#106531 = VERTEX_POINT ( 'NONE', #76599 ) ;
#106532 = CARTESIAN_POINT ( 'NONE',  ( 5.436732529336289588, -1.586671906620169104, 1.244382051841623538 ) ) ;
#106533 = CARTESIAN_POINT ( 'NONE',  ( -7.811469059767924605, 12.26513100303794168, -0.7998128361456281477 ) ) ;
#106534 = CARTESIAN_POINT ( 'NONE',  ( 1.499999999999990896, 4.275000000000021672, 1.214306433183764966E-14 ) ) ;
#106535 = CARTESIAN_POINT ( 'NONE',  ( 11.86145016429273191, 10.19999999999999929, 1.099999999999996758 ) ) ;
#106536 = CARTESIAN_POINT ( 'NONE',  ( 1.622189073652591240, 2.139406107190901185, -0.3685050674664645531 ) ) ;
#106537 = DIRECTION ( 'NONE',  ( 0.000000000000000000, 1.000000000000000000, 0.000000000000000000 ) ) ;
#106538 = CARTESIAN_POINT ( 'NONE',  ( 0.1938080739139167730, 1.976361990896974508, -0.7691651810952588875 ) ) ;
#106539 = CARTESIAN_POINT ( 'NONE',  ( 0.7499999999999902300, 2.264583334016148530, 1.299038105676669330 ) ) ;
#106540 = CARTESIAN_POINT ( 'NONE',  ( -1.797304807700269569, 14.48004927660067764, -11.89862588611542726 ) ) ;
#106541 = SURFACE_STYLE_USAGE ( .BOTH. , #91331 ) ;
#106542 = CARTESIAN_POINT ( 'NONE',  ( 4.895464504754282409, 8.144056917144915531, 1.010406422583273178 ) ) ;
#106543 = CARTESIAN_POINT ( 'NONE',  ( 0.9837496482606482573, 1.382075509872608299, 1.528818673835147024 ) ) ;
#106544 = CARTESIAN_POINT ( 'NONE',  ( -8.130085669689073313, 12.63685038127928806, 0.7998128361456481317 ) ) ;
#106545 = CARTESIAN_POINT ( 'NONE',  ( -0.6823417656250003738, 0.7177083336747519526, -1.181850606188749264 ) ) ;
#106546 = CARTESIAN_POINT ( 'NONE',  ( -0.4019237886466871523, 9.198664549684631098, -1.499999999999998668 ) ) ;
#106547 = VERTEX_POINT ( 'NONE', #130761 ) ;
#106548 = CARTESIAN_POINT ( 'NONE',  ( 3.176317266091326807, 0.8619891151622931513, 1.707069686517001195 ) ) ;
#106549 = CIRCLE ( 'NONE', #6118, 1.224999999999996980 ) ;
#106550 = CARTESIAN_POINT ( 'NONE',  ( 4.961649905909814251, 1.750258134581949232, -0.2615843724830448913 ) ) ;
#106551 = CARTESIAN_POINT ( 'NONE',  ( 5.254667053748194760, 8.288139441751686931, 1.199719254218452047 ) ) ;
#106552 = CARTESIAN_POINT ( 'NONE',  ( -4.334856428067329404, 6.080418470877079429, -1.599625672291256295 ) ) ;
#106553 = CARTESIAN_POINT ( 'NONE',  ( 0.2986855335190057859, -0.2218818089524568216, -1.797891974444510765 ) ) ;
#106555 = CARTESIAN_POINT ( 'NONE',  ( 6.116788041597909675, 0.1929307199614685164, 1.905880049602140636 ) ) ;
#106554 = CARTESIAN_POINT ( 'NONE',  ( 7.721398836998401904, -6.134628647623499909, 7.721398836998376147 ) ) ;
#106556 = CARTESIAN_POINT ( 'NONE',  ( 0.4849360239999983557, 1.980737741294085419, 0.6024896509310638804 ) ) ;
#106557 = CARTESIAN_POINT ( 'NONE',  ( -1.402160292154681736E-14, -0.8656249996585829720, 1.575800808251672791 ) ) ;
#106558 = AXIS2_PLACEMENT_3D ( 'NONE', #214401, #132179, #64986 ) ;
#106559 = CARTESIAN_POINT ( 'NONE',  ( 5.998880656844745474, 1.528293836345222312, -1.078463600801618405 ) ) ;
#106560 = CARTESIAN_POINT ( 'NONE',  ( 2.666400811807769777, -1.259032629953384719, 1.322343945743660543 ) ) ;
#106561 = ADVANCED_FACE ( 'NONE', ( #47332 ), #39578, .T. ) ;
#106563 = CARTESIAN_POINT ( 'NONE',  ( 6.465908158583062892, 6.764574590967027845, 0.2795716154820517829 ) ) ;
#106562 = CARTESIAN_POINT ( 'NONE',  ( 6.059228469117068805, -1.890744221452178353, -1.137928576693452820 ) ) ;
#106564 = CARTESIAN_POINT ( 'NONE',  ( 1.364683531249988757, 0.6343750003414208027, 0.000000000000000000 ) ) ;
#106565 = CARTESIAN_POINT ( 'NONE',  ( 2.840340301219072217, -1.062657783794159538, 1.767763702702547679 ) ) ;
#106566 = CARTESIAN_POINT ( 'NONE',  ( -8.538937818508475885, 8.856515631215026829, 1.040834085586084257E-14 ) ) ;
#106567 = CARTESIAN_POINT ( 'NONE',  ( 9.250740883225924804, 9.686952540052077509, 1.040834085586084257E-14 ) ) ;
#106568 = CARTESIAN_POINT ( 'NONE',  ( 4.005544317833563461, 6.760553239859419250, -1.199719254218452047 ) ) ;
#106569 = CARTESIAN_POINT ( 'NONE',  ( 0.6499751493908960676, 0.6786997614584532323, -2.052318101833712660 ) ) ;
#106570 = CARTESIAN_POINT ( 'NONE',  ( 6.408651866624735405, 0.6456447432892989946, 1.967203394946090977 ) ) ;
#106571 =( BOUNDED_SURFACE ( )  B_SPLINE_SURFACE ( 3, 3, ( 
 ( #185995, #120019, #203304, #54951, #121104, #33354, #139418, #92811, #39772, #23499, #205453, #123251, #6171, #105877, #157801, #7238 ),
 ( #106961, #10452, #204364, #73315, #125365, #88531, #56020, #72239, #24565, #171901, #141581, #8325, #191328, #57086, #189215, #138347 ),
 ( #206520, #109107, #142636, #140509, #42994, #75469, #76525, #91748, #207589, #154592, #188140, #9397, #158854, #175122, #59208, #122174 ),
 ( #26708, #89605, #40855, #155656, #172986, #74409, #38704, #208645, #90671, #60277, #156734, #187071, #58152, #104784, #124311, #190270 ),
 ( #41927, #108038, #25636, #174064, #170830, #22421, #94941, #11524, #2440, #18706, #209709, #159919, #97075, #179380, #12581, #126434 ),
 ( #79725, #145841, #133584, #128576, #78653, #46187, #93881, #110172, #129638, #63484, #211846, #67439, #150877, #117355, #34957, #61353 ),
 ( #29927, #1378, #176183, #160989, #31000, #84789, #195625, #199588, #47260, #111237, #27782, #177240, #144781, #62412, #192397, #166044 ) ),
 .UNSPECIFIED., .T., .F., .F. ) 
 B_SPLINE_SURFACE_WITH_KNOTS ( ( 4, 3, 4 ),
 ( 4, 2, 2, 2, 2, 2, 2, 4 ),
 ( 0.000000000000000000, 0.5000000000000000000, 1.000000000000000000 ),
 ( 0.6095821870314059865, 0.6120980958896804491, 0.6146140047479549118, 0.6196458224645037260, 0.6297094578976014656, 0.6397880689092279027, 0.6448273744150412323, 0.6498666799208544509 ),
 .UNSPECIFIED. ) 
 GEOMETRIC_REPRESENTATION_ITEM ( )  RATIONAL_B_SPLINE_SURFACE ( (
 ( 1.000000000000000000, 1.000000000000000000, 1.000000000000000000, 1.000000000000000000, 1.000000000000000000, 1.000000000000000000, 1.000000000000000000, 1.000000000000000000, 1.000000000000000000, 1.000000000000000000, 1.000000000000000000, 1.000000000000000000, 1.000000000000000000, 1.000000000000000000, 1.000000000000000000, 1.000000000000000000),
 ( 0.3333333333333333703, 0.3333333333333333703, 0.3333333333333333703, 0.3333333333333333703, 0.3333333333333333703, 0.3333333333333333703, 0.3333333333333333703, 0.3333333333333333703, 0.3333333333333333703, 0.3333333333333333703, 0.3333333333333333703, 0.3333333333333333703, 0.3333333333333333703, 0.3333333333333333703, 0.3333333333333333703, 0.3333333333333333703),
 ( 0.3333333333333333703, 0.3333333333333333703, 0.3333333333333333703, 0.3333333333333333703, 0.3333333333333333703, 0.3333333333333333703, 0.3333333333333333703, 0.3333333333333333703, 0.3333333333333333703, 0.3333333333333333703, 0.3333333333333333703, 0.3333333333333333703, 0.3333333333333333703, 0.3333333333333333703, 0.3333333333333333703, 0.3333333333333333703),
 ( 1.000000000000000000, 1.000000000000000000, 1.000000000000000000, 1.000000000000000000, 1.000000000000000000, 1.000000000000000000, 1.000000000000000000, 1.000000000000000000, 1.000000000000000000, 1.000000000000000000, 1.000000000000000000, 1.000000000000000000, 1.000000000000000000, 1.000000000000000000, 1.000000000000000000, 1.000000000000000000),
 ( 0.3333333333333333703, 0.3333333333333333703, 0.3333333333333333703, 0.3333333333333333703, 0.3333333333333333703, 0.3333333333333333703, 0.3333333333333333703, 0.3333333333333333703, 0.3333333333333333703, 0.3333333333333333703, 0.3333333333333333703, 0.3333333333333333703, 0.3333333333333333703, 0.3333333333333333703, 0.3333333333333333703, 0.3333333333333333703),
 ( 0.3333333333333333703, 0.3333333333333333703, 0.3333333333333333703, 0.3333333333333333703, 0.3333333333333333703, 0.3333333333333333703, 0.3333333333333333703, 0.3333333333333333703, 0.3333333333333333703, 0.3333333333333333703, 0.3333333333333333703, 0.3333333333333333703, 0.3333333333333333703, 0.3333333333333333703, 0.3333333333333333703, 0.3333333333333333703),
 ( 1.000000000000000000, 1.000000000000000000, 1.000000000000000000, 1.000000000000000000, 1.000000000000000000, 1.000000000000000000, 1.000000000000000000, 1.000000000000000000, 1.000000000000000000, 1.000000000000000000, 1.000000000000000000, 1.000000000000000000, 1.000000000000000000, 1.000000000000000000, 1.000000000000000000, 1.000000000000000000) ) ) 
 REPRESENTATION_ITEM ( '' )  SURFACE ( )  );
#106572 = CARTESIAN_POINT ( 'NONE',  ( -1.364683531250000748, -0.4281249996585800854, 0.000000000000000000 ) ) ;
#106573 = CARTESIAN_POINT ( 'NONE',  ( 4.059979352932830743, 2.145800628424157974, -0.2601280725000321148 ) ) ;
#106575 = CARTESIAN_POINT ( 'NONE',  ( 2.084357000244409175, 1.132115006494602394, -1.602057852124554316 ) ) ;
#106574 = CARTESIAN_POINT ( 'NONE',  ( 4.723309930327257433, 1.758355855194023487, 0.9934411112178792580 ) ) ;
#106576 = LINE ( 'NONE', #4714, #80609 ) ;
#106577 = ORIENTED_EDGE ( 'NONE', *, *, #42175, .T. ) ;
#106580 = CARTESIAN_POINT ( 'NONE',  ( 7.131225611108096274, 8.382479970123348778, 1.082531754730558626 ) ) ;
#106579 = CARTESIAN_POINT ( 'NONE',  ( 1.001543065824772753E-15, -3.521874999522041083, 3.793834371823811669 ) ) ;
#106578 = DIRECTION ( 'NONE',  ( -0.000000000000000000, 1.000000000000000000, -0.000000000000000000 ) ) ;
#106581 = CARTESIAN_POINT ( 'NONE',  ( -6.095272577795516789, 9.268845886473535245, 1.199719254218452047 ) ) ;
#106582 = CARTESIAN_POINT ( 'NONE',  ( 2.852750215419812108, -1.865046845876184189, -0.7672916333427428626 ) ) ;
#106583 = CARTESIAN_POINT ( 'NONE',  ( -4.497554271431319250, 6.270232621468402989, -1.599625672291256295 ) ) ;
#106584 = FACE_OUTER_BOUND ( 'NONE', #25579, .T. ) ;
#106585 = CARTESIAN_POINT ( 'NONE',  ( 5.660397963661894849, 1.910509065610028090, 0.08734628876111423523 ) ) ;
#106587 = DIRECTION ( 'NONE',  ( 0.000000000000000000, 0.000000000000000000, -1.000000000000000000 ) ) ;
#106586 = B_SPLINE_CURVE_WITH_KNOTS ( 'NONE', 3,
 ( #51983, #16247, #81284, #34650, #146311, #131163, #150560, #33588, #1062, #163612, #17317, #180906, #18391, #113861, #82333, #101789, #63964, #114908, #183034, #35712, #62647, #67127, #197154, #50911, #184093, #100720, #84468, #48791, #2120, #68195 ),
 .UNSPECIFIED., .F., .F.,
 ( 4, 2, 2, 2, 2, 2, 2, 2, 2, 2, 2, 2, 2, 2, 4 ),
 ( -5.999999999772596264E-08, 0.0009256177583834637734, 0.001851295516766925239, 0.002776973275150386271, 0.003702651033533847953, 0.004628328791917308768, 0.005554006550300769583, 0.006479684308684230398, 0.007405362067067692081, 0.009256717583834615445, 0.01018239534221807886, 0.01110807310060153881, 0.01203375085898500049, 0.01295942861736846217, 0.01481078413413538554 ),
 .UNSPECIFIED. ) ;
#106588 = CARTESIAN_POINT ( 'NONE',  ( 5.951666246274803562, 7.006327377817825663, 1.082531754730558626 ) ) ;
#106590 = CARTESIAN_POINT ( 'NONE',  ( 3.866814677988283044, -0.2004539179165897023, -2.006445418776988010 ) ) ;
#106589 = CARTESIAN_POINT ( 'NONE',  ( -8.392133896734675247, 10.81390885098904420, 1.443375672974064550 ) ) ;
#106591 = CARTESIAN_POINT ( 'NONE',  ( 1.499999999999989120, 3.754166666666685082, 0.8660254037844524744 ) ) ;
#106592 = CARTESIAN_POINT ( 'NONE',  ( -1.402160292154681736E-14, 14.73437500034139980, 1.575800808251682339 ) ) ;
#106593 = VECTOR ( 'NONE', #102765, 1000.000000000000000 ) ;
#106594 = CARTESIAN_POINT ( 'NONE',  ( 6.370102249521607973, 0.8915232854993185851, 1.476320845237573787 ) ) ;
#106595 = CARTESIAN_POINT ( 'NONE',  ( 6.038177310039780643, 8.137902509836795417, -1.599625672291283607 ) ) ;
#106596 = CARTESIAN_POINT ( 'NONE',  ( 9.408995418203975447, 10.07950886410055524, 0.7216878364870438212 ) ) ;
#106597 = CARTESIAN_POINT ( 'NONE',  ( 10.99861980075107937, -9.900000000000074962, -0.1919816227428264854 ) ) ;
#106598 = CARTESIAN_POINT ( 'NONE',  ( 4.147608549738549755, 0.6325110726591242072, -1.760471310998643624 ) ) ;
#106599 = CARTESIAN_POINT ( 'NONE',  ( 4.663288057535368125, 8.288536188413402783, 0.5084364831346009916 ) ) ;
#106600 = CARTESIAN_POINT ( 'NONE',  ( 1.674760025662187735, 1.393346669028448392, -1.531324272915953744 ) ) ;
#106601 = CARTESIAN_POINT ( 'NONE',  ( -1.387358672531441961, 7.251968950356099342, -4.302625267141395149 ) ) ;
#106602 = ORIENTED_EDGE ( 'NONE', *, *, #190530, .T. ) ;
#106603 = CARTESIAN_POINT ( 'NONE',  ( 4.686278372178935392, 5.496354851410763409, 1.199719254218452047 ) ) ;
#106604 = CARTESIAN_POINT ( 'NONE',  ( -0.05311194370935175268, -1.802413661875476913, -0.9041393574176490588 ) ) ;
#106605 = CARTESIAN_POINT ( 'NONE',  ( 6.633470331352866900, -0.1302952867699505302, 1.781688180685939926 ) ) ;
#106606 = EDGE_CURVE ( 'NONE', #51151, #134523, #85200, .T. ) ;
#106607 = CARTESIAN_POINT ( 'NONE',  ( 3.865483193227626124, 7.523831135491951372, -0.7216878364870338292 ) ) ;
#106608 = FACE_OUTER_BOUND ( 'NONE', #87550, .T. ) ;
#106609 = CARTESIAN_POINT ( 'NONE',  ( 7.415946836550712185, 10.63539316174243865, 1.082531754730558626 ) ) ;
#106610 = EDGE_CURVE ( 'NONE', #12264, #207276, #1512, .T. ) ;
#106611 = CARTESIAN_POINT ( 'NONE',  ( 6.401421083946654100, 10.62007503124645957, -0.7998128361456291469 ) ) ;
#106613 = CARTESIAN_POINT ( 'NONE',  ( 6.380494711820015930, -0.5163536399260219012, -1.844617532318414632 ) ) ;
#106612 = CARTESIAN_POINT ( 'NONE',  ( -5.422371370461663176, 8.413518134592214537, -1.199719254218446718 ) ) ;
#106614 = CARTESIAN_POINT ( 'NONE',  ( 0.000000000000000000, -4.000000000000003553, 0.000000000000000000 ) ) ;
#106615 = SURFACE_STYLE_USAGE ( .BOTH. , #142301 ) ;
#106617 = ORIENTED_EDGE ( 'NONE', *, *, #32909, .T. ) ;
#106616 = CARTESIAN_POINT ( 'NONE',  ( 3.389175213736285386, 6.897862149426897460, 0.7216878364870317197 ) ) ;
#106618 = CARTESIAN_POINT ( 'NONE',  ( -6.860062538834774237, 10.94723069537516302, 0.7216878364870458196 ) ) ;
#106619 = CARTESIAN_POINT ( 'NONE',  ( 3.379894511112140787, 1.369989894601089775, 1.672159933133889442 ) ) ;
#106620 = CARTESIAN_POINT ( 'NONE',  ( -2.810282979782591006, 6.500690253046801814, 0.000000000000000000 ) ) ;
#106621 = EDGE_CURVE ( 'NONE', #40241, #5998, #163080, .T. ) ;
#106622 = CARTESIAN_POINT ( 'NONE',  ( 8.000720045840086669, 8.506797273001177828, 0.7216878364870267237 ) ) ;
#106623 = CARTESIAN_POINT ( 'NONE',  ( 0.9144942500491149984, -2.120778211678171488, 0.005759991200282586418 ) ) ;
#106624 = CARTESIAN_POINT ( 'NONE',  ( 5.666980381186065507, -1.651371415153819688, -0.7785968546244539379 ) ) ;
#106625 = CARTESIAN_POINT ( 'NONE',  ( 9.013329340612937557, 11.11377505082129069, -8.022259956411712523 ) ) ;
#106626 = CARTESIAN_POINT ( 'NONE',  ( 1.141796867408477967, 0.8028701493673767731, -1.800646566474963572 ) ) ;
#106627 = CARTESIAN_POINT ( 'NONE',  ( 3.550944491985886575, 0.2853618425060593378, 1.890879049853078087 ) ) ;
#106628 = ORIENTED_EDGE ( 'NONE', *, *, #52227, .T. ) ;
#106629 = CARTESIAN_POINT ( 'NONE',  ( -11.48243876534946040, 9.799999999999998934, -3.200000000000001510 ) ) ;
#106630 = CARTESIAN_POINT ( 'NONE',  ( 5.230891393285493685, -1.853837313009810028, -0.6654804215649990917 ) ) ;
#106631 = CARTESIAN_POINT ( 'NONE',  ( 0.6560686395847237229, -1.407132438187887136, 1.338565165000434876 ) ) ;
#106632 = ORIENTED_EDGE ( 'NONE', *, *, #51505, .T. ) ;
#106633 = CARTESIAN_POINT ( 'NONE',  ( -4.664887371553763096, 7.600063145858131364, -1.199719254218453823 ) ) ;
#106635 = CARTESIAN_POINT ( 'NONE',  ( -1.225000000000045386, 1.312500000682802259, -4.336808689942017736E-14 ) ) ;
#106634 = CARTESIAN_POINT ( 'NONE',  ( -5.472651281771599763, 6.413789912602166687, 1.199719254218452935 ) ) ;
#106636 = CARTESIAN_POINT ( 'NONE',  ( 5.356880090730850696, 9.263794182579101033, 0.7216878364870317197 ) ) ;
#106638 = VERTEX_POINT ( 'NONE', #641 ) ;
#106637 = CARTESIAN_POINT ( 'NONE',  ( 3.879479457080482696, 0.2311173251203814394, -1.898182577502210977 ) ) ;
#106639 = CARTESIAN_POINT ( 'NONE',  ( 1.255210933454937283, -1.738917431694649185, 1.358592805172780693 ) ) ;
#106640 = CARTESIAN_POINT ( 'NONE',  ( 9.333041836227119248, 3.553052365627043407, -7.472413793103452662 ) ) ;
#106641 = CARTESIAN_POINT ( 'NONE',  ( 6.639320575229259447, 0.002292789353198348111, 1.996863816985874118 ) ) ;
#106642 = CARTESIAN_POINT ( 'NONE',  ( 0.000000000000000000, -8.176568542494905500, 0.000000000000000000 ) ) ;
#106643 = CARTESIAN_POINT ( 'NONE',  ( -4.596923820214036560, 8.483565078729160547, 0.2266403168418751335 ) ) ;
#106644 = CARTESIAN_POINT ( 'NONE',  ( -0.08896015503664694846, 7.049507384514476449, -3.948637857580539201 ) ) ;
#106645 = CARTESIAN_POINT ( 'NONE',  ( 2.277862540309500083, -2.008769142935047380, 0.5008063122204224893 ) ) ;
#106646 = CARTESIAN_POINT ( 'NONE',  ( -5.388475986427523345, 8.373973519885682393, 1.199719254218452047 ) ) ;
#106647 = TOROIDAL_SURFACE ( 'NONE', #26953, 2.349999999999999645, 0.1000000000000000056 ) ;
#106648 = CARTESIAN_POINT ( 'NONE',  ( -4.603881723180708541, 8.384271979250147666, 0.04571010684512218092 ) ) ;
#106649 = CARTESIAN_POINT ( 'NONE',  ( 0.1280963075596490419, -1.331634228802502928, -1.703589906866372017 ) ) ;
#106650 = CARTESIAN_POINT ( 'NONE',  ( 4.313465427442102929, 8.184126765324453601, 0.7998128361456462443 ) ) ;
#106651 = CARTESIAN_POINT ( 'NONE',  ( -11.95061148709128140, 8.982475982309534146, -1.242198177808604198 ) ) ;
#106652 = CARTESIAN_POINT ( 'NONE',  ( 3.757017964762656703, 7.397288368949487491, -1.734723475976807094E-15 ) ) ;
#106653 = CARTESIAN_POINT ( 'NONE',  ( 1.772826578343081660, 3.950000000000036593, -0.4000000000000478728 ) ) ;
#106654 = CARTESIAN_POINT ( 'NONE',  ( 4.403700966340357681, 4.032072637018845107, -0.7998128361456211532 ) ) ;
#106655 = CARTESIAN_POINT ( 'NONE',  ( 1.364683531249996529, 13.27604166700806410, 0.7879004041258405033 ) ) ;
#106657 = CARTESIAN_POINT ( 'NONE',  ( -5.769876891067536206, 8.889217585290882795, 1.199719254218454489 ) ) ;
#106656 = CARTESIAN_POINT ( 'NONE',  ( 6.825078400183548055, 3.702925343214446663, 2.370119418288775925 ) ) ;
#106658 = CARTESIAN_POINT ( 'NONE',  ( 5.221237796217499394, 1.709784868986977902, 0.2885349091684140665 ) ) ;
#106659 = CARTESIAN_POINT ( 'NONE',  ( -4.711622075948912247, 5.455646162483875017, -1.199719254218446718 ) ) ;
#106660 = CIRCLE ( 'NONE', #47901, 0.08000000000000018208 ) ;
#106661 = CARTESIAN_POINT ( 'NONE',  ( 2.008725816923035978, 0.6454906730102347723, 1.967154155859623055 ) ) ;
#106662 = CARTESIAN_POINT ( 'NONE',  ( 3.374719764411674205, -0.4154235484931252942, -2.075916080105549177 ) ) ;
#106664 = CARTESIAN_POINT ( 'NONE',  ( 6.425674737872927089, 9.584038729905381970, -1.199719254218440723 ) ) ;
#106663 = B_SPLINE_CURVE_WITH_KNOTS ( 'NONE', 3,
 ( #18989, #69858, #120857, #22168, #85071, #185753, #38461 ),
 .UNSPECIFIED., .F., .F.,
 ( 4, 3, 4 ),
 ( 0.000000000000000000, 2.757963454290271384E-05, 5.739065715766676189E-05 ),
 .UNSPECIFIED. ) ;
#106666 = EDGE_CURVE ( 'NONE', #167216, #45056, #2298, .T. ) ;
#106665 = CARTESIAN_POINT ( 'NONE',  ( -1.201851678989727383E-14, 3.571875000341422357, 1.575800808251672791 ) ) ;
#106667 = CARTESIAN_POINT ( 'NONE',  ( 1.533974946755271240, 1.168952700103634390, 1.584878304665905180 ) ) ;
#106668 = CARTESIAN_POINT ( 'NONE',  ( 5.809489818682099127, 6.211223759639540987, 0.9523037572534819306 ) ) ;
#106669 = CYLINDRICAL_SURFACE ( 'NONE', #84058, 2.500000000000007994 ) ;
#106670 = CARTESIAN_POINT ( 'NONE',  ( 4.207168913946373934, -0.3938425722496830539, 2.258028373892074558 ) ) ;
#106671 = CARTESIAN_POINT ( 'NONE',  ( 1.945663734523142230, 0.6997465788082489757, -1.686465609443507763 ) ) ;
#106672 = ADVANCED_FACE ( 'NONE', ( #29999 ), #103601, .F. ) ;
#106673 = CARTESIAN_POINT ( 'NONE',  ( 6.215487077222150880, 6.216099443039444949, 0.000000000000000000 ) ) ;
#106674 = CARTESIAN_POINT ( 'NONE',  ( 6.439759776366769550, 8.536139043893143707, 1.443375672974076540 ) ) ;
#106675 = CARTESIAN_POINT ( 'NONE',  ( -6.835281999583978418, 11.12624609948998966, -0.7998128361456291469 ) ) ;
#106676 = CARTESIAN_POINT ( 'NONE',  ( 2.531496316177814787, -0.1932786158439051827, 2.003878288502713101 ) ) ;
#106677 = CARTESIAN_POINT ( 'NONE',  ( 3.045700443693433179, 1.383923128670875746, 1.390673908496591782 ) ) ;
#106678 = CARTESIAN_POINT ( 'NONE',  ( -6.821723845970312894, 11.11042825360738284, 0.000000000000000000 ) ) ;
#106679 = CARTESIAN_POINT ( 'NONE',  ( -4.740547266272593596, 8.682388910626682943, -0.7998128361456281477 ) ) ;
#106680 = CARTESIAN_POINT ( 'NONE',  ( 0.1751657365761339624, 7.629137130509054288, -2.644001943226172102 ) ) ;
#106682 = CARTESIAN_POINT ( 'NONE',  ( 4.082668839255446436, -0.1736907016443404450, -1.761279006307460371 ) ) ;
#106681 = CARTESIAN_POINT ( 'NONE',  ( 5.876921326125680523, 1.932075295558054240, -0.7991432938223922422 ) ) ;
#106683 = CARTESIAN_POINT ( 'NONE',  ( 6.021229617800532452, 6.197391773621639288, 0.000000000000000000 ) ) ;
#106684 = CARTESIAN_POINT ( 'NONE',  ( 1.078377591563362436, -2.138745004354754897, -0.4770250503970187572 ) ) ;
#106685 = CARTESIAN_POINT ( 'NONE',  ( 5.613164593121685364, -1.696513092703657799, 0.3873091720919922265 ) ) ;
#106686 = CARTESIAN_POINT ( 'NONE',  ( 6.591235234537977661, 10.84152487360300299, 0.7998128361456462443 ) ) ;
#106687 = CARTESIAN_POINT ( 'NONE',  ( -4.650083499807243115, 5.295740330745369207, -1.052294140492322283 ) ) ;
#106688 = CARTESIAN_POINT ( 'NONE',  ( 5.854147224351119227, 0.1731004610599009841, -2.292201554650086237 ) ) ;
#106689 = CARTESIAN_POINT ( 'NONE',  ( 0.1333692844072559558, 0.7140749627707367875, -2.136770008611441618 ) ) ;
#106690 = CARTESIAN_POINT ( 'NONE',  ( 5.395702507230883072, 0.1292110896585068891, 1.729053200853872596 ) ) ;
#106691 = CARTESIAN_POINT ( 'NONE',  ( 1.612255294781844706, -2.189918024983358080, 0.2725913246661854084 ) ) ;
#106692 = CARTESIAN_POINT ( 'NONE',  ( 5.723135995274492238, -1.960344405425541670, -0.9336216343173405763 ) ) ;
#106693 = CARTESIAN_POINT ( 'NONE',  ( -1.999999999999988010, 2.428612866367529932E-14, 1.500000000000001332 ) ) ;
#106694 = CARTESIAN_POINT ( 'NONE',  ( 0.09316046741510237983, 1.845552173327277501, 1.037660268145562004 ) ) ;
#106695 = CARTESIAN_POINT ( 'NONE',  ( 4.500000000000003553, -2.561000571632643674E-13, -2.052068128417943171 ) ) ;
#106696 = CARTESIAN_POINT ( 'NONE',  ( 6.827182134110200806, 2.035520418778674845, 2.394189263408800450 ) ) ;
#106697 = CARTESIAN_POINT ( 'NONE',  ( 4.875960570263176308, 1.108828003875685475, 1.575097709652195643 ) ) ;
#106698 = CARTESIAN_POINT ( 'NONE',  ( 1.717743135698499124, 1.849103211704594463, 1.230578002476825583 ) ) ;
#106699 = ORIENTED_EDGE ( 'NONE', *, *, #38876, .F. ) ;
#106700 = CARTESIAN_POINT ( 'NONE',  ( 1.499999999999989120, 4.254166666666687746, 0.8660254037844524744 ) ) ;
#106701 = CARTESIAN_POINT ( 'NONE',  ( 5.820528018968444961, 5.685037531751635953, 0.7998128361456341429 ) ) ;
#106702 = CARTESIAN_POINT ( 'NONE',  ( 5.445571254183207088, 9.504916896522420444, -0.7998128361456281477 ) ) ;
#106703 = VECTOR ( 'NONE', #127459, 1000.000000000000000 ) ;
#106704 = CARTESIAN_POINT ( 'NONE',  ( 3.370003599138057471, 0.5381768412672756074, -2.155016279732512974 ) ) ;
#106705 = CARTESIAN_POINT ( 'NONE',  ( -8.893785580884703279, 10.43879993486270585, 1.082531754730558626 ) ) ;
#106706 = FACE_OUTER_BOUND ( 'NONE', #18379, .T. ) ;
#106707 = CARTESIAN_POINT ( 'NONE',  ( 6.155038550924139429, 9.164333495178082600, 1.082531754730558626 ) ) ;
#106708 = CARTESIAN_POINT ( 'NONE',  ( -8.310784975052671442, 11.67937098999472667, -1.082531754730543083 ) ) ;
#106709 = CARTESIAN_POINT ( 'NONE',  ( 5.234856708652215751, 9.121433570154021453, 0.7216878364870317197 ) ) ;
#106710 = CARTESIAN_POINT ( 'NONE',  ( 2.127577483945505055, 0.4445034925110411539, 1.966644524931899563 ) ) ;
#106712 = CARTESIAN_POINT ( 'NONE',  ( 0.3036763228623740041, -1.592034637876770908, -1.310935287704196206 ) ) ;
#106711 = CARTESIAN_POINT ( 'NONE',  ( 8.589254009457354400, 9.979550084910457031, -1.199719254218446718 ) ) ;
#106713 = CARTESIAN_POINT ( 'NONE',  ( -10.99917004716958857, -6.764708007038216842, 0.1531059978909550534 ) ) ;
#106714 = CARTESIAN_POINT ( 'NONE',  ( 6.821160681006781523, 9.051383109298340557, 1.443375672974063439 ) ) ;
#106715 = CARTESIAN_POINT ( 'NONE',  ( 6.620655732516682157, 0.01042156863441953685, 1.726407961933309476 ) ) ;
#106716 = CARTESIAN_POINT ( 'NONE',  ( -2.530224277154541124, 2.018041202053984406, 11.90376931803457872 ) ) ;
#106717 = CARTESIAN_POINT ( 'NONE',  ( -1.201851678989727383E-14, 1.821875000341421691, 1.575800808251672791 ) ) ;
#106718 = CARTESIAN_POINT ( 'NONE',  ( 1.000807349803897628, 1.442299932730039869, 1.025250199436118503 ) ) ;
#106719 = CARTESIAN_POINT ( 'NONE',  ( 0.4752326960846975923, -2.001511663014220677, -0.2440270837566413387 ) ) ;
#106720 = CARTESIAN_POINT ( 'NONE',  ( 0.4504185290156897947, -1.555054577268409899, -0.9855837367087336709 ) ) ;
#106721 = CARTESIAN_POINT ( 'NONE',  ( 4.142302782979132125, 0.6112592793995803575, 2.209291399377455889 ) ) ;
#106722 = CARTESIAN_POINT ( 'NONE',  ( 2.044624030687072214, -1.478315374303545315, -1.097237131862264903 ) ) ;
#106723 = CARTESIAN_POINT ( 'NONE',  ( 10.07387183015377197, 11.71160420905630062, -1.199719254218440723 ) ) ;
#106724 = CARTESIAN_POINT ( 'NONE',  ( 7.416522329255045065, 14.99999999999999645, -9.452665224861386051 ) ) ;
#106725 = CARTESIAN_POINT ( 'NONE',  ( 3.487140482124751362, 1.650829432287181264, -0.7796944959364560113 ) ) ;
#106726 = CARTESIAN_POINT ( 'NONE',  ( 4.026017654026761150, -1.753031021560845559, 0.9963007555989014108 ) ) ;
#106727 = CARTESIAN_POINT ( 'NONE',  ( -9.938290294017125603, 11.55342575023019691, -1.199719254218441611 ) ) ;
#106729 = CARTESIAN_POINT ( 'NONE',  ( -9.584291988782265292, -7.189630408304557463, 0.001123102408834306858 ) ) ;
#106728 = CARTESIAN_POINT ( 'NONE',  ( 3.626065245518626412, -1.345661663401491293, -1.818709669598504997 ) ) ;
#106730 = CARTESIAN_POINT ( 'NONE',  ( 5.807678370005410429, -0.5150985282868367765, 2.041858835689168927 ) ) ;
#106731 = CARTESIAN_POINT ( 'NONE',  ( 9.257559171758622085, 13.68169161456526162, 6.840446529487702598 ) ) ;
#106732 = CARTESIAN_POINT ( 'NONE',  ( 2.066927875543830950, 1.535623996113824496, -1.388825173883188713 ) ) ;
#106733 = CARTESIAN_POINT ( 'NONE',  ( 5.190073875932979419, 4.949507698210251938, 0.7998128361456341429 ) ) ;
#106734 = CARTESIAN_POINT ( 'NONE',  ( 0.6801582343749813520, 0.005208333674754095366, 1.178068619123793015 ) ) ;
#106735 = CARTESIAN_POINT ( 'NONE',  ( 5.391314312714450274, -0.05227466736787074464, -2.120015263102632552 ) ) ;
#106737 = CARTESIAN_POINT ( 'NONE',  ( 0.8383531591091289981, 1.897801360490163569, 0.3304300003270659314 ) ) ;
#106736 = CARTESIAN_POINT ( 'NONE',  ( -8.157201976916404362, 12.66848607304450702, -0.7998128361456281477 ) ) ;
#106738 = CARTESIAN_POINT ( 'NONE',  ( -5.113360211009450040, 5.994616996712990975, -1.199719254218453823 ) ) ;
#106739 = CARTESIAN_POINT ( 'NONE',  ( 7.086107841436786181, 11.41887624831828418, 1.040834085586084257E-14 ) ) ;
#106740 = CARTESIAN_POINT ( 'NONE',  ( 4.217995187182915551, 7.935095128439824563, 0.7216878364870257245 ) ) ;
#106741 = CARTESIAN_POINT ( 'NONE',  ( 4.677432586336220055, 6.849818891840005364, 1.226792522213099979 ) ) ;
#106742 = CARTESIAN_POINT ( 'NONE',  ( -1.737499999999997824, -0.5979166657107508609, 3.009438278150925683 ) ) ;
#106743 = VECTOR ( 'NONE', #190395, 1000.000000000000000 ) ;
#106744 = CARTESIAN_POINT ( 'NONE',  ( -4.334856428067329404, 6.080418470877079429, -1.599625672291256295 ) ) ;
#106745 = CARTESIAN_POINT ( 'NONE',  ( 1.002519415922138002, -0.9925456330053865628, 1.987394366727333717 ) ) ;
#106746 = CARTESIAN_POINT ( 'NONE',  ( 2.608543117039106463, -0.8048738574607334773, -1.946287526097515430 ) ) ;
#106747 = CARTESIAN_POINT ( 'NONE',  ( -3.467853430045390706, 7.267855778353407459, 0.7998128361456352531 ) ) ;
#106748 = CARTESIAN_POINT ( 'NONE',  ( 6.913768267964901071, 10.15348118167935709, -1.199719254218441611 ) ) ;
#106749 = CARTESIAN_POINT ( 'NONE',  ( 5.770303593930925956, -0.8350939829899912681, -1.663081984830430793 ) ) ;
#106750 = CARTESIAN_POINT ( 'NONE',  ( 8.437251666405968464, 8.737881787095446384, 1.040834085586084257E-14 ) ) ;
#106751 = CARTESIAN_POINT ( 'NONE',  ( -11.04536101718726293, 10.19999999999999929, -1.100000000000000311 ) ) ;
#106752 = CARTESIAN_POINT ( 'NONE',  ( -6.211043768836215229, 8.339580045099285854, 1.443375672974064550 ) ) ;
#106753 = CARTESIAN_POINT ( 'NONE',  ( -7.185458225562757484, 11.32685899655781903, 0.7216878364870458196 ) ) ;
#106754 = CARTESIAN_POINT ( 'NONE',  ( -0.06985027309261250539, -2.078401542846250116, 0.4200961532789050379 ) ) ;
#106755 = CARTESIAN_POINT ( 'NONE',  ( -6.831329296439251131, 9.063246493969506545, -1.599625672291271394 ) ) ;
#106757 = CARTESIAN_POINT ( 'NONE',  ( 3.016010921186715432, 1.952665002612500533, -0.1895750030070641190 ) ) ;
#106756 = CARTESIAN_POINT ( 'NONE',  ( -1.225000000000005640, 1.387778780781445676E-14, -1.387778780781445676E-14 ) ) ;
#106758 = CARTESIAN_POINT ( 'NONE',  ( 2.272554088390315030, -1.330374092946192688, 1.703740541667747133 ) ) ;
#106760 = CARTESIAN_POINT ( 'NONE',  ( -4.775553520644376881, 6.797630844710244702, -1.243162211532616857 ) ) ;
#106759 = CARTESIAN_POINT ( 'NONE',  ( -4.634908411025374875, 6.500755460986618495, 1.599625672291263179 ) ) ;
#106761 = CARTESIAN_POINT ( 'NONE',  ( 1.364683531249988757, 2.134375000341422357, 1.214306433183764966E-14 ) ) ;
#106762 = CARTESIAN_POINT ( 'NONE',  ( 3.714586447349605081, -0.1257948980903991487, 1.735838019273880928 ) ) ;
#106763 = AXIS2_PLACEMENT_3D ( 'NONE', #46852, #99845, #131338 ) ;
#106764 = CARTESIAN_POINT ( 'NONE',  ( 7.307481608085759639, 7.627742752295940676, 1.040834085586084257E-14 ) ) ;
#106765 = CARTESIAN_POINT ( 'NONE',  ( -11.79406710134376191, 4.782197168659454434, 4.941180684906744780 ) ) ;
#106766 = CARTESIAN_POINT ( 'NONE',  ( 0.9366540776252421097, 2.129889809250965271, 0.3686189752144660714 ) ) ;
#106767 = CARTESIAN_POINT ( 'NONE',  ( 2.513045873335068237, 2.015604327017831654, 0.05229110803010171560 ) ) ;
#106768 = CARTESIAN_POINT ( 'NONE',  ( -10.95308175811721085, 12.30000000000000071, -1.800000000000001155 ) ) ;
#106769 = CARTESIAN_POINT ( 'NONE',  ( 0.6311622855796321652, 3.199999999999987743, 0.3999999999999646061 ) ) ;
#106770 = GEOMETRIC_CURVE_SET ( 'NONE', ( #168733, #3369, #103896, #127391 ) ) ;
#106771 = CARTESIAN_POINT ( 'NONE',  ( 2.465646028844501902, 1.933766160897397057, -0.3828895411656701997 ) ) ;
#106774 = VERTEX_POINT ( 'NONE', #88340 ) ;
#106773 = CARTESIAN_POINT ( 'NONE',  ( -5.533136088152923904, 6.588318536667425285, 1.082531754730549078 ) ) ;
#106772 = CARTESIAN_POINT ( 'NONE',  ( 6.539320575229249144, 0.007148032025052972194, 1.896977914940492393 ) ) ;
#106775 = CARTESIAN_POINT ( 'NONE',  ( -5.438229012412899799, 7.437962829272074750, -1.443375672974066548 ) ) ;
#106776 = CARTESIAN_POINT ( 'NONE',  ( 7.388267364804250725, 7.584343111885245570, -0.7998128361456341429 ) ) ;
#106777 = CARTESIAN_POINT ( 'NONE',  ( -5.444481204339554736, 8.509589284108232121, 1.199719254218454489 ) ) ;
#106778 = CARTESIAN_POINT ( 'NONE',  ( 2.350265711909118593, 0.9499565981557709371, -1.782299418695271198 ) ) ;
#106779 = DIRECTION ( 'NONE',  ( 1.000000000000000000, -0.000000000000000000, -0.000000000000000000 ) ) ;
#106780 = CARTESIAN_POINT ( 'NONE',  ( 6.088978940744814494, -0.3304744056438710387, -2.283700556900492451 ) ) ;
#106781 = CARTESIAN_POINT ( 'NONE',  ( 0.000000000000000000, -8.176568542494905500, 0.000000000000000000 ) ) ;
#106782 = CARTESIAN_POINT ( 'NONE',  ( 2.694135368495911731, 0.9291169126603683326, -1.727816930623335967 ) ) ;
#106783 = CARTESIAN_POINT ( 'NONE',  ( 8.341290820905593151, 10.75459192918846618, 1.599625672291281386 ) ) ;
#106784 = CARTESIAN_POINT ( 'NONE',  ( 0.6334356698059574464, 0.5880228326464317368, 1.928751028484784191 ) ) ;
#106785 = ORIENTED_EDGE ( 'NONE', *, *, #89006, .F. ) ;
#106786 = CARTESIAN_POINT ( 'NONE',  ( 2.694651208505644213, 1.530237149716510370, -1.463602791221560118 ) ) ;
#106788 = CARTESIAN_POINT ( 'NONE',  ( -7.705111371268023923, 7.883718109434487253, 1.040834085586084257E-14 ) ) ;
#106787 = CARTESIAN_POINT ( 'NONE',  ( -2.286521462199063492, 5.819358805874190743, 1.040834085586084257E-14 ) ) ;
#106789 = CARTESIAN_POINT ( 'NONE',  ( 1.745803608711377075, 0.5764907460206626366, 1.748616612666432868 ) ) ;
#106790 = EDGE_LOOP ( 'NONE', ( #34878, #119835, #51225, #32839 ) ) ;
#106791 = CARTESIAN_POINT ( 'NONE',  ( -9.215791728987058562, 11.77484298861683598, -1.599625672291263179 ) ) ;
#106792 = CARTESIAN_POINT ( 'NONE',  ( 9.768119350134290002, 11.88398385152791903, 6.892589425638673717 ) ) ;
#106793 = CARTESIAN_POINT ( 'NONE',  ( 4.394861267144759331, -2.057662932662501110, -0.5123870273424437904 ) ) ;
#106794 = CARTESIAN_POINT ( 'NONE',  ( 0.2339851986729903077, 0.3116528534230639247, 1.814411239467295101 ) ) ;
#106795 = CARTESIAN_POINT ( 'NONE',  ( -1.499999999999997780, 5.181250000682820378, 1.214306433183764966E-14 ) ) ;
#106796 = CARTESIAN_POINT ( 'NONE',  ( 7.613066949273408213, 8.840665181362512115, -1.199719254218441611 ) ) ;
#106797 = CARTESIAN_POINT ( 'NONE',  ( 6.556249800660121529, 9.806652646482286073, 1.199719254218452047 ) ) ;
#106798 = CARTESIAN_POINT ( 'NONE',  ( 4.903620131156614548, -0.5536938069644473659, 1.984910608926907960 ) ) ;
#106800 = CARTESIAN_POINT ( 'NONE',  ( 1.891909123491273492, -0.4922293657834125313, -1.774144672653771293 ) ) ;
#106799 = CARTESIAN_POINT ( 'NONE',  ( -7.714753101375940503, 8.959299025482085455, 1.199719254218462483 ) ) ;
#106801 = CARTESIAN_POINT ( 'NONE',  ( 1.364683531249988535, 4.655208333674755394, -0.7879004041258300672 ) ) ;
#106802 = CARTESIAN_POINT ( 'NONE',  ( -1.598423149420381106, 8.713846000021360894, 2.500000000000011102 ) ) ;
#106803 = CARTESIAN_POINT ( 'NONE',  ( 0.9311234436981525864, -1.603119629485603825, 3.474999999999998757 ) ) ;
#106804 = AXIS2_PLACEMENT_3D ( 'NONE', #54137, #35739, #149505 ) ;
#106805 = CARTESIAN_POINT ( 'NONE',  ( 0.5752038918783763943, -2.079344756725898691, -0.7397341299467049547 ) ) ;
#106806 = CARTESIAN_POINT ( 'NONE',  ( 3.743696771605113494, -1.710248914368957873, -1.481124664604586583 ) ) ;
#106807 = CARTESIAN_POINT ( 'NONE',  ( -8.242994207428740339, 9.679543332497402730, 1.082531754730558626 ) ) ;
#106808 = CARTESIAN_POINT ( 'NONE',  ( 3.164119808340008611, 1.811767227632065325, -0.004774541488360150264 ) ) ;
#106809 = CARTESIAN_POINT ( 'NONE',  ( 3.327253086410830729, -1.454009962414861912, -1.247479002808443704 ) ) ;
#106810 = CARTESIAN_POINT ( 'NONE',  ( 4.000488093070094564, 2.060113009926473726, 0.2059288336104248551 ) ) ;
#106811 = CARTESIAN_POINT ( 'NONE',  ( -1.201851678989727383E-14, 3.634375000341422357, 1.575800808251672791 ) ) ;
#106812 = CARTESIAN_POINT ( 'NONE',  ( 2.483225996990960027, 1.803144932609510143, -0.7974705804912070040 ) ) ;
#106813 = CARTESIAN_POINT ( 'NONE',  ( 0.5867820057828515568, -0.2326963965399355405, -1.912219011898611765 ) ) ;
#106814 = CARTESIAN_POINT ( 'NONE',  ( 4.100366707588389836, -0.5864361863821172527, -1.776433678864146382 ) ) ;
#106815 = EDGE_CURVE ( 'NONE', #68781, #45420, #133924, .T. ) ;
#106816 = CARTESIAN_POINT ( 'NONE',  ( 2.245130213409586961, 0.5076759487793567338, 2.251015715305480391 ) ) ;
#106817 = CARTESIAN_POINT ( 'NONE',  ( 4.211269073929763351, -1.546465011353677532, -1.035020834652039090 ) ) ;
#106818 = CARTESIAN_POINT ( 'NONE',  ( 1.364683531249988535, 4.405208333674754506, -0.7879004041258300672 ) ) ;
#106819 = CIRCLE ( 'NONE', #65297, 0.7499999999999997780 ) ;
#106820 = CARTESIAN_POINT ( 'NONE',  ( -3.100010679019018500, 6.768429558830820980, 1.040834085586084257E-14 ) ) ;
#106821 = CARTESIAN_POINT ( 'NONE',  ( 11.40591166468351503, 3.507114751586604129, -3.706005353348470255 ) ) ;
#106822 = B_SPLINE_CURVE_WITH_KNOTS ( 'NONE', 3,
 ( #206911, #122575, #140900, #188537, #123640, #109499 ),
 .UNSPECIFIED., .F., .F.,
 ( 4, 2, 4 ),
 ( 0.000000000000000000, 0.0003132070624402877746, 0.0006264141248805755492 ),
 .UNSPECIFIED. ) ;
#106823 = CARTESIAN_POINT ( 'NONE',  ( 0.4695305163736606668, 0.2040741594158005934, -2.096154701512464413 ) ) ;
#106824 = CARTESIAN_POINT ( 'NONE',  ( 4.650083499362880346, 4.527444958785877382, 0.7216878364870317197 ) ) ;
#106826 = CARTESIAN_POINT ( 'NONE',  ( -11.00006988736403102, -9.999999999999994671, 0.09199170129444225741 ) ) ;
#106825 = CARTESIAN_POINT ( 'NONE',  ( 1.364683531249990311, 4.926041667008083991, 0.7879004041258500513 ) ) ;
#106827 = CARTESIAN_POINT ( 'NONE',  ( 6.854756222516504849, -1.675677847961650313, 1.365199464886861946 ) ) ;
#106828 = CARTESIAN_POINT ( 'NONE',  ( 2.478903650112133317, -1.459102030866548994, 1.539066919819010781 ) ) ;
#106829 = FILL_AREA_STYLE ('',( #90542 ) ) ;
#106830 = CARTESIAN_POINT ( 'NONE',  ( 0.4748752182902976071, -1.459934291025711373, 1.395986992609834276 ) ) ;
#106831 = CARTESIAN_POINT ( 'NONE',  ( -0.6823417656250003738, 1.217708333674752286, -1.181850606188749264 ) ) ;
#106832 = CARTESIAN_POINT ( 'NONE',  ( -3.904385051055635270, 6.538571078664754843, 1.082531754730560403 ) ) ;
#106833 = CARTESIAN_POINT ( 'NONE',  ( 6.308621549060418054, 6.254479983525607523, 0.7998128361456341429 ) ) ;
#106834 = CARTESIAN_POINT ( 'NONE',  ( 1.353037089713942320, -1.704917477850418805, 1.328741451194020762 ) ) ;
#106837 = CARTESIAN_POINT ( 'NONE',  ( 3.199361063144961825, 6.676412307070352270, -0.7216878364870267237 ) ) ;
#106836 = CARTESIAN_POINT ( 'NONE',  ( 6.925078400183550364, 4.696033252921790968, 2.518291795588607052 ) ) ;
#106835 = CARTESIAN_POINT ( 'NONE',  ( 4.037295881819344956, 7.932205305423046582, -0.7998128361456362523 ) ) ;
#106838 = CARTESIAN_POINT ( 'NONE',  ( -4.787964524281469458, 5.614988695530339413, -1.199719254218453823 ) ) ;
#106839 = CARTESIAN_POINT ( 'NONE',  ( 6.122279814772176643, 1.995267444086584296, 0.2910868170948808786 ) ) ;
#106840 = CARTESIAN_POINT ( 'NONE',  ( -8.351459436338041442, 9.806086099558291025, -1.082531754730543971 ) ) ;
#106841 = CARTESIAN_POINT ( 'NONE',  ( 0.08191350661116909848, -1.027414926483052326, 1.935800647029708443 ) ) ;
#106842 = FILL_AREA_STYLE_COLOUR ( '', #101685 ) ;
#106844 = CARTESIAN_POINT ( 'NONE',  ( 1.364683531249996529, 10.71354166700806942, 0.7879004041258403923 ) ) ;
#106843 = CARTESIAN_POINT ( 'NONE',  ( 0.7083710243460902278, -2.251296572208848712, 0.2248925466769024495 ) ) ;
#106845 = CARTESIAN_POINT ( 'NONE',  ( -8.286004436246233951, 12.81875560892930466, 1.040834085586084257E-14 ) ) ;
#106847 = CARTESIAN_POINT ( 'NONE',  ( 1.177184062793021679, 1.451467631357589383, 1.250241458713635456 ) ) ;
#106846 = CARTESIAN_POINT ( 'NONE',  ( -4.717874267431199087, 8.448011045404303587, 1.040834085586084257E-14 ) ) ;
#106848 = CARTESIAN_POINT ( 'NONE',  ( -1.364683531250000748, 1.071875000341421247, 0.000000000000000000 ) ) ;
#106849 = CARTESIAN_POINT ( 'NONE',  ( -7.834948825496938163, -9.999999999999994671, -7.720982897393569466 ) ) ;
#106850 = CARTESIAN_POINT ( 'NONE',  ( -1.500000000000008216, 9.000000000000001776, 3.469446951953614189E-15 ) ) ;
#106851 = CARTESIAN_POINT ( 'NONE',  ( 2.648709078547459850, -1.434216206362935564, 0.9578970732360950757 ) ) ;
#106852 = CARTESIAN_POINT ( 'NONE',  ( 5.551137550152489553, 5.441024994791534120, 0.7998128361456352531 ) ) ;
#106853 = TOROIDAL_SURFACE ( 'NONE', #93053, 3.599999999999999201, 0.4999999999999998890 ) ;
#106854 = CARTESIAN_POINT ( 'NONE',  ( 0.4382651835369972826, 0.2938455168926180638, 1.745004787994571593 ) ) ;
#106855 =( BOUNDED_CURVE ( )  B_SPLINE_CURVE ( 2, ( #23090, #69707, #107635, #135811, #88122 ),
 .UNSPECIFIED., .F., .T. ) 
 B_SPLINE_CURVE_WITH_KNOTS ( ( 3, 2, 3 ),
 ( 0.2851912450777800423, 0.2874999999999999778, 0.2888802418687935192 ),
 .UNSPECIFIED. ) 
 CURVE ( )  GEOMETRIC_REPRESENTATION_ITEM ( )  RATIONAL_B_SPLINE_CURVE ( ( 0.9337969725178141278, 0.9257645179683744452, 1.000000000000000000, 0.9556198367076580436, 0.9406422459849084206 ) ) 
 REPRESENTATION_ITEM ( '' )  );
#106856 = CARTESIAN_POINT ( 'NONE',  ( 2.051433223282957297, -1.797157160989469427, 0.9072355583341712437 ) ) ;
#106857 = SURFACE_STYLE_FILL_AREA ( #139319 ) ;
#106858 = CARTESIAN_POINT ( 'NONE',  ( 8.550388431712704573, 13.12720360364021133, 0.000000000000000000 ) ) ;
#106859 = CARTESIAN_POINT ( 'NONE',  ( 4.085166796624926100, -0.2132991444873769959, -2.196430506890618695 ) ) ;
#106860 = EDGE_LOOP ( 'NONE', ( #41450, #131099, #109204, #69129 ) ) ;
#106861 = CARTESIAN_POINT ( 'NONE',  ( 7.849807752188022292, 11.14156422998596696, -1.082531754730543083 ) ) ;
#106862 = CARTESIAN_POINT ( 'NONE',  ( -5.589704470584107909, 9.743348658981940247, -0.7998128361456362523 ) ) ;
#106864 = CARTESIAN_POINT ( 'NONE',  ( 3.972279928656559100, -1.994873972748755442, -0.2930500606010341125 ) ) ;
#106863 = CARTESIAN_POINT ( 'NONE',  ( 4.371814246616528621, 0.4635510597098577712, -2.069045912693792566 ) ) ;
#106866 = ORIENTED_EDGE ( 'NONE', *, *, #45431, .T. ) ;
#106865 = CARTESIAN_POINT ( 'NONE',  ( 3.216879062660949362, 1.425012358211204422, -1.118398921490076026 ) ) ;
#106867 = CARTESIAN_POINT ( 'NONE',  ( 4.376249722160992839, 8.327651452488305850, 0.000000000000000000 ) ) ;
#106868 = ORIENTED_EDGE ( 'NONE', *, *, #191917, .T. ) ;
#106869 = CARTESIAN_POINT ( 'NONE',  ( 1.709613803025863188, -1.856884215550944850, 0.2259493607114013147 ) ) ;
#106870 = STYLED_ITEM ( 'NONE', ( #129639 ), #13191 ) ;
#106871 = CARTESIAN_POINT ( 'NONE',  ( 5.813091150998386247, 1.612263477354998864, 0.8566026058636074803 ) ) ;
#106872 = CARTESIAN_POINT ( 'NONE',  ( -4.451154503988200339, 4.087435097607984957, 1.214306433183764966E-14 ) ) ;
#106873 = DIRECTION ( 'NONE',  ( 0.7592566023653016805, 0.6507913734559627184, 4.115938288792103177E-15 ) ) ;
#106874 =( NAMED_UNIT ( * ) SI_UNIT ( $, .STERADIAN. ) SOLID_ANGLE_UNIT ( ) );
#106875 = CARTESIAN_POINT ( 'NONE',  ( -1.402160292154681736E-14, 1.509375000341420359, -1.575800808251659024 ) ) ;
#106876 = CARTESIAN_POINT ( 'NONE',  ( 2.421437874748389341, 3.696394713403123866, -11.55257195323928876 ) ) ;
#106877 = ORIENTED_EDGE ( 'NONE', *, *, #165849, .F. ) ;
#106878 = B_SPLINE_CURVE_WITH_KNOTS ( 'NONE', 3,
 ( #160527, #77137, #12132, #210328, #179983, #79278, #15319, #191935, #208192, #195168, #161611, #64099, #97680, #95560, #80341, #30542, #31604, #112916, #96622, #43599, #143258, #61966, #196233, #128122, #162676, #163738, #78204, #45735, #145395, #109718, #209247, #178927, #111853, #29469, #13201, #211393, #175723, #63022, #193011, #176778, #14246, #129190, #146441, #94489, #212454, #59825, #125978, #44665, #60891, #110778, #93421, #159458, #127051, #28394, #194082, #52111, #134460, #182084, #81407, #213512, #34774, #83527, #149610, #18525, #1192, #66183, #200464, #49974, #100846, #69394, #48918, #118237, #181038, #147490, #115039, #33715, #132329, #99792, #198334, #197278, #166932, #36909, #84603, #19594, #150691, #116093, #131291, #165859, #184222, #17444, #119300, #2253, #67256, #32654, #68329, #35844, #85667, #199397, #101923, #183170, #117, #102991, #133391, #169049, #98732, #51043, #117166, #65133, #164790, #167989, #151753, #3324, #135501, #201524, #16382, #53172, #185286, #82461, #148551, #205810, #55311, #173343, #136571, #23854, #21698, #89962, #20647, #186357, #120382, #24923, #37993, #22775, #88892, #172267, #154946, #5451, #73685, #203660, #188499, #8678, #202592, #42277, #74760, #140862, #104065, #139783, #86736, #54244, #108391, #91028, #57441, #190619, #156013, #157089, #40131, #71530, #70456, #137641, #123602, #105145, #58507, #170111, #39059, #6530, #72608, #171185, #189567, #107319, #121460, #41212, #87809, #138708, #204724, #152805, #56375, #122538, #153882, #187430, #206876, #106241, #7600, #124662, #4384, #211134, #9747, #94233, #210066, #158154, #13996, #145128, #208995, #46537, #75821, #128918, #96365, #192749, #43344, #44406, #28138, #146182, #111589, #110526, #59563, #80081, #25992, #212197, #141929, #177599, #60631, #77950, #160271, #176526, #62758, #61706, #193824, #11873, #66721, #112658, #194899, #207942, #144071, #127874, #29211, #125723, #109464, #79012, #45473, #95301, #161350, #12931, #191683, #178667, #10802, #126794, #30279, #132864, #50515, #162419, #198868, #174415, #142997, #76876, #175471, #92100, #27057, #93164, #159201, #199945, #186900, #118773, #4919, #19062, #154419, #68868, #70996, #134988, #69930, #202054, #200998, #203138, #169595, #170657, #21177, #54780, #20126, #101392, #103535, #5997, #119847, #117716, #185825, #116638, #67788, #1731, #120927, #133938, #184757, #36384, #53714, #102462, #167466, #100327, #37456, #87280, #153349, #38532, #138178, #104610, #22244, #51592, #137109, #182633, #150163, #204188, #88354, #72068, #34255, #166394, #17985, #136042, #85140, #84075, #183706, #35314, #52643, #86212, #151227, #168528, #152284, #3857, #2796, #92645, #142466, #40681, #10285, #56914, #173894, #124141, #55844, #190103, #140332, #91577, #122000, #143544, #59040, #57978, #26537, #75299, #158687, #105697, #41756, #157629, #39594, #110003, #76359, #90497, #208474, #171724, #60110, #192226, #74239, #106784, #126269, #9227, #43889, #156560, #206351, #155482, #176016, #187966, #27608, #23323, #125198, #8155, #25469, #107868, #141414, #172812, #207421, #93708, #191161, #159748, #11346, #77427, #89431, #42828, #7065, #123087, #108934, #73138, #174955, #139243, #205274, #24384, #189044, #161899, #97971, #13486, #162962, #80638, #79561, #145680, #178144, #49209, #48161, #81692, #113204 ),
 .UNSPECIFIED., .F., .F.,
 ( 4, 1, 1, 1, 1, 1, 1, 1, 1, 1, 1, 1, 1, 1, 1, 1, 1, 1, 1, 1, 1, 1, 1, 1, 1, 1, 1, 1, 1, 1, 1, 1, 1, 1, 1, 1, 1, 1, 1, 1, 1, 1, 1, 1, 1, 1, 1, 1, 1, 1, 1, 1, 1, 1, 1, 1, 1, 1, 1, 1, 1, 1, 1, 1, 1, 1, 1, 1, 1, 1, 1, 1, 1, 1, 1, 1, 1, 1, 1, 1, 1, 1, 1, 1, 1, 1, 1, 1, 1, 1, 1, 1, 1, 1, 1, 1, 1, 1, 1, 1, 1, 1, 1, 1, 1, 1, 1, 1, 1, 1, 1, 1, 1, 1, 1, 1, 1, 1, 1, 1, 1, 1, 1, 1, 1, 1, 1, 1, 1, 1, 1, 1, 1, 1, 1, 1, 1, 1, 1, 1, 1, 1, 1, 1, 1, 1, 1, 1, 1, 1, 1, 1, 1, 1, 1, 1, 1, 1, 1, 1, 1, 1, 1, 1, 1, 1, 1, 1, 1, 1, 1, 1, 1, 1, 1, 1, 1, 1, 1, 1, 1, 1, 1, 1, 1, 1, 1, 1, 1, 1, 1, 1, 1, 1, 1, 1, 1, 1, 1, 1, 1, 1, 1, 1, 1, 1, 1, 1, 1, 1, 1, 1, 1, 1, 1, 1, 1, 1, 1, 1, 1, 1, 1, 1, 1, 1, 1, 1, 1, 1, 1, 1, 1, 1, 1, 1, 1, 1, 1, 1, 1, 1, 1, 1, 1, 1, 1, 1, 1, 1, 1, 1, 1, 1, 1, 1, 1, 1, 1, 1, 1, 1, 1, 1, 1, 1, 1, 1, 1, 1, 1, 1, 1, 1, 1, 1, 1, 1, 1, 1, 1, 1, 1, 1, 1, 1, 1, 1, 1, 1, 1, 1, 1, 1, 1, 1, 1, 1, 1, 1, 1, 1, 1, 1, 1, 1, 1, 1, 1, 1, 1, 1, 1, 1, 1, 1, 1, 1, 1, 1, 1, 1, 1, 1, 1, 1, 1, 1, 1, 1, 1, 1, 1, 1, 1, 1, 1, 1, 1, 1, 1, 1, 1, 1, 1, 1, 1, 1, 1, 1, 1, 1, 1, 1, 1, 1, 1, 1, 1, 1, 1, 1, 1, 1, 1, 1, 1, 1, 1, 1, 1, 1, 1, 1, 1, 1, 1, 1, 1, 1, 1, 1, 1, 1, 4 ),
 ( 0.000000000000000000, 0.002600033395298661284, 0.005208813367820810773, 0.007813200023264601363, 0.01041635779573905213, 0.01302082523971277370, 0.01562491580351430334, 0.01822918961192645723, 0.02083333155136493989, 0.02343746137460561707, 0.02604174567981391505, 0.02864576082122225614, 0.03125012338981237453, 0.03385410379569547823, 0.03645843966640821554, 0.03906250599122108869, 0.04166672065998115043, 0.04427093656960304907, 0.04687500111868234121, 0.04947933663890847350, 0.05208331727515622817, 0.05468767913406928638, 0.05729168951085979872, 0.05989597295159828499, 0.06250011041458469752, 0.06510424634142775169, 0.06770853038940542745, 0.07031253939703428768, 0.07291690072920921362, 0.07552088074063932621, 0.07812521459448035221, 0.08072927904253822395, 0.08333349217322323643, 0.08593770650149938628, 0.08854176936806532061, 0.09114610329512429221, 0.09375008230893774885, 0.09635444258075796797, 0.09895845137230636912, 0.1015627332241899466, 0.1041668691376404637, 0.1067710034717011397, 0.1093752859901425123, 0.1119792934252105548, 0.1145836532378000650, 0.1171876317139315254, 0.1197919640503514460, 0.1223960270027875247, 0.1250002386107842423, 0.1276044514713231270, 0.1302085128224930721, 0.1328128452953424854, 0.1354168228245230532, 0.1380211816480703679, 0.1406251889951717071, 0.1432294693974442978, 0.1458336039016293884, 0.1484377367829480265, 0.1510420179109137340, 0.1536460239143070949, 0.1562503823458506746, 0.1588543594276481397, 0.1614586903853630351, 0.1640627519827278502, 0.1666669622076225599, 0.1692711737400035832, 0.1718752337163205746, 0.1744795648736557347, 0.1770835410591554138, 0.1796878985729436218, 0.1822919046164021839, 0.1848961837081005144, 0.1875003169431251615, 0.1901044485118078553, 0.1927087283883223978, 0.1953127331008320255, 0.1979170902898210183, 0.2005210661182068033, 0.2031253958358791578, 0.2057294562186703923, 0.2083336651999991573, 0.2109378755437518183, 0.2135419342857080849, 0.2161462642661750033, 0.2187502392488957503, 0.2213545955913898966, 0.2239586004719608947, 0.2265628783920732026, 0.2291670104979939837, 0.2317711408940984485, 0.2343754196581391558, 0.2369794232205082452, 0.2395837793053874898, 0.2421877540212369617, 0.2447920826374832270, 0.2473961419461526701, 0.2500003498234057431, 0.2526045591180144934, 0.2552086167660569949, 0.2578129457082574683, 0.2604169196290564980, 0.2630212749386780513, 0.2656252787970727613, 0.2682295556845439854, 0.2708336868013750398, 0.2734378161649161920, 0.2760420939554183439, 0.2786460965083475960, 0.2812504516275206035, 0.2838544253716674404, 0.2864587530250631842, 0.2890628114000217685, 0.2916670183126490179, 0.2942712266975582858, 0.2968752833920936807, 0.2994796114345903981, 0.3020835844342854570, 0.3046879388494173613, 0.3072919418263086455, 0.3098962178200457829, 0.3125003480877632800, 0.3151044765587182606, 0.3177087535145803887, 0.3203127551987332566, 0.3229171094905676220, 0.3255210824038090589, 0.3281254092328941829, 0.3307294668145174810, 0.3333336729019333866, 0.3359378805165532667, 0.3385419363979534357, 0.3411462636792753078, 0.3437502358986498918, 0.3463545895576419231, 0.3489585917936692261, 0.3515628670325462446, 0.3541669965910940188, 0.3567711243094072171, 0.3593754005694961839, 0.3619794015255044517, 0.3645837551283364619, 0.3671877273514386752, 0.3697920534947228832, 0.3723961104233561858, 0.3750003158249449187, 0.3776045228086560845, 0.3802085780172632101, 0.3828129046759103926, 0.3854168762557192984, 0.3880212292968930887, 0.3906252309326675998, 0.3932295055555311003, 0.3958336345448258409, 0.3984377616504144459, 0.4010420373535708016, 0.4036460377220391638, 0.4062503907741795706, 0.4088543624478828686, 0.4114586880438503846, 0.4140627444598136697, 0.4166669493149349202, 0.4192711558070936761, 0.4218752104832254046, 0.4244795366576747386, 0.4270835077386489487, 0.4296878603003031483, 0.4322918614764136302, 0.4348961356220873986, 0.4375002641820237570, 0.4401043908147829753, 0.4427086660998260093, 0.4453126660213379551, 0.4479170186610768045, 0.4505209899261007900, 0.4531253151132156320, 0.4557293711568096706, 0.4583335756048029785, 0.4609377817447468106, 0.4635418360287018591, 0.4661461618574116450, 0.4687501325802634344, 0.4713544848006788190, 0.4739584856576960492, 0.4765627594649867738, 0.4791668877354426925, 0.4817710140352507997, 0.4843752890409837031, 0.4869792886561065681, 0.4895836410217184742, 0.4921876120187673176, 0.4947919369354787933, 0.4973959927469893683, 0.5000001969271801183, 0.5026044028542325792, 0.5052084568862954539, 0.5078127825077110025, 0.5104167530131399344, 0.5130211050305848453, 0.5156251057090676104, 0.5182293793167697116, 0.5208335074376115870, 0.5234376335443351458, 0.5260419084095501185, 0.5286459078588399141, 0.5312502600885893322, 0.5338542309583571566, 0.5364585557431046370, 0.5390626114628084276, 0.5416668155145124564, 0.5442710213679887721, 0.5468750752884355970, 0.5494794008409938924, 0.5520833712696913143, 0.5546877232224267651, 0.5572917238629264691, 0.5598959974098275394, 0.5625001255209155504, 0.5651042515744146844, 0.5677085264378984863, 0.5703125258619060611, 0.5729168780940517847, 0.5755208489772277725, 0.5781251737684461878, 0.5807292295366155432, 0.5833334335991446906, 0.5859376395183565345, 0.5885416934674594369, 0.5911460190895951872, 0.5937499895822500040, 0.5963543416085342885, 0.5989583423516006144, 0.6015626159764864145, 0.6041667442176794633, 0.6067708703578130747, 0.6093751453583519107, 0.6119791448976270587, 0.6145834972704286026, 0.6171874683077025470, 0.6197917932438269384, 0.6223958492007358734, 0.6250000534134032559, 0.6276042595376638555, 0.6302083136556971832, 0.6328126394858472059, 0.6354166101831504321, 0.6380209624212449526, 0.6406249634074311361, 0.6432292372490908683, 0.6458333657602520761, 0.6484374921268833969, 0.6510417674032679125, 0.6536457671983656459, 0.6562501198500874100, 0.6588540911821543222, 0.6614584164016259482, 0.6640624726875546946, 0.6666666771896793131, 0.6692708836583093346, 0.6718749380855545406, 0.6744792642621626477, 0.6770832353048136243, 0.6796875878929879988, 0.6822915892628557133, 0.6848958634600870177, 0.6874999923810890534, 0.6901041191140900866, 0.6927083948051209195, 0.6953123949966061312, 0.6979167480655225075, 0.7005207198330885010, 0.7031250454743595002, 0.7057291022295995031, 0.7083333071605121267, 0.7109375141128444486, 0.7135415689895947544, 0.7161458956511181917, 0.7187498671798290273, 0.7213542202563657524, 0.7239582221504904380, 0.7265624968421051655, 0.7291666263128349090, 0.7317707535520923123, 0.7343750297965853102, 0.7369790305250381035, 0.7395833841494394711, 0.7421873564932268685, 0.7447916826947649227, 0.7473957400596251688, 0.7499999455586733310, 0.7526041531340577073, 0.7552082086006238759, 0.7578125358855373195, 0.7604165080410384414, 0.7630208617442386654, 0.7656248643032155243, 0.7682291396280439555, 0.7708332697884082707, 0.7734373976738285750, 0.7760416746106194585, 0.7786456760166404756, 0.7812500303348380859, 0.7838540033955903041, 0.7864583302958847444, 0.7890623884106959807, 0.7916665946172487534, 0.7942708029550582527, 0.7968748591517740287, 0.7994791871985751364, 0.8020831601216208417, 0.8046875145898089166, 0.8072915179542569097, 0.8098957940511537501, 0.8124999250410844809, 0.8151040537125986418, 0.8177083314805486669, 0.8203123337047645292, 0.8229166888550945025, 0.8255206627735817149, 0.8281249905111484066, 0.8307290495162685806, 0.8333332565697225691, 0.8359374658093579047, 0.8385415228765847884, 0.8411458518237998616, 0.8437498256551729803, 0.8463541810267020127, 0.8489581853372698550, 0.8515624623451190089, 0.8541665943045783083, 0.8567707239021479237, 0.8593750026401490993, 0.8619790058232168484, 0.8645833619440471685, 0.8671873368610717447, 0.8697916655744575287, 0.8723957256102774505, 0.8749999336500613456, 0.8776041439309557601, 0.8802082020090884473, 0.8828125319952765393, 0.8854165068757942070, 0.8880208632890512765, 0.8906248686864229880, 0.8932291467441429988, 0.8958332798131283248, 0.8984374104767501867, 0.9010416903237299380, 0.9036456946063434748, 0.9062500518360779855, 0.9088540278924787108, 0.9114583577202677311, 0.9140624189272162914, 0.9166666280927961985, 0.9192708395544209043, 0.9218748987838942810, 0.9244792299476556341, 0.9270832060181642964, 0.9296875636115721209, 0.9322915702365133228, 0.9348958494830461596, 0.9374999838014769216, 0.9401041156712998115, 0.9427083967663798525, 0.9453124022892170908, 0.9479167607665550666, 0.9505207380999710631, 0.9531250691809918241, 0.9557291317261836783, 0.9583333421310490374, 0.9609375547886240820, 0.9635416155522130710, 0.9661459483928183101, 0.9687499245033458495, 0.9713542829945021051, 0.9739582954330652242, 0.9765625745907361432, 0.9791667024412501474, 0.9817708385604039245, 0.9843751096149007118, 0.9869791944699233266, 0.9895836584107432499, 0.9921868132917668337, 0.9947911946869415489, 0.9973999724172807335, 1.000000000000000000 ),
 .UNSPECIFIED. ) ;
#106879 = CARTESIAN_POINT ( 'NONE',  ( 7.200788982633824276, 7.573544365927161515, 0.000000000000000000 ) ) ;
#106880 = CARTESIAN_POINT ( 'NONE',  ( -4.719646871332968452, 5.639247783710797712, 1.082531754730549078 ) ) ;
#106881 = EDGE_CURVE ( 'NONE', #19175, #54861, #96681, .T. ) ;
#106882 = CARTESIAN_POINT ( 'NONE',  ( -6.473091995881817162, 6.516638514809040217, 0.7998128361456281477 ) ) ;
#106883 = CARTESIAN_POINT ( 'NONE',  ( 3.885109016898562029, -1.979880364965879380, -0.7601140796509860964 ) ) ;
#106885 = CARTESIAN_POINT ( 'NONE',  ( -10.88575987782614796, 5.812703298851592315, -6.395352192321499984 ) ) ;
#106884 = CARTESIAN_POINT ( 'NONE',  ( -0.02948999725182251466, 1.364966664109868555, -2.179895196203474050 ) ) ;
#106886 = CARTESIAN_POINT ( 'NONE',  ( 5.167239647397361857, 0.1962102620695851674, -1.961592271633934903 ) ) ;
#106887 = CARTESIAN_POINT ( 'NONE',  ( 0.6823417656249899377, 1.092708333674752286, 1.181850606188755259 ) ) ;
#106888 = VERTEX_POINT ( 'NONE', #54764 ) ;
#106889 = CARTESIAN_POINT ( 'NONE',  ( 0.4216853220532343904, -1.500587716210170841, -1.493872543894637417 ) ) ;
#106890 = CARTESIAN_POINT ( 'NONE',  ( 8.361447513987284808, 14.02696274858952030, 8.607981746264741219 ) ) ;
#106891 = CARTESIAN_POINT ( 'NONE',  ( 1.012269475826784060, 2.068064858651061932, -0.09981174449213289779 ) ) ;
#106892 = CARTESIAN_POINT ( 'NONE',  ( 6.099189001301251523, 8.209082816308541197, 1.599625672291268286 ) ) ;
#106893 = ORIENTED_EDGE ( 'NONE', *, *, #61884, .F. ) ;
#106894 = CARTESIAN_POINT ( 'NONE',  ( 4.960304097753311936, 6.880383762169266504, 1.599625672291268286 ) ) ;
#106895 = CARTESIAN_POINT ( 'NONE',  ( 4.376249722160992839, 8.327651452488305850, 0.000000000000000000 ) ) ;
#106897 = CARTESIAN_POINT ( 'NONE',  ( 4.761938266897790761, 6.578680616179308771, 1.599625672291267398 ) ) ;
#106896 = CARTESIAN_POINT ( 'NONE',  ( 3.416043810090535260, 1.326132273491455349, -1.616208110139333742 ) ) ;
#106898 = CARTESIAN_POINT ( 'NONE',  ( 6.821687566331318564, 7.987665577921906568, 1.199719254218452935 ) ) ;
#106901 = EDGE_LOOP ( 'NONE', ( #143646, #80265, #189458, #30687 ) ) ;
#106900 = CARTESIAN_POINT ( 'NONE',  ( 1.734716041023535160, 1.690356777636679686, 0.6517371015684128022 ) ) ;
#106899 = CARTESIAN_POINT ( 'NONE',  ( 2.432394421669949569, 1.770131964307398498, 0.4459858026567494194 ) ) ;
#106902 = CARTESIAN_POINT ( 'NONE',  ( 5.654950187766193181, -1.741821662664808645, 1.355018943897445149 ) ) ;
#106903 = AXIS2_PLACEMENT_3D ( 'NONE', #70979, #116622, #182615 ) ;
#106904 = CARTESIAN_POINT ( 'NONE',  ( 1.387358672531572079, 7.315968950354051259, 4.254625267138675504 ) ) ;
#106905 = CARTESIAN_POINT ( 'NONE',  ( 3.856632026064894525, 0.7917978285330304900, 2.060012427959257764 ) ) ;
#106906 = CARTESIAN_POINT ( 'NONE',  ( 7.365103760721646076, 9.615707025640515937, 1.599625672291281386 ) ) ;
#106907 = CARTESIAN_POINT ( 'NONE',  ( -11.78331023100045627, 12.29999999999998295, 1.799999999999999600 ) ) ;
#106908 = EDGE_CURVE ( 'NONE', #42950, #176800, #178047, .T. ) ;
#106909 = CARTESIAN_POINT ( 'NONE',  ( 2.807167725247063483, 1.639017566557477990, -0.9848878580655600068 ) ) ;
#106910 = CARTESIAN_POINT ( 'NONE',  ( 9.759171643738394408, 10.28012176064996197, 0.000000000000000000 ) ) ;
#106911 = CARTESIAN_POINT ( 'NONE',  ( 4.932118098221458524, 1.189261692661430114, 1.694535115018414917 ) ) ;
#106913 = CARTESIAN_POINT ( 'NONE',  ( 1.808247988047292143, 2.517446015412736493, 2.499984125739858065 ) ) ;
#106912 = CARTESIAN_POINT ( 'NONE',  ( 0.000000000000000000, -6.134628647623513231, 10.91970695577495931 ) ) ;
#106914 = CARTESIAN_POINT ( 'NONE',  ( 6.321842903100939104, 1.263506803105146847, -1.790488031206059372 ) ) ;
#106915 = VERTEX_POINT ( 'NONE', #79287 ) ;
#106916 = ORIENTED_EDGE ( 'NONE', *, *, #151300, .T. ) ;
#106917 = AXIS2_PLACEMENT_3D ( 'NONE', #117007, #164636, #85509 ) ;
#106918 = CARTESIAN_POINT ( 'NONE',  ( 0.3866926556111174862, 2.897682894409570054, 2.027578619373079594 ) ) ;
#106919 = CARTESIAN_POINT ( 'NONE',  ( 3.576318658954677598, 7.394398545414291313, 0.7998128361456281477 ) ) ;
#106920 = CARTESIAN_POINT ( 'NONE',  ( 3.285556943750000070, -1.421874999522041660, 0.000000000000000000 ) ) ;
#106921 =( NAMED_UNIT ( * ) PLANE_ANGLE_UNIT ( ) SI_UNIT ( $, .RADIAN. ) );
#106922 = CARTESIAN_POINT ( 'NONE',  ( -7.483737605063437215, 10.71448239167390604, 1.082531754730549967 ) ) ;
#106923 = CARTESIAN_POINT ( 'NONE',  ( 3.237364818613055473, 6.998952398349030268, -1.734723475976807094E-15 ) ) ;
#106924 = CARTESIAN_POINT ( 'NONE',  ( 5.295788417638883416, -1.460108768623759712, -1.467927865959644862 ) ) ;
#106925 = CARTESIAN_POINT ( 'NONE',  ( 4.301339506872517759, 1.548173799611574530, 1.146357790588454106 ) ) ;
#106926 = CARTESIAN_POINT ( 'NONE',  ( 0.03478015955125923070, -1.617804660175032661, 1.203375172262765913 ) ) ;
#106927 = CARTESIAN_POINT ( 'NONE',  ( -4.889337272013151825, 4.909234758358784312, -0.4031905389056227307 ) ) ;
#106928 = CARTESIAN_POINT ( 'NONE',  ( 5.481239241674765950, 9.616805891921051952, -0.7998128361456481317 ) ) ;
#106930 = EDGE_CURVE ( 'NONE', #95637, #190177, #20339, .T. ) ;
#106929 = DIRECTION ( 'NONE',  ( 1.000000000000000000, 0.000000000000000000, 0.000000000000000000 ) ) ;
#106931 = CARTESIAN_POINT ( 'NONE',  ( 0.7971425760184660536, 1.793611693402120455, 1.258865353619270433 ) ) ;
#106932 = CARTESIAN_POINT ( 'NONE',  ( 4.916531288042031989, 1.256637652550334883, -1.324621001416517840 ) ) ;
#106933 = EDGE_CURVE ( 'NONE', #148211, #92970, #209011, .T. ) ;
#106934 = CARTESIAN_POINT ( 'NONE',  ( 5.017926250833595780, 7.907978821730911712, -1.082531754730548412 ) ) ;
#106935 = CARTESIAN_POINT ( 'NONE',  ( 8.561083932025322696, 12.07534945641652158, -1.199719254218446718 ) ) ;
#106936 = CARTESIAN_POINT ( 'NONE',  ( -6.954406449166956605, 7.078172043641714595, -0.7998128361456362523 ) ) ;
#106937 = CARTESIAN_POINT ( 'NONE',  ( 4.761938266897790761, 6.578680616179308771, 1.599625672291267398 ) ) ;
#106938 = CARTESIAN_POINT ( 'NONE',  ( 4.016958651398847557, 7.908478536599129249, -0.7998128361456362523 ) ) ;
#106939 = ORIENTED_EDGE ( 'NONE', *, *, #171579, .F. ) ;
#106941 = CARTESIAN_POINT ( 'NONE',  ( 5.994395146102541538, -1.073393154543872852, 1.702996195706570681 ) ) ;
#106940 = CARTESIAN_POINT ( 'NONE',  ( 2.770863647982471534, 1.747605724785822767, -0.5798694457997202178 ) ) ;
#106942 = CARTESIAN_POINT ( 'NONE',  ( 1.740083653633100580, -2.182622149841602521, -0.7203450084119922270 ) ) ;
#106943 = CARTESIAN_POINT ( 'NONE',  ( 6.631700630569578259, 1.878258136613653040, -0.5663492180864730940 ) ) ;
#106944 = CARTESIAN_POINT ( 'NONE',  ( -4.608882153641705059, 7.464447381635583412, -1.199719254218452047 ) ) ;
#106945 = CARTESIAN_POINT ( 'NONE',  ( -6.903494779225470168, -6.732807188596399151, 6.688963559358022337 ) ) ;
#106946 = CARTESIAN_POINT ( 'NONE',  ( -3.216308754939891212, 4.775446185561722956, -1.599625672291262513 ) ) ;
#106947 = DIRECTION ( 'NONE',  ( 8.659560562354967371E-17, 0.7071067811865445751, -0.7071067811865504593 ) ) ;
#106948 = CARTESIAN_POINT ( 'NONE',  ( -7.946487431385463651, 8.443525889470736345, 0.7216878364870317197 ) ) ;
#106950 = CARTESIAN_POINT ( 'NONE',  ( 1.270139834521961886, -1.189467451172643964, 1.443775233441677130 ) ) ;
#106949 = CARTESIAN_POINT ( 'NONE',  ( 2.612926333352751929, -0.2020284733853395243, 2.080942194061443651 ) ) ;
#106951 = CARTESIAN_POINT ( 'NONE',  ( 1.563827143785265328, 1.649830188709809686, -1.158509706484150970 ) ) ;
#106952 = CARTESIAN_POINT ( 'NONE',  ( 6.792271770766432404, 10.86814146596211472, 1.040834085586084257E-14 ) ) ;
#106953 = CARTESIAN_POINT ( 'NONE',  ( 1.364683531249990311, 4.446875000341417028, 1.214306433183764966E-14 ) ) ;
#106954 = CARTESIAN_POINT ( 'NONE',  ( 2.401564422585287684, -0.6675299454344629790, -1.607540830017651023 ) ) ;
#106955 = CARTESIAN_POINT ( 'NONE',  ( 5.124091990960999432, 8.065525525174782828, -1.199719254218452047 ) ) ;
#106957 = DIRECTION ( 'NONE',  ( 0.000000000000000000, 0.000000000000000000, -1.000000000000000000 ) ) ;
#106956 = LINE ( 'NONE', #172981, #86028 ) ;
#106958 = CARTESIAN_POINT ( 'NONE',  ( 2.420142186669431705, 1.127438667474765621, -1.305497878543178336 ) ) ;
#106959 = CARTESIAN_POINT ( 'NONE',  ( 2.384552795368581890, -0.3778730364575392797, -2.158588602542845347 ) ) ;
#106960 = CARTESIAN_POINT ( 'NONE',  ( 5.197975494389605267, -0.7968864405506062010, 2.058166701804148957 ) ) ;
#106961 = CARTESIAN_POINT ( 'NONE',  ( -9.979823206198361163, 5.589814398814591634, -5.978750339097100408 ) ) ;
#106962 = STYLED_ITEM ( 'NONE', ( #184660 ), #213132 ) ;
#106963 = CARTESIAN_POINT ( 'NONE',  ( 2.887734989934476193, -2.027295339332426227, 0.7774125151447373039 ) ) ;
#106964 = CARTESIAN_POINT ( 'NONE',  ( 0.5569169099325711469, -1.540613122784354916, -0.9793164655157863274 ) ) ;
#106965 = CARTESIAN_POINT ( 'NONE',  ( 4.329393036353162749, -1.639139883998712799, -1.340335314225228780 ) ) ;
#106966 = CARTESIAN_POINT ( 'NONE',  ( 6.539320575229279342, 6.038407674219216759, 2.491644695858772796 ) ) ;
#106967 = ORIENTED_EDGE ( 'NONE', *, *, #175034, .T. ) ;
#106969 = CARTESIAN_POINT ( 'NONE',  ( -0.6823417656250212460, 0.8635416670080899859, 1.181850606188755259 ) ) ;
#106968 = CARTESIAN_POINT ( 'NONE',  ( 4.792671637142519536, 1.906707348304257366, -1.272296631038958070 ) ) ;
#106970 = CARTESIAN_POINT ( 'NONE',  ( 6.827182134110238998, -0.009824402486291110986, 2.288967694407703313 ) ) ;
#106971 = CARTESIAN_POINT ( 'NONE',  ( 4.273844736805816780, 6.009238164405336313, 1.599625672291267398 ) ) ;
#106972 = CARTESIAN_POINT ( 'NONE',  ( 0.8211285067932658777, 1.603129840700336706, -1.388046135824993366 ) ) ;
#106973 = CARTESIAN_POINT ( 'NONE',  ( -6.263503779833496488, 6.409768619334935913, 0.7216878364870317197 ) ) ;
#106974 = CARTESIAN_POINT ( 'NONE',  ( 5.192409644353875642, 5.160158794608717514, 1.040834085586084257E-14 ) ) ;
#106975 = CARTESIAN_POINT ( 'NONE',  ( -7.199016378732087773, 7.501199984716642177, 0.7216878364870317197 ) ) ;
#106976 = CARTESIAN_POINT ( 'NONE',  ( 4.760321332173959696, 4.726332107057286791, 0.000000000000000000 ) ) ;
#106977 = EDGE_LOOP ( 'NONE', ( #37017, #138031, #132027, #57959 ) ) ;
#106978 = CARTESIAN_POINT ( 'NONE',  ( 4.746720300533005421, 1.994071680685698400, -0.2986252114312442640 ) ) ;
#106980 = CARTESIAN_POINT ( 'NONE',  ( 3.731348124473393479, 0.05553323764710679095, -2.061997793915891553 ) ) ;
#106979 = CARTESIAN_POINT ( 'NONE',  ( 5.820528018968444961, 5.685037531751635953, 0.7998128361456341429 ) ) ;
#106982 = CARTESIAN_POINT ( 'NONE',  ( -0.1409997244346088141, 4.088373444016307978, -2.555100908668860082 ) ) ;
#106981 = CARTESIAN_POINT ( 'NONE',  ( 1.907519672996849103, 3.236073672982398008, 0.4612874649729346022 ) ) ;
#106983 = CARTESIAN_POINT ( 'NONE',  ( 6.016786309414542622, 10.24161080428416426, 0.7998128361456341429 ) ) ;
#106984 = CARTESIAN_POINT ( 'NONE',  ( 3.285556943749998737, -3.755208332855373587, -1.896917185911906500 ) ) ;
#106985 = CARTESIAN_POINT ( 'NONE',  ( -15.75000000000000000, 10.19999999999998153, 3.199999999999997957 ) ) ;
#106986 = CARTESIAN_POINT ( 'NONE',  ( 5.648420989521034663, -1.729380818958951460, 1.345873388983606533 ) ) ;
#106987 = CARTESIAN_POINT ( 'NONE',  ( 3.533827422916273164, -1.646839391163470223, 1.163268690995450383 ) ) ;
#106988 = CARTESIAN_POINT ( 'NONE',  ( 3.544333174469185721, -1.503253232081468216, 1.062929765333266108 ) ) ;
#106989 = CARTESIAN_POINT ( 'NONE',  ( 6.551614543901692400, 8.666636272683888365, 1.599625672291281386 ) ) ;
#106990 = CARTESIAN_POINT ( 'NONE',  ( 6.510779352739587189, 1.350450193652263930, -1.228632259304612839 ) ) ;
#106991 = CARTESIAN_POINT ( 'NONE',  ( 0.2296305240335142495, 2.293118238291039113, 0.1608910274224564507 ) ) ;
#106992 = CARTESIAN_POINT ( 'NONE',  ( -5.716734326456539783, 9.821273814174633188, -0.7998128361456231517 ) ) ;
#106993 = CARTESIAN_POINT ( 'NONE',  ( 6.297788943421148922, -0.7692995465161235336, 2.127847719713715335 ) ) ;
#106994 = CARTESIAN_POINT ( 'NONE',  ( 2.350341522438728514, 2.105628791459000393, 0.05071553880554508648 ) ) ;
#106995 = CARTESIAN_POINT ( 'NONE',  ( -6.473091995881817162, 6.516638514809040217, 0.7998128361456281477 ) ) ;
#106996 = CARTESIAN_POINT ( 'NONE',  ( 5.940443861082012944, 10.08226827123770697, 0.7998128361456462443 ) ) ;
#106997 = CARTESIAN_POINT ( 'NONE',  ( 7.200788982189461507, 8.533913579710086239, -1.082531754730548412 ) ) ;
#106998 = DIRECTION ( 'NONE',  ( -2.081668171172168513E-16, 3.906259695683824168E-18, -1.000000000000000000 ) ) ;
#106999 = CARTESIAN_POINT ( 'NONE',  ( -7.413611068574208041, 7.543634422958360730, 0.7998128361456341429 ) ) ;
#107000 = CARTESIAN_POINT ( 'NONE',  ( 7.334597914868727919, 9.580116872145431728, -1.443375672974058777 ) ) ;
#107001 = CARTESIAN_POINT ( 'NONE',  ( 4.081185262901700028, 7.719248740676039056, 0.6171906885068592086 ) ) ;
#107002 = CARTESIAN_POINT ( 'NONE',  ( -6.274726165026268454, 6.214935368819085149, 0.7998128361456341429 ) ) ;
#107003 = CARTESIAN_POINT ( 'NONE',  ( 4.131244869123442243, 2.031816273447330623, 0.8983479855831574268 ) ) ;
#107004 = CARTESIAN_POINT ( 'NONE',  ( 2.660326705311684581, -1.510451929809487170, 1.587989696798755235 ) ) ;
#107005 = CARTESIAN_POINT ( 'NONE',  ( 0.6982365061397632910, -0.7907169553198112322, 2.060542492664858560 ) ) ;
#107007 = COLOUR_RGB ( '', 0.09019608, 0.27058824, 0.51372549) ;
#107006 = CARTESIAN_POINT ( 'NONE',  ( -5.093022980588950865, 5.970890227889075419, -1.199719254218453823 ) ) ;
#107008 = CARTESIAN_POINT ( 'NONE',  ( 4.844172697165038066, -0.9265620464425131653, 1.729294158640543699 ) ) ;
#107009 = CARTESIAN_POINT ( 'NONE',  ( 7.892817981449907982, 12.36003807833360391, 0.7998128361456462443 ) ) ;
#107010 = DIRECTION ( 'NONE',  ( 0.7592566023653005702, -0.6507913734559639396, 0.000000000000000000 ) ) ;
#107011 = CARTESIAN_POINT ( 'NONE',  ( -1.201851678989727383E-14, 1.071875000341418138, 1.575800808251672791 ) ) ;
#107012 = CARTESIAN_POINT ( 'NONE',  ( 6.610000000000006537, 0.002781820520842553934, 2.000159646111852929 ) ) ;
#107014 = EDGE_LOOP ( 'NONE', ( #160259, #71249, #22437, #70535 ) ) ;
#107013 = CARTESIAN_POINT ( 'NONE',  ( -6.778713617152821058, 7.971215977175476475, 1.082531754730549967 ) ) ;
#107015 = CARTESIAN_POINT ( 'NONE',  ( 3.322626870553476941, -0.8629183168706102691, -1.937285153019531414 ) ) ;
#107016 = CARTESIAN_POINT ( 'NONE',  ( -4.228163802615396705, 6.026220084508304708, -1.599625672291271394 ) ) ;
#107017 = CARTESIAN_POINT ( 'NONE',  ( 5.770447993230207295, -1.374857387916775364, 1.668144713590607120 ) ) ;
#107018 = CARTESIAN_POINT ( 'NONE',  ( 3.579498943475650563, -0.9044721095569520086, 1.603693017070174864 ) ) ;
#107019 = CARTESIAN_POINT ( 'NONE',  ( -5.752954180755987856, 6.096397935365156506, 0.6526304460669953844 ) ) ;
#107020 = CARTESIAN_POINT ( 'NONE',  ( 1.364683531249986537, 1.217708333674754950, -0.7879004041258239610 ) ) ;
#107021 = CARTESIAN_POINT ( 'NONE',  ( 6.650362500428334656, -1.339898832705511911, 1.110426912289312451 ) ) ;
#107022 = CARTESIAN_POINT ( 'NONE',  ( 6.827182134110219458, 2.993868409037139688, 2.165198344177218903 ) ) ;
#107023 = CARTESIAN_POINT ( 'NONE',  ( 4.365362273920252889, 4.195270195769483124, 0.7216878364870317197 ) ) ;
#107024 = CARTESIAN_POINT ( 'NONE',  ( 11.87716655177446157, 6.749247459756340994, -1.730190197624842829 ) ) ;
#107025 = CARTESIAN_POINT ( 'NONE',  ( 4.030267251519312310, 1.158562084521784108, -1.824840551714689507 ) ) ;
#107026 = VECTOR ( 'NONE', #1000, 1000.000000000000000 ) ;
#107027 = CARTESIAN_POINT ( 'NONE',  ( -4.249591082879585535, 7.045274465746411252, 1.199719254218464037 ) ) ;
#107028 = CARTESIAN_POINT ( 'NONE',  ( 5.360703810585087048, -0.7282664037663032497, 1.880147357087233129 ) ) ;
#107029 = CARTESIAN_POINT ( 'NONE',  ( -6.819388077549415783, 10.89977715720891815, 0.7216878364870458196 ) ) ;
#107030 = CARTESIAN_POINT ( 'NONE',  ( 3.292016909520224743, -0.8776455207864016783, 1.975710135277891633 ) ) ;
#107031 = CARTESIAN_POINT ( 'NONE',  ( 3.180892574772069992, -0.1416633064414400678, -1.966302885814166013 ) ) ;
#107032 = CARTESIAN_POINT ( 'NONE',  ( -15.75000000000000000, 10.90000000000000036, -3.600000000000002309 ) ) ;
#107033 = CARTESIAN_POINT ( 'NONE',  ( 0.5875216112017033199, -0.2866185507822028855, -2.289643093864159429 ) ) ;
#107034 = CARTESIAN_POINT ( 'NONE',  ( 3.233719155016498092, -1.381502681103630392, -1.529336839808728365 ) ) ;
#107035 = CARTESIAN_POINT ( 'NONE',  ( 5.372584366608633921, -0.05174306282297027465, -1.941541108160367513 ) ) ;
#107037 = VERTEX_POINT ( 'NONE', #12143 ) ;
#107036 = CARTESIAN_POINT ( 'NONE',  ( -6.670248387799091461, 10.72578085250020585, 0.000000000000000000 ) ) ;
#107038 = CARTESIAN_POINT ( 'NONE',  ( -6.200875153403786477, 8.327716660428123419, -1.599625672291271394 ) ) ;
#107039 =( LENGTH_UNIT ( ) NAMED_UNIT ( * ) SI_UNIT ( .MILLI., .METRE. ) );
#107040 = ORIENTED_EDGE ( 'NONE', *, *, #58752, .F. ) ;
#107041 = CARTESIAN_POINT ( 'NONE',  ( -7.009202228140751778, 9.200488570962775725, -1.443375672974058777 ) ) ;
#107042 = CARTESIAN_POINT ( 'NONE',  ( 2.362605853119781774, 0.9431403173822919817, 1.995201469058570432 ) ) ;
#107043 = CARTESIAN_POINT ( 'NONE',  ( 0.000000000000000000, -4.134374999522041350, -3.793834371823813001 ) ) ;
#107044 = ORIENTED_EDGE ( 'NONE', *, *, #18201, .T. ) ;
#107045 = CARTESIAN_POINT ( 'NONE',  ( 0.4966286816309881114, 0.3102001241638470685, 1.834739031104109408 ) ) ;
#107046 =( BOUNDED_CURVE ( )  B_SPLINE_CURVE ( 2, ( #7187, #189162, #75418, #109050, #73259 ),
 .UNSPECIFIED., .F., .T. ) 
 B_SPLINE_CURVE_WITH_KNOTS ( ( 3, 2, 3 ),
 ( 0.1312500000637053799, 0.1333333333333333315, 0.1375000000000000111 ),
 .UNSPECIFIED. ) 
 CURVE ( )  GEOMETRIC_REPRESENTATION_ITEM ( )  RATIONAL_B_SPLINE_CURVE ( ( 0.9330127018922194093, 0.9330127039405957667, 1.000000000000000000, 0.8660254037844387076, 1.000000000000000000 ) ) 
 REPRESENTATION_ITEM ( '' )  );
#107047 = CARTESIAN_POINT ( 'NONE',  ( -0.02919842301646497981, 2.009414862388910983, -2.487882213790572283 ) ) ;
#107048 = CARTESIAN_POINT ( 'NONE',  ( -0.7500000000000215383, 4.972916667349482012, 1.299038105676671107 ) ) ;
#107049 = CARTESIAN_POINT ( 'NONE',  ( 4.184706906298553797, 7.590773377710720915, -0.8858016571234141878 ) ) ;
#107051 = CARTESIAN_POINT ( 'NONE',  ( 0.7500000000000006661, 12.61458333401613352, 1.299038105676657340 ) ) ;
#107050 = CARTESIAN_POINT ( 'NONE',  ( -6.567035442730039030, 6.789466400107097677, -0.3981859287331638297 ) ) ;
#107052 = CARTESIAN_POINT ( 'NONE',  ( 5.806566994037906326, 1.625791660643903791, 0.8640615347050364381 ) ) ;
#107053 = ORIENTED_EDGE ( 'NONE', *, *, #96162, .T. ) ;
#107054 = CARTESIAN_POINT ( 'NONE',  ( 1.938423425814293388, 2.038317423364948588, 0.3033609537064930750 ) ) ;
#107055 = CARTESIAN_POINT ( 'NONE',  ( -5.758872628492444169E-14, 0.4531250003414521998, 1.570758158831760287 ) ) ;
#107056 = B_SPLINE_CURVE_WITH_KNOTS ( 'NONE', 3,
 ( #30164, #62649, #148192, #147130 ),
 .UNSPECIFIED., .F., .F.,
 ( 4, 4 ),
 ( 0.000000000000000000, 6.033646489354524308E-05 ),
 .UNSPECIFIED. ) ;
#107057 = CARTESIAN_POINT ( 'NONE',  ( -7.369020184227459858, 8.555943955475521889, 1.199719254218450271 ) ) ;
#107058 = DIRECTION ( 'NONE',  ( -0.000000000000000000, -1.000000000000000000, -0.000000000000000000 ) ) ;
#107059 = SURFACE_SIDE_STYLE ('',( #186101 ) ) ;
#107060 = CARTESIAN_POINT ( 'NONE',  ( 4.147904930777053245, 6.926640621626830807, -1.199719254218452047 ) ) ;
#107061 = ADVANCED_FACE ( 'NONE', ( #47886 ), #52363, .F. ) ;
#107062 = CARTESIAN_POINT ( 'NONE',  ( 1.200152769736504421, -2.061077815970461025, -0.0008511993763692102862 ) ) ;
#107064 = CARTESIAN_POINT ( 'NONE',  ( 4.528748383445759806, -1.681502307688139908, 0.7506017836093890061 ) ) ;
#107063 = DIRECTION ( 'NONE',  ( 0.7592566023652989049, 0.6507913734559658270, 0.000000000000000000 ) ) ;
#107065 = CARTESIAN_POINT ( 'NONE',  ( 6.283314124929436417, 9.417951348137970413, -1.199719254218440723 ) ) ;
#107066 = CARTESIAN_POINT ( 'NONE',  ( -5.336015975430226099, 8.383046517047350932, -1.199719254218453823 ) ) ;
#107068 = ORIENTED_EDGE ( 'NONE', *, *, #11886, .T. ) ;
#107067 = CARTESIAN_POINT ( 'NONE',  ( -0.2409995289980246813, 5.721856934700204178, -2.594540323675114113 ) ) ;
#107069 = CARTESIAN_POINT ( 'NONE',  ( 4.793709216081707858, 1.633822259641436903, 1.483752339651790653 ) ) ;
#107070 = CARTESIAN_POINT ( 'NONE',  ( 0.7554163591718568993, -1.825703804718967316, -1.157005318491082901 ) ) ;
#107071 = CARTESIAN_POINT ( 'NONE',  ( 3.696500153570709379, 1.422608671726926177, -1.429447704489300364 ) ) ;
#107072 = MECHANICAL_DESIGN_GEOMETRIC_PRESENTATION_REPRESENTATION (  '', ( #2753 ), #41329 ) ;
#107073 = CARTESIAN_POINT ( 'NONE',  ( -5.504247177468192476, 7.444707678511436555, 1.443375672974064550 ) ) ;
#107074 = CARTESIAN_POINT ( 'NONE',  ( -0.1229892814952095459, -1.709044814581164973, -0.8582256167319823881 ) ) ;
#107075 = CARTESIAN_POINT ( 'NONE',  ( 1.077361674225948418, 1.530160568918725872, 1.313541346884481209 ) ) ;
#107076 = EDGE_CURVE ( 'NONE', #205543, #161998, #41097, .T. ) ;
#107077 = CARTESIAN_POINT ( 'NONE',  ( 7.648208051440442468, 8.095533279534887328, 0.000000000000000000 ) ) ;
#107078 = AXIS2_PLACEMENT_3D ( 'NONE', #209593, #176069, #78547 ) ;
#107079 = CARTESIAN_POINT ( 'NONE',  ( 0.07536363704235481131, 0.6997989235110781969, -2.226667633679416447 ) ) ;
#107080 = ADVANCED_FACE ( 'NONE', ( #163750 ), #149621, .T. ) ;
#107081 = CARTESIAN_POINT ( 'NONE',  ( 6.516268831907007453, -1.911747763583053317, 0.05203757306279645223 ) ) ;
#107082 = CARTESIAN_POINT ( 'NONE',  ( 0.000000000000000000, 6.499999999999999112, 0.000000000000000000 ) ) ;
#107083 = CARTESIAN_POINT ( 'NONE',  ( 0.2857447052702493662, -0.8859512962964136706, 1.647562673099879138 ) ) ;
#107084 = CARTESIAN_POINT ( 'NONE',  ( 2.729704159269104924, 0.7212915320151757070, -1.883313052590728454 ) ) ;
#107086 = CARTESIAN_POINT ( 'NONE',  ( -4.671932466396476968, 7.377723763423310821, 1.128687292116478114 ) ) ;
#107085 = CARTESIAN_POINT ( 'NONE',  ( -1.364683531250012516, 1.030208333674754062, 0.7879004041258379498 ) ) ;
#107088 = CARTESIAN_POINT ( 'NONE',  ( 4.319037722229518650, 1.925386421186209507, 0.8538897750212376403 ) ) ;
#107087 = CARTESIAN_POINT ( 'NONE',  ( -8.259941899223614215, 10.65968485389279508, -1.599625672291263179 ) ) ;
#107089 = CARTESIAN_POINT ( 'NONE',  ( 6.934105498385400246, 10.17720795050327354, -1.199719254218441611 ) ) ;
#107091 = CARTESIAN_POINT ( 'NONE',  ( -7.181014916732457287, 11.52960116949655678, -0.7998128361456291469 ) ) ;
#107090 = CARTESIAN_POINT ( 'NONE',  ( 5.435893244436359240, 5.306573304789342416, -0.7998128361456481317 ) ) ;
#107092 = CARTESIAN_POINT ( 'NONE',  ( -0.05097232478516647985, -6.890735599540036560, -9.605899910213521409 ) ) ;
#107093 = CARTESIAN_POINT ( 'NONE',  ( 4.447524238883529435, -1.845004865869297905, 0.8223427699834483517 ) ) ;
#107094 = CARTESIAN_POINT ( 'NONE',  ( 1.364683531249990311, 4.884375000341417916, 1.214306433183764966E-14 ) ) ;
#107095 = CARTESIAN_POINT ( 'NONE',  ( 8.093854517678360949, 12.38665467069271386, 1.040834085586084257E-14 ) ) ;
#107096 = CARTESIAN_POINT ( 'NONE',  ( 4.833375328034618335, -1.978455579520097762, 0.8711445904842631816 ) ) ;
#107097 = CARTESIAN_POINT ( 'NONE',  ( 5.742760583840166966, 8.857581893525663830, 1.199719254218452047 ) ) ;
#107098 = CARTESIAN_POINT ( 'NONE',  ( 1.364683531249986537, -0.03229166632525094088, -0.7879004041258309554 ) ) ;
#107100 =( LENGTH_UNIT ( ) NAMED_UNIT ( * ) SI_UNIT ( .MILLI., .METRE. ) );
#107099 = CARTESIAN_POINT ( 'NONE',  ( 5.722423353419669567, 8.833855124701747386, 1.199719254218451159 ) ) ;
#107101 = CARTESIAN_POINT ( 'NONE',  ( 7.904040366642684390, 11.20483561351640844, 1.082531754730558626 ) ) ;
#107103 = CARTESIAN_POINT ( 'NONE',  ( -6.735605996566196296E-15, -8.407420853759283830, 10.91970695577496286 ) ) ;
#107102 = CARTESIAN_POINT ( 'NONE',  ( 1.715514515588032030, -1.861668902569445283, -1.117036959414873465 ) ) ;
#107105 = CARTESIAN_POINT ( 'NONE',  ( 0.9953642579336658969, -1.841430844361633845, 2.783310008858119066E-05 ) ) ;
#107104 = CARTESIAN_POINT ( 'NONE',  ( -5.802526556968872207, 6.832331073627524454, 1.082531754730548412 ) ) ;
#107106 = CARTESIAN_POINT ( 'NONE',  ( 0.6823417656249882723, 1.926041667008083991, -1.181850606188749264 ) ) ;
#107107 = CARTESIAN_POINT ( 'NONE',  ( 3.263397454411249399, 2.137687552337414587, -0.4822058812353549606 ) ) ;
#107108 = CARTESIAN_POINT ( 'NONE',  ( -0.3617799047494653641, -7.723163706540470130, 10.97113338213672407 ) ) ;
#107109 = CARTESIAN_POINT ( 'NONE',  ( 3.538171838403024516, 1.019457259465136101, -2.019903332531754803 ) ) ;
#107110 = CARTESIAN_POINT ( 'NONE',  ( -7.206322340863467346, 8.366129804884193888, 1.199719254218450271 ) ) ;
#107111 = CARTESIAN_POINT ( 'NONE',  ( -0.6823417656249969321, 4.780208333674755394, -1.181850606188749264 ) ) ;
#107112 = CARTESIAN_POINT ( 'NONE',  ( 6.297309100973213170, 6.875137029808006339, 0.7249047842670247599 ) ) ;
#107113 = CARTESIAN_POINT ( 'NONE',  ( 0.7500000000000006661, 12.41666666666666607, -1.299038105676657340 ) ) ;
#107114 = CARTESIAN_POINT ( 'NONE',  ( 5.072158865288233009, 7.010880990960010273, 1.443375672974065660 ) ) ;
#107115 = CARTESIAN_POINT ( 'NONE',  ( 3.831107792978345472, -1.636083747181043879, 0.6751729126634566924 ) ) ;
#107116 = CIRCLE ( 'NONE', #131236, 0.05000000000000002359 ) ;
#107117 = CARTESIAN_POINT ( 'NONE',  ( 8.782984583554449998, 9.141236857102018831, 1.040834085586084257E-14 ) ) ;
#107118 = CARTESIAN_POINT ( 'NONE',  ( 1.325372091284286569, -0.05194335737490791277, 2.105495032795675847 ) ) ;
#107120 = CARTESIAN_POINT ( 'NONE',  ( -1.500000000000013101, 1.879166666666692187, -0.8660254037844313801 ) ) ;
#107119 = CARTESIAN_POINT ( 'NONE',  ( -8.012344526598182026E-15, 10.29687500034139447, -1.575800808251669460 ) ) ;
#107121 = CARTESIAN_POINT ( 'NONE',  ( 0.9593497616274889728, 1.608103478905052119, 1.136861374779022604 ) ) ;
#107122 = CARTESIAN_POINT ( 'NONE',  ( -3.797165540279144214, 6.587721009371067638, 1.199719254218452935 ) ) ;
#107123 = DIRECTION ( 'NONE',  ( 0.6507913734559640506, -0.7592566023653004592, 0.000000000000000000 ) ) ;
#107125 = ORIENTED_EDGE ( 'NONE', *, *, #170395, .T. ) ;
#107124 = CARTESIAN_POINT ( 'NONE',  ( 5.396671993488243224, -1.769204348786549641, -0.3888369506312178703 ) ) ;
#107126 = CARTESIAN_POINT ( 'NONE',  ( 6.968527767744098433, 9.153035033833367251, 1.443375672974076540 ) ) ;
#107127 = CARTESIAN_POINT ( 'NONE',  ( 8.224992744984721327, 12.74757530245756243, 1.040834085586084257E-14 ) ) ;
#107128 = CARTESIAN_POINT ( 'NONE',  ( 4.627732503263369601, -1.150995203733524930, -1.474563928533303869 ) ) ;
#107129 = CARTESIAN_POINT ( 'NONE',  ( 3.083589872104280705, 5.684939719841914929, 1.199719254218450271 ) ) ;
#107130 = ORIENTED_EDGE ( 'NONE', *, *, #206779, .F. ) ;
#107131 = CARTESIAN_POINT ( 'NONE',  ( 4.979381509686323426, -0.1069728651886258930, 2.067640925720988232 ) ) ;
#107132 = CARTESIAN_POINT ( 'NONE',  ( -0.6124999999999967137, 1.541666666666677177, 1.060881119635903147 ) ) ;
#107133 = CARTESIAN_POINT ( 'NONE',  ( -4.109529958273628658, 7.808552361378938045, 0.7216878364870338292 ) ) ;
#107134 = DIRECTION ( 'NONE',  ( 0.000000000000000000, 0.000000000000000000, -1.000000000000000000 ) ) ;
#107135 = CARTESIAN_POINT ( 'NONE',  ( 8.215351014876830504, 11.67199438640995801, -1.199719254218446718 ) ) ;
#107136 = CARTESIAN_POINT ( 'NONE',  ( -1.501703635994465547, 8.650726486491324252, 2.563578082221948495 ) ) ;
#107137 = CARTESIAN_POINT ( 'NONE',  ( 7.693325821111733021, 7.940244644243982464, -0.7998128361456341429 ) ) ;
#107138 = CARTESIAN_POINT ( 'NONE',  ( -4.910932872253781944, 4.686298128553559650, -0.3332635495145727100 ) ) ;
#107139 = CARTESIAN_POINT ( 'NONE',  ( 1.364683531249988757, -0.1156249996585798079, 0.000000000000000000 ) ) ;
#107140 = CARTESIAN_POINT ( 'NONE',  ( -1.500000000000001332, 0.4000000000000253353, 0.000000000000000000 ) ) ;
#107141 = CARTESIAN_POINT ( 'NONE',  ( 3.402741375674179114, 0.4741672551989496998, 1.903589013717405853 ) ) ;
#107142 = CARTESIAN_POINT ( 'NONE',  ( 1.581407437776818581, 1.356094323556347181, -1.492024998029889860 ) ) ;
#107143 = EDGE_CURVE ( 'NONE', #93709, #209328, #82507, .T. ) ;
#107144 = CARTESIAN_POINT ( 'NONE',  ( 11.41381675112453387, 13.40000000000000036, -3.704697986577182522 ) ) ;
#107145 = CARTESIAN_POINT ( 'NONE',  ( -11.33772463945037146, 10.19999999999998153, 3.599999999999999201 ) ) ;
#107146 = CARTESIAN_POINT ( 'NONE',  ( 2.090876104454452378, 1.629797177321444579, -0.9178172146045021629 ) ) ;
#107147 = CARTESIAN_POINT ( 'NONE',  ( 0.6823417656249917140, 5.592708333674749177, 1.181850606188765695 ) ) ;
#107148 = CARTESIAN_POINT ( 'NONE',  ( 3.656497369231588745, 2.003880934342232578, 0.1932520657266077191 ) ) ;
#107150 = CARTESIAN_POINT ( 'NONE',  ( 2.829822700998831486, 0.7593016614581545864, -1.976571788296621834 ) ) ;
#107149 = CARTESIAN_POINT ( 'NONE',  ( -5.585596099150182958, 8.499983968108443477, -1.082531754730544860 ) ) ;
#107151 = CARTESIAN_POINT ( 'NONE',  ( -0.7500000000000215383, 4.972916667349482012, 1.299038105676671107 ) ) ;
#107152 = CARTESIAN_POINT ( 'NONE',  ( 4.492674960910642667, 2.029786422369950216, 0.4070406814440513665 ) ) ;
#107153 = CARTESIAN_POINT ( 'NONE',  ( 5.345657705538078730, 9.458627433094950021, 0.7998128361456331437 ) ) ;
#107155 = CARTESIAN_POINT ( 'NONE',  ( 6.720655732516655156, 7.629137130509086262, 2.673739711112704143 ) ) ;
#107154 = CARTESIAN_POINT ( 'NONE',  ( 0.04657986452102218927, -1.676603903080859492, 1.248863468804935151 ) ) ;
#107157 = EDGE_LOOP ( 'NONE', ( #195706, #151817 ) ) ;
#107156 = CARTESIAN_POINT ( 'NONE',  ( 5.104447739783800841, -0.6163660037172628003, -1.718524672285254740 ) ) ;
#107158 = CARTESIAN_POINT ( 'NONE',  ( 6.916630921265960019, 11.22115317478565188, 0.7998128361456462443 ) ) ;
#107159 = CARTESIAN_POINT ( 'NONE',  ( 0.001697632222342148299, 14.56227640660409683, 11.93887725717812209 ) ) ;
#107160 = CARTESIAN_POINT ( 'NONE',  ( -11.86145016429273191, 13.40000000000000036, 1.099999999999996980 ) ) ;
#107161 = CARTESIAN_POINT ( 'NONE',  ( -10.28135750008142324, 4.005690466847553033, 7.422021812076344816 ) ) ;
#107162 = CARTESIAN_POINT ( 'NONE',  ( 8.066738210006692000, 8.513542121203711233, 0.7216878364870458196 ) ) ;
#107163 = CARTESIAN_POINT ( 'NONE',  ( 0.6823417656249969321, 12.08854166700806765, -1.181850606188757036 ) ) ;
#107164 = CARTESIAN_POINT ( 'NONE',  ( 5.813130153884224605, 1.560705751063670377, -1.104717755519408984 ) ) ;
#107165 = CARTESIAN_POINT ( 'NONE',  ( -7.784352752540590004, 12.23349531127272094, 0.7998128361456481317 ) ) ;
#107166 = CARTESIAN_POINT ( 'NONE',  ( 4.157546660884947620, 8.002221537674429896, 1.040834085586084257E-14 ) ) ;
#107167 = CARTESIAN_POINT ( 'NONE',  ( -11.84668730067608422, 10.90000000000000036, -1.400000000000001688 ) ) ;
#107168 = CARTESIAN_POINT ( 'NONE',  ( -1.000000000000017097, 8.600000000000013856, -0.3999999999999858113 ) ) ;
#107169 = CARTESIAN_POINT ( 'NONE',  ( 4.578903193113299963, 6.365139696764064325, 1.599625672291267398 ) ) ;
#107170 = ORIENTED_EDGE ( 'NONE', *, *, #76005, .T. ) ;
#107171 = CARTESIAN_POINT ( 'NONE',  ( -5.264308783856126439, 9.363720357799287797, -0.7998128361456362523 ) ) ;
#107172 = VECTOR ( 'NONE', #76960, 1000.000000000000114 ) ;
#107173 = CARTESIAN_POINT ( 'NONE',  ( 5.343375128634678006, 0.3905785925618041610, -1.978055652833633271 ) ) ;
#107174 = DIRECTION ( 'NONE',  ( 0.000000000000000000, -1.000000000000000000, 0.000000000000000000 ) ) ;
#107175 = DIRECTION ( 'NONE',  ( 0.000000000000000000, -1.000000000000000000, 0.000000000000000000 ) ) ;
#107176 = CARTESIAN_POINT ( 'NONE',  ( -6.486551268120854807, 6.767445667853342783, -0.2095380678983837508 ) ) ;
#107177 = CARTESIAN_POINT ( 'NONE',  ( -5.761852096127856981, 5.824508321678349532, 0.000000000000000000 ) ) ;
#107178 = CARTESIAN_POINT ( 'NONE',  ( 10.56143847536557878, 11.42402576412244386, 0.000000000000000000 ) ) ;
#107179 = CARTESIAN_POINT ( 'NONE',  ( 2.360148646665951144, -1.969129416856093551, 0.04326586078102003657 ) ) ;
#107180 = CARTESIAN_POINT ( 'NONE',  ( 4.903922820734956112, -1.081083478763317007, -1.701937824264573518 ) ) ;
#107181 = CARTESIAN_POINT ( 'NONE',  ( -7.867809214632013770, 8.073532260025807261, 1.040834085586084257E-14 ) ) ;
#107183 = EDGE_CURVE ( 'NONE', #136751, #31895, #118250, .T. ) ;
#107182 = CARTESIAN_POINT ( 'NONE',  ( 6.727182134110202938, 2.016807574165893513, 2.492494991173601182 ) ) ;
#107184 = CARTESIAN_POINT ( 'NONE',  ( 5.050807487124363782, -1.850163549229045579, -1.174163402404400092 ) ) ;
#107185 =( LENGTH_UNIT ( ) NAMED_UNIT ( * ) SI_UNIT ( .MILLI., .METRE. ) );
#107186 = CARTESIAN_POINT ( 'NONE',  ( 2.995051018759773420, 1.652986441767102743, -0.9890191681132395329 ) ) ;
#107187 = CARTESIAN_POINT ( 'NONE',  ( -9.020252271793614440, 9.418049160047695878, 0.7998128361456462443 ) ) ;
#107188 = CARTESIAN_POINT ( 'NONE',  ( 1.270916165646590379, 3.041024509562812561, 0.7750000000000135669 ) ) ;
#107189 = CARTESIAN_POINT ( 'NONE',  ( -0.02244404828157658613, -0.004869073801674199918, -2.189079685368473527 ) ) ;
#107190 = CARTESIAN_POINT ( 'NONE',  ( -0.4288785890452923022, 3.049942316455306113, -0.4000000000000062395 ) ) ;
#107191 = CARTESIAN_POINT ( 'NONE',  ( -1.364683531250000748, 13.10937500034139980, 0.000000000000000000 ) ) ;
#107192 = CARTESIAN_POINT ( 'NONE',  ( 5.473741331615251227, 7.409117525016355010, -1.599625672291262513 ) ) ;
#107193 = CARTESIAN_POINT ( 'NONE',  ( -6.709229400515914321, -7.621055083280779741, 6.726126798027523002 ) ) ;
#107194 = CARTESIAN_POINT ( 'NONE',  ( 5.234856708652235291, 5.279956712948652431, 0.7216878364870338292 ) ) ;
#107195 = ORIENTED_EDGE ( 'NONE', *, *, #15512, .F. ) ;
#107197 = CARTESIAN_POINT ( 'NONE',  ( 3.317044347720001785, 1.585670248135360838, -1.240117154037506886 ) ) ;
#107196 = CARTESIAN_POINT ( 'NONE',  ( 5.987831981441136264, -1.833028718050220940, -0.1737628300680846560 ) ) ;
#107198 = CARTESIAN_POINT ( 'NONE',  ( 5.114793989753786185, 0.7273159113986256141, -2.180329384352611033 ) ) ;
#107200 = CARTESIAN_POINT ( 'NONE',  ( 3.467479172597370596, -0.3673618142193516012, 1.824136687861827921 ) ) ;
#107199 = CARTESIAN_POINT ( 'NONE',  ( 3.588273936444265289, 7.344317902764286643, -0.3372145678562175064 ) ) ;
#107201 = CARTESIAN_POINT ( 'NONE',  ( 1.001543065824772753E-15, -0.3718749995220430038, 3.793834371823811669 ) ) ;
#107203 = EDGE_CURVE ( 'NONE', #30182, #62825, #183411, .T. ) ;
#107202 = DIRECTION ( 'NONE',  ( 0.000000000000000000, 0.000000000000000000, -1.000000000000000000 ) ) ;
#107204 = DIRECTION ( 'NONE',  ( 1.000000000000000000, -0.000000000000000000, -0.000000000000000000 ) ) ;
#107205 = CARTESIAN_POINT ( 'NONE',  ( -6.021792782764022078, 10.17717534653336209, -0.7998128361456291469 ) ) ;
#107206 = CARTESIAN_POINT ( 'NONE',  ( -5.831415467653581430, 5.975941931783510519, 0.7216878364870257245 ) ) ;
#107207 = CARTESIAN_POINT ( 'NONE',  ( 5.899963319545262763, -0.7533809947482277281, -1.950465142816688813 ) ) ;
#107208 = CARTESIAN_POINT ( 'NONE',  ( 5.558479791922850133, 6.547609847740540445, -1.082531754730542195 ) ) ;
#107209 = ORIENTED_EDGE ( 'NONE', *, *, #117977, .T. ) ;
#107210 = B_SPLINE_CURVE_WITH_KNOTS ( 'NONE', 3,
 ( #43448, #58610, #174521, #124765, #26097, #190724 ),
 .UNSPECIFIED., .F., .F.,
 ( 4, 2, 4 ),
 ( 0.000000000000000000, 0.0003168911866439334617, 0.0006337823732878669234 ),
 .UNSPECIFIED. ) ;
#107211 = CARTESIAN_POINT ( 'NONE',  ( 5.594708818112484217, 5.774250729507365953, 0.6894988139244705438 ) ) ;
#107213 = CARTESIAN_POINT ( 'NONE',  ( 4.325214697959421706, 5.004837554829479451, 1.199719254218462483 ) ) ;
#107212 = CARTESIAN_POINT ( 'NONE',  ( -4.816538118508267630, 5.092449105792602460, -0.9495590845017554127 ) ) ;
#107214 = CARTESIAN_POINT ( 'NONE',  ( 5.971300253285758863, 0.1196647562241616447, -1.720808320142935610 ) ) ;
#107215 = CARTESIAN_POINT ( 'NONE',  ( -5.786632634934295361, 5.645492917045106473, 0.7998128361456341429 ) ) ;
#107216 = CARTESIAN_POINT ( 'NONE',  ( 1.336079928753497681, 0.5043104442001166143, -1.659204044645303355 ) ) ;
#107217 = CARTESIAN_POINT ( 'NONE',  ( -9.052987461608243080, 14.55305228048848676, 7.822201588416328732 ) ) ;
#107218 = DIRECTION ( 'NONE',  ( 0.000000000000000000, 0.000000000000000000, 1.000000000000000000 ) ) ;
#107219 = CARTESIAN_POINT ( 'NONE',  ( 0.000000000000000000, 2.000000000000001776, 0.000000000000000000 ) ) ;
#107220 = CARTESIAN_POINT ( 'NONE',  ( 5.664936021742177807, 1.649023742746661192, -1.412335049966114253 ) ) ;
#107221 = CARTESIAN_POINT ( 'NONE',  ( 4.635264976507449397, -1.668059998867366778, 0.7425182445051290436 ) ) ;
#107222 = CARTESIAN_POINT ( 'NONE',  ( 2.324987154519737143, -1.791562868964852395, -0.7996954790665600221 ) ) ;
#107223 = DIRECTION ( 'NONE',  ( 1.000000000000000000, -7.387867266669436732E-31, 0.000000000000000000 ) ) ;
#107224 = CARTESIAN_POINT ( 'NONE',  ( -8.306341666666730461, 12.84248237775322643, 1.040834085586084257E-14 ) ) ;
#107225 = CARTESIAN_POINT ( 'NONE',  ( 8.111855979677986994, 8.358253485912799263, 1.040834085586084257E-14 ) ) ;
#107226 = STYLED_ITEM ( 'NONE', ( #199747 ), #159239 ) ;
#107227 = CARTESIAN_POINT ( 'NONE',  ( 3.774183692772983267, 2.104302197123971485, -0.2610650231627819062 ) ) ;
#107228 = CARTESIAN_POINT ( 'NONE',  ( 9.498553103985692303, -9.900000000000005684, -0.1657978611541485181 ) ) ;
#107229 = DIRECTION ( 'NONE',  ( 0.000000000000000000, -1.000000000000000000, 0.000000000000000000 ) ) ;
#107230 = ADVANCED_FACE ( 'NONE', ( #132340 ), #185296, .T. ) ;
#107231 = B_SPLINE_CURVE_WITH_KNOTS ( 'NONE', 1,
 ( #157680, #120984 ),
 .UNSPECIFIED., .F., .F.,
 ( 2, 2 ),
 ( 0.3873181335520736179, 1.000000000000000000 ),
 .UNSPECIFIED. ) ;
#107232 = CARTESIAN_POINT ( 'NONE',  ( -5.077710034904439951, 6.555083676148210081, -1.223860624452234980 ) ) ;
#107233 = CARTESIAN_POINT ( 'NONE',  ( 2.131770371054972912, 1.982354287819853456, -0.5969549857752221023 ) ) ;
#107235 = CARTESIAN_POINT ( 'NONE',  ( 1.364683531249986537, -0.8239583329919186738, 0.7879004041258500513 ) ) ;
#107234 = CARTESIAN_POINT ( 'NONE',  ( -11.32145367647657785, 0.9706168436483550988, 3.678563289475746068 ) ) ;
#107237 = ORIENTED_EDGE ( 'NONE', *, *, #100151, .F. ) ;
#107236 = CARTESIAN_POINT ( 'NONE',  ( 3.721504678736448302, 1.905620783811642571, 1.141157194635911365 ) ) ;
#107238 = CARTESIAN_POINT ( 'NONE',  ( 2.233388324916096845, 2.298236692437699791, 0.05235245155727624722 ) ) ;
#107240 = CARTESIAN_POINT ( 'NONE',  ( 6.977413162628444354, -0.1478290182607009950, 2.029965231729473185 ) ) ;
#107239 = CARTESIAN_POINT ( 'NONE',  ( 9.788623719386617239, 11.48277776311499387, -1.082531754730537088 ) ) ;
#107242 = CARTESIAN_POINT ( 'NONE',  ( 3.475000000000000533, -0.4958333333333350690, -2.006292185433951047 ) ) ;
#107241 = CARTESIAN_POINT ( 'NONE',  ( 5.011674058906918638, 5.875983152593414971, 1.199719254218452047 ) ) ;
#107243 = LINE ( 'NONE', #73602, #37091 ) ;
#107244 = CARTESIAN_POINT ( 'NONE',  ( -10.96028113393447434, -5.411711732698798905, 0.1309013025973318201 ) ) ;
#107245 = DIRECTION ( 'NONE',  ( -0.000000000000000000, -1.000000000000000000, -0.000000000000000000 ) ) ;
#107246 = CARTESIAN_POINT ( 'NONE',  ( -0.2106725631050176684, -0.004273297132624876912, -2.003483006309703995 ) ) ;
#107247 = CARTESIAN_POINT ( 'NONE',  ( 3.381609400508314600, 1.093566088711795281, 1.333772831174476758 ) ) ;
#107248 = CARTESIAN_POINT ( 'NONE',  ( 2.272673044126482189, -0.3494851828299733176, -1.985868527484459856 ) ) ;
#107249 = CARTESIAN_POINT ( 'NONE',  ( 2.514614159817552430, -2.143548176638510938, 0.8305585572774812908 ) ) ;
#107250 = CARTESIAN_POINT ( 'NONE',  ( 3.849113346294403382, -1.852342442990447813, 1.298737409825992062 ) ) ;
#107251 = CARTESIAN_POINT ( 'NONE',  ( 5.725249284967181218, -0.05305106314347144553, 2.105570132020935237 ) ) ;
#107252 = CARTESIAN_POINT ( 'NONE',  ( -5.641601317062233001, 9.595968946632336127, -0.7216878364870338292 ) ) ;
#107253 = ORIENTED_EDGE ( 'NONE', *, *, #78683, .T. ) ;
#107254 = CARTESIAN_POINT ( 'NONE',  ( 3.426767255637660270, 0.04027588734063606429, 1.769438255327019593 ) ) ;
#107256 = CARTESIAN_POINT ( 'NONE',  ( 0.07670252363861564115, -2.225146658028719582, -0.5502862128906602646 ) ) ;
#107255 = CARTESIAN_POINT ( 'NONE',  ( 4.706088717274906408, 5.623429937309770921, 1.082531754730549078 ) ) ;
#107257 = CARTESIAN_POINT ( 'NONE',  ( 5.296754776809613041, 1.507285696749562476, 1.057021923447129197 ) ) ;
#107258 = CARTESIAN_POINT ( 'NONE',  ( -3.918470089549458635, 4.530302178351167441, -1.199719254218452047 ) ) ;
#107259 = CARTESIAN_POINT ( 'NONE',  ( 5.525378525699438548, -1.388074942811763357, -1.695776126864618316 ) ) ;
#107260 = CARTESIAN_POINT ( 'NONE',  ( -3.918470089549458635, 4.530302178351167441, -1.199719254218452047 ) ) ;
#107261 = CARTESIAN_POINT ( 'NONE',  ( 0.05568803613164878541, 15.46908327293036400, 11.99987078441405508 ) ) ;
#107262 = CARTESIAN_POINT ( 'NONE',  ( 5.600075274486990828, 0.8424382930321882013, -1.891409743246947217 ) ) ;
#107263 = CARTESIAN_POINT ( 'NONE',  ( -0.1706859984542466180, -1.561801110730935971, -1.275320528755889526 ) ) ;
#107264 = CARTESIAN_POINT ( 'NONE',  ( 1.499999999999987566, -0.9437499993171851731, 0.000000000000000000 ) ) ;
#107265 = CARTESIAN_POINT ( 'NONE',  ( 4.459546661884671970, 0.4205705884572363829, -1.879884317620848178 ) ) ;
#107266 = CARTESIAN_POINT ( 'NONE',  ( -1.364683531250010295, 10.63020833367473195, 0.7879004041258445001 ) ) ;
#107267 = CARTESIAN_POINT ( 'NONE',  ( -3.145128448690323264, 4.692402494937224056, -1.443375672974059665 ) ) ;
#107268 = CARTESIAN_POINT ( 'NONE',  ( 0.3697636260225238836, -1.880949819439242443, -1.181558314010826116 ) ) ;
#107270 = VERTEX_POINT ( 'NONE', #188509 ) ;
#107269 = CARTESIAN_POINT ( 'NONE',  ( 5.076602173674213070, 4.887400388900169368, 0.000000000000000000 ) ) ;
#107272 = DIRECTION ( 'NONE',  ( 0.000000000000000000, 1.000000000000000000, 0.000000000000000000 ) ) ;
#107271 = CARTESIAN_POINT ( 'NONE',  ( -5.316205630334276400, 5.374863788244313767, -0.7216878364870338292 ) ) ;
#107273 = CARTESIAN_POINT ( 'NONE',  ( 3.246287715468270108, 5.874753870433235825, 1.199719254218450271 ) ) ;
#107274 = CARTESIAN_POINT ( 'NONE',  ( 7.842350841322883959, -5.412329794880678335, -7.657759090810039915 ) ) ;
#107275 = CARTESIAN_POINT ( 'NONE',  ( 1.419999999999990603, 6.120000000000041851, 2.580000000000000515 ) ) ;
#107276 = CARTESIAN_POINT ( 'NONE',  ( 9.348381460497192208, 13.52536904890506797, 7.450314784081282227 ) ) ;
#107277 = CARTESIAN_POINT ( 'NONE',  ( 10.19536832735223975, 10.99694392477354477, 0.000000000000000000 ) ) ;
#107278 = CARTESIAN_POINT ( 'NONE',  ( 0.9417639971489067952, 1.314929008279978495, 1.456166070238865018 ) ) ;
#107279 = CARTESIAN_POINT ( 'NONE',  ( -0.6823417656250003738, 1.280208333674752508, -1.181850606188749264 ) ) ;
#107280 = DIRECTION ( 'NONE',  ( -1.000000000000000000, -7.047314121155791443E-15, -8.638326563840826660E-31 ) ) ;
#107281 = CARTESIAN_POINT ( 'NONE',  ( 5.371523934717264304, -0.2895824386080196322, 1.940264742196501802 ) ) ;
#107282 = CARTESIAN_POINT ( 'NONE',  ( -6.970863535720637216, 11.28442455831609337, 0.7998128361456481317 ) ) ;
#107283 = CARTESIAN_POINT ( 'NONE',  ( -6.060131475184148186, 6.172500930577367484, 0.7216878364870317197 ) ) ;
#107284 = CARTESIAN_POINT ( 'NONE',  ( 6.543834100630380846, 0.8322713294773576020, -1.995267709627518427 ) ) ;
#107286 = ORIENTED_EDGE ( 'NONE', *, *, #52227, .F. ) ;
#107285 = CARTESIAN_POINT ( 'NONE',  ( -7.203459687562382641, 7.298457811777897319, -0.7998128361456291469 ) ) ;
#107287 = CARTESIAN_POINT ( 'NONE',  ( 1.364683531249992088, 5.384375000341417916, 1.214306433183764966E-14 ) ) ;
#107288 = CARTESIAN_POINT ( 'NONE',  ( 1.844777716111935861, -1.582881869529973562, 0.9963996312925410548 ) ) ;
#107289 = CARTESIAN_POINT ( 'NONE',  ( 0.05276861106134726059, -1.135576942788417254, 1.310739833803043819 ) ) ;
#107291 = CARTESIAN_POINT ( 'NONE',  ( 4.405938146338868933, -0.9375679901368579872, -1.981035393479456008 ) ) ;
#107290 = CARTESIAN_POINT ( 'NONE',  ( -0.6801582343750125492, 2.182291667008062763, 1.178068619123824323 ) ) ;
#107292 = CARTESIAN_POINT ( 'NONE',  ( 4.102763937057193999, -0.7201832649769298600, -2.192400882750038971 ) ) ;
#107293 = CARTESIAN_POINT ( 'NONE',  ( 6.678986887005352813, -0.09631167155637165855, -2.058642716137318640 ) ) ;
#107294 = CARTESIAN_POINT ( 'NONE',  ( 2.361185668158103379, 1.904436331314839137, -0.3790439726399745246 ) ) ;
#107295 = CARTESIAN_POINT ( 'NONE',  ( -5.382223794500843539, 7.302347065049529462, -1.443375672974051449 ) ) ;
#107296 = FACE_OUTER_BOUND ( 'NONE', #125728, .T. ) ;
#107297 = CARTESIAN_POINT ( 'NONE',  ( 5.625269520628737752, 1.871107552910089122, 0.9978724776121964402 ) ) ;
#107298 = CARTESIAN_POINT ( 'NONE',  ( 1.360316468749980023, 0.01562500034139879812, -2.255140518769849223E-14 ) ) ;
#107299 = CARTESIAN_POINT ( 'NONE',  ( 3.516250148862578584, -1.862017090670412767, 0.7743150488077471527 ) ) ;
#107300 = CARTESIAN_POINT ( 'NONE',  ( -5.409340101728186134, 5.413244328212063472, 0.7216878364870317197 ) ) ;
#107301 = CARTESIAN_POINT ( 'NONE',  ( -5.932574734431526942, 9.079031735882207244, 1.199719254218454489 ) ) ;
#107302 = CARTESIAN_POINT ( 'NONE',  ( 9.049177462117294013, 12.64479190819049670, -1.199719254218446718 ) ) ;
#107303 = CARTESIAN_POINT ( 'NONE',  ( 1.277666653898035021, 1.085793613588705853, 1.467558327050644484 ) ) ;
#107304 = CARTESIAN_POINT ( 'NONE',  ( -5.936491157937300756, 8.019268665717216749, 1.599625672291263179 ) ) ;
#107305 = CARTESIAN_POINT ( 'NONE',  ( -0.06970559732546230403, 15.50808405863728723, 11.99964040566943346 ) ) ;
#107306 = CARTESIAN_POINT ( 'NONE',  ( -10.83925572545687999, 5.627432043407305962, 6.488667418600654102 ) ) ;
#107307 = ORIENTED_EDGE ( 'NONE', *, *, #198854, .F. ) ;
#107308 = CARTESIAN_POINT ( 'NONE',  ( 5.998915433584960155, 1.686223865786851128, -1.184587077384538167 ) ) ;
#107309 = CARTESIAN_POINT ( 'NONE',  ( -7.553300976144794454, 7.984808358356614733, -0.7216878364870338292 ) ) ;
#107310 = CARTESIAN_POINT ( 'NONE',  ( 3.660338286009610975, 6.253849852777763729, -1.082531754730543083 ) ) ;
#107311 = CARTESIAN_POINT ( 'NONE',  ( -5.264643720808155791, 5.036505850564608089, 0.000000000000000000 ) ) ;
#107312 = CARTESIAN_POINT ( 'NONE',  ( -5.691079914216616409, 6.283969663839313213, 1.134429477820863008 ) ) ;
#107313 = CARTESIAN_POINT ( 'NONE',  ( 4.055335607603890224, -1.756228124781366917, 0.9972510931155349478 ) ) ;
#107314 = CARTESIAN_POINT ( 'NONE',  ( 5.180443790456886077, 1.093758630767979412, 1.933306047416243567 ) ) ;
#107316 = CARTESIAN_POINT ( 'NONE',  ( 7.619319141200063150, 9.912291636198670375, 1.443375672974076540 ) ) ;
#107315 = CARTESIAN_POINT ( 'NONE',  ( -8.086512275908061653, 8.398962174839683215, 0.000000000000000000 ) ) ;
#107317 = CARTESIAN_POINT ( 'NONE',  ( 6.657217119509961201, 7.725507046638470321, -1.199719254218446718 ) ) ;
#107318 = CARTESIAN_POINT ( 'NONE',  ( 4.452062314400541787, 2.060485596604546110, -0.04854883430290175134 ) ) ;
#107319 = CARTESIAN_POINT ( 'NONE',  ( 3.692029868468839737, 1.730865839653324079, 1.034166058993556181 ) ) ;
#107320 = ORIENTED_EDGE ( 'NONE', *, *, #88039, .F. ) ;
#107321 = DIRECTION ( 'NONE',  ( 1.000000000000000000, -0.000000000000000000, -0.000000000000000000 ) ) ;
#107322 = CARTESIAN_POINT ( 'NONE',  ( 4.222474775652216294, 7.013638773981186958, 1.199719254218462483 ) ) ;
#107324 = EDGE_LOOP ( 'NONE', ( #43640, #213094 ) ) ;
#107323 = CARTESIAN_POINT ( 'NONE',  ( -5.921879234118920365, 10.13088588310589699, 0.000000000000000000 ) ) ;
#107325 = CARTESIAN_POINT ( 'NONE',  ( 4.701115458738250652, 8.361069499448168685, -0.6471830670988186762 ) ) ;
#107326 = CARTESIAN_POINT ( 'NONE',  ( 3.550157523342875709, 1.823840110401256931, -0.8594984857327039318 ) ) ;
#107327 = CARTESIAN_POINT ( 'NONE',  ( 2.800538183361205302, 1.555518290611109800, 0.9846574483025125613 ) ) ;
#107328 = CARTESIAN_POINT ( 'NONE',  ( 3.853900823548666921, 8.531065964594311879, 2.447540105570115809 ) ) ;
#107329 = CARTESIAN_POINT ( 'NONE',  ( 0.5929126122562259349, -2.290994082922478636, -0.2767204673215419852 ) ) ;
#107330 = CARTESIAN_POINT ( 'NONE',  ( 7.506374323821472849, 8.786466794993730289, -1.199719254218452047 ) ) ;
#107331 = CARTESIAN_POINT ( 'NONE',  ( 3.515052679271633895, 1.952536648612019921, 0.9277410485990513767 ) ) ;
#107332 = CARTESIAN_POINT ( 'NONE',  ( 8.666686507633574621, 11.13422023037111330, 1.599625672291281386 ) ) ;
#107333 = CARTESIAN_POINT ( 'NONE',  ( -5.768104287610143821, 8.816873204598778102, -1.199719254218440723 ) ) ;
#107334 = EDGE_CURVE ( 'NONE', #123356, #199128, #71540, .T. ) ;
#107335 = AXIS2_PLACEMENT_3D ( 'NONE', #184051, #69217, #179813 ) ;
#107336 = CARTESIAN_POINT ( 'NONE',  ( 2.952824900933643804, 1.623659768481898302, 1.626969957801235989 ) ) ;
#107337 = CARTESIAN_POINT ( 'NONE',  ( -11.48243876534946217, 12.21999999999998288, 3.199999999999997957 ) ) ;
#107338 = CARTESIAN_POINT ( 'NONE',  ( 2.219420098953532428, -1.815089452277141691, 0.4520615115926190919 ) ) ;
#107339 = CARTESIAN_POINT ( 'NONE',  ( 5.577018171352951192, -0.04780089932613153236, -1.971040553531088868 ) ) ;
#107341 = CARTESIAN_POINT ( 'NONE',  ( -7.761116589180078407, 8.019333873657032541, 0.000000000000000000 ) ) ;
#107340 = CARTESIAN_POINT ( 'NONE',  ( 0.6823417656249917140, 4.092708333674755394, 1.181850606188765695 ) ) ;
#107343 = CARTESIAN_POINT ( 'NONE',  ( 0.9267433102794273569, 1.311770220233858586, -1.774563083084364834 ) ) ;
#107342 = CARTESIAN_POINT ( 'NONE',  ( -4.225337428953291230, 8.081310767087481750, 0.7998128361456341429 ) ) ;
#107344 = CARTESIAN_POINT ( 'NONE',  ( -1.436838838544789221, 7.449283400311735193, -4.203727439823564893 ) ) ;
#107345 = CARTESIAN_POINT ( 'NONE',  ( 5.192936529234042808, 6.017179691316550283, -1.199719254218452047 ) ) ;
#107346 = CARTESIAN_POINT ( 'NONE',  ( -6.084912014434944894, 5.993485526462540847, -0.7998128361456291469 ) ) ;
#107347 = CARTESIAN_POINT ( 'NONE',  ( -2.331034670843834533E-15, -9.418601272600245267, -9.907592596884320812 ) ) ;
#107348 = CARTESIAN_POINT ( 'NONE',  ( 6.280149219824591178, -1.055055557545642175, 1.665224566959803143 ) ) ;
#107349 = CARTESIAN_POINT ( 'NONE',  ( 6.112023189137078205, -2.291079414021851779, 0.2760875835842706016 ) ) ;
#107350 = CARTESIAN_POINT ( 'NONE',  ( 6.672303541529164050, -0.8785034406106060345, -1.640621795851913367 ) ) ;
#107351 = CARTESIAN_POINT ( 'NONE',  ( 3.291897078901334428, -1.381674118267547602, -1.531590470265832726 ) ) ;
#107352 = CARTESIAN_POINT ( 'NONE',  ( 6.399085315970131305, 8.488685506763726352, -1.443375672974057666 ) ) ;
#107353 = EDGE_CURVE ( 'NONE', #15325, #147186, #77610, .T. ) ;
#107354 = CARTESIAN_POINT ( 'NONE',  ( 4.934241560730721510, 4.721313007132757811, 0.000000000000000000 ) ) ;
#107355 = CARTESIAN_POINT ( 'NONE',  ( 6.765155463094751909, 8.915767345075790828, 1.443375672974076540 ) ) ;
#107356 = CARTESIAN_POINT ( 'NONE',  ( -0.6823417656250003738, 3.030208333674754062, -1.181850606188749264 ) ) ;
#107357 = CARTESIAN_POINT ( 'NONE',  ( -6.714760661030930500, 14.53011251428762840, 9.955875793587102507 ) ) ;
#107358 = CARTESIAN_POINT ( 'NONE',  ( 5.219525951136835928, 7.112532914458205013, -1.443375672974051449 ) ) ;
#107359 = CARTESIAN_POINT ( 'NONE',  ( 5.898927382237683759, 0.4177183949424836396, 2.130464630886391486 ) ) ;
#107360 = CARTESIAN_POINT ( 'NONE',  ( 0.4288785890452437299, 3.049942316455264812, -0.4196807566835009662 ) ) ;
#107361 =( REPRESENTATION_RELATIONSHIP ('NONE','NONE', #84563, #113740 ) REPRESENTATION_RELATIONSHIP_WITH_TRANSFORMATION ( #104559 )SHAPE_REPRESENTATION_RELATIONSHIP( ) );
#107363 = CARTESIAN_POINT ( 'NONE',  ( 5.442854017605395889, -1.455216020186438364, -1.127989967910733915 ) ) ;
#107362 = CARTESIAN_POINT ( 'NONE',  ( -3.633221978782304351, 4.301475732409860697, -1.082531754730549967 ) ) ;
#107365 = CARTESIAN_POINT ( 'NONE',  ( 6.620655732516632419, 1.270823175217004941, 2.040803978124502205 ) ) ;
#107364 = CARTESIAN_POINT ( 'NONE',  ( -0.6823417656249969321, 5.467708333674756283, -1.181850606188749264 ) ) ;
#107366 = LINE ( 'NONE', #157133, #46199 ) ;
#107367 = CARTESIAN_POINT ( 'NONE',  ( 1.506454395378247121E-16, 4.099999999999999645, 2.250000000000000000 ) ) ;
#107368 = CARTESIAN_POINT ( 'NONE',  ( 6.579017896966585788, -0.1030185651522512180, -2.260299859776133236 ) ) ;
#107369 = CARTESIAN_POINT ( 'NONE',  ( -4.520189846367452802, 7.221058948360024488, -1.319278014013465894 ) ) ;
#107370 = CYLINDRICAL_SURFACE ( 'NONE', #179386, 0.3999999999999997446 ) ;
#107371 = CARTESIAN_POINT ( 'NONE',  ( 6.596403382356258227, 6.772441155557838321, -0.1798620802159808241 ) ) ;
#107372 = CARTESIAN_POINT ( 'NONE',  ( -4.570507181138272479, 7.385989907086349504, 1.082531754730549967 ) ) ;
#107373 = CARTESIAN_POINT ( 'NONE',  ( 0.4867802866235851345, -1.800715477623024086, -0.6440170976053718466 ) ) ;
#107374 = CARTESIAN_POINT ( 'NONE',  ( 1.410649291501327118, 1.558696297929580199, 0.8383436984091273692 ) ) ;
#107375 = CARTESIAN_POINT ( 'NONE',  ( 0.02974158317493520720, -1.875378228685410376, 0.3729384364157954379 ) ) ;
#107376 = CARTESIAN_POINT ( 'NONE',  ( 4.753012104044548991, -1.692955597047377747, 1.252381512178860401 ) ) ;
#107378 = CARTESIAN_POINT ( 'NONE',  ( 3.778834734487185099, 1.616410871901182711, -1.027684692424314594 ) ) ;
#107377 = CARTESIAN_POINT ( 'NONE',  ( -2.941756144040970522, 5.415504020480993219, -1.082531754730543083 ) ) ;
#107379 = CARTESIAN_POINT ( 'NONE',  ( -0.02244404828157393894, 7.629137130509076492, -2.789100637983292774 ) ) ;
#107380 = B_SPLINE_CURVE_WITH_KNOTS ( 'NONE', 3,
 ( #135367, #35703, #186214, #202447, #36766, #122393, #20511, #169969, #86596, #53023 ),
 .UNSPECIFIED., .F., .F.,
 ( 4, 3, 3, 4 ),
 ( 3.112925509940513280E-16, 3.125186881574499746E-05, 5.993688232072589769E-05, 8.863274572801039055E-05 ),
 .UNSPECIFIED. ) ;
#107381 = CARTESIAN_POINT ( 'NONE',  ( 4.457443581450992731, 1.580467340599530424, 1.175029403372893855 ) ) ;
#107382 = CARTESIAN_POINT ( 'NONE',  ( 6.170177014438331220, 2.014108787598484440, -0.1525786406279260876 ) ) ;
#107383 = CARTESIAN_POINT ( 'NONE',  ( -0.4019237886467001974, 11.05133545031537068, 1.500000000000001998 ) ) ;
#107384 = CARTESIAN_POINT ( 'NONE',  ( 2.887410755087606695, 1.321643875934110479, 1.324118206929347563 ) ) ;
#107386 = ORIENTED_EDGE ( 'NONE', *, *, #173872, .T. ) ;
#107385 = CARTESIAN_POINT ( 'NONE',  ( 5.496639145235802104, -0.4250261254647030307, -1.671567591930831043 ) ) ;
#107388 = CARTESIAN_POINT ( 'NONE',  ( 4.690757960648224589, 6.495636925554817864, 1.443375672974062551 ) ) ;
#107387 = CARTESIAN_POINT ( 'NONE',  ( 2.596532132193625664, -2.201043451360765957, -0.1612727490639675743 ) ) ;
#107389 = VECTOR ( 'NONE', #197687, 1000.000000000000000 ) ;
#107390 = CARTESIAN_POINT ( 'NONE',  ( 1.364683531249988535, 3.426041667008085323, 0.7879004041258500513 ) ) ;
#107391 = CARTESIAN_POINT ( 'NONE',  ( 6.637165056451467038, -0.09505199798197358496, -1.959668910398344233 ) ) ;
#107392 = CARTESIAN_POINT ( 'NONE',  ( 6.753933077901968396, 11.03133902419432566, 0.7998128361456462443 ) ) ;
#107393 = CARTESIAN_POINT ( 'NONE',  ( -8.469039510030723861, 13.03229652834454733, 1.040834085586084257E-14 ) ) ;
#107394 = CARTESIAN_POINT ( 'NONE',  ( -8.794101853178666772, 3.696394713403118537, -7.873312689837527856 ) ) ;
#107395 = CARTESIAN_POINT ( 'NONE',  ( -3.567766978690493307, 7.314145241780881435, 1.040834085586084257E-14 ) ) ;
#107396 = CARTESIAN_POINT ( 'NONE',  ( 7.960263458454529761, -6.452016313277121107, 7.960263458454502228 ) ) ;
#107397 = EDGE_LOOP ( 'NONE', ( #31006, #59581, #39863, #133603, #10718, #92167, #135857, #51586, #68055, #19584, #37172, #199398, #77277, #75549 ) ) ;
#107398 = CARTESIAN_POINT ( 'NONE',  ( 1.539598694730393680, 1.913698299121506352, -0.7905179490511196061 ) ) ;
#107399 = CARTESIAN_POINT ( 'NONE',  ( 1.499999999999989120, 3.754166666666685082, 0.8660254037844524744 ) ) ;
#107400 = CARTESIAN_POINT ( 'NONE',  ( 6.094553744542824170, 7.069066442510145265, 1.199719254218462483 ) ) ;
#107401 = CARTESIAN_POINT ( 'NONE',  ( 4.065465959251388206, 5.836405933916976707, -1.599625672291269396 ) ) ;
#107402 = CARTESIAN_POINT ( 'NONE',  ( 6.569000932001921811, -1.639521903533578850, 1.344440124909966450 ) ) ;
#107403 = FACE_OUTER_BOUND ( 'NONE', #176188, .T. ) ;
#107404 = CARTESIAN_POINT ( 'NONE',  ( -1.364683531250012516, 4.488541667008090208, -0.7879004041258300672 ) ) ;
#107405 = ORIENTED_EDGE ( 'NONE', *, *, #99953, .F. ) ;
#107407 = CARTESIAN_POINT ( 'NONE',  ( 9.788623719386617239, 11.48277776311499387, -1.082531754730537088 ) ) ;
#107406 = CARTESIAN_POINT ( 'NONE',  ( -11.41381675112453564, 11.03005666089993220, -3.704697986577182522 ) ) ;
#107408 = CARTESIAN_POINT ( 'NONE',  ( 5.888046020683161075, -0.05228737891407529703, 2.015604419750731680 ) ) ;
#107409 = CARTESIAN_POINT ( 'NONE',  ( 4.891753643660703865, -1.905893201010636195, 0.1940691045876908327 ) ) ;
#107410 = CARTESIAN_POINT ( 'NONE',  ( 6.639320575229256782, 3.693993153770461113, 2.517469677323687538 ) ) ;
#107411 = CARTESIAN_POINT ( 'NONE',  ( 2.859115728684503477, 0.3189004193784421015, -2.168101852914063876 ) ) ;
#107412 = CARTESIAN_POINT ( 'NONE',  ( -1.499999999999997780, 2.181250000682817713, 1.214306433183764966E-14 ) ) ;
#107413 = CARTESIAN_POINT ( 'NONE',  ( 1.880979024232478425, -1.749874716401520036, -0.7718601483891265325 ) ) ;
#107414 = CARTESIAN_POINT ( 'NONE',  ( -4.882907879216086933, 8.848476292394087395, -0.7998128361456281477 ) ) ;
#107416 = CARTESIAN_POINT ( 'NONE',  ( 6.521125090989952078, -1.891168486443073116, 0.9521521135891182208 ) ) ;
#107415 = CARTESIAN_POINT ( 'NONE',  ( -4.908906423376278028, 4.799815971864533459, -0.1755478183662619873 ) ) ;
#107417 = CARTESIAN_POINT ( 'NONE',  ( 1.364683531249997417, 10.29687500034139802, 2.602085213965210642E-15 ) ) ;
#107419 = CARTESIAN_POINT ( 'NONE',  ( -6.805266759416629618, 6.904175738932996964, 0.000000000000000000 ) ) ;
#107418 = CARTESIAN_POINT ( 'NONE',  ( 5.829655996829377962, 1.081331853127937448, -1.906115348727636549 ) ) ;
#107421 = ORIENTED_EDGE ( 'NONE', *, *, #207656, .T. ) ;
#107420 = CARTESIAN_POINT ( 'NONE',  ( 2.731144534912807842, -1.610196803864067938, 0.6186328129335681991 ) ) ;
#107422 = CARTESIAN_POINT ( 'NONE',  ( -1.580854408705412606, -0.9623865910009720137, 1.305104700536227735 ) ) ;
#107423 = CARTESIAN_POINT ( 'NONE',  ( 5.495132332240461714, 5.305409230568988832, 0.7998128361456341429 ) ) ;
#107424 = CARTESIAN_POINT ( 'NONE',  ( -1.368157835711294013, 13.37576698399829134, -0.1511644340184340740 ) ) ;
#107425 = FACE_BOUND ( 'NONE', #128766, .T. ) ;
#107426 = CARTESIAN_POINT ( 'NONE',  ( 11.52469724861194145, 9.720000066487687107, -3.346365485506883175 ) ) ;
#107427 = CARTESIAN_POINT ( 'NONE',  ( 5.494078562035752178, 7.432844293840273231, -1.599625672291262513 ) ) ;
#107428 = CARTESIAN_POINT ( 'NONE',  ( 0.4356160240586420263, -9.063431457505059186, -9.626717610576610795 ) ) ;
#107429 = ORIENTED_EDGE ( 'NONE', *, *, #153998, .F. ) ;
#107430 = CARTESIAN_POINT ( 'NONE',  ( 3.022498986271242138, 2.800000000000017586, 2.500000000000000444 ) ) ;
#107431 = CIRCLE ( 'NONE', #186806, 12.00000000000000355 ) ;
#107432 = ORIENTED_EDGE ( 'NONE', *, *, #16992, .T. ) ;
#107433 = CARTESIAN_POINT ( 'NONE',  ( 2.842218536208180435, 1.004546245467073717, -1.507189720918320486 ) ) ;
#107434 = VERTEX_POINT ( 'NONE', #169059 ) ;
#107435 = CARTESIAN_POINT ( 'NONE',  ( 8.971744963941056028, 11.49012176272984931, 1.599625672291281386 ) ) ;
#107436 = CARTESIAN_POINT ( 'NONE',  ( 5.086243903782109221, 5.962981304947771122, -1.199719254218452047 ) ) ;
#107437 = CARTESIAN_POINT ( 'NONE',  ( 3.967288593341521175, -1.508176260789632739, -1.003069782103764185 ) ) ;
#107438 = CARTESIAN_POINT ( 'NONE',  ( 7.634649897826744080, 9.040084647953621655, 1.082531754730549078 ) ) ;
#107439 = CARTESIAN_POINT ( 'NONE',  ( -10.93053916617011012, -8.254340240174407484, 0.1907932708458889848 ) ) ;
#107440 = CARTESIAN_POINT ( 'NONE',  ( 5.830449476509543594, 6.014588727829297987, 0.4175459632603968352 ) ) ;
#107441 = ORIENTED_EDGE ( 'NONE', *, *, #173426, .T. ) ;
#107443 = CARTESIAN_POINT ( 'NONE',  ( -0.6823417656250039265, 14.56770833367473195, -1.181850606188755259 ) ) ;
#107442 = CARTESIAN_POINT ( 'NONE',  ( 5.547250370032299038, 1.641257983771953866, -0.8773172063531119447 ) ) ;
#107444 = CARTESIAN_POINT ( 'NONE',  ( 3.022943291168778579, -1.688106736905025995, 0.9054777632113325536 ) ) ;
#107445 = CARTESIAN_POINT ( 'NONE',  ( 0.9381830591699467092, 1.797733097909786304, 0.3167546781352030272 ) ) ;
#107446 = CARTESIAN_POINT ( 'NONE',  ( 4.801282209253342259, 8.127660309270595462, 0.8325795361681764817 ) ) ;
#107447 = CARTESIAN_POINT ( 'NONE',  ( -10.60630082101195804, 5.715768461961713953, -4.896526734066639186 ) ) ;
#107448 = CARTESIAN_POINT ( 'NONE',  ( 5.094250900851895025, 7.824382189606214233, 1.140223938556598871 ) ) ;
#107449 = CARTESIAN_POINT ( 'NONE',  ( -11.44786932348540986, 9.799999999999982947, 3.303370173849762725 ) ) ;
#107450 = LINE ( 'NONE', #173477, #46501 ) ;
#107451 = DIRECTION ( 'NONE',  ( 0.000000000000000000, 0.000000000000000000, -1.000000000000000000 ) ) ;
#107452 = CARTESIAN_POINT ( 'NONE',  ( 5.965224400332808763, 9.903252867122883885, -0.7216878364870267237 ) ) ;
#107453 = CARTESIAN_POINT ( 'NONE',  ( 5.717622241336643540, 0.3879015478767386949, -1.930678852912662391 ) ) ;
#107454 = CARTESIAN_POINT ( 'NONE',  ( -4.600294193738529103, 4.261431402316699035, -0.7998128361456221525 ) ) ;
#107455 = CARTESIAN_POINT ( 'NONE',  ( -10.62873463776380056, 13.79999999999998295, 3.199999999999997957 ) ) ;
#107456 = EDGE_CURVE ( 'NONE', #126346, #137780, #167451, .T. ) ;
#107457 = CARTESIAN_POINT ( 'NONE',  ( 1.464907584622468173, 0.1521959979720881595, -2.085151142678423497 ) ) ;
#107458 = CARTESIAN_POINT ( 'NONE',  ( 5.983413252614310451, 1.779745538724048171, -0.7376744472527080321 ) ) ;
#107459 = CARTESIAN_POINT ( 'NONE',  ( -7.067878151425722955, 7.140279352951794500, 0.7998128361456341429 ) ) ;
#107460 = CARTESIAN_POINT ( 'NONE',  ( 2.889462524698828361, 1.289687736819044472, 1.292329967842877014 ) ) ;
#107461 = CARTESIAN_POINT ( 'NONE',  ( 2.895379187063460869, 1.892502543702856865, -1.135010264495312837 ) ) ;
#107462 = CYLINDRICAL_SURFACE ( 'NONE', #141537, 10.25000000000000000 ) ;
#107463 = CARTESIAN_POINT ( 'NONE',  ( 0.7207899753199145110, 1.446443371814851941, -1.251069288267861346 ) ) ;
#107464 = ORIENTED_EDGE ( 'NONE', *, *, #208716, .T. ) ;
#107465 = CARTESIAN_POINT ( 'NONE',  ( 1.152721088564850671, -0.4753370964276568134, -1.911210599630641882 ) ) ;
#107466 = CARTESIAN_POINT ( 'NONE',  ( 2.999484396081523396, -1.939716604588328508, 0.09806999327347488971 ) ) ;
#107467 = VERTEX_POINT ( 'NONE', #40139 ) ;
#107468 = CARTESIAN_POINT ( 'NONE',  ( -11.48243876534946217, 9.719999999999998863, -3.200000000000001510 ) ) ;
#107470 = CARTESIAN_POINT ( 'NONE',  ( 6.244940914744545601, -0.2718465296328761438, -1.840820509183779263 ) ) ;
#107469 = CARTESIAN_POINT ( 'NONE',  ( -5.815521545619021460, 5.749472989502435460, -0.7998128361456362523 ) ) ;
#107471 = CARTESIAN_POINT ( 'NONE',  ( 4.411198876399872404, 6.239761003923544713, -1.599625672291273171 ) ) ;
#107473 = EDGE_CURVE ( 'NONE', #212473, #30537, #4980, .T. ) ;
#107472 = LINE ( 'NONE', #149497, #76947 ) ;
#107474 = CARTESIAN_POINT ( 'NONE',  ( 8.615316546479974136, 12.13862083994696839, 1.199719254218450271 ) ) ;
#107475 = CARTESIAN_POINT ( 'NONE',  ( -4.776215253764153346, 8.794277906025310898, -0.7998128361456362523 ) ) ;
#107476 = CARTESIAN_POINT ( 'NONE',  ( 2.138457411672203712, 0.4836887423533155483, 2.137355272389021899 ) ) ;
#107477 = CARTESIAN_POINT ( 'NONE',  ( 3.097897175693991478, 6.151267098325809535, -0.8540112008112433761 ) ) ;
#107478 = CARTESIAN_POINT ( 'NONE',  ( 4.864343252252968597, 8.897093904262280972, 0.000000000000000000 ) ) ;
#107480 =( BOUNDED_SURFACE ( )  B_SPLINE_SURFACE ( 1, 2, ( 
 ( #133663, #150955, #18781, #103259, #202858, #120650, #83793, #378, #50243, #132594, #2519, #149888, #20904, #134718, #87000, #153072, #16648, #82733, #4649, #70719, #198596, #200724, #116363, #182353, #52375, #35034, #118504, #135768, #184486, #1453, #19854, #199664, #117436, #183433, #36103, #85941, #152014, #69660, #189831, #75026, #56643, #156286, #107591, #105416, #208204, #8946, #10011, #92374, #23043, #76087, #72870, #24119, #173623, #121727, #187692, #59836, #104330, #170378, #25195, #91299, #174684, #89159, #171454, #142189, #41480, #39321, #157357, #186629, #137906, #71791, #190887, #141138, #42553, #155212, #207148, #58771, #108656, #204999, #55573, #122807, #40406, #158411, #123866, #38256, #124926, #140050, #6793, #203925, #21965, #138976, #26258, #88073, #188766, #5714, #154147, #106508, #172535, #90222, #7870, #73958, #206075, #57709, #77149, #111865, #128134, #194098, #146453, #47889, #125989, #46814, #15331, #94501, #193026, #176792, #160539, #28407, #109730, #78218, #143270, #210341, #212468, #29482, #12145, #61980, #64112, #144341, #80354, #44678, #45747, #177870, #110790, #209260, #159472, #96634, #178941, #95573, #191946, #43612, #79289, #112928, #162688, #147502, #161623, #13216, #145407, #211407, #63037, #11070, #97694, #179996, #129204, #195181, #30555, #14263, #130254, #196245, #114001, #175737, #31620, #60905, #163752, #81421, #213523, #27330, #93432, #127064, #49988, #98745, #133406, #201536, #181050, #134473, #65146, #169061, #131302, #83542, #200477, #32666, #197293, #135514, #101936, #52123, #183181, #152820, #164803, #67267, #100860, #1205, #18537, #35857, #199411, #16395, #115052, #150703, #2265, #51056, #166944, #48934, #119312, #117180, #185298, #116106, #69407, #168001, #53184, #66198, #33728, #19607, #36922, #68341, #85679, #118252, #82474, #184233, #34785, #17457, #148564, #151767, #103005, #20658, #84614, #3336, #86748, #130, #132342, #198348, #182097, #99806, #165871, #149623, #107330, #26001, #5462, #189577, #73696, #157099, #140874, #124672, #173354, #91039, #23865 ),
 ( #120394, #6542, #40141, #154956, #172278, #41225, #72620, #186369, #54257, #89972, #156024, #138719, #106254, #202604, #58517, #56386, #190629, #55321, #24936, #8688, #206885, #22786, #87821, #88903, #204737, #42290, #7613, #108401, #74770, #139794, #153893, #170124, #174425, #71542, #205821, #123614, #39070, #38004, #92110, #4396, #104076, #137652, #70467, #136584, #121472, #203672, #21710, #122549, #188511, #57454, #187443, #105157, #171196, #79021, #47621, #126803, #10811, #209004, #192759, #60641, #141939, #110535, #109473, #28147, #30288, #61715, #44416, #94242, #178673, #176536, #112665, #76886, #160281, #11883, #143006, #27068, #191693, #128930, #211144, #77959, #158165, #75832, #144080, #43353, #95310, #210076, #127883, #177608, #193833, #207952, #45484, #175481, #111600, #80086, #59575, #12942, #9757, #113733, #125732, #29220, #145138, #93176, #159210, #14002, #194907, #62766, #161359, #31356, #46545, #96373, #162425, #146190, #212205, #63841, #129998, #195988, #179739, #182916, #34532, #17197, #133143, #81160, #151503, #149359, #6012, #148305, #134207, #51868, #19340, #115850, #180788, #181835, #165607, #72082, #100603, #138193, #117989, #50787, #32411, #48671, #204203, #164543, #166679, #2005, #132084, #131046, #35593, #200216, #213270, #98477, #68071, #183982, #214304, #16128, #114788, #83271, #99544, #941, #101671, #85419, #97431, #18271, #55857, #65935, #82212, #198094, #49721, #33470, #147243, #67006, #199143, #116916, #167741, #84353, #150443, #122013, #187980, #163486, #15068, #64899, #197036, #206364, #24397, #123100, #73152, #10296, #92656, #140346, #39606, #171738, #207433, #26548, #76370, #61193, #74252, #25484, #157642, #9239, #8168, #139258, #11357, #93720, #57991, #41769, #158698, #124154, #142477, #75311, #126280, #89444, #190115, #205289, #191172, #107882, #141427, #59052, #90509, #155496, #156574, #56927, #173909, #176027, #7079, #108946, #105710, #143555, #23335, #91590, #174966, #189057, #40694, #110014, #208485, #60121, #125210, #127352, #106797, #42839, #192238, #43900, #27619 ) ),
 .UNSPECIFIED., .F., .F., .F. ) 
 B_SPLINE_SURFACE_WITH_KNOTS ( ( 2, 2 ),
 ( 3, 2, 2, 2, 2, 2, 2, 2, 2, 2, 2, 2, 2, 2, 2, 2, 2, 2, 2, 2, 2, 2, 2, 2, 2, 2, 2, 2, 2, 2, 2, 2, 2, 2, 2, 2, 2, 2, 2, 2, 2, 2, 2, 2, 2, 2, 2, 2, 2, 2, 2, 2, 2, 2, 2, 2, 2, 2, 2, 2, 2, 2, 2, 2, 2, 2, 2, 2, 2, 2, 2, 2, 2, 2, 2, 2, 2, 2, 2, 2, 2, 2, 2, 2, 2, 2, 2, 2, 2, 2, 2, 2, 2, 2, 2, 2, 2, 2, 2, 2, 2, 2, 2, 2, 2, 2, 2, 2, 2, 2, 2, 2, 2, 2, 2, 2, 2, 2, 2, 2, 3 ),
 ( 0.000000000000000000, 1.000000000000000000 ),
 ( 0.000000000000000000, 0.008333333333333333218, 0.01666666666666666644, 0.02500000000000000139, 0.03333333333333333287, 0.04166666666666666435, 0.05000000000000000278, 0.05833333333333333426, 0.06666666666666666574, 0.07499999999999999722, 0.08333333333333332871, 0.09166666666666666019, 0.1000000000000000056, 0.1083333333333333370, 0.1166666666666666685, 0.1250000000000000000, 0.1333333333333333315, 0.1416666666666666630, 0.1499999999999999944, 0.1583333333333333259, 0.1666666666666666574, 0.1749999999999999889, 0.1833333333333333204, 0.1916666666666666796, 0.2000000000000000111, 0.2083333333333333426, 0.2166666666666666741, 0.2250000000000000056, 0.2333333333333333370, 0.2416666666666666685, 0.2500000000000000000, 0.2583333333333333592, 0.2666666666666666630, 0.2750000000000000222, 0.2833333333333333259, 0.2916666666666666852, 0.2999999999999999889, 0.3083333333333333481, 0.3166666666666666519, 0.3250000000000000111, 0.3333333333333333148, 0.3416666666666666741, 0.3499999999999999778, 0.3583333333333333370, 0.3666666666666666408, 0.3750000000000000000, 0.3833333333333333592, 0.3916666666666666630, 0.4000000000000000222, 0.4083333333333333259, 0.4166666666666666852, 0.4249999999999999889, 0.4333333333333333481, 0.4416666666666666519, 0.4500000000000000111, 0.4583333333333333148, 0.4666666666666666741, 0.4749999999999999778, 0.4833333333333333370, 0.4916666666666666408, 0.5000000000000000000, 0.5083333333333333037, 0.5166666666666667185, 0.5250000000000000222, 0.5333333333333333259, 0.5416666666666666297, 0.5500000000000000444, 0.5583333333333333481, 0.5666666666666666519, 0.5749999999999999556, 0.5833333333333333703, 0.5916666666666666741, 0.5999999999999999778, 0.6083333333333332815, 0.6166666666666666963, 0.6250000000000000000, 0.6333333333333333037, 0.6416666666666667185, 0.6500000000000000222, 0.6583333333333333259, 0.6666666666666666297, 0.6750000000000000444, 0.6833333333333333481, 0.6916666666666666519, 0.6999999999999999556, 0.7083333333333333703, 0.7166666666666666741, 0.7249999999999999778, 0.7333333333333332815, 0.7416666666666666963, 0.7500000000000000000, 0.7583333333333333037, 0.7666666666666667185, 0.7750000000000000222, 0.7833333333333333259, 0.7916666666666666297, 0.8000000000000000444, 0.8083333333333333481, 0.8166666666666666519, 0.8249999999999999556, 0.8333333333333333703, 0.8416666666666666741, 0.8499999999999999778, 0.8583333333333332815, 0.8666666666666666963, 0.8750000000000000000, 0.8833333333333333037, 0.8916666666666667185, 0.9000000000000000222, 0.9083333333333333259, 0.9166666666666666297, 0.9250000000000000444, 0.9333333333333333481, 0.9416666666666666519, 0.9499999999999999556, 0.9583333333333333703, 0.9666666666666666741, 0.9749999999999999778, 0.9833333333333332815, 0.9916666666666666963, 1.000000000000000000 ),
 .UNSPECIFIED. ) 
 GEOMETRIC_REPRESENTATION_ITEM ( )  RATIONAL_B_SPLINE_SURFACE ( (
 ( 1.000000000000000000, 0.8660254037844387076, 1.000000000000000000, 0.8660254037844387076, 1.000000000000000000, 0.8660254037844387076, 1.000000000000000000, 0.8660254037844387076, 1.000000000000000000, 0.8660254037844387076, 1.000000000000000000, 0.8660254037844387076, 1.000000000000000000, 0.8660254037844387076, 1.000000000000000000, 0.8660254037844387076, 1.000000000000000000, 0.8660254037844387076, 1.000000000000000000, 0.8660254037844387076, 1.000000000000000000, 0.8660254037844387076, 1.000000000000000000, 0.8660254037844387076, 1.000000000000000000, 0.8660254037844387076, 1.000000000000000000, 0.8660254037844387076, 1.000000000000000000, 0.8660254037844387076, 1.000000000000000000, 0.8660254037844387076, 1.000000000000000000, 0.8660254037844387076, 1.000000000000000000, 0.8660254037844387076, 1.000000000000000000, 0.8660254037844387076, 1.000000000000000000, 0.8660254037844387076, 1.000000000000000000, 0.8660254037844387076, 1.000000000000000000, 0.8660254037844387076, 1.000000000000000000, 0.8660254037844387076, 1.000000000000000000, 0.8660254037844387076, 1.000000000000000000, 0.8660254037844387076, 1.000000000000000000, 0.8660254037844387076, 1.000000000000000000, 0.8660254037844387076, 1.000000000000000000, 0.8660254037844387076, 1.000000000000000000, 0.8660254037844387076, 1.000000000000000000, 0.8660254037844387076, 1.000000000000000000, 0.8660254037844387076, 1.000000000000000000, 0.8660254037844387076, 1.000000000000000000, 0.8660254037844387076, 1.000000000000000000, 0.8660254037844387076, 1.000000000000000000, 0.8660254037844387076, 1.000000000000000000, 0.8660254037844387076, 1.000000000000000000, 0.8660254037844387076, 1.000000000000000000, 0.8660254037844387076, 1.000000000000000000, 0.8660254037844387076, 1.000000000000000000, 0.8660254037844387076, 1.000000000000000000, 0.8660254037844387076, 1.000000000000000000, 0.8660254037844387076, 1.000000000000000000, 0.8660254037844387076, 1.000000000000000000, 0.8660254037844387076, 1.000000000000000000, 0.8660254037844387076, 1.000000000000000000, 0.8660254037844387076, 1.000000000000000000, 0.8660254037844387076, 1.000000000000000000, 0.8660254037844387076, 1.000000000000000000, 0.8660254037844387076, 1.000000000000000000, 0.8660254037844387076, 1.000000000000000000, 0.8660254037844387076, 1.000000000000000000, 0.8660254037844387076, 1.000000000000000000, 0.8660254037844387076, 1.000000000000000000, 0.8660254037844387076, 1.000000000000000000, 0.8660254037844387076, 1.000000000000000000, 0.8660254037844387076, 1.000000000000000000, 0.8660254037844387076, 1.000000000000000000, 0.8660254037844387076, 1.000000000000000000, 0.8660254037844387076, 1.000000000000000000, 0.8660254037844387076, 1.000000000000000000, 0.8660254037844387076, 1.000000000000000000, 0.8660254037844387076, 1.000000000000000000, 0.8660254037844387076, 1.000000000000000000, 0.8660254037844387076, 1.000000000000000000, 0.8660254037844387076, 1.000000000000000000, 0.8660254037844387076, 1.000000000000000000, 0.8660254037844387076, 1.000000000000000000, 0.8660254037844387076, 1.000000000000000000, 0.8660254037844387076, 1.000000000000000000, 0.8660254037844387076, 1.000000000000000000, 0.8660254037844387076, 1.000000000000000000, 0.8660254037844387076, 1.000000000000000000, 0.8660254037844387076, 1.000000000000000000, 0.8660254037844387076, 1.000000000000000000, 0.8660254037844387076, 1.000000000000000000, 0.8660254037844387076, 1.000000000000000000, 0.8660254037844387076, 1.000000000000000000, 0.8660254037844387076, 1.000000000000000000, 0.8660254037844387076, 1.000000000000000000, 0.8660254037844387076, 1.000000000000000000, 0.8660254037844387076, 1.000000000000000000, 0.8660254037844387076, 1.000000000000000000, 0.8660254037844387076, 1.000000000000000000, 0.8660254037844387076, 1.000000000000000000, 0.8660254037844387076, 1.000000000000000000, 0.8660254037844387076, 1.000000000000000000, 0.8660254037844387076, 1.000000000000000000, 0.8660254037844387076, 1.000000000000000000, 0.8660254037844387076, 1.000000000000000000, 0.8660254037844387076, 1.000000000000000000, 0.8660254037844387076, 1.000000000000000000, 0.8660254037844387076, 1.000000000000000000, 0.8660254037844387076, 1.000000000000000000, 0.8660254037844387076, 1.000000000000000000, 0.8660254037844387076, 1.000000000000000000, 0.8660254037844387076, 1.000000000000000000, 0.8660254037844387076, 1.000000000000000000, 0.8660254037844387076, 1.000000000000000000, 0.8660254037844387076, 1.000000000000000000, 0.8660254037844387076, 1.000000000000000000, 0.8660254037844387076, 1.000000000000000000, 0.8660254037844387076, 1.000000000000000000, 0.8660254037844387076, 1.000000000000000000, 0.8660254037844387076, 1.000000000000000000, 0.8660254037844387076, 1.000000000000000000, 0.8660254037844387076, 1.000000000000000000, 0.8660254037844387076, 1.000000000000000000, 0.8660254037844387076, 1.000000000000000000, 0.8660254037844387076, 1.000000000000000000, 0.8660254037844387076, 1.000000000000000000, 0.8660254037844387076, 1.000000000000000000, 0.8660254037844387076, 1.000000000000000000, 0.8660254037844387076, 1.000000000000000000, 0.8660254037844387076, 1.000000000000000000, 0.8660254037844387076, 1.000000000000000000, 0.8660254037844387076, 1.000000000000000000, 0.8660254037844387076, 1.000000000000000000, 0.8660254037844387076, 1.000000000000000000, 0.8660254037844387076, 1.000000000000000000, 0.8660254037844387076, 1.000000000000000000),
 ( 1.000000000000000000, 0.8660254037844387076, 1.000000000000000000, 0.8660254037844387076, 1.000000000000000000, 0.8660254037844387076, 1.000000000000000000, 0.8660254037844387076, 1.000000000000000000, 0.8660254037844387076, 1.000000000000000000, 0.8660254037844387076, 1.000000000000000000, 0.8660254037844387076, 1.000000000000000000, 0.8660254037844387076, 1.000000000000000000, 0.8660254037844387076, 1.000000000000000000, 0.8660254037844387076, 1.000000000000000000, 0.8660254037844387076, 1.000000000000000000, 0.8660254037844387076, 1.000000000000000000, 0.8660254037844387076, 1.000000000000000000, 0.8660254037844387076, 1.000000000000000000, 0.8660254037844387076, 1.000000000000000000, 0.8660254037844387076, 1.000000000000000000, 0.8660254037844387076, 1.000000000000000000, 0.8660254037844387076, 1.000000000000000000, 0.8660254037844387076, 1.000000000000000000, 0.8660254037844387076, 1.000000000000000000, 0.8660254037844387076, 1.000000000000000000, 0.8660254037844387076, 1.000000000000000000, 0.8660254037844387076, 1.000000000000000000, 0.8660254037844387076, 1.000000000000000000, 0.8660254037844387076, 1.000000000000000000, 0.8660254037844387076, 1.000000000000000000, 0.8660254037844387076, 1.000000000000000000, 0.8660254037844387076, 1.000000000000000000, 0.8660254037844387076, 1.000000000000000000, 0.8660254037844387076, 1.000000000000000000, 0.8660254037844387076, 1.000000000000000000, 0.8660254037844387076, 1.000000000000000000, 0.8660254037844387076, 1.000000000000000000, 0.8660254037844387076, 1.000000000000000000, 0.8660254037844387076, 1.000000000000000000, 0.8660254037844387076, 1.000000000000000000, 0.8660254037844387076, 1.000000000000000000, 0.8660254037844387076, 1.000000000000000000, 0.8660254037844387076, 1.000000000000000000, 0.8660254037844387076, 1.000000000000000000, 0.8660254037844387076, 1.000000000000000000, 0.8660254037844387076, 1.000000000000000000, 0.8660254037844387076, 1.000000000000000000, 0.8660254037844387076, 1.000000000000000000, 0.8660254037844387076, 1.000000000000000000, 0.8660254037844387076, 1.000000000000000000, 0.8660254037844387076, 1.000000000000000000, 0.8660254037844387076, 1.000000000000000000, 0.8660254037844387076, 1.000000000000000000, 0.8660254037844387076, 1.000000000000000000, 0.8660254037844387076, 1.000000000000000000, 0.8660254037844387076, 1.000000000000000000, 0.8660254037844387076, 1.000000000000000000, 0.8660254037844387076, 1.000000000000000000, 0.8660254037844387076, 1.000000000000000000, 0.8660254037844387076, 1.000000000000000000, 0.8660254037844387076, 1.000000000000000000, 0.8660254037844387076, 1.000000000000000000, 0.8660254037844387076, 1.000000000000000000, 0.8660254037844387076, 1.000000000000000000, 0.8660254037844387076, 1.000000000000000000, 0.8660254037844387076, 1.000000000000000000, 0.8660254037844387076, 1.000000000000000000, 0.8660254037844387076, 1.000000000000000000, 0.8660254037844387076, 1.000000000000000000, 0.8660254037844387076, 1.000000000000000000, 0.8660254037844387076, 1.000000000000000000, 0.8660254037844387076, 1.000000000000000000, 0.8660254037844387076, 1.000000000000000000, 0.8660254037844387076, 1.000000000000000000, 0.8660254037844387076, 1.000000000000000000, 0.8660254037844387076, 1.000000000000000000, 0.8660254037844387076, 1.000000000000000000, 0.8660254037844387076, 1.000000000000000000, 0.8660254037844387076, 1.000000000000000000, 0.8660254037844387076, 1.000000000000000000, 0.8660254037844387076, 1.000000000000000000, 0.8660254037844387076, 1.000000000000000000, 0.8660254037844387076, 1.000000000000000000, 0.8660254037844387076, 1.000000000000000000, 0.8660254037844387076, 1.000000000000000000, 0.8660254037844387076, 1.000000000000000000, 0.8660254037844387076, 1.000000000000000000, 0.8660254037844387076, 1.000000000000000000, 0.8660254037844387076, 1.000000000000000000, 0.8660254037844387076, 1.000000000000000000, 0.8660254037844387076, 1.000000000000000000, 0.8660254037844387076, 1.000000000000000000, 0.8660254037844387076, 1.000000000000000000, 0.8660254037844387076, 1.000000000000000000, 0.8660254037844387076, 1.000000000000000000, 0.8660254037844387076, 1.000000000000000000, 0.8660254037844387076, 1.000000000000000000, 0.8660254037844387076, 1.000000000000000000, 0.8660254037844387076, 1.000000000000000000, 0.8660254037844387076, 1.000000000000000000, 0.8660254037844387076, 1.000000000000000000, 0.8660254037844387076, 1.000000000000000000, 0.8660254037844387076, 1.000000000000000000, 0.8660254037844387076, 1.000000000000000000, 0.8660254037844387076, 1.000000000000000000, 0.8660254037844387076, 1.000000000000000000, 0.8660254037844387076, 1.000000000000000000, 0.8660254037844387076, 1.000000000000000000, 0.8660254037844387076, 1.000000000000000000, 0.8660254037844387076, 1.000000000000000000, 0.8660254037844387076, 1.000000000000000000, 0.8660254037844387076, 1.000000000000000000, 0.8660254037844387076, 1.000000000000000000, 0.8660254037844387076, 1.000000000000000000, 0.8660254037844387076, 1.000000000000000000, 0.8660254037844387076, 1.000000000000000000, 0.8660254037844387076, 1.000000000000000000, 0.8660254037844387076, 1.000000000000000000, 0.8660254037844387076, 1.000000000000000000, 0.8660254037844387076, 1.000000000000000000, 0.8660254037844387076, 1.000000000000000000, 0.8660254037844387076, 1.000000000000000000, 0.8660254037844387076, 1.000000000000000000, 0.8660254037844387076, 1.000000000000000000) ) ) 
 REPRESENTATION_ITEM ( '' )  SURFACE ( )  );
#107479 = DIRECTION ( 'NONE',  ( -0.7797859179643623628, 0.6260462619842697141, 0.000000000000000000 ) ) ;
#107482 = CARTESIAN_POINT ( 'NONE',  ( 5.893767612163585135, -2.000732204962274441, 0.2516274335107801519 ) ) ;
#107481 = CARTESIAN_POINT ( 'NONE',  ( 2.420285107995377327, 1.192830232448302441, -1.382225081888274643 ) ) ;
#107483 = CARTESIAN_POINT ( 'NONE',  ( -8.514157279702017078, 12.87700789305364069, -0.7216878364870267237 ) ) ;
#107484 = CARTESIAN_POINT ( 'NONE',  ( -4.593509350353649268, 8.487843406384373068, -0.1931319778552646749 ) ) ;
#107485 = CARTESIAN_POINT ( 'NONE',  ( 6.925078400183550364, 2.979478345347878587, 2.309228228758605450 ) ) ;
#107486 = CARTESIAN_POINT ( 'NONE',  ( 8.402302512167096893, 10.82577223566020841, -1.599625672291268286 ) ) ;
#107487 = CARTESIAN_POINT ( 'NONE',  ( 2.033698780422585006, -1.258094322230184581, -1.459052628860134648 ) ) ;
#107488 = CARTESIAN_POINT ( 'NONE',  ( 5.647302737930705696, 1.731814717071546772, -0.9215059220915235993 ) ) ;
#107489 = CARTESIAN_POINT ( 'NONE',  ( 1.500000000000001332, 15.37500000000000000, 0.000000000000000000 ) ) ;
#107490 = CARTESIAN_POINT ( 'NONE',  ( -6.015013705957189316, 10.16926642359206134, 0.7998128361456481317 ) ) ;
#107491 = CARTESIAN_POINT ( 'NONE',  ( 3.928111819657337911, 5.605883094398769195, 1.599625672291267398 ) ) ;
#107492 = CARTESIAN_POINT ( 'NONE',  ( -6.116136693096208887, 6.308116694799912771, 0.7216878364870257245 ) ) ;
#107493 = EDGE_CURVE ( 'NONE', #89199, #180510, #162723, .T. ) ;
#107494 = CARTESIAN_POINT ( 'NONE',  ( -1.874158809982213958, 3.299964346911606228, -0.4000000000000374922 ) ) ;
#107495 = CARTESIAN_POINT ( 'NONE',  ( 11.92619526913699879, 13.39999999999998259, 1.328859060402684644 ) ) ;
#107496 = CARTESIAN_POINT ( 'NONE',  ( 5.278213287142951238, -1.102824678039602269, -1.751873656341627505 ) ) ;
#107497 = CARTESIAN_POINT ( 'NONE',  ( -1.364683531250012516, 2.551041667008089320, -0.7879004041258289570 ) ) ;
#107498 = CARTESIAN_POINT ( 'NONE',  ( 5.643294731490863470, 0.9288382957042642385, 2.102849567203187053 ) ) ;
#107499 = CARTESIAN_POINT ( 'NONE',  ( 7.795575138177731844, 8.197185204069915798, 1.040834085586084257E-14 ) ) ;
#107501 = DIRECTION ( 'NONE',  ( 0.000000000000000000, 1.000000000000000000, 0.000000000000000000 ) ) ;
#107500 = CARTESIAN_POINT ( 'NONE',  ( 5.885648082108199119, 6.999582529615296700, 1.082531754730549967 ) ) ;
#107502 = CARTESIAN_POINT ( 'NONE',  ( -0.01123377539814351088, -0.5141151231248282105, -2.242550872947962404 ) ) ;
#107503 = CARTESIAN_POINT ( 'NONE',  ( -0.03749947599225316591, -9.978860283170366330, -9.579600585153681180 ) ) ;
#107504 = CARTESIAN_POINT ( 'NONE',  ( -7.422162748838431412, 7.623887726591770608, -0.7998128361456362523 ) ) ;
#107505 = CARTESIAN_POINT ( 'NONE',  ( 4.611236491138351212, -1.904185011576609465, 0.3803074441277309314 ) ) ;
#107506 = CARTESIAN_POINT ( 'NONE',  ( 8.337901282279995385, 11.71100668175994386, -1.082531754730543083 ) ) ;
#107507 = ORIENTED_EDGE ( 'NONE', *, *, #49082, .T. ) ;
#107508 = CARTESIAN_POINT ( 'NONE',  ( 6.047114369478562956, 0.1942372860762129894, 1.902532258075719351 ) ) ;
#107509 = CARTESIAN_POINT ( 'NONE',  ( 6.581054485068423610, -0.09077197429533871709, -1.722499283940544634 ) ) ;
#107510 = CARTESIAN_POINT ( 'NONE',  ( 6.192592252150040721, 1.490973663936447480, -1.357864438797616868 ) ) ;
#107512 = CARTESIAN_POINT ( 'NONE',  ( 3.374996487695185010, 6.371758841431772957, -0.9566735593157035256 ) ) ;
#107511 = CARTESIAN_POINT ( 'NONE',  ( -9.677822722056413696, 10.18521468535430685, 1.040834085586084257E-14 ) ) ;
#107513 = CARTESIAN_POINT ( 'NONE',  ( 1.642778471875000035, -2.063541666188710266, -2.845375778867859751 ) ) ;
#107515 = CARTESIAN_POINT ( 'NONE',  ( 1.340303658288226396, 0.3404796732740902887, 1.736595688552546424 ) ) ;
#107514 = CARTESIAN_POINT ( 'NONE',  ( 1.113355907768112774, -2.039295093617380594, 0.4597149659458180104 ) ) ;
#107516 = DIRECTION ( 'NONE',  ( -0.000000000000000000, 1.000000000000000000, -0.000000000000000000 ) ) ;
#107518 = CARTESIAN_POINT ( 'NONE',  ( 4.048992419199006321, -1.904907007256863904, -1.274792539085588539 ) ) ;
#107517 = CARTESIAN_POINT ( 'NONE',  ( 4.598150373690133463, 5.393538853173795111, -1.199719254218452047 ) ) ;
#107519 = CARTESIAN_POINT ( 'NONE',  ( 2.536699030922508591, -1.289252169270055370, -1.169197435003018315 ) ) ;
#107520 = STYLED_ITEM ( 'NONE', ( #124267 ), #168834 ) ;
#107521 = CARTESIAN_POINT ( 'NONE',  ( 2.319350913329641717, -1.342983818224493531, 1.096632721805221200 ) ) ;
#107522 = CARTESIAN_POINT ( 'NONE',  ( -1.360316468750026875, 2.671875000341383810, -2.602085213965210642E-14 ) ) ;
#107523 = CARTESIAN_POINT ( 'NONE',  ( 1.732617751151921404, -1.765751579927745007, -0.5880843478397956847 ) ) ;
#107524 = CARTESIAN_POINT ( 'NONE',  ( 2.893231026729268685, 0.2635377995367886861, 2.155045766152231757 ) ) ;
#107525 = CARTESIAN_POINT ( 'NONE',  ( 5.178324605415663306, 8.128796908705222535, 1.199719254218462483 ) ) ;
#107526 = CARTESIAN_POINT ( 'NONE',  ( 3.784388871581423786, -0.6371526190629381858, -1.913262240507591416 ) ) ;
#107527 = CARTESIAN_POINT ( 'NONE',  ( 1.812500000000001554, 1.451031289061194052, 1.451031289061046170 ) ) ;
#107528 =( BOUNDED_CURVE ( )  B_SPLINE_CURVE ( 2, ( #57267, #71351, #202415, #106066, #203481, #104966, #204550 ),
 .UNSPECIFIED., .F., .T. ) 
 B_SPLINE_CURVE_WITH_KNOTS ( ( 3, 2, 2, 3 ),
 ( 0.3959408239114771688, 0.3988095238095238360, 0.4047619047619047672, 0.4076306046599514343 ),
 .UNSPECIFIED. ) 
 CURVE ( )  GEOMETRIC_REPRESENTATION_ITEM ( )  RATIONAL_B_SPLINE_CURVE ( ( 0.9331000818465632340, 0.9354320710352570512, 1.000000000000000000, 0.8660254037844387076, 1.000000000000000000, 0.9354320710352564960, 0.9331000818465632340 ) ) 
 REPRESENTATION_ITEM ( '' )  );
#107529 = CARTESIAN_POINT ( 'NONE',  ( -1.500000000000013101, 3.160416667349486008, -0.8660254037844313801 ) ) ;
#107530 = CARTESIAN_POINT ( 'NONE',  ( 0.7625677631861004224, -1.397537113076696036, 1.326088851308028449 ) ) ;
#107531 = CARTESIAN_POINT ( 'NONE',  ( -1.364683531250010295, 14.38020833367473372, 0.7879004041258445001 ) ) ;
#107532 = CARTESIAN_POINT ( 'NONE',  ( 4.887093103977882436, -2.092044318328468488, -0.7474293538695072625 ) ) ;
#107533 = ORIENTED_EDGE ( 'NONE', *, *, #120547, .F. ) ;
#107534 = CARTESIAN_POINT ( 'NONE',  ( -0.2108831679770959699, 2.036692374882024037, -2.313561348563981657 ) ) ;
#107535 = CARTESIAN_POINT ( 'NONE',  ( 1.499999999999989120, 1.025000000000019007, 0.000000000000000000 ) ) ;
#107536 = CARTESIAN_POINT ( 'NONE',  ( 7.670162217029129259, 9.971608557999250166, 1.599625672291281386 ) ) ;
#107537 = CARTESIAN_POINT ( 'NONE',  ( -0.6823417656250246877, -0.1989583329919109023, 1.181850606188755259 ) ) ;
#107538 = CARTESIAN_POINT ( 'NONE',  ( 0.06548277170575435291, -1.780103896928236118, 1.328506668625312859 ) ) ;
#107539 = CARTESIAN_POINT ( 'NONE',  ( 5.090269282739749102, 1.010147525469132557, -1.681691772506640481 ) ) ;
#107541 = CARTESIAN_POINT ( 'NONE',  ( -5.992340707560165569, 8.014150130285418783, 1.443375672974064550 ) ) ;
#107540 = CARTESIAN_POINT ( 'NONE',  ( 9.571693261567961741, 11.22969222899322617, 1.082531754730548412 ) ) ;
#107542 = DIRECTION ( 'NONE',  ( 0.000000000000000000, -1.000000000000000000, 0.000000000000000000 ) ) ;
#107543 = CARTESIAN_POINT ( 'NONE',  ( 5.940765808339826037, 0.4328084161881738945, 2.220481174026817772 ) ) ;
#107544 = CARTESIAN_POINT ( 'NONE',  ( -6.292392690518223475, 6.513748691792265788, -0.7216878364870338292 ) ) ;
#107545 = CARTESIAN_POINT ( 'NONE',  ( 2.734894939886590937, -1.973151212864039605, -0.6010335745895727388 ) ) ;
#107546 = CARTESIAN_POINT ( 'NONE',  ( -6.043183783389232566, 8.073467052085995022, 1.599625672291269396 ) ) ;
#107547 = ORIENTED_EDGE ( 'NONE', *, *, #21794, .F. ) ;
#107548 = CARTESIAN_POINT ( 'NONE',  ( 1.499999999999989120, 2.056250000682817269, 1.214306433183764966E-14 ) ) ;
#107549 = CARTESIAN_POINT ( 'NONE',  ( -1.001543065824772872E-14, 4.634375000341418804, 1.575800808251672791 ) ) ;
#107550 = CARTESIAN_POINT ( 'NONE',  ( 4.270664716992385479, -1.744513905240049567, -0.6754176267826096369 ) ) ;
#107551 = CARTESIAN_POINT ( 'NONE',  ( 3.304998880318401167, 1.097559245703746855, -1.342624595404175780 ) ) ;
#107552 = CARTESIAN_POINT ( 'NONE',  ( 1.680815414582544243, 1.200268842161634097, 1.260572391871515263 ) ) ;
#107553 = CARTESIAN_POINT ( 'NONE',  ( 1.013678699313476095, -2.235087565253154107, 0.5086484811528817485 ) ) ;
#107554 = CARTESIAN_POINT ( 'NONE',  ( 0.5521677985501523001, 0.6901698128830742185, -2.096122547012829962 ) ) ;
#107555 = CARTESIAN_POINT ( 'NONE',  ( 4.581631739359020017, -0.9839878911236143999, 1.844693108308750551 ) ) ;
#107556 = CARTESIAN_POINT ( 'NONE',  ( 5.982362851901904754, -0.2873240852911072007, -1.920464370370161600 ) ) ;
#107558 = ORIENTED_EDGE ( 'NONE', *, *, #42400, .F. ) ;
#107557 = DIRECTION ( 'NONE',  ( 0.000000000000000000, -1.000000000000000000, -1.804652791718263484E-16 ) ) ;
#107559 = CARTESIAN_POINT ( 'NONE',  ( 0.1588275700346117869, 1.163271727376416376, 1.646837250247008777 ) ) ;
#107560 = CARTESIAN_POINT ( 'NONE',  ( 0.0004480315400831600455, -0.9938866557669153723, 1.873244595478529728 ) ) ;
#107561 = DIRECTION ( 'NONE',  ( 0.6483454320283789096, 0.000000000000000000, -0.7613463080411795314 ) ) ;
#107562 = CARTESIAN_POINT ( 'NONE',  ( -7.506410603460441422, 11.90922947067921278, -0.7998128361456291469 ) ) ;
#107563 = CARTESIAN_POINT ( 'NONE',  ( 7.091078035147269532, 8.231678114882006625, 1.199719254218462483 ) ) ;
#107564 = CYLINDRICAL_SURFACE ( 'NONE', #205127, 11.99999999999999112 ) ;
#107565 = CARTESIAN_POINT ( 'NONE',  ( 4.406759617291758246, 1.409692282476209924, -1.160130723419292353 ) ) ;
#107566 = CARTESIAN_POINT ( 'NONE',  ( 1.835297179245497068, 0.2165863673247066801, 2.196102686035047213 ) ) ;
#107567 = VERTEX_POINT ( 'NONE', #153891 ) ;
#107568 = CARTESIAN_POINT ( 'NONE',  ( -2.997761361953021009, 6.511488999004883205, -0.7216878364870458196 ) ) ;
#107569 = UNCERTAINTY_MEASURE_WITH_UNIT (LENGTH_MEASURE( 1.000000000000000082E-05 ), #50152, 'distance_accuracy_value', 'NONE');
#107570 = DIRECTION ( 'NONE',  ( 0.000000000000000000, -1.000000000000000000, 0.000000000000000000 ) ) ;
#107571 = CARTESIAN_POINT ( 'NONE',  ( 3.285556943749998737, -2.092708332855377051, -1.896917185911906500 ) ) ;
#107572 = CARTESIAN_POINT ( 'NONE',  ( -8.016948904382338981, 8.247528564734524892, -0.7998128361456291469 ) ) ;
#107573 = CARTESIAN_POINT ( 'NONE',  ( 1.336200995665462354, -1.125576746034629094, -1.676869184967361814 ) ) ;
#107574 = CARTESIAN_POINT ( 'NONE',  ( 11.92619526913699879, 10.19999999999998153, 1.328859060402684644 ) ) ;
#107575 = CARTESIAN_POINT ( 'NONE',  ( -3.851398154733808088, 6.650992392901508232, -1.199719254218450271 ) ) ;
#107576 = CARTESIAN_POINT ( 'NONE',  ( 2.799463494909336880, -1.375353214051901807, -1.253764128285854706 ) ) ;
#107577 = CARTESIAN_POINT ( 'NONE',  ( 2.354312230267378236, 5.898448035287240820, -0.7998128361456281477 ) ) ;
#107578 = DIRECTION ( 'NONE',  ( -3.491481338843133750E-15, -0.000000000000000000, -1.000000000000000000 ) ) ;
#107579 = VERTEX_POINT ( 'NONE', #7611 ) ;
#107580 = CARTESIAN_POINT ( 'NONE',  ( -5.091250377131585125, 5.898545847196970726, 1.199719254218450271 ) ) ;
#107581 =( GEOMETRIC_REPRESENTATION_CONTEXT ( 3 ) GLOBAL_UNCERTAINTY_ASSIGNED_CONTEXT ( ( #17857 ) ) GLOBAL_UNIT_ASSIGNED_CONTEXT ( ( #202827, #189799, #155182 ) ) REPRESENTATION_CONTEXT ( 'NONE', 'WORKASPACE' ) );
#107582 = CARTESIAN_POINT ( 'NONE',  ( -8.890396042259075315, 11.39521468743417998, -1.599625672291263179 ) ) ;
#107583 = CARTESIAN_POINT ( 'NONE',  ( 3.404746562951189937, 1.438594061741470753, -1.123979961188771304 ) ) ;
#107585 = CARTESIAN_POINT ( 'NONE',  ( -3.976064435573588796, 7.848781721302746206, 0.05846302465613295585 ) ) ;
#107584 = CARTESIAN_POINT ( 'NONE',  ( -4.167152111353897403, 5.955039778036558040, 1.599625672291270506 ) ) ;
#107586 = CARTESIAN_POINT ( 'NONE',  ( 6.127784903196001665, 7.091900248975262500, -1.102264294108054266 ) ) ;
#107587 = CARTESIAN_POINT ( 'NONE',  ( 0.1745346383498986020, -0.7352478164647980874, -1.569626033853884106 ) ) ;
#107588 = CARTESIAN_POINT ( 'NONE',  ( 6.509700743154069436, -0.8726169035938921015, -1.621212818125779220 ) ) ;
#107589 = VECTOR ( 'NONE', #47396, 1000.000000000000000 ) ;
#107590 = CARTESIAN_POINT ( 'NONE',  ( 4.776155900897590456, 1.325808183606682622, 1.888659687595494407 ) ) ;
#107591 = CARTESIAN_POINT ( 'NONE',  ( 3.379725431556547477, 7.165039780116438273, -1.734723475976807094E-15 ) ) ;
#107592 = CARTESIAN_POINT ( 'NONE',  ( 0.6497718435918962143, 0.6490781098625525436, -1.955935974237718256 ) ) ;
#107593 = CARTESIAN_POINT ( 'NONE',  ( 5.296431564432884542, 9.330920591813708143, 1.040834085586084257E-14 ) ) ;
#107594 = EDGE_CURVE ( 'NONE', #104090, #172895, #113265, .T. ) ;
#107595 = CARTESIAN_POINT ( 'NONE',  ( 6.081499288503829703, 1.550124037452194958, -1.697122508851423905 ) ) ;
#107596 = FACE_OUTER_BOUND ( 'NONE', #127837, .T. ) ;
#107597 = CARTESIAN_POINT ( 'NONE',  ( -5.562588163356775972, 9.711712967216715953, 0.7998128361456291469 ) ) ;
#107598 = CARTESIAN_POINT ( 'NONE',  ( 5.225416543158964977, -1.776039340814106637, 0.5876355328483380269 ) ) ;
#107599 = ORIENTED_EDGE ( 'NONE', *, *, #158884, .F. ) ;
#107601 = CARTESIAN_POINT ( 'NONE',  ( -5.147255595043616516, 6.034161611419515125, 1.199719254218452935 ) ) ;
#107600 = CARTESIAN_POINT ( 'NONE',  ( 1.880979024232478425, -1.749874716401520036, -0.7718601483891265325 ) ) ;
#107602 = CARTESIAN_POINT ( 'NONE',  ( 4.758537496233657293, 0.8426522330295079799, 2.039869969286691731 ) ) ;
#107603 = CARTESIAN_POINT ( 'NONE',  ( 4.768830992622041798, -0.2625661012465319022, -2.100967800990781509 ) ) ;
#107604 = CARTESIAN_POINT ( 'NONE',  ( -1.225000000000005640, 0.5625000006828015930, -1.734723475976807094E-15 ) ) ;
#107605 = CARTESIAN_POINT ( 'NONE',  ( 6.883263157960369583, 7.629137130509070275, 2.546189081643289942 ) ) ;
#107606 = CARTESIAN_POINT ( 'NONE',  ( 6.034787771414195312, 6.213209619504250547, -0.7216878364870458196 ) ) ;
#107607 = CARTESIAN_POINT ( 'NONE',  ( -4.434925645001610128, 8.188180662561590495, 0.7216878364870338292 ) ) ;
#107608 = CARTESIAN_POINT ( 'NONE',  ( 2.116686800396328838, -1.088458544310743736, -2.034734824932447506 ) ) ;
#107609 = CARTESIAN_POINT ( 'NONE',  ( 3.209375601822930690, -1.602329130913646926, -1.131729396966949963 ) ) ;
#107610 = CARTESIAN_POINT ( 'NONE',  ( 6.773846765307987461, -7.473374494058229622, 6.773846765307971474 ) ) ;
#107611 = CARTESIAN_POINT ( 'NONE',  ( 6.860222192644392258, -2.062229998417430377, 0.04471529749722201463 ) ) ;
#107612 = CARTESIAN_POINT ( 'NONE',  ( 4.202664430556257713, 4.965825259479493603, 1.082531754730560403 ) ) ;
#107613 = CARTESIAN_POINT ( 'NONE',  ( 3.067887898442204442, 6.801229324816399746, 0.7998128361456271485 ) ) ;
#107614 = VERTEX_POINT ( 'NONE', #73694 ) ;
#107615 = CARTESIAN_POINT ( 'NONE',  ( 5.384000029850495750, -2.016708404008683786, 0.004832792792668073358 ) ) ;
#107616 = CARTESIAN_POINT ( 'NONE',  ( -9.755255220232635693, 11.33988483081495957, -1.199719254218441611 ) ) ;
#107617 = CARTESIAN_POINT ( 'NONE',  ( -0.1608832656953863849, 7.629137130509072939, -2.497055476982701361 ) ) ;
#107618 = CARTESIAN_POINT ( 'NONE',  ( -11.69380381030441107, 8.410673437356566140, -1.083569014401829955 ) ) ;
#107619 = CARTESIAN_POINT ( 'NONE',  ( 7.397945374551106568, 11.78268670361832093, -0.7998128361456291469 ) ) ;
#107620 = CARTESIAN_POINT ( 'NONE',  ( 1.868283874303029446, -2.155004017527381244, 0.2628641719419066991 ) ) ;
#107621 = CARTESIAN_POINT ( 'NONE',  ( 11.89942855770814312, 11.29999999999999893, -0.7000000000000009548 ) ) ;
#107622 = SURFACE_STYLE_FILL_AREA ( #190920 ) ;
#107623 = CARTESIAN_POINT ( 'NONE',  ( -11.89197369110780045, 9.800000000000000711, -0.8056055387119882560 ) ) ;
#107624 = CARTESIAN_POINT ( 'NONE',  ( 5.469253881944042384, 7.602781119232224327, 1.336104631850141944 ) ) ;
#107625 = CARTESIAN_POINT ( 'NONE',  ( 0.9485937975238111219, 0.5957422345228384764, 1.972812641012058776 ) ) ;
#107627 = CARTESIAN_POINT ( 'NONE',  ( 6.727182134110207379, 6.038252846411742425, 2.505853901327475874 ) ) ;
#107626 = CARTESIAN_POINT ( 'NONE',  ( -0.02224634325196857970, 4.078913133451218087, -2.843768138527980049 ) ) ;
#107628 = CARTESIAN_POINT ( 'NONE',  ( 1.364683531249988757, 0.8843750003414210248, 0.000000000000000000 ) ) ;
#107629 = ORIENTED_EDGE ( 'NONE', *, *, #145579, .T. ) ;
#107630 = CARTESIAN_POINT ( 'NONE',  ( 3.756429630051653756, 1.903336793139897010, 0.1845653119916731144 ) ) ;
#107631 = B_SPLINE_CURVE_WITH_KNOTS ( 'NONE', 3,
 ( #139332, #37539, #205361, #168602, #135064, #123169 ),
 .UNSPECIFIED., .F., .F.,
 ( 4, 2, 4 ),
 ( 0.000000000000000000, 0.001226111284895901356, 0.002452222569791802712 ),
 .UNSPECIFIED. ) ;
#107632 = CARTESIAN_POINT ( 'NONE',  ( 5.049538948550310380, 0.5532318831848512808, -1.681206329525422483 ) ) ;
#107633 = CARTESIAN_POINT ( 'NONE',  ( 7.212011367826596242, 7.378711115411311638, 0.000000000000000000 ) ) ;
#107634 = CARTESIAN_POINT ( 'NONE',  ( -3.079673448598517549, 6.744702790006905424, 1.040834085586084257E-14 ) ) ;
#107636 = CARTESIAN_POINT ( 'NONE',  ( 6.239839116978105338, 1.910102730490463641, -0.1462054744419109820 ) ) ;
#107635 = CARTESIAN_POINT ( 'NONE',  ( 3.974511587100456822, 7.788680618259193444, 1.040834085586084257E-14 ) ) ;
#107637 = CARTESIAN_POINT ( 'NONE',  ( -0.7500000000000215383, 0.1916666666666871910, 1.299038105676659116 ) ) ;
#107638 = CARTESIAN_POINT ( 'NONE',  ( 0.9595327444568906294, 1.691550050060253829, 1.193477315110213599 ) ) ;
#107639 = CARTESIAN_POINT ( 'NONE',  ( 1.499999999999989120, 5.795833333333350268, -0.8660254037844323793 ) ) ;
#107640 = CARTESIAN_POINT ( 'NONE',  ( 6.508674657442179878, 1.384610780642284711, -1.258058027910214927 ) ) ;
#107641 = CARTESIAN_POINT ( 'NONE',  ( 2.596107596775329540, -1.820790993511243849, -0.1344670722737417168 ) ) ;
#107643 = CARTESIAN_POINT ( 'NONE',  ( 4.771497086726927073, 8.161215468402982509, 0.7801120568680236511 ) ) ;
#107642 = CARTESIAN_POINT ( 'NONE',  ( 6.006501602161061548, -0.7906231143557163055, -2.060575041408031272 ) ) ;
#107644 = CARTESIAN_POINT ( 'NONE',  ( 1.364683531249988757, 0.3843750003414206362, 0.000000000000000000 ) ) ;
#107645 = CARTESIAN_POINT ( 'NONE',  ( 2.752447824977616087, -2.056971473714273468, -0.1544007921008266060 ) ) ;
#107646 = CARTESIAN_POINT ( 'NONE',  ( -7.985916173649233230, 9.275655943134292869, -1.199719254218446718 ) ) ;
#107647 = CARTESIAN_POINT ( 'NONE',  ( 8.052653171512838881, 11.48218023581863001, -1.199719254218446718 ) ) ;
#107648 = CARTESIAN_POINT ( 'NONE',  ( 4.385172619016207918, 7.203452924572514959, 1.199719254218462483 ) ) ;
#107649 = AXIS2_PLACEMENT_3D ( 'NONE', #56578, #42479, #55504 ) ;
#107650 = B_SPLINE_CURVE_WITH_KNOTS ( 'NONE', 3,
 ( #15489, #161780, #78374, #145562, #179091, #30713, #98906 ),
 .UNSPECIFIED., .F., .F.,
 ( 4, 3, 4 ),
 ( -2.180065393121582080E-06, 0.000000000000000000, 4.270488675893448704E-05 ),
 .UNSPECIFIED. ) ;
#107651 = CARTESIAN_POINT ( 'NONE',  ( 0.7554163591718568993, -1.825703804718967316, -1.157005318491082901 ) ) ;
#107652 = CARTESIAN_POINT ( 'NONE',  ( 6.156284269057003655, 9.340026192945279249, -1.199719254218452047 ) ) ;
#107653 = EDGE_CURVE ( 'NONE', #80718, #164527, #136386, .T. ) ;
#107654 = CARTESIAN_POINT ( 'NONE',  ( 5.406714943436663035, 0.5975561702324573288, 1.982271326387271770 ) ) ;
#107655 = CARTESIAN_POINT ( 'NONE',  ( 1.364683531249988757, -0.5531249996585801965, 0.000000000000000000 ) ) ;
#107656 = CARTESIAN_POINT ( 'NONE',  ( 3.374459016379764087, -1.290570702369205014, 1.733878788530067938 ) ) ;
#107657 = CARTESIAN_POINT ( 'NONE',  ( -4.603364586660168456, 8.384938909114524108, 0.004600842637982396899 ) ) ;
#107659 = CARTESIAN_POINT ( 'NONE',  ( 2.189831975649577878, -1.279155337443920404, -1.487614327915102841 ) ) ;
#107658 = CARTESIAN_POINT ( 'NONE',  ( 2.649087060217536926, 0.2492969965636695762, 2.004170148778378735 ) ) ;
#107660 = CARTESIAN_POINT ( 'NONE',  ( 7.698131257602417676, -5.543994141378494334, 7.787098537122152386 ) ) ;
#107661 = PRODUCT ( 'cover for positive', 'cover for positive', '', ( #197768 ) ) ;
#107664 = CARTESIAN_POINT ( 'NONE',  ( 7.632877294813741109, 8.007371053478589573, 1.040834085586084257E-14 ) ) ;
#107663 = CARTESIAN_POINT ( 'NONE',  ( 0.000000000000000000, -0.4374999999999981126, -4.012584370867899430 ) ) ;
#107662 =( NAMED_UNIT ( * ) PLANE_ANGLE_UNIT ( ) SI_UNIT ( $, .RADIAN. ) );
#107665 = CARTESIAN_POINT ( 'NONE',  ( -6.607619761813764647, 8.802252036906432764, 1.599625672291269396 ) ) ;
#107666 = CARTESIAN_POINT ( 'NONE',  ( 1.551970632248239612, 1.040795554343958429, 1.727062486439542965 ) ) ;
#107668 = CARTESIAN_POINT ( 'NONE',  ( 6.462441986028243157, -2.002789442531027309, -0.8901952361822994542 ) ) ;
#107667 = CARTESIAN_POINT ( 'NONE',  ( -5.579343907223557331, 6.467988298970945849, 1.199719254218450271 ) ) ;
#107669 = CARTESIAN_POINT ( 'NONE',  ( 5.639828713160493834, 5.682147708216442439, 1.040834085586084257E-14 ) ) ;
#107670 = CARTESIAN_POINT ( 'NONE',  ( 5.467032840998240495, -1.503656711810175350, 1.181500457595338505 ) ) ;
#107671 = CARTESIAN_POINT ( 'NONE',  ( -4.274898507010545856, 3.881803101134051470, -0.7998128361456221525 ) ) ;
#107672 = CARTESIAN_POINT ( 'NONE',  ( 3.985733972293228344, 7.593847367743336463, 1.040834085586084257E-14 ) ) ;
#107674 = CARTESIAN_POINT ( 'NONE',  ( 3.005482631727268039, -1.942536929278560365, 0.5405117225928540714 ) ) ;
#107673 = CARTESIAN_POINT ( 'NONE',  ( -9.286972035236635392, 9.937148250638648150, -0.7216878364870267237 ) ) ;
#107675 = CARTESIAN_POINT ( 'NONE',  ( -1.499999999999997780, 3.650000000000021227, 1.214306433183764966E-14 ) ) ;
#107676 = CARTESIAN_POINT ( 'NONE',  ( -0.6823417656250039265, 13.13020833367473017, -1.181850606188755259 ) ) ;
#107677 = CARTESIAN_POINT ( 'NONE',  ( -0.005825499538506145533, -0.3671160670182890273, -1.691004160741523155 ) ) ;
#107678 = CARTESIAN_POINT ( 'NONE',  ( 7.862802741282558294, 8.137967717776607657, 0.000000000000000000 ) ) ;
#107679 = CARTESIAN_POINT ( 'NONE',  ( 9.422553571817644524, 10.09532670998316384, 0.000000000000000000 ) ) ;
#107680 = PRESENTATION_LAYER_ASSIGNMENT (  '', '', ( #200954 ) ) ;
#107681 = CARTESIAN_POINT ( 'NONE',  ( -0.4307572970103041854, 3.041534709929983205, 0.4240169840791090383 ) ) ;
#107682 = CARTESIAN_POINT ( 'NONE',  ( 4.217926093758464390, -0.9595593063399066036, -1.605508702137818045 ) ) ;
#107683 = LINE ( 'NONE', #123956, #81842 ) ;
#107684 = CARTESIAN_POINT ( 'NONE',  ( 1.622023338512183832, 2.040292009219225378, -0.3499636251925800079 ) ) ;
#107685 = CARTESIAN_POINT ( 'NONE',  ( -6.577113915960828727, 9.727031097712693253, -1.082531754730549967 ) ) ;
#107686 = EDGE_LOOP ( 'NONE', ( #177600, #37019, #191347, #42007, #81610, #147876, #89515 ) ) ;
#107687 = CARTESIAN_POINT ( 'NONE',  ( 5.564695703766185275, 5.456842840674144490, 0.000000000000000000 ) ) ;
#107688 = CARTESIAN_POINT ( 'NONE',  ( 0.03478015955125923070, -1.617804660175032661, 1.203375172262765913 ) ) ;
#107689 = CARTESIAN_POINT ( 'NONE',  ( 0.01741795466771427214, -0.4834593703179098645, 1.745828368453090418 ) ) ;
#107690 = CARTESIAN_POINT ( 'NONE',  ( 4.380693030546916944, 6.204170850428461392, 1.443375672974058777 ) ) ;
#107691 = DIRECTION ( 'NONE',  ( 0.000000000000000000, 1.000000000000000000, 0.000000000000000000 ) ) ;
#107692 = ORIENTED_EDGE ( 'NONE', *, *, #192009, .F. ) ;
#107693 = VECTOR ( 'NONE', #89009, 1000.000000000000000 ) ;
#107694 = CARTESIAN_POINT ( 'NONE',  ( 9.056483423804305488, 9.668244870634271848, 1.040834085586084257E-14 ) ) ;
#107696 = CARTESIAN_POINT ( 'NONE',  ( 6.913768267964901071, 10.15348118167935709, -1.199719254218441611 ) ) ;
#107695 = CARTESIAN_POINT ( 'NONE',  ( 1.170277241841523264, -0.8789641444944886750, -1.754005360843587047 ) ) ;
#107697 = CARTESIAN_POINT ( 'NONE',  ( 6.222283718431360633, 1.895538691748376081, 0.2756032664797089526 ) ) ;
#107698 = FACE_OUTER_BOUND ( 'NONE', #189269, .T. ) ;
#107699 = CARTESIAN_POINT ( 'NONE',  ( -4.091466733727974869, 3.979520368983120449, -0.5407646501769195480 ) ) ;
#107700 = SPHERICAL_SURFACE ( 'NONE', #122507, 0.08000000000000000167 ) ;
#107702 = ORIENTED_EDGE ( 'NONE', *, *, #51590, .T. ) ;
#107701 = CARTESIAN_POINT ( 'NONE',  ( 5.341549334104200852, 5.334155099317434257, 0.7216878364870317197 ) ) ;
#107703 = CARTESIAN_POINT ( 'NONE',  ( -8.839552966430023417, 9.415159337030921449, -0.7216878364870267237 ) ) ;
#107704 = CARTESIAN_POINT ( 'NONE',  ( 2.782270202741622178, -1.112240752214749273, 1.853481441253836071 ) ) ;
#107705 = CARTESIAN_POINT ( 'NONE',  ( -7.607533591043815768, 8.048079742405473525, 0.000000000000000000 ) ) ;
#107706 = CARTESIAN_POINT ( 'NONE',  ( 7.851580356089786328, 8.332800968292465527, 0.000000000000000000 ) ) ;
#107707 = CARTESIAN_POINT ( 'NONE',  ( -4.451154503988200339, 4.087435097607984957, 1.214306433183764966E-14 ) ) ;
#107708 = CARTESIAN_POINT ( 'NONE',  ( 5.877927443470423619, 1.089437568142386015, 1.464738158297604453 ) ) ;
#107709 = CARTESIAN_POINT ( 'NONE',  ( 8.816397291392808810, 13.32355858800980464, 7.672907388467486989 ) ) ;
#107710 = CARTESIAN_POINT ( 'NONE',  ( 1.546097919708361079, 1.968910558940571320, 0.1009371868440200049 ) ) ;
#107711 = CARTESIAN_POINT ( 'NONE',  ( 3.691585721427274258, 1.799035686688513325, -0.6489376663148455071 ) ) ;
#107712 = ORIENTED_EDGE ( 'NONE', *, *, #75384, .F. ) ;
#107713 = LINE ( 'NONE', #26382, #125564 ) ;
#107714 = CARTESIAN_POINT ( 'NONE',  ( 5.512145389550558328, 1.967385609537531277, -0.09471018678799088264 ) ) ;
#107715 = ORIENTED_EDGE ( 'NONE', *, *, #102521, .F. ) ;
#107716 = CARTESIAN_POINT ( 'NONE',  ( 6.444875487053635332, -1.562622460104126310, -1.153009275138028089 ) ) ;
#107717 = ORIENTED_EDGE ( 'NONE', *, *, #203982, .T. ) ;
#107718 = CARTESIAN_POINT ( 'NONE',  ( -3.962726036944197894, 7.845207153068690431, -0.7998128361456481317 ) ) ;
#107720 = CARTESIAN_POINT ( 'NONE',  ( 6.521762860236213655, -0.4636855090699961712, 2.076960040381255812 ) ) ;
#107719 = CARTESIAN_POINT ( 'NONE',  ( -4.285259070371116863, 7.157163461145040095, 1.199719254218452935 ) ) ;
#107722 = ADVANCED_FACE ( 'NONE', ( #88901 ), #207331, .T. ) ;
#107721 = CARTESIAN_POINT ( 'NONE',  ( 6.170369307550806148, 10.21286493553572328, 0.7216878364870317197 ) ) ;
#107724 = VERTEX_POINT ( 'NONE', #1887 ) ;
#107723 = CARTESIAN_POINT ( 'NONE',  ( 3.404848115249804685, -0.3755933644018424888, -1.874856250562627391 ) ) ;
#107725 = CARTESIAN_POINT ( 'NONE',  ( 0.8509352111321017986, 0.6423128672003556305, 2.111239891224323983 ) ) ;
#107726 = CARTESIAN_POINT ( 'NONE',  ( 9.622290429756468200, 3.756446959784728534, -7.170831222936548066 ) ) ;
#107727 = CARTESIAN_POINT ( 'NONE',  ( -0.04057498839846879202, -1.478066481919372510, -1.213044814162365981 ) ) ;
#107728 = CARTESIAN_POINT ( 'NONE',  ( -6.773846765317318663, -7.246166700180828535, 6.773846765317342644 ) ) ;
#107730 = CARTESIAN_POINT ( 'NONE',  ( 6.234959169399230561, 0.1841439077357870380, 1.816378869960999509 ) ) ;
#107729 = PRODUCT_DEFINITION_FORMATION_WITH_SPECIFIED_SOURCE ( 'ANY', '', #157772, .NOT_KNOWN. ) ;
#107731 = CARTESIAN_POINT ( 'NONE',  ( 2.488806849732328796, 2.007603858877416769, 0.5053560088097222014 ) ) ;
#107732 = CARTESIAN_POINT ( 'NONE',  ( -4.726989112658928072, 8.666571064744069020, 1.040834085586084257E-14 ) ) ;
#107733 = AXIS2_PLACEMENT_3D ( 'NONE', #89711, #7345, #103812 ) ;
#107734 = CARTESIAN_POINT ( 'NONE',  ( -5.265531293961836390, 7.681012046988098696, -1.216234931179949186 ) ) ;
#107735 = CARTESIAN_POINT ( 'NONE',  ( 1.284279953904119864, 2.827889714876734129, -0.7749999999999910294 ) ) ;
#107736 = CARTESIAN_POINT ( 'NONE',  ( 6.754772315933175619, -1.444328698515121800, 1.188528157999017454 ) ) ;
#107737 = CARTESIAN_POINT ( 'NONE',  ( 4.625302960556422427, 8.547937220624488575, 1.040834085586084257E-14 ) ) ;
#107738 = CIRCLE ( 'NONE', #14260, 0.4800000000000000933 ) ;
#107739 = CARTESIAN_POINT ( 'NONE',  ( -10.50059885609813115, 5.377696206510352184, -5.808392519734754345 ) ) ;
#107740 = CARTESIAN_POINT ( 'NONE',  ( 5.261973015879598314, 5.311592404713873172, -0.7216878364870458196 ) ) ;
#107741 = CARTESIAN_POINT ( 'NONE',  ( 0.05097232478520832832, -6.890735599539905110, 9.605899910213587134 ) ) ;
#107742 = CARTESIAN_POINT ( 'NONE',  ( 6.777182134110200096, 7.629137130509069387, 2.789055895399249696 ) ) ;
#107743 = CARTESIAN_POINT ( 'NONE',  ( -8.012344526598182026E-15, 12.10937500034140157, -1.575800808251669460 ) ) ;
#107745 = CARTESIAN_POINT ( 'NONE',  ( -7.306918443122272677, 7.489436036589583345, 0.7998128361456341429 ) ) ;
#107744 = CARTESIAN_POINT ( 'NONE',  ( 6.825078400183556049, 7.053092130845653784, 2.453807127456457238 ) ) ;
#107746 = CARTESIAN_POINT ( 'NONE',  ( 5.361839092321889488, -0.05056905708066515570, -1.733610765856267388 ) ) ;
#107747 = CARTESIAN_POINT ( 'NONE',  ( -5.278201874421821316, 5.052323696447222900, 0.7998128361456341429 ) ) ;
#107748 = CARTESIAN_POINT ( 'NONE',  ( 2.500909639826456754, 0.4493149015136475022, 2.020762751476639529 ) ) ;
#107749 = CARTESIAN_POINT ( 'NONE',  ( 3.691103677939993499, 1.816986910410453682, 1.086596289330623799 ) ) ;
#107750 = CARTESIAN_POINT ( 'NONE',  ( 6.262976894508937242, 9.394224579314053969, -1.199719254218440723 ) ) ;
#107751 = CARTESIAN_POINT ( 'NONE',  ( 1.364683531249988535, 3.655208333674750509, -0.7879004041258239610 ) ) ;
#107752 = CARTESIAN_POINT ( 'NONE',  ( 1.358185265713553136, -1.969629313231166856, -0.005369267927731942967 ) ) ;
#107753 = CARTESIAN_POINT ( 'NONE',  ( 5.593492625449885125, 6.357122791843209164, 1.180528715873955692 ) ) ;
#107755 = CARTESIAN_POINT ( 'NONE',  ( 11.88168509644349058, 12.21999999999999886, -1.685788023084331400 ) ) ;
#107754 = CARTESIAN_POINT ( 'NONE',  ( -1.737499999999997824, -1.341666666666668117, 3.009438278150925683 ) ) ;
#107756 = CARTESIAN_POINT ( 'NONE',  ( 3.310744302307960574, 2.072215845705066339, 0.9802597712869900448 ) ) ;
#107757 = CARTESIAN_POINT ( 'NONE',  ( 1.383131112650197281, 1.687622997524572677, -0.6969523973551354779 ) ) ;
#107758 = CARTESIAN_POINT ( 'NONE',  ( 5.554000203453580475, 6.508696987897830688, -1.199719254218452047 ) ) ;
#107759 = CARTESIAN_POINT ( 'NONE',  ( 5.951666246274797345, 7.966696592119163256, 1.443375672974062551 ) ) ;
#107760 = CARTESIAN_POINT ( 'NONE',  ( -8.518600588087975822, 8.832788862391110385, 1.040834085586084257E-14 ) ) ;
#107761 = CARTESIAN_POINT ( 'NONE',  ( 3.111590725901419940, 1.589763268213672420, 1.235112918372171187 ) ) ;
#107762 = CARTESIAN_POINT ( 'NONE',  ( 3.801568999928582659, -1.482573837031101016, -1.284759613706359271 ) ) ;
#107763 = CARTESIAN_POINT ( 'NONE',  ( -9.494787648271923786, 9.971673765939062406, 1.040834085586084257E-14 ) ) ;
#107764 = CARTESIAN_POINT ( 'NONE',  ( -5.215082642750900277, 9.236013516518044142, 0.000000000000000000 ) ) ;
#107765 = LINE ( 'NONE', #60009, #137094 ) ;
#107767 = CARTESIAN_POINT ( 'NONE',  ( 4.662845455860040289, -1.581648675543185334, -0.7943582009959786472 ) ) ;
#107766 = CARTESIAN_POINT ( 'NONE',  ( 5.630836714711354496, -1.890471120482087652, 0.8929869209393003215 ) ) ;
#107768 = CARTESIAN_POINT ( 'NONE',  ( -2.830620210203090181, 6.524417021870718258, 0.000000000000000000 ) ) ;
#107769 = CARTESIAN_POINT ( 'NONE',  ( 0.6213436022244859247, -2.079703760468250451, 0.6910661131078955632 ) ) ;
#107770 = CARTESIAN_POINT ( 'NONE',  ( 5.595574051893665413, -1.740516469239574704, 0.006108698158355239591 ) ) ;
#107771 = CARTESIAN_POINT ( 'NONE',  ( 7.727257484784855635, 11.10255193463598111, -1.199719254218446718 ) ) ;
#107772 = DIRECTION ( 'NONE',  ( -0.7592566023652990159, 0.6507913734559659380, -9.407858945810539579E-15 ) ) ;
#107773 = CARTESIAN_POINT ( 'NONE',  ( 6.381448165025822128, -0.6081200552338487109, -2.216719476268604438 ) ) ;
#107774 = DIRECTION ( 'NONE',  ( 0.6507913734559641616, 0.7592566023653004592, 0.000000000000000000 ) ) ;
#107775 = CARTESIAN_POINT ( 'NONE',  ( 5.079290571759123019, 1.194821443462086963, -1.256652284620445759 ) ) ;
#107776 = CARTESIAN_POINT ( 'NONE',  ( 6.004372733575126020, 2.168386774327632160, 0.1126981005201161401 ) ) ;
#107777 = DIRECTION ( 'NONE',  ( -8.638326563840814399E-31, 0.000000000000000000, -1.000000000000000000 ) ) ;
#107778 = CARTESIAN_POINT ( 'NONE',  ( -0.04742653102243841318, -1.377616979729365809, 1.608019283586498371 ) ) ;
#107779 = CARTESIAN_POINT ( 'NONE',  ( 3.156250000000002665, -1.895863743164019288, 0.7852924748301466362 ) ) ;
#107780 = CARTESIAN_POINT ( 'NONE',  ( 6.827182134110224787, 2.015384445464900587, 2.492173930675382731 ) ) ;
#107781 = CARTESIAN_POINT ( 'NONE',  ( 4.331023931135844940, 0.09395156538319178463, 1.924209479612617235 ) ) ;
#107782 = CARTESIAN_POINT ( 'NONE',  ( 1.499999999999997113, 10.67708333401613530, -0.8660254037844378194 ) ) ;
#107783 = CARTESIAN_POINT ( 'NONE',  ( 1.278328015487300462, 2.187630646761177466, -0.3845124374818161828 ) ) ;
#107784 = ORIENTED_EDGE ( 'NONE', *, *, #157376, .T. ) ;
#107785 = CARTESIAN_POINT ( 'NONE',  ( -1.500000000000011324, 4.420833333333352044, 0.8660254037844403729 ) ) ;
#107786 = CARTESIAN_POINT ( 'NONE',  ( 4.310602774141044868, 7.116454772218158809, -1.199719254218452047 ) ) ;
#107787 = CARTESIAN_POINT ( 'NONE',  ( 7.644099680006512187, 7.812537802962739697, 1.040834085586084257E-14 ) ) ;
#107788 = CARTESIAN_POINT ( 'NONE',  ( 2.315342353584739055, 1.782219222887641674, -1.325647956807120220 ) ) ;
#107789 = CARTESIAN_POINT ( 'NONE',  ( -8.107412671292051343, 10.48173408797264194, 1.443375672974090751 ) ) ;
#107790 = CARTESIAN_POINT ( 'NONE',  ( -0.02900071798685523866, 4.082342745036794618, -2.728474045032194262 ) ) ;
#107791 = CARTESIAN_POINT ( 'NONE',  ( 5.829642864196151741, 9.745074408296771296, 0.7216878364870438212 ) ) ;
#107792 = CARTESIAN_POINT ( 'NONE',  ( -8.134528978075012517, 12.43410820782212767, 1.040834085586084257E-14 ) ) ;
#107793 = MECHANICAL_DESIGN_GEOMETRIC_PRESENTATION_REPRESENTATION (  '', ( #149100 ), #35041 ) ;
#107794 = CARTESIAN_POINT ( 'NONE',  ( 7.512626515748113576, 7.937354821227203594, 0.7216878364870267237 ) ) ;
#107795 = CARTESIAN_POINT ( 'NONE',  ( 0.8971115437808926396, -0.9091470795906559932, -1.799921601489597123 ) ) ;
#107797 = CARTESIAN_POINT ( 'NONE',  ( 0.2333540202161610289, 0.003568502611739353923, -2.045944795905803471 ) ) ;
#107796 = CARTESIAN_POINT ( 'NONE',  ( 8.646349277213076334, 11.11049346154719508, 1.599625672291281386 ) ) ;
#107798 = CARTESIAN_POINT ( 'NONE',  ( -10.98997987423604528, -6.700000000000002842, 0.4694063952341869794 ) ) ;
#107799 = CARTESIAN_POINT ( 'NONE',  ( 7.322812364712459221, 7.715904978352238430, 0.000000000000000000 ) ) ;
#107800 = CARTESIAN_POINT ( 'NONE',  ( -1.364683531249997417, 3.009375000341422801, 1.214306433183764966E-14 ) ) ;
#107801 = CARTESIAN_POINT ( 'NONE',  ( 0.9304724923206836307, 0.1222484634449630542, 1.765570801851876537 ) ) ;
#107802 = CARTESIAN_POINT ( 'NONE',  ( 0.4049229342097167006, -1.081068455937021611, -1.701946057285643743 ) ) ;
#107803 = CARTESIAN_POINT ( 'NONE',  ( 5.477983384163819025, -1.699738153848131983, -0.3734572171999461232 ) ) ;
#107804 = CARTESIAN_POINT ( 'NONE',  ( 4.019262574452024062, -2.193609252165360513, 0.6655472109698862271 ) ) ;
#107805 = CARTESIAN_POINT ( 'NONE',  ( -1.364683531250000748, -0.4906249996585801409, 0.000000000000000000 ) ) ;
#107806 = CARTESIAN_POINT ( 'NONE',  ( 2.589598559577494186, -1.836209955096680613, -0.1354230481333124070 ) ) ;
#107807 = CARTESIAN_POINT ( 'NONE',  ( 10.39640486358069360, 11.02356051713265650, 0.7998128361456462443 ) ) ;
#107808 = CARTESIAN_POINT ( 'NONE',  ( 2.854317205943053271, 0.6132515345431620579, 1.719634925709014439 ) ) ;
#107809 = CARTESIAN_POINT ( 'NONE',  ( 3.902970337090125863, -1.038992709432768891, -1.728002613881730598 ) ) ;
#107810 = CARTESIAN_POINT ( 'NONE',  ( -10.64045162862669081, 11.30828174301964140, -0.7998128361456221525 ) ) ;
#107812 = CARTESIAN_POINT ( 'NONE',  ( 9.167121402339585501, 14.44227982134217569, -8.755495446810726889 ) ) ;
#107811 = CARTESIAN_POINT ( 'NONE',  ( 2.518781164845237175, 1.478067295746248400, -1.713045486838754794 ) ) ;
#107813 = CARTESIAN_POINT ( 'NONE',  ( 5.508848719172433128, 1.596710022150628294, -1.373279487321391379 ) ) ;
#107814 = CARTESIAN_POINT ( 'NONE',  ( 9.227221554775363543, 13.86401727962134878, 6.887592563684543201 ) ) ;
#107815 = CARTESIAN_POINT ( 'NONE',  ( 2.717306809760032138, -1.800131872397674471, -1.022606600864908399 ) ) ;
#107816 = CARTESIAN_POINT ( 'NONE',  ( 5.217190183160311356, 4.981143389975473568, -0.7998128361456211532 ) ) ;
#107817 = CARTESIAN_POINT ( 'NONE',  ( 1.360316468749965590, 1.067708333674703081, -0.7853790794159082322 ) ) ;
#107818 = CARTESIAN_POINT ( 'NONE',  ( 4.424552244980545446, -0.9075887007226298708, -1.916591080935086788 ) ) ;
#107819 = APPLICATION_PROTOCOL_DEFINITION ( 'draft international standard', 'automotive_design', 1998, #63005 ) ;
#107821 = CARTESIAN_POINT ( 'NONE',  ( 0.5219392174641559468, -1.029590632097213687, -1.628125521969860712 ) ) ;
#107820 = CARTESIAN_POINT ( 'NONE',  ( -3.972175818679615222, 4.696921878956699103, 1.082531754730558626 ) ) ;
#107822 = CARTESIAN_POINT ( 'NONE',  ( -4.573896719763875574, 6.429575154514868274, -1.599625672291271394 ) ) ;
#107823 = CARTESIAN_POINT ( 'NONE',  ( 9.921869487102386032, 10.46993591124128997, 0.000000000000000000 ) ) ;
#107824 = CARTESIAN_POINT ( 'NONE',  ( 4.028181036591620412, 7.713645286083276709, -0.7216878364870338292 ) ) ;
#107825 = CARTESIAN_POINT ( 'NONE',  ( 4.490901714065265615, 7.023505696618186356, 1.148426366857359771 ) ) ;
#107826 = CARTESIAN_POINT ( 'NONE',  ( 3.475000000000000533, -0.8312499990440826991, 0.000000000000000000 ) ) ;
#107827 = CARTESIAN_POINT ( 'NONE',  ( -4.066556009095094737, 6.831733546331167695, 1.199719254218464037 ) ) ;
#107828 = CARTESIAN_POINT ( 'NONE',  ( 0.7389115964958146154, 1.317144317036992973, -1.788695212975628168 ) ) ;
#107829 = CARTESIAN_POINT ( 'NONE',  ( 2.256984296129550760, -1.628445616851754263, 1.335386477757320778 ) ) ;
#107830 = CARTESIAN_POINT ( 'NONE',  ( -3.546339698426324460, 6.295090860542775779, -1.199719254218450271 ) ) ;
#107831 = CARTESIAN_POINT ( 'NONE',  ( 7.293396569147545527, 10.59638086639245280, 1.199719254218460707 ) ) ;
#107832 = CARTESIAN_POINT ( 'NONE',  ( 6.719592977537645062, 0.3186052404706584129, -1.833303987817246794 ) ) ;
#107833 = CARTESIAN_POINT ( 'NONE',  ( 6.317209508963599340, 9.457495962844502557, 1.199719254218462483 ) ) ;
#107834 =( LENGTH_UNIT ( ) NAMED_UNIT ( * ) SI_UNIT ( .MILLI., .METRE. ) );
#107835 = CARTESIAN_POINT ( 'NONE',  ( -5.912764389335557702, 8.951956649983198844, 1.082531754730550855 ) ) ;
#107836 = CARTESIAN_POINT ( 'NONE',  ( -9.164948653157999559, 10.75515685251491504, -1.082531754730539753 ) ) ;
#107837 = CARTESIAN_POINT ( 'NONE',  ( 0.2113915902133572944, 1.759560880827226947, -1.183302968686468226 ) ) ;
#107839 = CARTESIAN_POINT ( 'NONE',  ( 3.525789274851616639, 1.914599547803575330, -0.4273510147508317591 ) ) ;
#107838 = CARTESIAN_POINT ( 'NONE',  ( -0.6125000000000279110, -0.7083333333333247106, 1.060881119635904923 ) ) ;
#107840 = CARTESIAN_POINT ( 'NONE',  ( 2.219795081190904629, -2.096929600374438429, 0.5247480557022954351 ) ) ;
#107842 = CARTESIAN_POINT ( 'NONE',  ( -5.590823505525904125, 6.198478227408987351, -0.8910005059661347815 ) ) ;
#107841 = CARTESIAN_POINT ( 'NONE',  ( -5.646044625448194410, 5.551749915969804938, 0.000000000000000000 ) ) ;
#107843 = CARTESIAN_POINT ( 'NONE',  ( -0.6823417656250003738, 1.967708333674753174, -1.181850606188749264 ) ) ;
#107844 = CARTESIAN_POINT ( 'NONE',  ( 3.152039231231161587, -1.317153252834550425, 1.137565551706197775 ) ) ;
#107845 = CARTESIAN_POINT ( 'NONE',  ( 5.450014563013511726, 8.341805509282339770, -1.082531754730543083 ) ) ;
#107846 = CARTESIAN_POINT ( 'NONE',  ( -11.87988507903381219, 5.100570458969788668, 4.764376171217361566 ) ) ;
#107847 = CARTESIAN_POINT ( 'NONE',  ( 9.921869487102386032, 10.46993591124128997, 0.000000000000000000 ) ) ;
#107848 = AXIS2_PLACEMENT_3D ( 'NONE', #186492, #173482, #119433 ) ;
#107849 = EDGE_LOOP ( 'NONE', ( #93549, #146992, #27058, #51332, #76360 ) ) ;
#107850 = EDGE_CURVE ( 'NONE', #72330, #53448, #64089, .T. ) ;
#107851 = CARTESIAN_POINT ( 'NONE',  ( 2.038435264984053585, 1.930122609968443204, -0.5825652091262025767 ) ) ;
#107852 = CARTESIAN_POINT ( 'NONE',  ( 6.825078400183554272, 2.951006455646578264, 2.596623860847916188 ) ) ;
#107853 = CARTESIAN_POINT ( 'NONE',  ( -4.995253251992230581, 4.792493313604505367, 0.000000000000000000 ) ) ;
#107854 = CARTESIAN_POINT ( 'NONE',  ( 1.885558555406470660, 1.358073900086468333, 1.429321910850362753 ) ) ;
#107857 = ORIENTED_EDGE ( 'NONE', *, *, #22239, .T. ) ;
#107856 = CARTESIAN_POINT ( 'NONE',  ( -3.526529353330350336, 7.128384988945109413, -0.7216878364870458196 ) ) ;
#107855 = CARTESIAN_POINT ( 'NONE',  ( -15.75000000000000000, 13.40000000000000036, -3.600000000000002309 ) ) ;
#107858 = CARTESIAN_POINT ( 'NONE',  ( -6.739811759324840779, 7.035737605399991601, -0.7216878364870338292 ) ) ;
#107859 = CARTESIAN_POINT ( 'NONE',  ( 5.580062740476173566, 8.667767742934335828, 1.199719254218451159 ) ) ;
#107860 = EDGE_CURVE ( 'NONE', #134499, #12777, #167623, .T. ) ;
#107861 = CARTESIAN_POINT ( 'NONE',  ( -5.010620288702242853, 8.003418215864698482, -1.199719254218453823 ) ) ;
#107862 = CARTESIAN_POINT ( 'NONE',  ( 1.945969044768879552, -1.321035068824018222, -1.527795347589502972 ) ) ;
#107863 = CARTESIAN_POINT ( 'NONE',  ( -1.309956906536927201, 4.151654029309398197, 0.4145166106152409768 ) ) ;
#107864 = CARTESIAN_POINT ( 'NONE',  ( 5.368347952151684588, 1.131674353116480569, 2.010972138180310065 ) ) ;
#107865 = CARTESIAN_POINT ( 'NONE',  ( 6.848121815800094936, -0.8396676627679277027, 1.771385694100804375 ) ) ;
#107866 = CARTESIAN_POINT ( 'NONE',  ( 2.676550354755039773, 1.285117694784821518, -1.482265789204496143 ) ) ;
#107867 = CARTESIAN_POINT ( 'NONE',  ( 8.829384350997564468, 11.32403438096243775, 1.599625672291281386 ) ) ;
#107868 = CARTESIAN_POINT ( 'NONE',  ( 0.3873425458618061645, -0.6819987885887255352, -1.897696807414723574 ) ) ;
#107869 = ORIENTED_EDGE ( 'NONE', *, *, #209210, .F. ) ;
#107870 = CARTESIAN_POINT ( 'NONE',  ( 1.850927149041701192, -1.938055702826226190, -0.8530577433697658085 ) ) ;
#107873 = EDGE_LOOP ( 'NONE', ( #155945, #70031, #78055 ) ) ;
#107872 = CARTESIAN_POINT ( 'NONE',  ( -7.867809214632013770, 8.073532260025807261, 1.040834085586084257E-14 ) ) ;
#107871 = CARTESIAN_POINT ( 'NONE',  ( -2.948008335967658322, 5.526761261015804116, 1.199719254218462483 ) ) ;
#107874 = CARTESIAN_POINT ( 'NONE',  ( 2.396224210035051261, 1.478860665732561808, -1.096489538662905217 ) ) ;
#107875 = ORIENTED_EDGE ( 'NONE', *, *, #55359, .F. ) ;
#107876 = CARTESIAN_POINT ( 'NONE',  ( -7.960608749518247151, 12.43912730774665576, 0.000000000000000000 ) ) ;
#107877 = FACE_OUTER_BOUND ( 'NONE', #189745, .T. ) ;
#107878 = CARTESIAN_POINT ( 'NONE',  ( 3.217144136595586179, 1.669276650691432495, -1.307696563879121365 ) ) ;
#107879 = CARTESIAN_POINT ( 'NONE',  ( 0.6031360380127914755, -1.832534659106283659, 0.1778487281504093076 ) ) ;
#107880 = CARTESIAN_POINT ( 'NONE',  ( 0.7499999999999902300, 4.597916667349482012, -1.299038105676658228 ) ) ;
#107881 = CARTESIAN_POINT ( 'NONE',  ( 8.437251666405968464, 8.737881787095446384, 1.040834085586084257E-14 ) ) ;
#107882 = CARTESIAN_POINT ( 'NONE',  ( 6.770317605177710085, 8.992066187497757213, 1.599625672291268286 ) ) ;
#107883 = CARTESIAN_POINT ( 'NONE',  ( 4.534483719690214798, 2.020231433191475467, 0.4058933888440272031 ) ) ;
#107885 = CARTESIAN_POINT ( 'NONE',  ( 1.135996871135702024, 0.3593859243370273182, 1.805655672011026391 ) ) ;
#107884 = CARTESIAN_POINT ( 'NONE',  ( -8.688077508258798431, 9.030511935923748013, -0.7998128361456291469 ) ) ;
#107886 = CARTESIAN_POINT ( 'NONE',  ( -0.6823417656250212460, 4.551041667008086655, 1.181850606188767472 ) ) ;
#107887 =( NAMED_UNIT ( * ) SI_UNIT ( $, .STERADIAN. ) SOLID_ANGLE_UNIT ( ) );
#107888 = CARTESIAN_POINT ( 'NONE',  ( -2.972980823146582186, 6.690504403638126263, 0.000000000000000000 ) ) ;
#107889 = CARTESIAN_POINT ( 'NONE',  ( -0.08972248771637633680, -9.919998018256677597, -10.99963958991169477 ) ) ;
#107890 = AXIS2_PLACEMENT_3D ( 'NONE', #117969, #147223, #99526 ) ;
#107891 = CARTESIAN_POINT ( 'NONE',  ( 1.559489335033688251, -1.894147805384650995, -1.132260830144316888 ) ) ;
#107892 = CARTESIAN_POINT ( 'NONE',  ( 3.462467831702148668, 1.013738371934786331, 2.022624228200241348 ) ) ;
#107893 = AXIS2_PLACEMENT_3D ( 'NONE', #47971, #132428, #82557 ) ;
#107894 = CARTESIAN_POINT ( 'NONE',  ( -8.188761592974046266, 10.57664116326830595, -1.443375672974059665 ) ) ;
#107896 = EDGE_CURVE ( 'NONE', #47756, #116455, #60556, .T. ) ;
#107895 = CARTESIAN_POINT ( 'NONE',  ( 3.392628153686805259, -1.747241832701627473, -0.4783254123041839057 ) ) ;
#107897 = CARTESIAN_POINT ( 'NONE',  ( 2.782342135839787289, -0.5608490805640730104, -1.831745072482870107 ) ) ;
#107898 = CARTESIAN_POINT ( 'NONE',  ( 4.422371208857902580, 0.9731212702417373350, 1.827393648576709717 ) ) ;
#107899 = CARTESIAN_POINT ( 'NONE',  ( -1.201851678989727383E-14, 3.134375000341420137, 1.575800808251672791 ) ) ;
#107900 = CARTESIAN_POINT ( 'NONE',  ( 2.412907133309648788, 1.760172955399338823, 0.8881188249313717309 ) ) ;
#107901 = CARTESIAN_POINT ( 'NONE',  ( 1.254767684091241620, -1.520462189517374219, 1.182783339890740359 ) ) ;
#107902 = CARTESIAN_POINT ( 'NONE',  ( 3.379631771358857950, 1.185797501207178861, 1.446808710765794315 ) ) ;
#107903 = CARTESIAN_POINT ( 'NONE',  ( 2.772455145383013519, 1.235390390761299306, 1.949004725048721243 ) ) ;
#107904 = CARTESIAN_POINT ( 'NONE',  ( 3.965176940185519250, 1.595341564286660629, 0.9581005465538834365 ) ) ;
#107905 = CARTESIAN_POINT ( 'NONE',  ( 0.6823417656249899377, 4.926041667008086655, -1.181850606188754593 ) ) ;
#107906 = CARTESIAN_POINT ( 'NONE',  ( -3.411848212133334446, 7.132240014130862171, 0.7998128361456341429 ) ) ;
#107907 = CARTESIAN_POINT ( 'NONE',  ( 5.601490020740366838, 9.686822124172440596, 1.040834085586084257E-14 ) ) ;
#107908 = DIRECTION ( 'NONE',  ( 0.000000000000000000, 0.000000000000000000, -1.000000000000000000 ) ) ;
#107909 = CARTESIAN_POINT ( 'NONE',  ( 0.06524607375175436874, -1.882416456675739092, -0.9446200181052357703 ) ) ;
#107910 = EDGE_CURVE ( 'NONE', #181742, #148656, #163121, .T. ) ;
#107912 = CARTESIAN_POINT ( 'NONE',  ( 0.4019237886466816012, 8.926335450315372455, -1.499999999999998668 ) ) ;
#107911 = CARTESIAN_POINT ( 'NONE',  ( 1.364683531249988535, 3.426041667008085323, 0.7879004041258500513 ) ) ;
#107913 = CARTESIAN_POINT ( 'NONE',  ( -1.913245249192567110, 8.998828458478531189, -0.7749999999999996891 ) ) ;
#107914 = CARTESIAN_POINT ( 'NONE',  ( 2.057031522680652369, 0.4693188842763912905, 2.067847215655476134 ) ) ;
#107915 = CARTESIAN_POINT ( 'NONE',  ( 0.1936255187755825669, 1.883021768735486434, -0.7310382463305180600 ) ) ;
#107916 = CARTESIAN_POINT ( 'NONE',  ( -1.402160292154681736E-14, 0.1968750003414221628, -1.575800808251665908 ) ) ;
#107917 = CARTESIAN_POINT ( 'NONE',  ( -4.663641653420935285, 5.503632019488245319, 1.082531754730560403 ) ) ;
#107918 = ADVANCED_FACE ( 'NONE', ( #48313 ), #178245, .F. ) ;
#107919 = CARTESIAN_POINT ( 'NONE',  ( 4.123651276850781144, 7.962676922967908411, -0.7998128361456221525 ) ) ;
#107920 = CARTESIAN_POINT ( 'NONE',  ( 0.8081717762262634608, -2.151237856378166224, 0.2110218573620133986 ) ) ;
#107923 = CARTESIAN_POINT ( 'NONE',  ( 4.690757960648231695, 5.535267711253469614, 1.082531754730560403 ) ) ;
#107922 = CARTESIAN_POINT ( 'NONE',  ( 6.925078400183593885, 7.629137130509070275, 2.455651831298297338 ) ) ;
#107921 = CARTESIAN_POINT ( 'NONE',  ( 4.050854035433010480, 7.948023151305657841, 0.000000000000000000 ) ) ;
#107924 = CARTESIAN_POINT ( 'NONE',  ( -4.167152111353897403, 5.955039778036558040, 1.599625672291270506 ) ) ;
#107925 = CARTESIAN_POINT ( 'NONE',  ( 5.296111364736042937, -0.9110065213352031011, -1.799124599017036585 ) ) ;
#107927 = CARTESIAN_POINT ( 'NONE',  ( -6.089020385868862739, 8.197219431637373432, -1.443375672974066548 ) ) ;
#107926 = CARTESIAN_POINT ( 'NONE',  ( -9.517460647113315630, 10.20605163116143821, 0.7216878364870438212 ) ) ;
#107928 = CARTESIAN_POINT ( 'NONE',  ( -9.367496997608917297, 14.57669131241553728, -7.413898975919227752 ) ) ;
#107930 = CARTESIAN_POINT ( 'NONE',  ( -0.6823417656250039265, 11.31770833367473728, -1.181850606188755259 ) ) ;
#107929 = CARTESIAN_POINT ( 'NONE',  ( 0.3392369075362114961, 0.3904986559340599128, 2.228413801644222758 ) ) ;
#107931 = CARTESIAN_POINT ( 'NONE',  ( -9.646789991323334590, 11.21334206375407305, 1.199719254218462483 ) ) ;
#107933 = CARTESIAN_POINT ( 'NONE',  ( 0.2631137269465182449, 1.787087189245086583, -0.6902753917677264539 ) ) ;
#107932 = CARTESIAN_POINT ( 'NONE',  ( -6.222829318548141586, 6.362315081168691044, 0.7216878364870317197 ) ) ;
#107934 = CARTESIAN_POINT ( 'NONE',  ( -0.6823417656250246877, 0.6135416670080897639, 1.181850606188755259 ) ) ;
#107935 = CARTESIAN_POINT ( 'NONE',  ( 4.000000000000012434, 5.499999999999998224, -0.7500000000000006661 ) ) ;
#107936 = CARTESIAN_POINT ( 'NONE',  ( -1.500000000000001110, 8.770833333333337478, 0.8660254037844419273 ) ) ;
#107937 = CARTESIAN_POINT ( 'NONE',  ( 3.263966975432155415, 0.7763617936313322865, 1.540355606630551710 ) ) ;
#107938 = CARTESIAN_POINT ( 'NONE',  ( 4.167152111353856547, 5.955039778036558040, 1.599625672291262513 ) ) ;
#107939 = CARTESIAN_POINT ( 'NONE',  ( 6.638652492546827766, 7.774124658506663010, 1.199719254218452047 ) ) ;
#107940 = CARTESIAN_POINT ( 'NONE',  ( 0.7722622890447777833, -1.663610408097391691, -0.6040080933595278756 ) ) ;
#107941 = CARTESIAN_POINT ( 'NONE',  ( 2.244791168117025837, 1.953224514136771006, 0.4868699220301163089 ) ) ;
#107942 = CARTESIAN_POINT ( 'NONE',  ( 4.489439581592091777, 1.972811803287272348, -0.9889974963176446643 ) ) ;
#107943 = EDGE_LOOP ( 'NONE', ( #194964, #204189, #211346, #7404, #4193 ) ) ;
#107944 = CARTESIAN_POINT ( 'NONE',  ( 8.744645890689993095, 9.304434415334227992, -0.7216878364870197293 ) ) ;
#107946 = CARTESIAN_POINT ( 'NONE',  ( 3.198842376697589085, 1.824128004127192559, 0.8596145101084637918 ) ) ;
#107945 = CARTESIAN_POINT ( 'NONE',  ( 3.826904873358004888, 1.498484187726952799, -1.500593194838243605 ) ) ;
#107948 = VERTEX_POINT ( 'NONE', #210027 ) ;
#107947 = CARTESIAN_POINT ( 'NONE',  ( 3.199259029290311140, 1.635763741490828593, -0.7788767334107206119 ) ) ;
#107949 = CARTESIAN_POINT ( 'NONE',  ( 6.384963997392946844, 6.413822516572072807, 0.7998128361456352531 ) ) ;
#107950 = ORIENTED_EDGE ( 'NONE', *, *, #177010, .T. ) ;
#107951 = CARTESIAN_POINT ( 'NONE',  ( 1.006479672118578916, 1.419055151971573059, -1.218976214888117804 ) ) ;
#107952 = CIRCLE ( 'NONE', #201239, 6.329999999999995630 ) ;
#107953 = CARTESIAN_POINT ( 'NONE',  ( 6.041596546049881944, -1.325759876995153075, -1.255439798616593716 ) ) ;
#107955 = CARTESIAN_POINT ( 'NONE',  ( 2.026450851813020648, 0.4238854151232730461, 1.868046764376835922 ) ) ;
#107954 = CARTESIAN_POINT ( 'NONE',  ( -4.600294193738529103, 4.261431402316699035, -0.7998128361456221525 ) ) ;
#107956 = CARTESIAN_POINT ( 'NONE',  ( 1.244123718695675729, 3.233005466778238191, 0.7750000000000152323 ) ) ;
#107957 = CARTESIAN_POINT ( 'NONE',  ( -1.201851678989727383E-14, 1.134375000341418582, 1.575800808251672791 ) ) ;
#107958 = CARTESIAN_POINT ( 'NONE',  ( 2.269535221382996681, 3.870433085555836428, -11.40607948006776340 ) ) ;
#107959 = ORIENTED_EDGE ( 'NONE', *, *, #147857, .F. ) ;
#107960 = CARTESIAN_POINT ( 'NONE',  ( 5.383996398402570271, 9.295429874862735531, 0.000000000000000000 ) ) ;
#107961 = CARTESIAN_POINT ( 'NONE',  ( -4.095971805104331231, 5.871996087412059140, 1.443375672974065660 ) ) ;
#107962 = CARTESIAN_POINT ( 'NONE',  ( -7.598418745816086783, 7.829519723065708092, 0.000000000000000000 ) ) ;
#107963 = CARTESIAN_POINT ( 'NONE',  ( 3.586284538990120119, 1.181046903802232206, 1.761068336431830472 ) ) ;
#107965 = CARTESIAN_POINT ( 'NONE',  ( -12.15057777967900243, 9.234859088329544718, 2.778757836088345812 ) ) ;
#107964 = CARTESIAN_POINT ( 'NONE',  ( -0.02988540731099428513, 0.2551080090007939449, -1.761437810625957834 ) ) ;
#107966 = CARTESIAN_POINT ( 'NONE',  ( 4.850830000233872674, -1.585153962374891812, 1.171817952366477344 ) ) ;
#107967 = CARTESIAN_POINT ( 'NONE',  ( 0.1760394598168211200, 1.990691791301450575, -0.2996127288820998325 ) ) ;
#107968 = ORIENTED_EDGE ( 'NONE', *, *, #184338, .F. ) ;
#107969 = CARTESIAN_POINT ( 'NONE',  ( 0.1052747227462194346, -0.09900681772390507174, 2.115024835901352596 ) ) ;
#107970 = PRESENTATION_STYLE_ASSIGNMENT (( #124242 ) ) ;
#107971 = CARTESIAN_POINT ( 'NONE',  ( 1.838419004579601834, -1.109345826794335688, 1.747895861591180156 ) ) ;
#107972 = CARTESIAN_POINT ( 'NONE',  ( 7.503511670520385479, 7.718794801887437274, 0.7998128361456281477 ) ) ;
#107973 = CARTESIAN_POINT ( 'NONE',  ( 5.987861119090863049, 7.014868056141362551, 1.199719254218452047 ) ) ;
#107974 = CARTESIAN_POINT ( 'NONE',  ( 7.537407054554579489, 7.758339416593960536, 0.000000000000000000 ) ) ;
#107976 = CARTESIAN_POINT ( 'NONE',  ( 6.193377243344257543, 6.120028293523423812, -0.7998128361456281477 ) ) ;
#107975 = CARTESIAN_POINT ( 'NONE',  ( 3.820331522234471144, 1.985175722263971654, 0.6558375257153716831 ) ) ;
#107978 = EDGE_CURVE ( 'NONE', #150870, #165149, #149231, .T. ) ;
#107977 = CARTESIAN_POINT ( 'NONE',  ( 7.526711554241970248, 8.810193563817646734, -1.199719254218452047 ) ) ;
#107980 = ORIENTED_EDGE ( 'NONE', *, *, #5002, .F. ) ;
#107979 = CARTESIAN_POINT ( 'NONE',  ( 0.9963917123081984517, -1.767100618702711179, -0.3976972079893052459 ) ) ;
#107981 = CARTESIAN_POINT ( 'NONE',  ( 5.672569038193632451, -1.402732290180560337, 1.703733612381942653 ) ) ;
#107982 = CARTESIAN_POINT ( 'NONE',  ( 7.065207446497155708, 9.336104335703744539, 0.000000000000000000 ) ) ;
#107983 = MECHANICAL_DESIGN_GEOMETRIC_PRESENTATION_REPRESENTATION (  '', ( #145980 ), #163273 ) ;
#107984 = CARTESIAN_POINT ( 'NONE',  ( 4.050008041959299199, 0.7462531942188170841, -2.076888956485785975 ) ) ;
#107985 = CARTESIAN_POINT ( 'NONE',  ( 8.620286740190458374, 8.951422706510690830, 1.040834085586084257E-14 ) ) ;
#107986 = CARTESIAN_POINT ( 'NONE',  ( -5.935365280120787013, 6.088755149432644842, -0.6770708583819718962 ) ) ;
#107987 = CARTESIAN_POINT ( 'NONE',  ( 3.106014470790594562, -0.7728303494197851231, 1.749331318715248385 ) ) ;
#107988 = CARTESIAN_POINT ( 'NONE',  ( 10.08456733046637765, 10.65975006183261087, 0.000000000000000000 ) ) ;
#107989 = CARTESIAN_POINT ( 'NONE',  ( 5.811005889236001032, -1.634438611397070806, 1.270752202701043609 ) ) ;
#107991 = CARTESIAN_POINT ( 'NONE',  ( 3.239309987758617115, -1.907233169736745060, 1.017530501952010447 ) ) ;
#107990 = CARTESIAN_POINT ( 'NONE',  ( -1.786765180256111307E-13, 7.629137130509076492, -2.599999999999921929 ) ) ;
#107992 = CARTESIAN_POINT ( 'NONE',  ( 6.480031355044912900, -2.148842909532014289, -0.4297212958329286736 ) ) ;
#107993 = VERTEX_POINT ( 'NONE', #141894 ) ;
#107994 = ORIENTED_EDGE ( 'NONE', *, *, #39268, .F. ) ;
#107995 = CARTESIAN_POINT ( 'NONE',  ( 3.475000000000000533, -2.260416665710749839, 2.006292185433948827 ) ) ;
#107996 = CARTESIAN_POINT ( 'NONE',  ( -3.469446951953614189E-15, 3.507114751586604129, 11.99288524841339054 ) ) ;
#107997 = CARTESIAN_POINT ( 'NONE',  ( 4.386945222473598527, 7.275797305264619652, -1.199719254218452047 ) ) ;
#107998 = CARTESIAN_POINT ( 'NONE',  ( -1.364683531250014514, 15.15104166700806587, -0.7879004041258335089 ) ) ;
#107999 = CARTESIAN_POINT ( 'NONE',  ( -2.844178363816758814, 6.540234867753325076, -0.7998128361456481317 ) ) ;
#108000 = CARTESIAN_POINT ( 'NONE',  ( -6.534666852106790103, 10.56760239419251590, 0.7216878364870458196 ) ) ;
#108001 = CARTESIAN_POINT ( 'NONE',  ( 4.037295881819344956, 7.932205305423046582, -0.7998128361456362523 ) ) ;
#108002 = CARTESIAN_POINT ( 'NONE',  ( 5.559458666840932928, 1.689222788819956245, 1.196583256836199149 ) ) ;
#108003 = CARTESIAN_POINT ( 'NONE',  ( 4.037660154168158932, -1.329308714249255452, -1.394617731102282709 ) ) ;
#108004 = CARTESIAN_POINT ( 'NONE',  ( 0.2281389574181335589, 2.011207032379238591, 0.1455110067964115739 ) ) ;
#108005 =( LENGTH_UNIT ( ) NAMED_UNIT ( * ) SI_UNIT ( .MILLI., .METRE. ) );
#108006 = CARTESIAN_POINT ( 'NONE',  ( 3.923105346307896202, 5.670318552149568703, -1.599625672291269396 ) ) ;
#108007 = DIRECTION ( 'NONE',  ( 8.638326563840814399E-31, -0.000000000000000000, 1.000000000000000000 ) ) ;
#108008 = CARTESIAN_POINT ( 'NONE',  ( 0.4983068789779531160, -0.7420642642406435341, -2.062120472104383317 ) ) ;
#108009 = CARTESIAN_POINT ( 'NONE',  ( 4.775911370473768791, 1.053640644303525331, 1.490772598166143048 ) ) ;
#108010 = EDGE_CURVE ( 'NONE', #56038, #140828, #42242, .T. ) ;
#108011 = CARTESIAN_POINT ( 'NONE',  ( 4.882344714696929877, 8.710169577206153591, -0.7216878364870458196 ) ) ;
#108012 = CARTESIAN_POINT ( 'NONE',  ( 2.846849068745292755, 6.265148313604064434, 0.000000000000000000 ) ) ;
#108013 = CARTESIAN_POINT ( 'NONE',  ( -4.281342646865346602, 8.216926531310035031, 0.7998128361456352531 ) ) ;
#108014 = CARTESIAN_POINT ( 'NONE',  ( 5.876533236880477240, 5.820653295974182129, 0.7998128361456352531 ) ) ;
#108015 = ORIENTED_EDGE ( 'NONE', *, *, #109929, .F. ) ;
#108017 = CARTESIAN_POINT ( 'NONE',  ( 5.695569903961543723, 1.858472494656268958, -0.7744561248179144819 ) ) ;
#108016 = CARTESIAN_POINT ( 'NONE',  ( 2.806014743833367131, 1.331929863061011465, -1.271513748034671654 ) ) ;
#108018 = CARTESIAN_POINT ( 'NONE',  ( 0.6854589470919645322, -1.231871052372325526, -1.940221060253940699 ) ) ;
#108019 = CARTESIAN_POINT ( 'NONE',  ( 6.438335799692933570, -1.052282694883142078, 1.655480336553965648 ) ) ;
#108020 = CARTESIAN_POINT ( 'NONE',  ( -5.205440912643032547, 8.160432600470439723, 1.199719254218452047 ) ) ;
#108021 = CARTESIAN_POINT ( 'NONE',  ( 0.4350687514514707255, -7.666862915010147717, -10.91132967064556070 ) ) ;
#108022 = CARTESIAN_POINT ( 'NONE',  ( -2.598358995313378550, 6.183169261174235487, 0.7998128361456341429 ) ) ;
#108023 = DIRECTION ( 'NONE',  ( 0.000000000000000000, 0.000000000000000000, -1.000000000000000000 ) ) ;
#108024 = CARTESIAN_POINT ( 'NONE',  ( -3.474632506852224356, 7.275764701294714420, -0.7998128361456481317 ) ) ;
#108026 = CARTESIAN_POINT ( 'NONE',  ( 1.006479672118578916, 1.419055151971573059, -1.218976214888117804 ) ) ;
#108025 = CARTESIAN_POINT ( 'NONE',  ( 2.806283438348840420, 1.512464495701435929, -1.443730951476623670 ) ) ;
#108027 = CARTESIAN_POINT ( 'NONE',  ( 2.038435264984053585, 1.930122609968443204, -0.5825652091262025767 ) ) ;
#108028 = CARTESIAN_POINT ( 'NONE',  ( 8.053180056837369705, 11.37883191874353805, -1.082531754730543083 ) ) ;
#108029 = VERTEX_POINT ( 'NONE', #174377 ) ;
#108030 = CARTESIAN_POINT ( 'NONE',  ( -1.364683531250012516, 3.801041667008087099, -0.7879004041258300672 ) ) ;
#108031 = CARTESIAN_POINT ( 'NONE',  ( 2.612550116648149512, -0.1684838578246611873, 1.732238525843646570 ) ) ;
#108032 = CARTESIAN_POINT ( 'NONE',  ( 4.985647801523278133, 6.839675073242382553, -1.599625672291256295 ) ) ;
#108034 = CYLINDRICAL_SURFACE ( 'NONE', #44311, 0.09999999999999971412 ) ;
#108033 =( NAMED_UNIT ( * ) PLANE_ANGLE_UNIT ( ) SI_UNIT ( $, .RADIAN. ) );
#108035 = CARTESIAN_POINT ( 'NONE',  ( 2.719059632816126282, -0.1691219839104734501, 1.716555610488319505 ) ) ;
#108036 = CARTESIAN_POINT ( 'NONE',  ( 3.122796855005858241, 0.05607861761174406934, 2.191015320347329709 ) ) ;
#108037 = CARTESIAN_POINT ( 'NONE',  ( 4.723365791888975096, -0.1103408873950258995, 2.204240794804641190 ) ) ;
#108038 = CARTESIAN_POINT ( 'NONE',  ( -11.75342398721120141, 4.618418902329548992, -5.022351803590792585 ) ) ;
#108039 = SURFACE_STYLE_USAGE ( .BOTH. , #171902 ) ;
#108040 = CARTESIAN_POINT ( 'NONE',  ( 1.973704989461112946, -0.2689809023317759618, 2.154309762211854107 ) ) ;
#108041 = CARTESIAN_POINT ( 'NONE',  ( 1.101864800459760207, -1.825872481749410525, -0.002338443969775172437 ) ) ;
#108042 = CARTESIAN_POINT ( 'NONE',  ( 3.555961197718297218, 1.179765190368966321, 1.758020836099948747 ) ) ;
#108043 = MECHANICAL_DESIGN_GEOMETRIC_PRESENTATION_REPRESENTATION (  '', ( #194545 ), #4186 ) ;
#108044 = DIRECTION ( 'NONE',  ( -1.000000000000000000, 0.000000000000000000, 0.000000000000000000 ) ) ;
#108045 = ORIENTED_EDGE ( 'NONE', *, *, #95054, .F. ) ;
#108047 = CARTESIAN_POINT ( 'NONE',  ( 1.364683531249988757, 1.946875000341415030, 0.000000000000000000 ) ) ;
#108046 = CARTESIAN_POINT ( 'NONE',  ( 3.755682109644884026, 2.274985096322924338, -0.2814536430481278662 ) ) ;
#108048 = CARTESIAN_POINT ( 'NONE',  ( 0.3282377607281221632, 2.676335450315374676, -1.225000000000002753 ) ) ;
#108049 = CARTESIAN_POINT ( 'NONE',  ( 5.040934186182656873, 4.775511393501539636, 1.040834085586084257E-14 ) ) ;
#108050 = CARTESIAN_POINT ( 'NONE',  ( 5.654997643673960184, 0.4312606369310955645, 2.178877383265501066 ) ) ;
#108051 = CARTESIAN_POINT ( 'NONE',  ( -5.748293942514180799, 7.729428904398431222, -1.443375672974052559 ) ) ;
#108052 = EDGE_CURVE ( 'NONE', #38980, #29585, #115691, .T. ) ;
#108053 = CARTESIAN_POINT ( 'NONE',  ( 4.256897045010922476, 5.029096643009940415, -1.082531754730548412 ) ) ;
#108054 = CARTESIAN_POINT ( 'NONE',  ( -6.900736999231456004, 8.113576589600553390, 1.082531754730549967 ) ) ;
#108055 = CARTESIAN_POINT ( 'NONE',  ( 3.255366281057017197, 6.812028071292901998, -0.7216878364870338292 ) ) ;
#108056 = VERTEX_POINT ( 'NONE', #144031 ) ;
#108057 = CARTESIAN_POINT ( 'NONE',  ( 4.219375079941334761, 1.978050461189932552, 0.3905991720301109082 ) ) ;
#108059 = CARTESIAN_POINT ( 'NONE',  ( 2.975492196776472031, -0.2068670369150918398, 2.052202205628439913 ) ) ;
#108058 = CARTESIAN_POINT ( 'NONE',  ( 5.113396490648394632, 9.117379672398465473, 1.040834085586084257E-14 ) ) ;
#108060 = CARTESIAN_POINT ( 'NONE',  ( -4.092446641025072829, 3.979529022206003575, 0.4031905389056175126 ) ) ;
#108061 = CARTESIAN_POINT ( 'NONE',  ( 5.383996397958233260, 5.453953017138946535, -0.7216878364870458196 ) ) ;
#108062 = CARTESIAN_POINT ( 'NONE',  ( 3.285556943749998737, -3.405208332855374831, -1.896917185911906500 ) ) ;
#108063 = CARTESIAN_POINT ( 'NONE',  ( 6.527279143455773536, -1.428284688129980440, -1.662137905815167294 ) ) ;
#108064 = CARTESIAN_POINT ( 'NONE',  ( 3.568982563115063567, -0.9913999084223242830, 1.755768870528086056 ) ) ;
#108065 = CARTESIAN_POINT ( 'NONE',  ( 2.964219115174483665, -1.702287218311925310, -0.7022057971969236645 ) ) ;
#108066 = CARTESIAN_POINT ( 'NONE',  ( 5.957918438201454059, 9.038323046955323292, -1.199719254218440723 ) ) ;
#108067 = CARTESIAN_POINT ( 'NONE',  ( 6.211906940382025510, -1.811394037990306627, 0.2264786762415857968 ) ) ;
#108068 = CARTESIAN_POINT ( 'NONE',  ( -5.879432169820529630, 10.01108796476595764, -0.7998128361456221525 ) ) ;
#108069 = CARTESIAN_POINT ( 'NONE',  ( 0.2282871097136250915, -1.394050316402313916, -1.782836666206646603 ) ) ;
#108070 = CARTESIAN_POINT ( 'NONE',  ( 2.139418596640904280, -1.880839966478216052, 0.9477614987608102837 ) ) ;
#108071 = CARTESIAN_POINT ( 'NONE',  ( -6.123442655227560927, 7.173046514967467147, 1.199719254218452047 ) ) ;
#108072 = CARTESIAN_POINT ( 'NONE',  ( 7.065770611016287006, 11.39514947949436774, 1.040834085586084257E-14 ) ) ;
#108073 = CARTESIAN_POINT ( 'NONE',  ( 7.810905894804431426, 8.285347430126213553, 0.000000000000000000 ) ) ;
#108074 = CARTESIAN_POINT ( 'NONE',  ( -7.497822643557261024, 8.706213491360317747, -1.199719254218446718 ) ) ;
#108075 = CARTESIAN_POINT ( 'NONE',  ( 7.987977580929924493, -5.530730635397370420, 7.987977580929896071 ) ) ;
#108076 = EDGE_CURVE ( 'NONE', #86666, #152917, #128882, .T. ) ;
#108077 = CARTESIAN_POINT ( 'NONE',  ( 8.405692050348340771, 8.908988268268968724, 1.040834085586084257E-14 ) ) ;
#108078 = CARTESIAN_POINT ( 'NONE',  ( 4.193481561896174270, 7.343914482741291216, -0.8359065270147625348 ) ) ;
#108079 = CARTESIAN_POINT ( 'NONE',  ( -3.588104209110990706, 7.337872010604796991, 1.040834085586084257E-14 ) ) ;
#108080 = CARTESIAN_POINT ( 'NONE',  ( 3.603960747418310184, 1.611073206568460758, 1.529666071269941474 ) ) ;
#108081 = CARTESIAN_POINT ( 'NONE',  ( 0.7795418844130063141, 1.474435645617519164, 1.621430000501473900 ) ) ;
#108082 = CARTESIAN_POINT ( 'NONE',  ( 0.7860941533469123499, 1.484900681275106438, 1.632775826992872492 ) ) ;
#108083 = CARTESIAN_POINT ( 'NONE',  ( -4.716257332707368910, 6.595662536282280719, -1.599625672291271394 ) ) ;
#108084 = CARTESIAN_POINT ( 'NONE',  ( 4.826587731031282580, -1.282962940432516907, 1.484285152025546672 ) ) ;
#108085 = CARTESIAN_POINT ( 'NONE',  ( 9.511208455186636712, 11.05516360492796935, 1.199719254218453823 ) ) ;
#108086 = CARTESIAN_POINT ( 'NONE',  ( -5.429614816329291216, 6.304498938506903016, 1.045551501023216368 ) ) ;
#108087 = CARTESIAN_POINT ( 'NONE',  ( 3.195971524519376494, 4.751719416737803847, -1.599625672291262513 ) ) ;
#108088 = CARTESIAN_POINT ( 'NONE',  ( -0.6823417656250246877, 0.5510416670080897639, 1.181850606188755259 ) ) ;
#108089 = CARTESIAN_POINT ( 'NONE',  ( -3.187575512988701565, 6.732938841879847480, 0.000000000000000000 ) ) ;
#108091 = ORIENTED_EDGE ( 'NONE', *, *, #209517, .F. ) ;
#108090 = CARTESIAN_POINT ( 'NONE',  ( -6.073689629242165822, 7.148687991279732756, -1.082531754730544860 ) ) ;
#108092 = CARTESIAN_POINT ( 'NONE',  ( 3.533539421053989660, -0.1523460092780377639, 2.115156586662121363 ) ) ;
#108093 = CARTESIAN_POINT ( 'NONE',  ( -3.447516199624892419, 7.244129009529488350, 0.7998128361456352531 ) ) ;
#108094 = CARTESIAN_POINT ( 'NONE',  ( 5.559502693676295237, 0.4258712887980077300, -2.119171757835013548 ) ) ;
#108095 = CARTESIAN_POINT ( 'NONE',  ( 4.282634502089007533, 1.642705626968201216, -0.8318752211165169053 ) ) ;
#108096 = CARTESIAN_POINT ( 'NONE',  ( 5.454314652423888354, -1.275559214091715354, 1.561879324423600668 ) ) ;
#108097 = CARTESIAN_POINT ( 'NONE',  ( -5.565401824202027115, 6.214873266482019432, 0.9197014482419992865 ) ) ;
#108098 = CARTESIAN_POINT ( 'NONE',  ( -1.201851678989727383E-14, 1.884375000341422135, 1.575800808251672791 ) ) ;
#108099 = CARTESIAN_POINT ( 'NONE',  ( 0.1865103356883268948, 1.287481616103260063, 1.171338548376497535 ) ) ;
#108100 = CARTESIAN_POINT ( 'NONE',  ( 6.827182134110164391, 0.5838490905608649806, 1.963161153048794905 ) ) ;
#108101 = CARTESIAN_POINT ( 'NONE',  ( 3.470524135418292300, 5.072030796119872953, -1.443375672974057666 ) ) ;
#108102 = CARTESIAN_POINT ( 'NONE',  ( 10.50000000000000178, 10.89999999999998259, 3.599999999999999201 ) ) ;
#108103 = CARTESIAN_POINT ( 'NONE',  ( 4.364260218091946975, 1.016419123106377276, 1.907829002176253175 ) ) ;
#108104 = CIRCLE ( 'NONE', #69962, 0.04999999999999985706 ) ;
#108105 = CARTESIAN_POINT ( 'NONE',  ( 5.343124974464078747, -1.122324884721880078, 1.674632237393176792 ) ) ;
#108106 = CARTESIAN_POINT ( 'NONE',  ( -8.975134502122321223, 9.573337795338607847, 1.040834085586084257E-14 ) ) ;
#108108 = CARTESIAN_POINT ( 'NONE',  ( 3.590839768554392908, -0.4196827604958653923, -2.120402733634827452 ) ) ;
#108107 = AXIS2_PLACEMENT_3D ( 'NONE', #31718, #147600, #182203 ) ;
#108109 = CARTESIAN_POINT ( 'NONE',  ( 3.690661264905565009, -0.3812834177611671982, -1.933973196684968920 ) ) ;
#108110 = CARTESIAN_POINT ( 'NONE',  ( -0.07626876867936756288, -1.353788312843669406, -1.724171373301164767 ) ) ;
#108111 = CARTESIAN_POINT ( 'NONE',  ( 1.220229771213819481, -2.250799921053967090, 0.5081616799173671595 ) ) ;
#108112 = CARTESIAN_POINT ( 'NONE',  ( 3.708323652925065161, -0.8317495340520587588, -1.885651027073296904 ) ) ;
#108113 = CARTESIAN_POINT ( 'NONE',  ( 5.987830644705256056, -1.933104919717167025, -0.1861817195589876295 ) ) ;
#108115 = VERTEX_POINT ( 'NONE', #206839 ) ;
#108114 = CARTESIAN_POINT ( 'NONE',  ( -8.337901282280023807, 8.829899038855916871, 0.7216878364870438212 ) ) ;
#108116 = CARTESIAN_POINT ( 'NONE',  ( -6.631873415740034083, 7.766215735565355160, 1.199719254218452047 ) ) ;
#108117 = CARTESIAN_POINT ( 'NONE',  ( 6.889999999999967706, 0.005249217920031542736, 1.719840535937327441 ) ) ;
#108118 = ADVANCED_FACE ( 'NONE', ( #208961 ), #157383, .T. ) ;
#108120 = ORIENTED_EDGE ( 'NONE', *, *, #147025, .F. ) ;
#108119 = CARTESIAN_POINT ( 'NONE',  ( -4.468294144155606773, 7.370704380560280100, 1.199719254218452935 ) ) ;
#108121 = CARTESIAN_POINT ( 'NONE',  ( -6.493992390821436977, 10.52014885602626393, 0.7216878364870458196 ) ) ;
#108122 = CARTESIAN_POINT ( 'NONE',  ( 2.837189949676882428, 0.2689455771197127310, 2.190246129917215789 ) ) ;
#108123 = CARTESIAN_POINT ( 'NONE',  ( -1.642778471874998480, -3.288541666188707246, 2.845375778867863303 ) ) ;
#108124 = CARTESIAN_POINT ( 'NONE',  ( 6.280128941539553367, -1.086961472313338284, -1.632890767417946032 ) ) ;
#108125 = CARTESIAN_POINT ( 'NONE',  ( 6.539320575229230492, 2.428701779328062749, 2.485127258459709054 ) ) ;
#108126 = CARTESIAN_POINT ( 'NONE',  ( -1.500000000000011324, 4.202083334016156080, 0.8660254037844403729 ) ) ;
#108127 = CARTESIAN_POINT ( 'NONE',  ( 4.536316240020330071, 7.212700717958764329, -1.298556639521078582 ) ) ;
#108129 = FACE_OUTER_BOUND ( 'NONE', #28388, .T. ) ;
#108128 = PLANE ( 'NONE',  #135438 ) ;
#108130 = CARTESIAN_POINT ( 'NONE',  ( 4.892441406782114477, 1.528958278715689234, -1.025397978904031060 ) ) ;
#108131 = ORIENTED_EDGE ( 'NONE', *, *, #120712, .T. ) ;
#108132 = CARTESIAN_POINT ( 'NONE',  ( 2.448182087220668102, 2.060414928722671402, 0.05179878229087316738 ) ) ;
#108133 = CARTESIAN_POINT ( 'NONE',  ( 0.6801582343750038895, 0.3072916670080680368, -1.178068619123848526 ) ) ;
#108134 = CARTESIAN_POINT ( 'NONE',  ( -6.235860587281615075, 9.362588887548838557, -1.199719254218440723 ) ) ;
#108135 = CARTESIAN_POINT ( 'NONE',  ( 10.91805698906627242, -9.914767083041231999, -0.1897524941850662061 ) ) ;
#108136 = CARTESIAN_POINT ( 'NONE',  ( 6.469000917296717112, -1.638331675554663747, 1.346054232038436105 ) ) ;
#108137 = CARTESIAN_POINT ( 'NONE',  ( 4.497554271431305040, 6.270232621468402989, -1.599625672291256295 ) ) ;
#108138 = VECTOR ( 'NONE', #89914, 1000.000000000000000 ) ;
#108139 = CARTESIAN_POINT ( 'NONE',  ( 0.8134386948647929216, -0.3029782207385351422, 2.038374528180360912 ) ) ;
#108140 = EDGE_CURVE ( 'NONE', #206526, #27864, #132043, .T. ) ;
#108142 = CARTESIAN_POINT ( 'NONE',  ( 4.511176471348508521, -1.804767551675333204, 0.3638508048048467169 ) ) ;
#108141 = CARTESIAN_POINT ( 'NONE',  ( -11.04536101718726293, 0.000000000000000000, 1.099999999999996758 ) ) ;
#108143 = CARTESIAN_POINT ( 'NONE',  ( 5.784525094524856748, 9.900363043587685041, 1.040834085586084257E-14 ) ) ;
#108144 = CARTESIAN_POINT ( 'NONE',  ( -4.911830889935877131, 4.710851378956548707, 0.3897001052374938213 ) ) ;
#108145 =( BOUNDED_SURFACE ( )  B_SPLINE_SURFACE ( 1, 2, ( 
 ( #39120, #139841, #6589, #22836, #105203, #70514, #122596, #173406, #171240, #204784, #88950, #155004, #189626, #87868, #172324, #72668, #188559, #106302, #90018, #205870, #57504, #86800, #123663, #41274, #104126, #91090, #136629, #202656, #54305, #24987, #186417, #20342, #68004, #168739, #34466, #182847, #201216, #85356, #21393, #116846, #18202, #183918, #33400, #84286, #200152, #167673, #152493, #870, #166612, #3009, #69079, #199075, #37677, #35530, #118990, #135199, #52857, #184969, #66935, #102681, #181767, #202278, #87504, #133077, #99479, #120066, #51806, #150372, #117924, #36594, #103754, #132016, #115778, #149289, #169804, #70147, #153568, #86428, #17130, #19274, #100537, #50721, #65867, #4076, #198026, #1942, #165537, #136258, #53930, #83206, #186042, #134144, #49655, #101606, #151438, #88577, #156780, #26752, #56064, #203346, #72285, #138393, #157844, #92853, #122222, #25680, #6215, #123294, #108079, #140553, #187114, #41967, #188182, #191374, #207631, #91788, #154634, #8366, #5137, #39817, #54998, #204411, #105924, #9440, #71213, #171949, #75510, #23538, #189258, #74449, #206566, #89647, #137330, #174108, #43040, #125407, #155700, #109152, #7282, #58193, #121150, #24608, #124352, #73359, #141622, #175165, #139464, #170874, #205494, #57128, #59249, #107002, #40897, #173027, #38747, #190309, #104829, #90717, #22465, #203335, #54988, #182838, #133067, #153557, #152484, #37667, #166602, #4066, #134135, #17119, #150363, #1933, #19264, #67993, #84276, #200142, #135189, #121140, #83196, #117914, #199065, #149278, #5128, #66925, #103743, #85346, #18191, #101595, #186031, #183907, #100527, #51796, #69069, #167663, #187103, #165527, #116837, #151427, #202268, #35518, #3000, #71203, #38737, #52844, #201205, #118979, #184958, #50711, #34455, #137319, #36584, #102671, #168729, #20331, #169794, #86417, #70136, #136248, #53919, #859, #120056, #21383, #87492, #92842, #124341, #60306, #190299, #105913, #104819, #88567, #173017, #192428, #158886, #10482, #154625, #157833, #91776, #191361, #171938, #9430, #73349, #170865, #89637, #155689, #24598, #7272, #23529, #139452, #74439, #126465, #22455, #57118, #138383, #6205, #76556, #72274, #43028, #90707, #205484, #40887, #125396, #123285, #39807, #189248, #8355, #106992, #204401, #56054, #122211, #156769, #141611, #140541, #206555, #142666, #188173, #58183, #41956, #108068, #174096, #25669, #75500, #208677, #207620, #59237, #109140, #175153, #26739, #127544, #77626, #94973, #61385, #65605, #159952, #163159, #144812, #32080, #63520, #213985, #129672, #45156, #44083, #27814, #112337, #131755, #98168, #164216, #93911, #97107, #161019, #79755, #28889, #111270, #128607, #110202, #31033, #14744, #12614, #11556, #96043, #212943, #78687, #177273, #209743, #64580, #80836, #15803, #210819, #47291, #13685, #62444, #194574, #46220, #178349, #29957, #162096, #145871, #143748, #211879, #193515, #130721, #179412, #146926, #195657, #113406, #196712, #48353, #114464, #180464, #81889, #147975, #176212, #166334, #50458, #149020, #197760, #1673, #20064, #595, #150101, #21113, #87219, #66661, #165271, #185764, #34194, #200935, #167409, #116577, #67727, #17926, #182572, #100269, #84010, #133878, #181512, #199885, #132808, #152224, #118711, #86153, #198812, #51530, #117655, #99221, #134930, #19001, #183648, #184699, #35252, #101328, #85082, #151166, #49398, #2737, #3795, #68808, #52583, #153283, #4859, #36320, #16866, #37396, #102398, #69869, #168466, #135978, #201993, #115517, #53651, #119783, #103471, #169533, #70938, #33141, #82946, #92592, #203074, #89372, #170594, #54718, #191104, #38473, #9169, #205213, #138120, #73082, #157576, #155421, #72007, #105636, #40624, #139183, #158634, #137048, #88296, #56855, #173835, #204129, #39535, #42772, #10231, #24329, #123029, #90437, #188980, #104550, #22180, #108879, #55782, #156505, #154357, #5936, #75244, #121939, #187905, #171664, #23260, #120867, #7005, #41700, #106727, #125147, #8094, #186841, #74183, #172754, #140276, #206295, #57920, #124085, #174903, #26482, #190048, #107810, #25412, #91517, #141356, #207370, #58990, #142413, #66146 ),
 ( #78435, #180999, #147453, #43833, #175959, #199361, #77371, #32618, #27554, #109949, #165823, #159693, #93650, #127284, #11292, #100810, #192172, #198297, #177015, #67219, #98696, #34737, #164754, #143486, #76306, #60055, #213476, #166895, #133355, #51008, #126210, #132291, #193255, #115001, #61124, #209483, #160762, #208421, #49938, #116059, #44902, #111010, #131256, #33679, #28632, #94719, #12356, #99754, #182049, #117129, #65100, #82425, #48882, #197243, #16344, #148515, #81, #17407, #83490, #149573, #1157, #183131, #184188, #187391, #153843, #121420, #35809, #201487, #167951, #134424, #170075, #202554, #53133, #5414, #19554, #119262, #85631, #101886, #18487, #36871, #55272, #151718, #185248, #56339, #122500, #3288, #200427, #6494, #71492, #105106, #69356, #137604, #102954, #84564, #135465, #169013, #86700, #20611, #152768, #4349, #54206, #188461, #150653, #70418, #52073, #2215, #72569, #118200, #171145, #136535, #120344, #186320, #39023, #37955, #104028, #21661, #87767, #203621, #40092, #68291, #22737, #88855, #154910, #138668, #204689, #106204, #127834, #23819, #124625, #205771, #89924, #11832, #73648, #44365, #25954, #173305, #108353, #192709, #190583, #107283, #140824, #75785, #174375, #193786, #172231, #123565, #92060, #208959, #24884, #74720, #77909, #45435, #59524, #158117, #125684, #9709, #139747, #57400, #144029, #90989, #191642, #189528, #41176, #110488, #157052, #8640, #206837, #58470, #155975, #42240, #76838, #141892, #160233, #43306, #7562, #109426, #207903, #175431, #27017, #93125, #159164, #210024, #61666, #10763, #142957, #60592, #126750, #176487, #28098, #94193, #177558, #98436, #82168, #13957, #78971, #163443, #65895, #80041, #178628, #62719, #132041, #164500, #165562, #162379, #114746, #81114, #30240, #63794, #146144, #96324, #212159, #129951, #195940, #95259, #47575, #128880, #198051, #32371, #214262, #194861, #113690, #46494, #12892, #48629, #147199, #179692, #16085, #112617, #31309, #97387, #15023, #111549, #213225, #148263, #64856, #131002, #149316, #895, #196994, #145091, #99505, #49680, #115807, #180744, #181794, #33428, #29170, #17157, #83231, #66963, #133102, #199099, #161309, #211095, #166635, #169832, #151463, #38772, #70172, #6242, #136284, #51830, #50745, #34489, #119016, #138418, #104853, #170898, #100564, #103781, #167699, #86453, #35553, #117948, #135227, #116872, #37705, #21419, #19300, #18228, #102706, #5166, #85381, #183943, #1965, #71240, #87528, #22490, #101633, #53955, #20369, #3036, #69105, #201240, #52881, #184997, #36621, #168763, #84312, #152518, #68029, #137356, #186068, #153594, #134167, #4103, #200177, #150397, #202304, #120093, #203371, #55025, #121174, #187143, #88602, #154658, #182873, #72313, #26777, #7311, #156805, #27853, #93950, #73388, #171977, #192469, #191400, #76596, #205521, #43066, #173055, #56092, #189283, #40923, #58220, #107029, #123320, #24635, #174134, #159991, #122248, #8392, #23567, #188207, #44121, #105953, #142708, #124379, #57155, #140581, #10522, #74474, #139493, #90743, #108106, #206592, #11592, #204438, #155727, #190337, #92880, #41999, #25708, #110242, #77666, #91816, #157874, #9467, #75538, #89677, #141649, #176252, #207660, #59279, #125438, #109179, #208718, #175191, #158926, #60344, #126505, #39846, #46255, #64619, #163199, #99262, #194612, #96080, #47328, #111309, #162133, #63554, #31070, #15842, #78724, #29995, #80874, #146964, #62483, #115556, #113443, #196753, #212979, #130758, #48394, #144851, #180503, #45195, #65649, #165310, #210857, #177312, #197802, #129710, #13722, #195693, #114507, #181553, #209781, #193553, #12653, #33181, #148014, #16904, #32121, #95011, #97146, #112373, #128647, #143786, #98204, #61420, #178384, #28926, #164254, #81928, #161060, #214024, #79795, #127584, #131796, #49437, #145908, #211919, #179448, #14782, #66701, #150143, #1715, #21158, #104592, #133921, #103516, #84056, #200978, #152265, #69911, #67770, #170637, #119827, #120909, #203118, #199928, #186881, #183690, #20107, #149060, #102440, #136021, #51573, #169575, #54760, #117699, #34237, #166377, #35296, #153327, #184737, #134970, #151208, #132848 ) ),
 .UNSPECIFIED., .F., .F., .T. ) 
 B_SPLINE_SURFACE_WITH_KNOTS ( ( 2, 2 ),
 ( 3, 2, 2, 2, 2, 2, 2, 2, 2, 2, 2, 2, 2, 2, 2, 2, 2, 2, 2, 2, 2, 2, 2, 2, 2, 2, 2, 2, 2, 2, 2, 2, 2, 2, 2, 2, 2, 2, 2, 2, 2, 2, 2, 2, 2, 2, 2, 2, 2, 2, 2, 2, 2, 2, 2, 2, 2, 2, 2, 2, 2, 2, 2, 2, 2, 2, 2, 2, 2, 2, 2, 2, 2, 2, 2, 2, 2, 2, 2, 2, 2, 2, 2, 2, 2, 2, 2, 2, 2, 2, 2, 2, 2, 2, 2, 2, 2, 2, 2, 2, 2, 2, 2, 2, 2, 2, 2, 2, 2, 2, 2, 2, 2, 2, 2, 2, 2, 2, 2, 2, 2, 2, 2, 2, 2, 2, 2, 2, 2, 2, 2, 2, 2, 2, 2, 2, 2, 2, 2, 2, 2, 2, 2, 2, 2, 2, 2, 2, 2, 2, 2, 2, 2, 2, 2, 2, 2, 2, 2, 2, 2, 2, 2, 2, 2, 2, 2, 2, 2, 2, 2, 2, 2, 2, 2, 2, 2, 2, 2, 2, 2, 2, 2, 2, 2, 2, 2, 2, 2, 2, 2, 2, 2, 2, 2, 2, 2, 2, 2, 2, 2, 2, 2, 2, 2, 2, 2, 2, 2, 2, 2, 2, 2, 2, 2, 2, 2, 2, 2, 2, 2, 2, 2, 2, 2, 2, 2, 2, 2, 2, 2, 2, 2, 2, 2, 2, 2, 2, 2, 2, 3 ),
 ( 0.000000000000000000, 1.000000000000000000 ),
 ( 0.000000000000000000, 0.004166666666666666609, 0.008333333333333333218, 0.01250000000000000069, 0.01666666666666666644, 0.02083333333333333218, 0.02500000000000000139, 0.02916666666666666713, 0.03333333333333333287, 0.03749999999999999861, 0.04166666666666666435, 0.04583333333333333010, 0.05000000000000000278, 0.05416666666666666852, 0.05833333333333333426, 0.06250000000000000000, 0.06666666666666666574, 0.07083333333333333148, 0.07499999999999999722, 0.07916666666666666297, 0.08333333333333332871, 0.08749999999999999445, 0.09166666666666666019, 0.09583333333333333981, 0.1000000000000000056, 0.1041666666666666713, 0.1083333333333333370, 0.1125000000000000028, 0.1166666666666666685, 0.1208333333333333343, 0.1250000000000000000, 0.1291666666666666796, 0.1333333333333333315, 0.1375000000000000111, 0.1416666666666666630, 0.1458333333333333426, 0.1499999999999999944, 0.1541666666666666741, 0.1583333333333333259, 0.1625000000000000056, 0.1666666666666666574, 0.1708333333333333370, 0.1749999999999999889, 0.1791666666666666685, 0.1833333333333333204, 0.1875000000000000000, 0.1916666666666666796, 0.1958333333333333315, 0.2000000000000000111, 0.2041666666666666630, 0.2083333333333333426, 0.2124999999999999944, 0.2166666666666666741, 0.2208333333333333259, 0.2250000000000000056, 0.2291666666666666574, 0.2333333333333333370, 0.2374999999999999889, 0.2416666666666666685, 0.2458333333333333204, 0.2500000000000000000, 0.2541666666666666519, 0.2583333333333333592, 0.2625000000000000111, 0.2666666666666666630, 0.2708333333333333148, 0.2750000000000000222, 0.2791666666666666741, 0.2833333333333333259, 0.2874999999999999778, 0.2916666666666666852, 0.2958333333333333370, 0.2999999999999999889, 0.3041666666666666408, 0.3083333333333333481, 0.3125000000000000000, 0.3166666666666666519, 0.3208333333333333592, 0.3250000000000000111, 0.3291666666666666630, 0.3333333333333333148, 0.3375000000000000222, 0.3416666666666666741, 0.3458333333333333259, 0.3499999999999999778, 0.3541666666666666852, 0.3583333333333333370, 0.3624999999999999889, 0.3666666666666666408, 0.3708333333333333481, 0.3750000000000000000, 0.3791666666666666519, 0.3833333333333333592, 0.3875000000000000111, 0.3916666666666666630, 0.3958333333333333148, 0.4000000000000000222, 0.4041666666666666741, 0.4083333333333333259, 0.4124999999999999778, 0.4166666666666666852, 0.4208333333333333370, 0.4249999999999999889, 0.4291666666666666408, 0.4333333333333333481, 0.4375000000000000000, 0.4416666666666666519, 0.4458333333333333592, 0.4500000000000000111, 0.4541666666666666630, 0.4583333333333333148, 0.4625000000000000222, 0.4666666666666666741, 0.4708333333333333259, 0.4749999999999999778, 0.4791666666666666852, 0.4833333333333333370, 0.4874999999999999889, 0.4916666666666666408, 0.4958333333333333481, 0.5000000000000000000, 0.5041666666666666519, 0.5083333333333333037, 0.5124999999999999556, 0.5166666666666667185, 0.5208333333333333703, 0.5250000000000000222, 0.5291666666666666741, 0.5333333333333333259, 0.5374999999999999778, 0.5416666666666666297, 0.5458333333333332815, 0.5500000000000000444, 0.5541666666666666963, 0.5583333333333333481, 0.5625000000000000000, 0.5666666666666666519, 0.5708333333333333037, 0.5749999999999999556, 0.5791666666666667185, 0.5833333333333333703, 0.5875000000000000222, 0.5916666666666666741, 0.5958333333333333259, 0.5999999999999999778, 0.6041666666666666297, 0.6083333333333332815, 0.6125000000000000444, 0.6166666666666666963, 0.6208333333333333481, 0.6250000000000000000, 0.6291666666666666519, 0.6333333333333333037, 0.6374999999999999556, 0.6416666666666667185, 0.6458333333333333703, 0.6500000000000000222, 0.6541666666666666741, 0.6583333333333333259, 0.6624999999999999778, 0.6666666666666666297, 0.6708333333333332815, 0.6750000000000000444, 0.6791666666666666963, 0.6833333333333333481, 0.6875000000000000000, 0.6916666666666666519, 0.6958333333333333037, 0.6999999999999999556, 0.7041666666666667185, 0.7083333333333333703, 0.7125000000000000222, 0.7166666666666666741, 0.7208333333333333259, 0.7249999999999999778, 0.7291666666666666297, 0.7333333333333332815, 0.7375000000000000444, 0.7416666666666666963, 0.7458333333333333481, 0.7500000000000000000, 0.7541666666666666519, 0.7583333333333333037, 0.7624999999999999556, 0.7666666666666667185, 0.7708333333333333703, 0.7750000000000000222, 0.7791666666666666741, 0.7833333333333333259, 0.7874999999999999778, 0.7916666666666666297, 0.7958333333333332815, 0.8000000000000000444, 0.8041666666666666963, 0.8083333333333333481, 0.8125000000000000000, 0.8166666666666666519, 0.8208333333333333037, 0.8249999999999999556, 0.8291666666666667185, 0.8333333333333333703, 0.8375000000000000222, 0.8416666666666666741, 0.8458333333333333259, 0.8499999999999999778, 0.8541666666666666297, 0.8583333333333332815, 0.8625000000000000444, 0.8666666666666666963, 0.8708333333333333481, 0.8750000000000000000, 0.8791666666666666519, 0.8833333333333333037, 0.8874999999999999556, 0.8916666666666667185, 0.8958333333333333703, 0.9000000000000000222, 0.9041666666666666741, 0.9083333333333333259, 0.9124999999999999778, 0.9166666666666666297, 0.9208333333333332815, 0.9250000000000000444, 0.9291666666666666963, 0.9333333333333333481, 0.9375000000000000000, 0.9416666666666666519, 0.9458333333333333037, 0.9499999999999999556, 0.9541666666666667185, 0.9583333333333333703, 0.9625000000000000222, 0.9666666666666666741, 0.9708333333333333259, 0.9749999999999999778, 0.9791666666666666297, 0.9833333333333332815, 0.9875000000000000444, 0.9916666666666666963, 0.9958333333333333481, 1.000000000000000000 ),
 .UNSPECIFIED. ) 
 GEOMETRIC_REPRESENTATION_ITEM ( )  RATIONAL_B_SPLINE_SURFACE ( (
 ( 1.000000000000000000, 0.8660254037844387076, 1.000000000000000000, 0.8660254037844387076, 1.000000000000000000, 0.8660254037844387076, 1.000000000000000000, 0.8660254037844387076, 1.000000000000000000, 0.8660254037844387076, 1.000000000000000000, 0.8660254037844387076, 1.000000000000000000, 0.8660254037844387076, 1.000000000000000000, 0.8660254037844387076, 1.000000000000000000, 0.8660254037844387076, 1.000000000000000000, 0.8660254037844387076, 1.000000000000000000, 0.8660254037844387076, 1.000000000000000000, 0.8660254037844387076, 1.000000000000000000, 0.8660254037844387076, 1.000000000000000000, 0.8660254037844387076, 1.000000000000000000, 0.8660254037844387076, 1.000000000000000000, 0.8660254037844387076, 1.000000000000000000, 0.8660254037844387076, 1.000000000000000000, 0.8660254037844387076, 1.000000000000000000, 0.8660254037844387076, 1.000000000000000000, 0.8660254037844387076, 1.000000000000000000, 0.8660254037844387076, 1.000000000000000000, 0.8660254037844387076, 1.000000000000000000, 0.8660254037844387076, 1.000000000000000000, 0.8660254037844387076, 1.000000000000000000, 0.8660254037844387076, 1.000000000000000000, 0.8660254037844387076, 1.000000000000000000, 0.8660254037844387076, 1.000000000000000000, 0.8660254037844387076, 1.000000000000000000, 0.8660254037844387076, 1.000000000000000000, 0.8660254037844387076, 1.000000000000000000, 0.8660254037844387076, 1.000000000000000000, 0.8660254037844387076, 1.000000000000000000, 0.8660254037844387076, 1.000000000000000000, 0.8660254037844387076, 1.000000000000000000, 0.8660254037844387076, 1.000000000000000000, 0.8660254037844387076, 1.000000000000000000, 0.8660254037844387076, 1.000000000000000000, 0.8660254037844387076, 1.000000000000000000, 0.8660254037844387076, 1.000000000000000000, 0.8660254037844387076, 1.000000000000000000, 0.8660254037844387076, 1.000000000000000000, 0.8660254037844387076, 1.000000000000000000, 0.8660254037844387076, 1.000000000000000000, 0.8660254037844387076, 1.000000000000000000, 0.8660254037844387076, 1.000000000000000000, 0.8660254037844387076, 1.000000000000000000, 0.8660254037844387076, 1.000000000000000000, 0.8660254037844387076, 1.000000000000000000, 0.8660254037844387076, 1.000000000000000000, 0.8660254037844387076, 1.000000000000000000, 0.8660254037844387076, 1.000000000000000000, 0.8660254037844387076, 1.000000000000000000, 0.8660254037844387076, 1.000000000000000000, 0.8660254037844387076, 1.000000000000000000, 0.8660254037844387076, 1.000000000000000000, 0.8660254037844387076, 1.000000000000000000, 0.8660254037844387076, 1.000000000000000000, 0.8660254037844387076, 1.000000000000000000, 0.8660254037844387076, 1.000000000000000000, 0.8660254037844387076, 1.000000000000000000, 0.8660254037844387076, 1.000000000000000000, 0.8660254037844387076, 1.000000000000000000, 0.8660254037844387076, 1.000000000000000000, 0.8660254037844387076, 1.000000000000000000, 0.8660254037844387076, 1.000000000000000000, 0.8660254037844387076, 1.000000000000000000, 0.8660254037844387076, 1.000000000000000000, 0.8660254037844387076, 1.000000000000000000, 0.8660254037844387076, 1.000000000000000000, 0.8660254037844387076, 1.000000000000000000, 0.8660254037844387076, 1.000000000000000000, 0.8660254037844387076, 1.000000000000000000, 0.8660254037844387076, 1.000000000000000000, 0.8660254037844387076, 1.000000000000000000, 0.8660254037844387076, 1.000000000000000000, 0.8660254037844387076, 1.000000000000000000, 0.8660254037844387076, 1.000000000000000000, 0.8660254037844387076, 1.000000000000000000, 0.8660254037844387076, 1.000000000000000000, 0.8660254037844387076, 1.000000000000000000, 0.8660254037844387076, 1.000000000000000000, 0.8660254037844387076, 1.000000000000000000, 0.8660254037844387076, 1.000000000000000000, 0.8660254037844387076, 1.000000000000000000, 0.8660254037844387076, 1.000000000000000000, 0.8660254037844387076, 1.000000000000000000, 0.8660254037844387076, 1.000000000000000000, 0.8660254037844387076, 1.000000000000000000, 0.8660254037844387076, 1.000000000000000000, 0.8660254037844387076, 1.000000000000000000, 0.8660254037844387076, 1.000000000000000000, 0.8660254037844387076, 1.000000000000000000, 0.8660254037844387076, 1.000000000000000000, 0.8660254037844387076, 1.000000000000000000, 0.8660254037844387076, 1.000000000000000000, 0.8660254037844387076, 1.000000000000000000, 0.8660254037844387076, 1.000000000000000000, 0.8660254037844387076, 1.000000000000000000, 0.8660254037844387076, 1.000000000000000000, 0.8660254037844387076, 1.000000000000000000, 0.8660254037844387076, 1.000000000000000000, 0.8660254037844387076, 1.000000000000000000, 0.8660254037844387076, 1.000000000000000000, 0.8660254037844387076, 1.000000000000000000, 0.8660254037844387076, 1.000000000000000000, 0.8660254037844387076, 1.000000000000000000, 0.8660254037844387076, 1.000000000000000000, 0.8660254037844387076, 1.000000000000000000, 0.8660254037844387076, 1.000000000000000000, 0.8660254037844387076, 1.000000000000000000, 0.8660254037844387076, 1.000000000000000000, 0.8660254037844387076, 1.000000000000000000, 0.8660254037844387076, 1.000000000000000000, 0.8660254037844387076, 1.000000000000000000, 0.8660254037844387076, 1.000000000000000000, 0.8660254037844387076, 1.000000000000000000, 0.8660254037844387076, 1.000000000000000000, 0.8660254037844387076, 1.000000000000000000, 0.8660254037844387076, 1.000000000000000000, 0.8660254037844387076, 1.000000000000000000, 0.8660254037844387076, 1.000000000000000000, 0.8660254037844387076, 1.000000000000000000, 0.8660254037844387076, 1.000000000000000000, 0.8660254037844387076, 1.000000000000000000, 0.8660254037844387076, 1.000000000000000000, 0.8660254037844387076, 1.000000000000000000, 0.8660254037844387076, 1.000000000000000000, 0.8660254037844387076, 1.000000000000000000, 0.8660254037844387076, 1.000000000000000000, 0.8660254037844387076, 1.000000000000000000, 0.8660254037844387076, 1.000000000000000000, 0.8660254037844387076, 1.000000000000000000, 0.8660254037844387076, 1.000000000000000000, 0.8660254037844387076, 1.000000000000000000, 0.8660254037844387076, 1.000000000000000000, 0.8660254037844387076, 1.000000000000000000, 0.8660254037844387076, 1.000000000000000000, 0.8660254037844387076, 1.000000000000000000, 0.8660254037844387076, 1.000000000000000000, 0.8660254037844387076, 1.000000000000000000, 0.8660254037844387076, 1.000000000000000000, 0.8660254037844387076, 1.000000000000000000, 0.8660254037844387076, 1.000000000000000000, 0.8660254037844387076, 1.000000000000000000, 0.8660254037844387076, 1.000000000000000000, 0.8660254037844387076, 1.000000000000000000, 0.8660254037844387076, 1.000000000000000000, 0.8660254037844387076, 1.000000000000000000, 0.8660254037844387076, 1.000000000000000000, 0.8660254037844387076, 1.000000000000000000, 0.8660254037844387076, 1.000000000000000000, 0.8660254037844387076, 1.000000000000000000, 0.8660254037844387076, 1.000000000000000000, 0.8660254037844387076, 1.000000000000000000, 0.8660254037844387076, 1.000000000000000000, 0.8660254037844387076, 1.000000000000000000, 0.8660254037844387076, 1.000000000000000000, 0.8660254037844387076, 1.000000000000000000, 0.8660254037844387076, 1.000000000000000000, 0.8660254037844387076, 1.000000000000000000, 0.8660254037844387076, 1.000000000000000000, 0.8660254037844387076, 1.000000000000000000, 0.8660254037844387076, 1.000000000000000000, 0.8660254037844387076, 1.000000000000000000, 0.8660254037844387076, 1.000000000000000000, 0.8660254037844387076, 1.000000000000000000, 0.8660254037844387076, 1.000000000000000000, 0.8660254037844387076, 1.000000000000000000, 0.8660254037844387076, 1.000000000000000000, 0.8660254037844387076, 1.000000000000000000, 0.8660254037844387076, 1.000000000000000000, 0.8660254037844387076, 1.000000000000000000, 0.8660254037844387076, 1.000000000000000000, 0.8660254037844387076, 1.000000000000000000, 0.8660254037844387076, 1.000000000000000000, 0.8660254037844387076, 1.000000000000000000, 0.8660254037844387076, 1.000000000000000000, 0.8660254037844387076, 1.000000000000000000, 0.8660254037844387076, 1.000000000000000000, 0.8660254037844387076, 1.000000000000000000, 0.8660254037844387076, 1.000000000000000000, 0.8660254037844387076, 1.000000000000000000, 0.8660254037844387076, 1.000000000000000000, 0.8660254037844387076, 1.000000000000000000, 0.8660254037844387076, 1.000000000000000000, 0.8660254037844387076, 1.000000000000000000, 0.8660254037844387076, 1.000000000000000000, 0.8660254037844387076, 1.000000000000000000, 0.8660254037844387076, 1.000000000000000000, 0.8660254037844387076, 1.000000000000000000, 0.8660254037844387076, 1.000000000000000000, 0.8660254037844387076, 1.000000000000000000, 0.8660254037844387076, 1.000000000000000000, 0.8660254037844387076, 1.000000000000000000, 0.8660254037844387076, 1.000000000000000000, 0.8660254037844387076, 1.000000000000000000, 0.8660254037844387076, 1.000000000000000000, 0.8660254037844387076, 1.000000000000000000, 0.8660254037844387076, 1.000000000000000000, 0.8660254037844387076, 1.000000000000000000, 0.8660254037844387076, 1.000000000000000000, 0.8660254037844387076, 1.000000000000000000, 0.8660254037844387076, 1.000000000000000000, 0.8660254037844387076, 1.000000000000000000, 0.8660254037844387076, 1.000000000000000000, 0.8660254037844387076, 1.000000000000000000, 0.8660254037844387076, 1.000000000000000000, 0.8660254037844387076, 1.000000000000000000, 0.8660254037844387076, 1.000000000000000000, 0.8660254037844387076, 1.000000000000000000, 0.8660254037844387076, 1.000000000000000000, 0.8660254037844387076, 1.000000000000000000, 0.8660254037844387076, 1.000000000000000000, 0.8660254037844387076, 1.000000000000000000, 0.8660254037844387076, 1.000000000000000000, 0.8660254037844387076, 1.000000000000000000, 0.8660254037844387076, 1.000000000000000000, 0.8660254037844387076, 1.000000000000000000, 0.8660254037844387076, 1.000000000000000000, 0.8660254037844387076, 1.000000000000000000, 0.8660254037844387076, 1.000000000000000000, 0.8660254037844387076, 1.000000000000000000, 0.8660254037844387076, 1.000000000000000000, 0.8660254037844387076, 1.000000000000000000, 0.8660254037844387076, 1.000000000000000000, 0.8660254037844387076, 1.000000000000000000, 0.8660254037844387076, 1.000000000000000000, 0.8660254037844387076, 1.000000000000000000, 0.8660254037844387076, 1.000000000000000000, 0.8660254037844387076, 1.000000000000000000, 0.8660254037844387076, 1.000000000000000000, 0.8660254037844387076, 1.000000000000000000, 0.8660254037844387076, 1.000000000000000000, 0.8660254037844387076, 1.000000000000000000, 0.8660254037844387076, 1.000000000000000000, 0.8660254037844387076, 1.000000000000000000, 0.8660254037844387076, 1.000000000000000000, 0.8660254037844387076, 1.000000000000000000, 0.8660254037844387076, 1.000000000000000000, 0.8660254037844387076, 1.000000000000000000),
 ( 1.000000000000000000, 0.8660254037844387076, 1.000000000000000000, 0.8660254037844387076, 1.000000000000000000, 0.8660254037844387076, 1.000000000000000000, 0.8660254037844387076, 1.000000000000000000, 0.8660254037844387076, 1.000000000000000000, 0.8660254037844387076, 1.000000000000000000, 0.8660254037844387076, 1.000000000000000000, 0.8660254037844387076, 1.000000000000000000, 0.8660254037844387076, 1.000000000000000000, 0.8660254037844387076, 1.000000000000000000, 0.8660254037844387076, 1.000000000000000000, 0.8660254037844387076, 1.000000000000000000, 0.8660254037844387076, 1.000000000000000000, 0.8660254037844387076, 1.000000000000000000, 0.8660254037844387076, 1.000000000000000000, 0.8660254037844387076, 1.000000000000000000, 0.8660254037844387076, 1.000000000000000000, 0.8660254037844387076, 1.000000000000000000, 0.8660254037844387076, 1.000000000000000000, 0.8660254037844387076, 1.000000000000000000, 0.8660254037844387076, 1.000000000000000000, 0.8660254037844387076, 1.000000000000000000, 0.8660254037844387076, 1.000000000000000000, 0.8660254037844387076, 1.000000000000000000, 0.8660254037844387076, 1.000000000000000000, 0.8660254037844387076, 1.000000000000000000, 0.8660254037844387076, 1.000000000000000000, 0.8660254037844387076, 1.000000000000000000, 0.8660254037844387076, 1.000000000000000000, 0.8660254037844387076, 1.000000000000000000, 0.8660254037844387076, 1.000000000000000000, 0.8660254037844387076, 1.000000000000000000, 0.8660254037844387076, 1.000000000000000000, 0.8660254037844387076, 1.000000000000000000, 0.8660254037844387076, 1.000000000000000000, 0.8660254037844387076, 1.000000000000000000, 0.8660254037844387076, 1.000000000000000000, 0.8660254037844387076, 1.000000000000000000, 0.8660254037844387076, 1.000000000000000000, 0.8660254037844387076, 1.000000000000000000, 0.8660254037844387076, 1.000000000000000000, 0.8660254037844387076, 1.000000000000000000, 0.8660254037844387076, 1.000000000000000000, 0.8660254037844387076, 1.000000000000000000, 0.8660254037844387076, 1.000000000000000000, 0.8660254037844387076, 1.000000000000000000, 0.8660254037844387076, 1.000000000000000000, 0.8660254037844387076, 1.000000000000000000, 0.8660254037844387076, 1.000000000000000000, 0.8660254037844387076, 1.000000000000000000, 0.8660254037844387076, 1.000000000000000000, 0.8660254037844387076, 1.000000000000000000, 0.8660254037844387076, 1.000000000000000000, 0.8660254037844387076, 1.000000000000000000, 0.8660254037844387076, 1.000000000000000000, 0.8660254037844387076, 1.000000000000000000, 0.8660254037844387076, 1.000000000000000000, 0.8660254037844387076, 1.000000000000000000, 0.8660254037844387076, 1.000000000000000000, 0.8660254037844387076, 1.000000000000000000, 0.8660254037844387076, 1.000000000000000000, 0.8660254037844387076, 1.000000000000000000, 0.8660254037844387076, 1.000000000000000000, 0.8660254037844387076, 1.000000000000000000, 0.8660254037844387076, 1.000000000000000000, 0.8660254037844387076, 1.000000000000000000, 0.8660254037844387076, 1.000000000000000000, 0.8660254037844387076, 1.000000000000000000, 0.8660254037844387076, 1.000000000000000000, 0.8660254037844387076, 1.000000000000000000, 0.8660254037844387076, 1.000000000000000000, 0.8660254037844387076, 1.000000000000000000, 0.8660254037844387076, 1.000000000000000000, 0.8660254037844387076, 1.000000000000000000, 0.8660254037844387076, 1.000000000000000000, 0.8660254037844387076, 1.000000000000000000, 0.8660254037844387076, 1.000000000000000000, 0.8660254037844387076, 1.000000000000000000, 0.8660254037844387076, 1.000000000000000000, 0.8660254037844387076, 1.000000000000000000, 0.8660254037844387076, 1.000000000000000000, 0.8660254037844387076, 1.000000000000000000, 0.8660254037844387076, 1.000000000000000000, 0.8660254037844387076, 1.000000000000000000, 0.8660254037844387076, 1.000000000000000000, 0.8660254037844387076, 1.000000000000000000, 0.8660254037844387076, 1.000000000000000000, 0.8660254037844387076, 1.000000000000000000, 0.8660254037844387076, 1.000000000000000000, 0.8660254037844387076, 1.000000000000000000, 0.8660254037844387076, 1.000000000000000000, 0.8660254037844387076, 1.000000000000000000, 0.8660254037844387076, 1.000000000000000000, 0.8660254037844387076, 1.000000000000000000, 0.8660254037844387076, 1.000000000000000000, 0.8660254037844387076, 1.000000000000000000, 0.8660254037844387076, 1.000000000000000000, 0.8660254037844387076, 1.000000000000000000, 0.8660254037844387076, 1.000000000000000000, 0.8660254037844387076, 1.000000000000000000, 0.8660254037844387076, 1.000000000000000000, 0.8660254037844387076, 1.000000000000000000, 0.8660254037844387076, 1.000000000000000000, 0.8660254037844387076, 1.000000000000000000, 0.8660254037844387076, 1.000000000000000000, 0.8660254037844387076, 1.000000000000000000, 0.8660254037844387076, 1.000000000000000000, 0.8660254037844387076, 1.000000000000000000, 0.8660254037844387076, 1.000000000000000000, 0.8660254037844387076, 1.000000000000000000, 0.8660254037844387076, 1.000000000000000000, 0.8660254037844387076, 1.000000000000000000, 0.8660254037844387076, 1.000000000000000000, 0.8660254037844387076, 1.000000000000000000, 0.8660254037844387076, 1.000000000000000000, 0.8660254037844387076, 1.000000000000000000, 0.8660254037844387076, 1.000000000000000000, 0.8660254037844387076, 1.000000000000000000, 0.8660254037844387076, 1.000000000000000000, 0.8660254037844387076, 1.000000000000000000, 0.8660254037844387076, 1.000000000000000000, 0.8660254037844387076, 1.000000000000000000, 0.8660254037844387076, 1.000000000000000000, 0.8660254037844387076, 1.000000000000000000, 0.8660254037844387076, 1.000000000000000000, 0.8660254037844387076, 1.000000000000000000, 0.8660254037844387076, 1.000000000000000000, 0.8660254037844387076, 1.000000000000000000, 0.8660254037844387076, 1.000000000000000000, 0.8660254037844387076, 1.000000000000000000, 0.8660254037844387076, 1.000000000000000000, 0.8660254037844387076, 1.000000000000000000, 0.8660254037844387076, 1.000000000000000000, 0.8660254037844387076, 1.000000000000000000, 0.8660254037844387076, 1.000000000000000000, 0.8660254037844387076, 1.000000000000000000, 0.8660254037844387076, 1.000000000000000000, 0.8660254037844387076, 1.000000000000000000, 0.8660254037844387076, 1.000000000000000000, 0.8660254037844387076, 1.000000000000000000, 0.8660254037844387076, 1.000000000000000000, 0.8660254037844387076, 1.000000000000000000, 0.8660254037844387076, 1.000000000000000000, 0.8660254037844387076, 1.000000000000000000, 0.8660254037844387076, 1.000000000000000000, 0.8660254037844387076, 1.000000000000000000, 0.8660254037844387076, 1.000000000000000000, 0.8660254037844387076, 1.000000000000000000, 0.8660254037844387076, 1.000000000000000000, 0.8660254037844387076, 1.000000000000000000, 0.8660254037844387076, 1.000000000000000000, 0.8660254037844387076, 1.000000000000000000, 0.8660254037844387076, 1.000000000000000000, 0.8660254037844387076, 1.000000000000000000, 0.8660254037844387076, 1.000000000000000000, 0.8660254037844387076, 1.000000000000000000, 0.8660254037844387076, 1.000000000000000000, 0.8660254037844387076, 1.000000000000000000, 0.8660254037844387076, 1.000000000000000000, 0.8660254037844387076, 1.000000000000000000, 0.8660254037844387076, 1.000000000000000000, 0.8660254037844387076, 1.000000000000000000, 0.8660254037844387076, 1.000000000000000000, 0.8660254037844387076, 1.000000000000000000, 0.8660254037844387076, 1.000000000000000000, 0.8660254037844387076, 1.000000000000000000, 0.8660254037844387076, 1.000000000000000000, 0.8660254037844387076, 1.000000000000000000, 0.8660254037844387076, 1.000000000000000000, 0.8660254037844387076, 1.000000000000000000, 0.8660254037844387076, 1.000000000000000000, 0.8660254037844387076, 1.000000000000000000, 0.8660254037844387076, 1.000000000000000000, 0.8660254037844387076, 1.000000000000000000, 0.8660254037844387076, 1.000000000000000000, 0.8660254037844387076, 1.000000000000000000, 0.8660254037844387076, 1.000000000000000000, 0.8660254037844387076, 1.000000000000000000, 0.8660254037844387076, 1.000000000000000000, 0.8660254037844387076, 1.000000000000000000, 0.8660254037844387076, 1.000000000000000000, 0.8660254037844387076, 1.000000000000000000, 0.8660254037844387076, 1.000000000000000000, 0.8660254037844387076, 1.000000000000000000, 0.8660254037844387076, 1.000000000000000000, 0.8660254037844387076, 1.000000000000000000, 0.8660254037844387076, 1.000000000000000000, 0.8660254037844387076, 1.000000000000000000, 0.8660254037844387076, 1.000000000000000000, 0.8660254037844387076, 1.000000000000000000, 0.8660254037844387076, 1.000000000000000000, 0.8660254037844387076, 1.000000000000000000, 0.8660254037844387076, 1.000000000000000000, 0.8660254037844387076, 1.000000000000000000, 0.8660254037844387076, 1.000000000000000000, 0.8660254037844387076, 1.000000000000000000, 0.8660254037844387076, 1.000000000000000000, 0.8660254037844387076, 1.000000000000000000, 0.8660254037844387076, 1.000000000000000000, 0.8660254037844387076, 1.000000000000000000, 0.8660254037844387076, 1.000000000000000000, 0.8660254037844387076, 1.000000000000000000, 0.8660254037844387076, 1.000000000000000000, 0.8660254037844387076, 1.000000000000000000, 0.8660254037844387076, 1.000000000000000000, 0.8660254037844387076, 1.000000000000000000, 0.8660254037844387076, 1.000000000000000000, 0.8660254037844387076, 1.000000000000000000, 0.8660254037844387076, 1.000000000000000000, 0.8660254037844387076, 1.000000000000000000, 0.8660254037844387076, 1.000000000000000000, 0.8660254037844387076, 1.000000000000000000, 0.8660254037844387076, 1.000000000000000000, 0.8660254037844387076, 1.000000000000000000, 0.8660254037844387076, 1.000000000000000000, 0.8660254037844387076, 1.000000000000000000, 0.8660254037844387076, 1.000000000000000000, 0.8660254037844387076, 1.000000000000000000, 0.8660254037844387076, 1.000000000000000000, 0.8660254037844387076, 1.000000000000000000, 0.8660254037844387076, 1.000000000000000000, 0.8660254037844387076, 1.000000000000000000, 0.8660254037844387076, 1.000000000000000000, 0.8660254037844387076, 1.000000000000000000, 0.8660254037844387076, 1.000000000000000000, 0.8660254037844387076, 1.000000000000000000, 0.8660254037844387076, 1.000000000000000000, 0.8660254037844387076, 1.000000000000000000, 0.8660254037844387076, 1.000000000000000000, 0.8660254037844387076, 1.000000000000000000, 0.8660254037844387076, 1.000000000000000000, 0.8660254037844387076, 1.000000000000000000, 0.8660254037844387076, 1.000000000000000000, 0.8660254037844387076, 1.000000000000000000, 0.8660254037844387076, 1.000000000000000000, 0.8660254037844387076, 1.000000000000000000, 0.8660254037844387076, 1.000000000000000000, 0.8660254037844387076, 1.000000000000000000, 0.8660254037844387076, 1.000000000000000000, 0.8660254037844387076, 1.000000000000000000) ) ) 
 REPRESENTATION_ITEM ( '' )  SURFACE ( )  );
#108146 = CARTESIAN_POINT ( 'NONE',  ( -4.793689830883590020, 7.750332681742931662, 1.199719254218452935 ) ) ;
#108148 = EDGE_LOOP ( 'NONE', ( #16991, #141260, #186748 ) ) ;
#108147 = CARTESIAN_POINT ( 'NONE',  ( -0.7500000000000179856, 10.54166666666667140, 1.299038105676658228 ) ) ;
#108149 = CARTESIAN_POINT ( 'NONE',  ( 4.565167970240332274, -1.970479184476851886, -0.9938812724585781577 ) ) ;
#108150 = CARTESIAN_POINT ( 'NONE',  ( 6.837213258907510749, -2.025504081721161143, 1.008097451810068268 ) ) ;
#108151 = CARTESIAN_POINT ( 'NONE',  ( -5.666945020832185875, 7.634521829102760115, 1.443375672974064550 ) ) ;
#108152 = CARTESIAN_POINT ( 'NONE',  ( 0.4570967503451648373, -1.639016809899789040, 0.9851245988263114262 ) ) ;
#108153 = CARTESIAN_POINT ( 'NONE',  ( 0.09298292169932984019, 1.756857073293972116, 0.9896806593640145033 ) ) ;
#108154 = CARTESIAN_POINT ( 'NONE',  ( -6.999862025036992286, -6.532648833121171172, 6.392587740394332307 ) ) ;
#108155 = CARTESIAN_POINT ( 'NONE',  ( 0.07536363704235479744, 6.947016338497881804, -2.739277465201896078 ) ) ;
#108156 = CARTESIAN_POINT ( 'NONE',  ( 5.760397938718036848, 1.910310778393434106, 0.08934430699411573251 ) ) ;
#108157 = CARTESIAN_POINT ( 'NONE',  ( 0.5845639792326964290, -0.2246964894469481722, -1.857040431621145959 ) ) ;
#108158 = CARTESIAN_POINT ( 'NONE',  ( 2.518767860054324625, 0.2516336668320385828, 2.000731427934741902 ) ) ;
#108160 = CARTESIAN_POINT ( 'NONE',  ( 4.477239461409222798, 0.0005595100435150377523, -2.106257355078521964 ) ) ;
#108159 = CARTESIAN_POINT ( 'NONE',  ( -8.503988664269602538, 10.94440607977979063, 1.599625672291269396 ) ) ;
#108161 = EDGE_CURVE ( 'NONE', #153466, #22324, #25652, .T. ) ;
#108162 = CARTESIAN_POINT ( 'NONE',  ( 7.422199028477372451, 10.74665040227725044, -1.199719254218441611 ) ) ;
#108164 = CARTESIAN_POINT ( 'NONE',  ( -7.853197290813634268, 10.18514947741448573, 1.599625672291295375 ) ) ;
#108163 = CARTESIAN_POINT ( 'NONE',  ( -1.500000000000015099, -0.1208333333333093396, -0.8660254037844383745 ) ) ;
#108165 = FACE_OUTER_BOUND ( 'NONE', #30748, .T. ) ;
#108166 = CARTESIAN_POINT ( 'NONE',  ( 4.236585392707596043, 1.239412559483305198, -1.594744479876673005 ) ) ;
#108167 = CARTESIAN_POINT ( 'NONE',  ( -1.364683531250012516, 4.238541667008090208, -0.7879004041258300672 ) ) ;
#108168 = ADVANCED_FACE ( 'NONE', ( #146146 ), #65897, .T. ) ;
#108169 = CARTESIAN_POINT ( 'NONE',  ( 9.747949258545622442, 10.47495501116581984, 0.000000000000000000 ) ) ;
#108170 = CARTESIAN_POINT ( 'NONE',  ( 4.323607124742586016, -2.069909602744592014, 0.6229453038564189971 ) ) ;
#108171 = CARTESIAN_POINT ( 'NONE',  ( 6.176621499477501054, 9.363752961769195693, -1.199719254218452047 ) ) ;
#108172 = CARTESIAN_POINT ( 'NONE',  ( -0.7499999999999972244, 4.858333333333353821, -1.299038105676652011 ) ) ;
#108174 = DIRECTION ( 'NONE',  ( 0.000000000000000000, 0.000000000000000000, 1.000000000000000000 ) ) ;
#108173 = CARTESIAN_POINT ( 'NONE',  ( 4.532168488718122390, 8.509556680138327778, 0.7998128361456271485 ) ) ;
#108175 = CARTESIAN_POINT ( 'NONE',  ( 7.849807752188022292, 11.14156422998596696, -1.082531754730543083 ) ) ;
#108177 = DIRECTION ( 'NONE',  ( 1.276756478318932585E-15, -1.000000000000000000, 1.665334536937738262E-16 ) ) ;
#108176 = CARTESIAN_POINT ( 'NONE',  ( 2.436178610684522461, 1.334241001675811500, 1.712780914784496122 ) ) ;
#108179 = CARTESIAN_POINT ( 'NONE',  ( 0.8898994657863326108, -0.4472179738511591895, -1.785967584704901912 ) ) ;
#108178 = CARTESIAN_POINT ( 'NONE',  ( -6.236387472606158333, 7.338502141871059870, -1.082531754730544860 ) ) ;
#108180 = CARTESIAN_POINT ( 'NONE',  ( -1.364683531250000748, 2.009375000341421913, 1.214306433183764966E-14 ) ) ;
#108181 = CARTESIAN_POINT ( 'NONE',  ( 3.316156725143477146, 1.388770557483296697, -1.695381604771596606 ) ) ;
#108182 = CARTESIAN_POINT ( 'NONE',  ( 6.983263157960383438, 0.5812290088160886325, 2.006563525967783868 ) ) ;
#108183 = CARTESIAN_POINT ( 'NONE',  ( 3.995213114784367026, 1.913063998889670714, -1.207689374757703771 ) ) ;
#108184 = CARTESIAN_POINT ( 'NONE',  ( -6.507023659554960204, 9.678945805201045971, 1.199719254218452047 ) ) ;
#108185 = CARTESIAN_POINT ( 'NONE',  ( 4.505092375653735992, -0.09411930587044713137, 2.014432893821124004 ) ) ;
#108186 = CARTESIAN_POINT ( 'NONE',  ( -1.001543065824772872E-14, 4.384375000341417916, 1.575800808251672791 ) ) ;
#108187 = CARTESIAN_POINT ( 'NONE',  ( 6.467812791377033577, 6.763347601114057639, -0.2696018389747659172 ) ) ;
#108188 = CARTESIAN_POINT ( 'NONE',  ( 1.499999999999993117, 12.85416666666666785, 0.8660254037844409281 ) ) ;
#108189 = CARTESIAN_POINT ( 'NONE',  ( 6.563555762791525972, 6.830105609444471426, -0.7216878364870458196 ) ) ;
#108190 = CARTESIAN_POINT ( 'NONE',  ( 4.147515422935190266, 0.5979684684156804098, -1.665763606213203518 ) ) ;
#108191 = AXIS2_PLACEMENT_3D ( 'NONE', #152239, #153299, #4875 ) ;
#108192 = CARTESIAN_POINT ( 'NONE',  ( 6.448874621594486989, 10.67543749183559143, 0.7998128361456462443 ) ) ;
#108193 = CARTESIAN_POINT ( 'NONE',  ( 0.5168062790325059774, 1.452128344422070283, -1.525477944039640432 ) ) ;
#108194 = AXIS2_PLACEMENT_3D ( 'NONE', #116427, #131607, #98015 ) ;
#108196 = CARTESIAN_POINT ( 'NONE',  ( -1.500000000000001332, 1.400000000000019229, 0.000000000000000000 ) ) ;
#108195 = CARTESIAN_POINT ( 'NONE',  ( -1.364683531250010295, 10.88020833367473372, 0.7879004041258445001 ) ) ;
#108197 = CARTESIAN_POINT ( 'NONE',  ( 1.117558341675929157, 0.3875481960372212931, -1.930861576554385062 ) ) ;
#108198 = CARTESIAN_POINT ( 'NONE',  ( 11.94105721237523277, 19.00000000000000000, 1.187919463087248273 ) ) ;
#108199 = CARTESIAN_POINT ( 'NONE',  ( 5.835564593388588683, 0.5826401998472263699, -1.930423629703325705 ) ) ;
#108200 = ORIENTED_EDGE ( 'NONE', *, *, #207059, .T. ) ;
#108201 = CARTESIAN_POINT ( 'NONE',  ( 7.646435448427411963, 8.023188899361205273, -0.7216878364870257245 ) ) ;
#108202 = CARTESIAN_POINT ( 'NONE',  ( 8.075853055234393452, 12.57357899774884658, 0.7998128361456462443 ) ) ;
#108203 = CARTESIAN_POINT ( 'NONE',  ( 4.399188623838041323, 1.502396186649012311, 1.114296746780506497 ) ) ;
#108204 = CARTESIAN_POINT ( 'NONE',  ( 4.539282502477016479, 4.190251095844947926, 0.7998128361456341429 ) ) ;
#108205 = ORIENTED_EDGE ( 'NONE', *, *, #91910, .F. ) ;
#108206 = CARTESIAN_POINT ( 'NONE',  ( 4.329010850845236291, -1.929826300244817272, -0.7499136367685383942 ) ) ;
#108207 = CARTESIAN_POINT ( 'NONE',  ( -4.757329562667670667E-14, 2.062499999999985789, 1.414508159514559438 ) ) ;
#108208 = CARTESIAN_POINT ( 'NONE',  ( -6.170369307550858551, 8.292126506933035657, 1.443375672974058777 ) ) ;
#108209 = DIRECTION ( 'NONE',  ( 1.000000000000000000, 0.000000000000000000, 0.000000000000000000 ) ) ;
#108210 = CARTESIAN_POINT ( 'NONE',  ( 8.106885785967500979, 11.54545161934907682, 1.199719254218460707 ) ) ;
#108211 = CARTESIAN_POINT ( 'NONE',  ( -8.696665468161981494, 12.23352791524263239, -1.199719254218446718 ) ) ;
#108212 = CARTESIAN_POINT ( 'NONE',  ( 7.126746022638799971, 8.343567110280638133, 1.199719254218452047 ) ) ;
#108213 = CARTESIAN_POINT ( 'NONE',  ( -4.044020806407789159, 7.347651935747151697, -0.7679206946173640080 ) ) ;
#108214 = CARTESIAN_POINT ( 'NONE',  ( -1.364683531249997417, 5.571875000341417916, 1.214306433183764966E-14 ) ) ;
#108215 = CARTESIAN_POINT ( 'NONE',  ( 4.176187491914356897, -1.006606191838583131, -1.683785057063936552 ) ) ;
#108216 = CARTESIAN_POINT ( 'NONE',  ( 2.108749758911751204, 0.7741990562295970602, -1.861730988020185329 ) ) ;
#108217 = CARTESIAN_POINT ( 'NONE',  ( -3.298376509874564988, 7.070132704820777825, 0.000000000000000000 ) ) ;
#108218 = CARTESIAN_POINT ( 'NONE',  ( 6.639320575229278099, 1.279659970127836388, 2.012538313910294807 ) ) ;
#108219 = CARTESIAN_POINT ( 'NONE',  ( 1.510794437334112672, 1.647127454408814362, 0.8865631655482277829 ) ) ;
#108220 = CARTESIAN_POINT ( 'NONE',  ( -0.6823417656249969321, 4.217708333674755394, -1.181850606188749264 ) ) ;
#108221 = CARTESIAN_POINT ( 'NONE',  ( 2.478773383088346716, -1.385198452255667290, 1.461135165768602029 ) ) ;
#108223 = CARTESIAN_POINT ( 'NONE',  ( 3.023186137256496764, -1.865899319694108272, 1.000581237753160879 ) ) ;
#108222 = CARTESIAN_POINT ( 'NONE',  ( -6.724481002698138532, 6.947575379343695623, -0.7216878364870278340 ) ) ;
#108224 = DIRECTION ( 'NONE',  ( 0.000000000000000000, 0.000000000000000000, 1.000000000000000000 ) ) ;
#108225 = CARTESIAN_POINT ( 'NONE',  ( 4.404779037558821386, 0.5491149005726041477, 1.996164414091922135 ) ) ;
#108226 = CARTESIAN_POINT ( 'NONE',  ( 5.820193082016415609, 10.01225203898631655, 0.000000000000000000 ) ) ;
#108228 = CARTESIAN_POINT ( 'NONE',  ( 11.78331023100045627, 13.79999999999998295, 1.799999999999999600 ) ) ;
#108227 = CARTESIAN_POINT ( 'NONE',  ( 0.3278234441896179518, 1.071198113070050972, -1.795324408978350439 ) ) ;
#108230 = ORIENTED_EDGE ( 'NONE', *, *, #14440, .T. ) ;
#108229 = CARTESIAN_POINT ( 'NONE',  ( 5.596661130663158623, -0.4455768995972574364, -1.770251349769519367 ) ) ;
#108231 = CARTESIAN_POINT ( 'NONE',  ( 8.751951852821344247, 10.16936423550178503, -1.199719254218446718 ) ) ;
#108232 = DIRECTION ( 'NONE',  ( 0.5265943820948186804, 0.4485553919811647305, 0.7221470882519708256 ) ) ;
#108234 = AXIS2_PLACEMENT_3D ( 'NONE', #65786, #83129, #30133 ) ;
#108233 = CARTESIAN_POINT ( 'NONE',  ( 2.852660156828608073, 6.479853949608683550, -0.1948928627674442193 ) ) ;
#108235 = CARTESIAN_POINT ( 'NONE',  ( -11.29165584589917870, 5.103824637450834700, 5.764786465619509137 ) ) ;
#108236 = CARTESIAN_POINT ( 'NONE',  ( -1.402160292154681736E-14, 12.23437500034140513, 1.575800808251682339 ) ) ;
#108237 = CARTESIAN_POINT ( 'NONE',  ( 6.551426578739074635, -1.705833205818767295, 0.8644478841580638395 ) ) ;
#108238 = CARTESIAN_POINT ( 'NONE',  ( -7.296259222448620463, 11.66405285949874759, 0.7998128361456481317 ) ) ;
#108239 = CARTESIAN_POINT ( 'NONE',  ( 4.957477724091233995, 8.935474444748447098, -0.7998128361456281477 ) ) ;
#108240 = CARTESIAN_POINT ( 'NONE',  ( -2.954552044183079750E-14, 2.734375000341431772, 1.570758158831788265 ) ) ;
#108241 = CARTESIAN_POINT ( 'NONE',  ( 2.806174607904299734, 5.257325561654889512, -1.082531754730543083 ) ) ;
#108242 = CARTESIAN_POINT ( 'NONE',  ( 6.933263157960373846, 7.629137130509066722, 2.546189081643289942 ) ) ;
#108243 = CARTESIAN_POINT ( 'NONE',  ( 5.034155109375821446, 4.767602470560229122, -0.7998128361456221525 ) ) ;
#108244 = ORIENTED_EDGE ( 'NONE', *, *, #67112, .F. ) ;
#108245 = CARTESIAN_POINT ( 'NONE',  ( -5.912237504011027767, 9.055304967058290799, 1.199719254218454489 ) ) ;
#108246 = CARTESIAN_POINT ( 'NONE',  ( 5.360953910674266965, -0.05231296482399727665, -2.015913715532565043 ) ) ;
#108247 = CARTESIAN_POINT ( 'NONE',  ( 0.1363799957456746648, -9.242177669965688125, -9.620888806888808986 ) ) ;
#108248 =( LENGTH_UNIT ( ) NAMED_UNIT ( * ) SI_UNIT ( .MILLI., .METRE. ) );
#108249 = STYLED_ITEM ( 'NONE', ( #122364 ), #79941 ) ;
#108250 = MECHANICAL_DESIGN_GEOMETRIC_PRESENTATION_REPRESENTATION (  '', ( #104800 ), #836 ) ;
#108251 = CARTESIAN_POINT ( 'NONE',  ( -6.466610638350029916, 6.780223854948245865, 0.3187201834274414058 ) ) ;
#108252 = CARTESIAN_POINT ( 'NONE',  ( -5.910991785878175975, 6.958873840688411860, -1.082531754730544860 ) ) ;
#108253 = CARTESIAN_POINT ( 'NONE',  ( 2.510230996824538430, 6.080353262937265413, 0.000000000000000000 ) ) ;
#108254 = CARTESIAN_POINT ( 'NONE',  ( 1.903111606826495938, -1.666530434877494304, 1.049136497343281738 ) ) ;
#108255 = CARTESIAN_POINT ( 'NONE',  ( 3.954703970953522774, -1.882481274494081980, -0.7231244775810635739 ) ) ;
#108256 = CARTESIAN_POINT ( 'NONE',  ( -6.347188469492005325, 10.55680364771601809, -0.7998128361456291469 ) ) ;
#108257 = CARTESIAN_POINT ( 'NONE',  ( 6.827182134110196365, 7.629137130509086262, 2.889055895399252005 ) ) ;
#108258 = CARTESIAN_POINT ( 'NONE',  ( 3.943468035136340255, 0.7389761752502190806, -2.063229655756371628 ) ) ;
#108259 = CARTESIAN_POINT ( 'NONE',  ( -2.749999999999996447, 8.900000000000027001, 1.273770014145090163E-14 ) ) ;
#108260 = CARTESIAN_POINT ( 'NONE',  ( 2.467692127658027701, 1.889608252265186694, -0.3738381972786026797 ) ) ;
#108261 = CARTESIAN_POINT ( 'NONE',  ( -6.997979842947967377, 11.31606025008131233, -0.7998128361456291469 ) ) ;
#108262 = CARTESIAN_POINT ( 'NONE',  ( 0.1329588055935396196, 2.886534925058126699, -2.334852352984605695 ) ) ;
#108263 = CARTESIAN_POINT ( 'NONE',  ( -10.44369633504468631, 5.112959841837461994, -5.232137017608345708 ) ) ;
#108264 = CARTESIAN_POINT ( 'NONE',  ( 6.988338112840064120, 10.24047933403371502, 1.199719254218460707 ) ) ;
#108265 = VECTOR ( 'NONE', #44609, 1000.000000000000000 ) ;
#108266 = CARTESIAN_POINT ( 'NONE',  ( 3.662674053986138656, 7.424870162959149589, 0.7998128361456321445 ) ) ;
#108267 = CARTESIAN_POINT ( 'NONE',  ( -7.037870247915954280, -8.233137084989836652, 6.381095703207990688 ) ) ;
#108268 = CARTESIAN_POINT ( 'NONE',  ( 6.211043768836181478, 7.379210830797944709, 1.082531754730549967 ) ) ;
#108269 = VERTEX_POINT ( 'NONE', #153318 ) ;
#108271 = CARTESIAN_POINT ( 'NONE',  ( 3.158842756365538129, 0.4911626674463653863, 1.952128870646198555 ) ) ;
#108270 = CARTESIAN_POINT ( 'NONE',  ( 5.583513413114173041, -0.8223277247318347971, 1.647484189299788682 ) ) ;
#108272 = CARTESIAN_POINT ( 'NONE',  ( 4.130415602100383943, 0.2865403768554532493, -2.280420282979139124 ) ) ;
#108274 = CARTESIAN_POINT ( 'NONE',  ( 3.678407310798579299, 1.183884816018574426, -1.435758196845798418 ) ) ;
#108273 = CARTESIAN_POINT ( 'NONE',  ( -0.1290005225502675879, -0.006633637972621592160, -2.173875058097324064 ) ) ;
#108275 = CARTESIAN_POINT ( 'NONE',  ( 3.285556943750000070, -0.6343749995220415716, 0.000000000000000000 ) ) ;
#108276 = LINE ( 'NONE', #93045, #32939 ) ;
#108277 = DIRECTION ( 'NONE',  ( 0.7797859179643623628, 0.6260462619842697141, 0.000000000000000000 ) ) ;
#108278 = CARTESIAN_POINT ( 'NONE',  ( -8.206763054973658100, 8.468978407091068306, 0.7998128361456602331 ) ) ;
#108279 = CARTESIAN_POINT ( 'NONE',  ( -5.180624094197616714, 5.216685329418210948, 0.7216878364870257245 ) ) ;
#108280 = CARTESIAN_POINT ( 'NONE',  ( 5.653879428721274358, 0.8482012749469816093, 1.911158475179574046 ) ) ;
#108281 = CARTESIAN_POINT ( 'NONE',  ( 5.816084710582486217, 9.729256562414162701, 1.040834085586084257E-14 ) ) ;
#108282 = VERTEX_POINT ( 'NONE', #31311 ) ;
#108284 = EDGE_CURVE ( 'NONE', #75994, #211791, #22225, .T. ) ;
#108283 = CIRCLE ( 'NONE', #21748, 0.08000000000000020983 ) ;
#108285 = CARTESIAN_POINT ( 'NONE',  ( -1.403499169904654842, 7.376709478544411169, 4.304123474982140429 ) ) ;
#108286 = DIRECTION ( 'NONE',  ( -0.009157509157509154465, 0.000000000000000000, -0.9999580691339163829 ) ) ;
#108287 = CARTESIAN_POINT ( 'NONE',  ( 6.111878173048258311, -1.710926958338830017, 0.2183984861162356628 ) ) ;
#108288 = CARTESIAN_POINT ( 'NONE',  ( -4.900382456335551140, 7.804531068111707270, 1.199719254218464037 ) ) ;
#108289 = CARTESIAN_POINT ( 'NONE',  ( 1.054805789555151696, -1.101345310128332367, 1.339526040370845772 ) ) ;
#108290 = DIRECTION ( 'NONE',  ( -0.1674078377058430267, 0.000000000000000000, 0.9858877298529756805 ) ) ;
#108291 = SURFACE_STYLE_FILL_AREA ( #24821 ) ;
#108292 = CARTESIAN_POINT ( 'NONE',  ( 6.086835205273840366, 2.090220906010348045, 0.5866831100012849243 ) ) ;
#108293 = CARTESIAN_POINT ( 'NONE',  ( 4.266095019097836172, 0.8626762044917112293, 1.609013669381313294 ) ) ;
#108294 = CARTESIAN_POINT ( 'NONE',  ( 2.676550354755039773, 1.285117694784821518, -1.482265789204496143 ) ) ;
#108295 = EDGE_CURVE ( 'NONE', #7144, #143545, #114748, .T. ) ;
#108296 = DIRECTION ( 'NONE',  ( 0.000000000000000000, -1.000000000000000000, 0.000000000000000000 ) ) ;
#108297 = CARTESIAN_POINT ( 'NONE',  ( 8.209625708274705502, 9.536650400197368427, 1.199719254218462483 ) ) ;
#108298 = CARTESIAN_POINT ( 'NONE',  ( 3.387459763963754700, 0.05019612904376415108, -2.120051327867578550 ) ) ;
#108299 = CARTESIAN_POINT ( 'NONE',  ( -3.307826292054316664, 4.882216645528547616, -1.443375672974059665 ) ) ;
#108300 = EDGE_CURVE ( 'NONE', #91407, #122503, #163445, .T. ) ;
#108301 = DIRECTION ( 'NONE',  ( 0.000000000000000000, 1.000000000000000000, 0.000000000000000000 ) ) ;
#108302 = CARTESIAN_POINT ( 'NONE',  ( -4.699291399009611681, 6.864061528938182555, -1.228208583504811990 ) ) ;
#108303 = CARTESIAN_POINT ( 'NONE',  ( 0.7607008448355723207, -0.6940761377024067258, -1.950597895851911456 ) ) ;
#108305 = CARTESIAN_POINT ( 'NONE',  ( -1.402160292154681736E-14, -0.8656249996585829720, 1.575800808251672791 ) ) ;
#108304 = CARTESIAN_POINT ( 'NONE',  ( -10.41646471606764024, 3.952576377580180989, 5.868867284226453762 ) ) ;
#108307 = ORIENTED_EDGE ( 'NONE', *, *, #72346, .F. ) ;
#108306 = CARTESIAN_POINT ( 'NONE',  ( 3.668779877082572138, 0.8004024921177651519, 2.072244876181651652 ) ) ;
#108308 = CARTESIAN_POINT ( 'NONE',  ( 1.846706770127172881, 0.3881029198684777803, -2.265567138619323018 ) ) ;
#108310 = CARTESIAN_POINT ( 'NONE',  ( 6.684441936803141360, 1.192331456891123187, -1.682829884528406428 ) ) ;
#108309 = CARTESIAN_POINT ( 'NONE',  ( 9.897088948295946764, 10.64895131587453569, 0.7216878364870438212 ) ) ;
#108312 = CARTESIAN_POINT ( 'NONE',  ( 1.642778471875001811, -3.492708332855375630, 2.845375778867859751 ) ) ;
#108311 = CARTESIAN_POINT ( 'NONE',  ( 3.379725431556547477, 7.165039780116438273, -1.734723475976807094E-15 ) ) ;
#108313 =( NAMED_UNIT ( * ) SI_UNIT ( $, .STERADIAN. ) SOLID_ANGLE_UNIT ( ) );
#108314 = DIRECTION ( 'NONE',  ( -0.000000000000000000, -8.546850786086437571E-32, -1.000000000000000000 ) ) ;
#108315 = CARTESIAN_POINT ( 'NONE',  ( -1.850000000000000089, -0.1967728318288185785, 0.5999999999999968692 ) ) ;
#108316 = CARTESIAN_POINT ( 'NONE',  ( -0.2102771530458458771, 0.2260464284578807270, -2.237246294970319127 ) ) ;
#108317 = CARTESIAN_POINT ( 'NONE',  ( 3.047548298876975537, 0.6224300751757807504, -1.608722921838340092 ) ) ;
#108318 = CARTESIAN_POINT ( 'NONE',  ( 2.219935720625454412, 0.9462983093676997637, -1.780669029686342331 ) ) ;
#108319 =( BOUNDED_SURFACE ( )  B_SPLINE_SURFACE ( 3, 3, ( 
 ( #108273, #174294, #10681, #192630, #126665, #61579, #211008, #160152, #79953, #161220 ),
 ( #110403, #60505, #206756, #44282, #76752, #207818, #75701, #78880, #93042, #42158 ),
 ( #176407, #94111, #58387, #62631, #208875, #95171, #109344, #124543, #12807, #128791 ),
 ( #9624, #145003, #194772, #175354, #26934, #29087, #96237, #142873, #159084, #91979 ),
 ( #162287, #25869, #46409, #28013, #112525, #11749, #190500, #158037, #77824, #141815 ),
 ( #178538, #143945, #209941, #127747, #193704, #30148, #45348, #59446, #125603, #191563 ),
 ( #43227, #111467, #177473, #13875, #48544, #47489, #147114, #148174, #19209, #196904 ) ),
 .UNSPECIFIED., .T., .F., .T. ) 
 B_SPLINE_SURFACE_WITH_KNOTS ( ( 4, 3, 4 ),
 ( 4, 1, 1, 1, 1, 1, 1, 4 ),
 ( 0.000000000000000000, 0.5000000000000000000, 1.000000000000000000 ),
 ( 0.000000000000000000, 0.09123828766142533242, 0.1830323254715014447, 0.2554767746403809325, 0.3605042187413262100, 0.5206858269973231312, 0.7335850107976985557, 1.000000000000000000 ),
 .UNSPECIFIED. ) 
 GEOMETRIC_REPRESENTATION_ITEM ( )  RATIONAL_B_SPLINE_SURFACE ( (
 ( 1.000000000000000000, 1.000000000000000000, 1.000000000000000000, 0.9999999999999997780, 1.000000000000000000, 1.000000000000000000, 1.000000000000000222, 1.000000000000000000, 1.000000000000000000, 1.000000000000000000),
 ( 0.3333333333333333703, 0.3333333333333333703, 0.3333333333333334259, 0.3333333333333332593, 0.3333333333333333703, 0.3333333333333333703, 0.3333333333333334814, 0.3333333333333333703, 0.3333333333333333703, 0.3333333333333333703),
 ( 0.3333333333333333703, 0.3333333333333333703, 0.3333333333333334259, 0.3333333333333332593, 0.3333333333333333703, 0.3333333333333333703, 0.3333333333333334814, 0.3333333333333333703, 0.3333333333333333703, 0.3333333333333333703),
 ( 1.000000000000000000, 1.000000000000000000, 1.000000000000000000, 0.9999999999999997780, 1.000000000000000000, 1.000000000000000000, 1.000000000000000222, 1.000000000000000000, 1.000000000000000000, 1.000000000000000000),
 ( 0.3333333333333333703, 0.3333333333333333703, 0.3333333333333334259, 0.3333333333333332593, 0.3333333333333333703, 0.3333333333333333703, 0.3333333333333334814, 0.3333333333333333703, 0.3333333333333333703, 0.3333333333333333703),
 ( 0.3333333333333333703, 0.3333333333333333703, 0.3333333333333334259, 0.3333333333333332593, 0.3333333333333333703, 0.3333333333333333703, 0.3333333333333334814, 0.3333333333333333703, 0.3333333333333333703, 0.3333333333333333703),
 ( 1.000000000000000000, 1.000000000000000000, 1.000000000000000000, 0.9999999999999997780, 1.000000000000000000, 1.000000000000000000, 1.000000000000000222, 1.000000000000000000, 1.000000000000000000, 1.000000000000000000) ) ) 
 REPRESENTATION_ITEM ( '' )  SURFACE ( )  );
#108320 = CARTESIAN_POINT ( 'NONE',  ( 2.497091698460200071, -2.273154071007321697, 0.3411551791231131059 ) ) ;
#108321 = CARTESIAN_POINT ( 'NONE',  ( 3.743696771605113494, -1.710248914368957873, -1.481124664604586583 ) ) ;
#108322 = CARTESIAN_POINT ( 'NONE',  ( 4.934254457356054502, 1.083321712992061814, -1.805932085151832789 ) ) ;
#108323 = CARTESIAN_POINT ( 'NONE',  ( -6.509323148336870091, 7.727203440215372865, 1.082531754730549078 ) ) ;
#108324 = CARTESIAN_POINT ( 'NONE',  ( 3.883871017828253613, -0.8741022562178245581, 1.538735937109585672 ) ) ;
#108326 = CARTESIAN_POINT ( 'NONE',  ( 5.882448709439383805, -0.3326909364035086081, -2.268010969791500742 ) ) ;
#108325 = CARTESIAN_POINT ( 'NONE',  ( 3.729901657090948230, 6.405283462364505631, 1.082531754730549078 ) ) ;
#108327 = CARTESIAN_POINT ( 'NONE',  ( 5.208873985248447802, -0.2666229848188906848, 1.821608446441948193 ) ) ;
#108328 = CARTESIAN_POINT ( 'NONE',  ( -4.623494077460110319, 5.352830164246910272, 1.199719254218462483 ) ) ;
#108329 = CARTESIAN_POINT ( 'NONE',  ( 5.626270559546821204, 6.626699076635176766, 1.082531754730560403 ) ) ;
#108330 = CARTESIAN_POINT ( 'NONE',  ( 1.499999999999990896, 4.025000000000021672, 1.214306433183764966E-14 ) ) ;
#108331 = CARTESIAN_POINT ( 'NONE',  ( 5.015667846030231303, -1.170523448010954315, -1.852474865436819274 ) ) ;
#108332 = CARTESIAN_POINT ( 'NONE',  ( -3.002240950422295995, 5.590032644546251817, -1.199719254218452935 ) ) ;
#108333 = CARTESIAN_POINT ( 'NONE',  ( -1.748134023616016330, 15.47021538507039828, 11.90627320348867357 ) ) ;
#108334 = CARTESIAN_POINT ( 'NONE',  ( 5.863751307568212390, -0.5067217619753560109, 2.007263066363853987 ) ) ;
#108335 = CARTESIAN_POINT ( 'NONE',  ( 4.318600669050608687, 4.999583595936801572, -2.419999999999996820 ) ) ;
#108336 = CIRCLE ( 'NONE', #11318, 0.8299999999999999600 ) ;
#108337 = CARTESIAN_POINT ( 'NONE',  ( -1.364683531250010295, 4.530208333674754506, 0.7879004041258379498 ) ) ;
#108338 = CARTESIAN_POINT ( 'NONE',  ( 3.598194957300792307, -1.924334687528261201, -0.09379112422614949152 ) ) ;
#108339 = CARTESIAN_POINT ( 'NONE',  ( -1.364683531250010295, 9.880208333674728394, 0.7879004041258445001 ) ) ;
#108340 = CARTESIAN_POINT ( 'NONE',  ( -2.928197990871687306, 5.399686175116803710, 1.082531754730560403 ) ) ;
#108341 = CARTESIAN_POINT ( 'NONE',  ( 0.03578803411239706023, -0.1004787818888741302, 2.219253419324648036 ) ) ;
#108342 = ORIENTED_EDGE ( 'NONE', *, *, #141897, .F. ) ;
#108344 = CIRCLE ( 'NONE', #59880, 0.07999999999999940492 ) ;
#108343 = CARTESIAN_POINT ( 'NONE',  ( -5.004368097219957789, 5.011053332944274352, 0.000000000000000000 ) ) ;
#108345 = CARTESIAN_POINT ( 'NONE',  ( 4.192495815123822744, 5.914331089109666983, -1.599625672291255185 ) ) ;
#108346 = CYLINDRICAL_SURFACE ( 'NONE', #45681, 1.500000000000005107 ) ;
#108347 = LINE ( 'NONE', #24877, #92544 ) ;
#108348 = CARTESIAN_POINT ( 'NONE',  ( 0.8362905744919849615, -1.092891352686057527, 1.629061181365853539 ) ) ;
#108349 = CARTESIAN_POINT ( 'NONE',  ( -1.402160292154681736E-14, 1.509375000341420359, -1.575800808251659024 ) ) ;
#108350 = CARTESIAN_POINT ( 'NONE',  ( 3.834746474454188013E-15, 8.843750000682797818, 1.500000000000001554 ) ) ;
#108351 = CARTESIAN_POINT ( 'NONE',  ( 6.127397123722368555, 0.1457569626216181913, -1.956525209266091192 ) ) ;
#108352 = CARTESIAN_POINT ( 'NONE',  ( -9.345647958521597687, 9.797677461230342999, 0.7998128361456462443 ) ) ;
#108353 = CARTESIAN_POINT ( 'NONE',  ( -5.544921637864838715, 6.531792001339513654, -1.082531754730543971 ) ) ;
#108354 = CARTESIAN_POINT ( 'NONE',  ( 0.08136044664198981147, -0.1580758092474404408, -2.227059435111256924 ) ) ;
#108356 = ORIENTED_EDGE ( 'NONE', *, *, #66919, .T. ) ;
#108355 = DIRECTION ( 'NONE',  ( -1.000000000000000000, 7.771561172376097755E-16, 4.440892098500627148E-16 ) ) ;
#108357 = CARTESIAN_POINT ( 'NONE',  ( -1.500000000000001332, -1.318749999317178734, 0.000000000000000000 ) ) ;
#108358 = CARTESIAN_POINT ( 'NONE',  ( 0.4209003391736841349, -0.09842406703440903515, 1.868101828653282226 ) ) ;
#108359 = CARTESIAN_POINT ( 'NONE',  ( 5.659468189498653601, -0.4240490459222304165, -1.681042783800198448 ) ) ;
#108361 = CARTESIAN_POINT ( 'NONE',  ( 3.316156725143477146, 1.388770557483296697, -1.695381604771596606 ) ) ;
#108360 = CARTESIAN_POINT ( 'NONE',  ( -1.360316468750021768, 0.6406250003414132310, -3.469446951953614189E-14 ) ) ;
#108362 = CARTESIAN_POINT ( 'NONE',  ( 4.243447643126375013, -2.009724547103900250, 1.133870999951855696 ) ) ;
#108363 = CARTESIAN_POINT ( 'NONE',  ( 0.3915709625425906615, 1.526647161510179318, 1.384594130533061129 ) ) ;
#108364 = CARTESIAN_POINT ( 'NONE',  ( 2.747912338643729413, 0.6545661140590716132, 1.828431812057261352 ) ) ;
#108365 = CARTESIAN_POINT ( 'NONE',  ( -5.138177029454855216, 7.017625839162543677, 1.443375672974064550 ) ) ;
#108366 = SURFACE_STYLE_FILL_AREA ( #88868 ) ;
#108367 = EDGE_CURVE ( 'NONE', #118849, #52465, #53337, .T. ) ;
#108368 = CARTESIAN_POINT ( 'NONE',  ( 4.728832233812888752, 1.460412846248357210, -1.537820402542383169 ) ) ;
#108369 = PRESENTATION_STYLE_ASSIGNMENT (( #206853 ) ) ;
#108370 = CARTESIAN_POINT ( 'NONE',  ( 3.164685561777963230, 1.281361203394768111, 1.556908733426412450 ) ) ;
#108371 = CARTESIAN_POINT ( 'NONE',  ( -5.544921637864841379, 5.571422787038166291, -0.7216878364870197293 ) ) ;
#108372 = CARTESIAN_POINT ( 'NONE',  ( -7.553827861469316396, 8.841829255582865699, -1.199719254218452047 ) ) ;
#108373 = CARTESIAN_POINT ( 'NONE',  ( 8.387690588348714726, 12.93738945304888333, 1.040834085586084257E-14 ) ) ;
#108374 = CARTESIAN_POINT ( 'NONE',  ( 1.207329354700342305, -0.4456725867950651621, 1.770335049871730071 ) ) ;
#108375 = CARTESIAN_POINT ( 'NONE',  ( -7.096767062110449942, 7.244259425409119046, -0.7998128361456362523 ) ) ;
#108376 = CARTESIAN_POINT ( 'NONE',  ( -5.926849427829407269, 6.943687749669614995, -1.199719254218453823 ) ) ;
#108377 = CARTESIAN_POINT ( 'NONE',  ( -10.87092197480563271, 4.494752981060541330, 4.557748927716649412 ) ) ;
#108378 = ORIENTED_EDGE ( 'NONE', *, *, #954, .F. ) ;
#108379 = CARTESIAN_POINT ( 'NONE',  ( 5.278222320829740077, -1.146742738506721704, 1.712165125756033968 ) ) ;
#108380 = CARTESIAN_POINT ( 'NONE',  ( -7.580417283372126391, 8.016444050121833698, 0.7216878364870317197 ) ) ;
#108381 = CARTESIAN_POINT ( 'NONE',  ( -3.903858165731105778, 6.641919395739846799, 1.199719254218464037 ) ) ;
#108382 = CARTESIAN_POINT ( 'NONE',  ( -5.348676671532174076, 6.524419919965190218, 1.372383455774844219 ) ) ;
#108383 = CARTESIAN_POINT ( 'NONE',  ( 4.565106334443884251, -1.620744288901782904, 1.204869856736161537 ) ) ;
#108385 = ORIENTED_EDGE ( 'NONE', *, *, #47358, .T. ) ;
#108384 = CARTESIAN_POINT ( 'NONE',  ( 5.321006124507968060, 1.683121437214535554, -1.449644825538060733 ) ) ;
#108387 = CARTESIAN_POINT ( 'NONE',  ( 9.625925876022625616, 11.29296361252366765, -1.082531754730537088 ) ) ;
#108386 = CARTESIAN_POINT ( 'NONE',  ( -6.050681693448748177, 10.28115541899069463, 0.7998128361456291469 ) ) ;
#108388 = CIRCLE ( 'NONE', #42637, 10.99999999999999112 ) ;
#108389 = CARTESIAN_POINT ( 'NONE',  ( 5.361359679200154105, 8.342337828120466980, 1.199719254218462483 ) ) ;
#108390 = CARTESIAN_POINT ( 'NONE',  ( 4.469639075930389893, 1.999461767218065678, -0.4989166988303375683 ) ) ;
#108391 = CARTESIAN_POINT ( 'NONE',  ( 4.026017654026761150, -1.753031021560845559, 0.9963007555989014108 ) ) ;
#108392 = ORIENTED_EDGE ( 'NONE', *, *, #69865, .F. ) ;
#108393 = ADVANCED_FACE ( 'NONE', ( #70971 ), #128734, .T. ) ;
#108394 = CARTESIAN_POINT ( 'NONE',  ( 4.650610384687404952, 5.384465856012134566, 1.199719254218462483 ) ) ;
#108396 = ORIENTED_EDGE ( 'NONE', *, *, #198949, .F. ) ;
#108395 = CARTESIAN_POINT ( 'NONE',  ( -1.673491136019439323E-15, 4.000007913748541810, -11.67999999982603399 ) ) ;
#108397 = CARTESIAN_POINT ( 'NONE',  ( 4.913571454530422322, 8.125067815752732514, -1.031885869761673069 ) ) ;
#108398 = CARTESIAN_POINT ( 'NONE',  ( 2.970077202574809228, 1.701686883299750264, 1.080900613174784475 ) ) ;
#108399 = CARTESIAN_POINT ( 'NONE',  ( 2.114959233223293822, -1.785989328681826027, 0.4467204754193611627 ) ) ;
#108400 = CARTESIAN_POINT ( 'NONE',  ( 1.331197006551400497, 2.225188506942116895, 0.6113326355875832174 ) ) ;
#108401 = CARTESIAN_POINT ( 'NONE',  ( 4.248501033035879004, 6.049946853332221153, -1.599625672291273171 ) ) ;
#108402 = CARTESIAN_POINT ( 'NONE',  ( 3.655696586050953378, 0.5291108212043382775, -2.095698868369605616 ) ) ;
#108403 = CARTESIAN_POINT ( 'NONE',  ( 9.097684769969825780, 10.57271930550834860, -1.199719254218446718 ) ) ;
#108404 = CARTESIAN_POINT ( 'NONE',  ( -6.911959384868566758, 6.958374125301778790, 1.040834085586084257E-14 ) ) ;
#108405 = CARTESIAN_POINT ( 'NONE',  ( 3.146212962842390937, -0.1666923573656608759, -2.292372948102610053 ) ) ;
#108406 = VERTEX_POINT ( 'NONE', #211139 ) ;
#108407 = LINE ( 'NONE', #94246, #166789 ) ;
#108408 = MECHANICAL_DESIGN_GEOMETRIC_PRESENTATION_REPRESENTATION (  '', ( #21865 ), #122189 ) ;
#108409 = CARTESIAN_POINT ( 'NONE',  ( 1.270139834521961886, -1.189467451172643964, 1.443775233441677130 ) ) ;
#108410 = AXIS2_PLACEMENT_3D ( 'NONE', #131985, #195879, #16028 ) ;
#108411 = CARTESIAN_POINT ( 'NONE',  ( 5.137557537983609812, -1.393591726081166771, -1.394729141857486532 ) ) ;
#108413 = CARTESIAN_POINT ( 'NONE',  ( 7.239690839573049708, 11.39013037956983965, 1.040834085586084257E-14 ) ) ;
#108412 = CARTESIAN_POINT ( 'NONE',  ( 0.6823417656249917140, 4.342708333674755394, 1.181850606188765695 ) ) ;
#108415 = CARTESIAN_POINT ( 'NONE',  ( 0.7860941533469123499, 1.484900681275106438, 1.632775826992872492 ) ) ;
#108414 = CARTESIAN_POINT ( 'NONE',  ( -6.413170354464012846, 7.440785820751486312, 1.199719254218450271 ) ) ;
#108416 = EDGE_CURVE ( 'NONE', #4829, #115502, #87500, .T. ) ;
#108417 = CARTESIAN_POINT ( 'NONE',  ( -1.500000000000057065, 7.361490936992524325, -4.203511340218408776 ) ) ;
#108418 = CARTESIAN_POINT ( 'NONE',  ( 5.168682875307768931, 7.053215992657626110, -1.599625672291256295 ) ) ;
#108419 = CARTESIAN_POINT ( 'NONE',  ( -5.005985031943793295, 6.863401842066301661, -1.599625672291256295 ) ) ;
#108420 = CARTESIAN_POINT ( 'NONE',  ( 6.539320575229258026, 4.689551739520863904, 2.765837357486185866 ) ) ;
#108421 = CARTESIAN_POINT ( 'NONE',  ( 5.084826545086224669, -0.2406546161831616404, -1.956650619579934469 ) ) ;
#108422 = CARTESIAN_POINT ( 'NONE',  ( 5.637451635233869496, -2.088540497258955408, 0.9818693799023417990 ) ) ;
#108423 = CARTESIAN_POINT ( 'NONE',  ( 6.144940932578938586, -0.2738450275633330100, -1.840644705263774217 ) ) ;
#108424 = ADVANCED_FACE ( 'NONE', ( #162422 ), #67490, .T. ) ;
#108425 = CARTESIAN_POINT ( 'NONE',  ( 3.327062588944328603, -1.903923626093235955, -0.7937240881994469532 ) ) ;
#108426 = CARTESIAN_POINT ( 'NONE',  ( 5.151735183512854199, 8.954182114166247430, -0.7216878364870257245 ) ) ;
#108427 = CIRCLE ( 'NONE', #91061, 0.1000000000000000472 ) ;
#108428 = CARTESIAN_POINT ( 'NONE',  ( 4.435452530326143616, 5.203724702582467998, -1.199719254218452047 ) ) ;
#108429 = CARTESIAN_POINT ( 'NONE',  ( 6.114364089638775646, 10.07724917131317355, 0.7216878364870438212 ) ) ;
#108430 = CARTESIAN_POINT ( 'NONE',  ( 0.6823417656249917140, 3.405208333674754506, 1.181850606188765695 ) ) ;
#108431 = CARTESIAN_POINT ( 'NONE',  ( -5.520326499667782549, 14.55310517179796470, 10.61470576409842614 ) ) ;
#108432 = CARTESIAN_POINT ( 'NONE',  ( 6.778713616708431644, 7.010846762355714468, 1.040834085586084257E-14 ) ) ;
#108433 = CARTESIAN_POINT ( 'NONE',  ( 5.740740459546420205, -2.117024774779395102, -0.4812451790989195621 ) ) ;
#108435 = CARTESIAN_POINT ( 'NONE',  ( 4.581507094455529838, -0.8636776874328588871, 1.626104626046148249 ) ) ;
#108434 = DIRECTION ( 'NONE',  ( 0.000000000000000000, -1.000000000000000000, 0.000000000000000000 ) ) ;
#108437 = CARTESIAN_POINT ( 'NONE',  ( 6.620655732516668834, 7.629137130509086262, 2.526260288887293814 ) ) ;
#108436 = DIRECTION ( 'NONE',  ( 0.000000000000000000, 0.000000000000000000, -1.000000000000000000 ) ) ;
#108438 = FACE_OUTER_BOUND ( 'NONE', #60816, .T. ) ;
#108439 = CARTESIAN_POINT ( 'NONE',  ( -1.930226670627066099, 8.999999999999998224, -0.7749999999999996891 ) ) ;
#108440 = CARTESIAN_POINT ( 'NONE',  ( 0.4392367245290337840, 0.3885019757292383913, 2.228643277672849976 ) ) ;
#108441 = CARTESIAN_POINT ( 'NONE',  ( -3.983506901647102083, 7.838413813543339437, 0.2012387096505599549 ) ) ;
#108442 = CARTESIAN_POINT ( 'NONE',  ( -0.5773502691896470473, -2.500000000000002220, 0.9999999999999991118 ) ) ;
#108443 = CARTESIAN_POINT ( 'NONE',  ( 6.231590709102786008, 7.018523052454695765, 1.002697108273574500 ) ) ;
#108444 = CARTESIAN_POINT ( 'NONE',  ( -5.438229012412911345, 5.517224400669388018, -0.7216878364870338292 ) ) ;
#108445 = CARTESIAN_POINT ( 'NONE',  ( 0.08246951281144777879, -1.249137507218839094, 1.448023666807837895 ) ) ;
#108446 = CARTESIAN_POINT ( 'NONE',  ( 0.2679308956112765872, -1.161373500300251216, 1.335597826242039154 ) ) ;
#108447 = CARTESIAN_POINT ( 'NONE',  ( 5.742843059509288750, 1.940770921862687182, 0.5345600180575919014 ) ) ;
#108448 = B_SPLINE_CURVE_WITH_KNOTS ( 'NONE', 3,
 ( #208891, #107217, #7494, #174310, #57337, #126683, #172161, #11766, #24819, #10698, #76768, #90921, #188390, #156986, #205702, #125619, #44298, #124559 ),
 .UNSPECIFIED., .F., .F.,
 ( 4, 2, 2, 2, 2, 2, 2, 2, 4 ),
 ( -5.999999999904574585E-08, 0.001344200983021300467, 0.002688461966042599710, 0.004032722949063899387, 0.005376983932085199064, 0.006721244915106497873, 0.008065505898127794948, 0.009409766881149092890, 0.01075402786417039083 ),
 .UNSPECIFIED. ) ;
#108449 = CARTESIAN_POINT ( 'NONE',  ( 5.035963992472171746, 7.962709526937818083, 1.199719254218462483 ) ) ;
#108450 = CARTESIAN_POINT ( 'NONE',  ( 4.383879424978657902, 1.373869114255725776, 1.596202613037283502 ) ) ;
#108451 = CARTESIAN_POINT ( 'NONE',  ( 3.638217106272136903, 0.6927189700525613336, 1.786146362908203944 ) ) ;
#108452 = DIRECTION ( 'NONE',  ( 0.000000000000000000, -1.000000000000000000, 0.000000000000000000 ) ) ;
#108453 = CARTESIAN_POINT ( 'NONE',  ( 3.930098287398839041, 1.092129198686382141, 1.638800773490353802 ) ) ;
#108454 = CARTESIAN_POINT ( 'NONE',  ( 5.677991919488574624, 1.989193807575660555, -0.3493085226990484959 ) ) ;
#108455 = CARTESIAN_POINT ( 'NONE',  ( 3.133525119713890472, -1.255248497922526463, -1.387151338369890574 ) ) ;
#108458 = VERTEX_POINT ( 'NONE', #129995 ) ;
#108457 = CARTESIAN_POINT ( 'NONE',  ( 0.7910927259777954523, -0.04954035392716604758, -1.911929172785244102 ) ) ;
#108456 = CARTESIAN_POINT ( 'NONE',  ( 5.197747934024010696, -0.6158827634895787106, 1.611369335837910644 ) ) ;
#108460 = CARTESIAN_POINT ( 'NONE',  ( 4.582292731738905722, 5.408724944192588424, -1.082531754730548412 ) ) ;
#108459 = CARTESIAN_POINT ( 'NONE',  ( 2.860232119962682784, 2.196193069775736362, -0.2169517147150926140 ) ) ;
#108461 = CARTESIAN_POINT ( 'NONE',  ( -1.402160292154681736E-14, 1.509375000341420359, -1.575800808251659024 ) ) ;
#108462 = CARTESIAN_POINT ( 'NONE',  ( 0.1509074155349584279, -0.4535863444464246497, -2.019966333402842817 ) ) ;
#108463 = CARTESIAN_POINT ( 'NONE',  ( 6.401421083946654100, 10.62007503124645957, -0.7998128361456291469 ) ) ;
#108464 = CARTESIAN_POINT ( 'NONE',  ( -7.257245574617336992, -6.363025497629771543, 6.640718169120116698 ) ) ;
#108465 = CARTESIAN_POINT ( 'NONE',  ( 10.56536251450128994, 13.75961062549474612, 3.404319718479180690 ) ) ;
#108466 = CARTESIAN_POINT ( 'NONE',  ( -5.915435094264120508, 5.795762452929912101, 0.000000000000000000 ) ) ;
#108467 = VERTEX_POINT ( 'NONE', #42283 ) ;
#108468 = CARTESIAN_POINT ( 'NONE',  ( 2.260293373024503616, -2.069953001785612479, 0.04851313490940312168 ) ) ;
#108469 = CARTESIAN_POINT ( 'NONE',  ( -1.500000000000013101, 3.129166666666689967, -0.8660254037844313801 ) ) ;
#108470 = CARTESIAN_POINT ( 'NONE',  ( 6.796715079152391148, 6.823922435299587974, 0.7998128361456341429 ) ) ;
#108471 = CARTESIAN_POINT ( 'NONE',  ( 4.848976215542928792, 5.686169002002086970, 1.199719254218452047 ) ) ;
#108472 = CARTESIAN_POINT ( 'NONE',  ( 6.463548717370299457, -1.702720583769131490, -1.263627255760652046 ) ) ;
#108473 = CARTESIAN_POINT ( 'NONE',  ( 0.7500000000000006661, 10.36458333401613174, 1.299038105676657340 ) ) ;
#108474 = CARTESIAN_POINT ( 'NONE',  ( -1.201851678989727383E-14, 2.821875000341418804, 1.575800808251672791 ) ) ;
#108476 = CARTESIAN_POINT ( 'NONE',  ( 9.408995418203963013, 12.00024729270324286, 1.443375672974076540 ) ) ;
#108475 = CARTESIAN_POINT ( 'NONE',  ( -11.78331023100045627, 11.29999999999999893, -1.800000000000001155 ) ) ;
#108477 = CARTESIAN_POINT ( 'NONE',  ( 5.149767453795408123, -0.2439937967673235231, -2.001204641050558397 ) ) ;
#108478 = CARTESIAN_POINT ( 'NONE',  ( 5.085127819360848456, 1.569905733240322343, 1.097627489654330990 ) ) ;
#108479 = DIRECTION ( 'NONE',  ( 1.000000000000000000, 0.000000000000000000, 0.000000000000000000 ) ) ;
#108480 = CARTESIAN_POINT ( 'NONE',  ( 2.595491417077447238, -0.6846416945752286098, 2.081959150545972914 ) ) ;
#108481 = DIRECTION ( 'NONE',  ( 0.8736852521944931116, 0.05518364616837929254, 0.4833516786910004304 ) ) ;
#108482 = CARTESIAN_POINT ( 'NONE',  ( 1.499999999999987121, 2.077083334016153415, -0.8660254037844262731 ) ) ;
#108483 = CARTESIAN_POINT ( 'NONE',  ( 5.537363252524067470, -0.04518311473342268708, 2.012845415592057208 ) ) ;
#108484 = CARTESIAN_POINT ( 'NONE',  ( 1.212987991671743204, 1.561712320281399835, -1.103468303573502673 ) ) ;
#108485 = CARTESIAN_POINT ( 'NONE',  ( -5.042743069279040036, 7.970618449879118828, 1.199719254218464037 ) ) ;
#108487 = CARTESIAN_POINT ( 'NONE',  ( -0.05311194370935175268, -1.802413661875476913, -0.9041393574176490588 ) ) ;
#108486 = CARTESIAN_POINT ( 'NONE',  ( -15.75000000000000000, 10.19999999999999929, -1.800000000000001155 ) ) ;
#108488 = CARTESIAN_POINT ( 'NONE',  ( 0.6823417656249934904, 9.255208333674728394, 1.181850606188764807 ) ) ;
#108490 = CARTESIAN_POINT ( 'NONE',  ( -6.414942957921379474, 7.513130201443591005, -1.199719254218452047 ) ) ;
#108489 = CARTESIAN_POINT ( 'NONE',  ( 3.685174051874222201, 1.515783366363635531, 1.440268600269165589 ) ) ;
#108492 = ORIENTED_EDGE ( 'NONE', *, *, #116347, .T. ) ;
#108491 = CARTESIAN_POINT ( 'NONE',  ( 2.203723468020501119, -1.724507683567375826, 0.03868650182545228799 ) ) ;
#108493 = CARTESIAN_POINT ( 'NONE',  ( 6.222909436229170588, 1.570324008046734221, -1.425282903188800798 ) ) ;
#108494 = CARTESIAN_POINT ( 'NONE',  ( 6.959412922516382771, 7.013736585890911535, 0.7998128361456341429 ) ) ;
#108495 = LINE ( 'NONE', #158260, #161238 ) ;
#108496 = CARTESIAN_POINT ( 'NONE',  ( -6.042630808230841359E-15, -2.318749999044084298, 3.474999999999999645 ) ) ;
#108497 = DIRECTION ( 'NONE',  ( -0.6507913734559640506, -0.7592566023653004592, 0.000000000000000000 ) ) ;
#108498 = CARTESIAN_POINT ( 'NONE',  ( 6.518772930072240790, 6.499656594706071822, -0.7998128361456281477 ) ) ;
#108499 = DIRECTION ( 'NONE',  ( -0.000000000000000000, -1.000000000000000000, -0.000000000000000000 ) ) ;
#108500 = VERTEX_POINT ( 'NONE', #108395 ) ;
#108501 = CARTESIAN_POINT ( 'NONE',  ( 3.299258901807587741, 1.636513117289538188, -0.7770104639905143218 ) ) ;
#108502 = EDGE_LOOP ( 'NONE', ( #30455, #211498 ) ) ;
#108503 = CARTESIAN_POINT ( 'NONE',  ( 4.878236342818665250, 4.585697242910212523, 1.040834085586084257E-14 ) ) ;
#108504 = CIRCLE ( 'NONE', #46141, 9.479622692290801567 ) ;
#108505 = CARTESIAN_POINT ( 'NONE',  ( 5.896870467300973750, 5.844380064798101237, 0.7998128361456352531 ) ) ;
#108506 = CARTESIAN_POINT ( 'NONE',  ( 3.844242791777858770, 0.9658850817777319131, -1.532267982868290579 ) ) ;
#108507 = CARTESIAN_POINT ( 'NONE',  ( 6.539320575229232269, 1.262224698349242669, 2.111181586620724637 ) ) ;
#108508 = CARTESIAN_POINT ( 'NONE',  ( 5.731063993565963521, 6.075950606329157289, 0.6577720730673256577 ) ) ;
#108509 = CARTESIAN_POINT ( 'NONE',  ( 3.578407426278474190, 1.182412371022481645, -1.437126236693661241 ) ) ;
#108510 = CARTESIAN_POINT ( 'NONE',  ( 1.669406806874464300, 1.322410700044797327, 1.386144426805105523 ) ) ;
#108511 = CARTESIAN_POINT ( 'NONE',  ( 1.483130931141176889, 1.688290157389197077, -0.6950536248920418103 ) ) ;
#108512 = CARTESIAN_POINT ( 'NONE',  ( 4.831967907651305794, 8.093680561842322874, 0.8807274918286764898 ) ) ;
#108513 = DIRECTION ( 'NONE',  ( 0.000000000000000000, 1.000000000000000000, -8.546850786086437571E-32 ) ) ;
#108514 = CARTESIAN_POINT ( 'NONE',  ( 5.510920874727778696, 7.454463421478725316, 1.249874847645112697 ) ) ;
#108515 = CARTESIAN_POINT ( 'NONE',  ( -11.52469724861192901, 9.720000066487669343, 3.346365485506925808 ) ) ;
#108516 = CARTESIAN_POINT ( 'NONE',  ( -1.458833446111217569, 8.740432391875483376, -2.548463833528520794 ) ) ;
#108517 = CARTESIAN_POINT ( 'NONE',  ( 7.944714827928056167, 8.371181508778631652, 0.7216878364870458196 ) ) ;
#108518 = CARTESIAN_POINT ( 'NONE',  ( 5.295741323871941297, -1.389945570378407380, -1.395530913269894091 ) ) ;
#108519 = CARTESIAN_POINT ( 'NONE',  ( -5.928993247877788697, 5.811580298812519807, 0.7998128361456341429 ) ) ;
#108520 = CARTESIAN_POINT ( 'NONE',  ( -2.193105066167346795, 5.702484939155337607, 2.420000000000010587 ) ) ;
#108521 = CARTESIAN_POINT ( 'NONE',  ( 6.509741685903361663, -1.029359178063901092, -1.934661654277470166 ) ) ;
#108522 = CARTESIAN_POINT ( 'NONE',  ( 5.139640169905585587, -1.362188071541370116, -1.362388069303143823 ) ) ;
#108523 = CARTESIAN_POINT ( 'NONE',  ( -6.566226467720086113, 6.555019055295208119, 1.040834085586084257E-14 ) ) ;
#108524 = CARTESIAN_POINT ( 'NONE',  ( 0.9381830591699467092, 1.797733097909786304, 0.3167546781352030272 ) ) ;
#108525 = CARTESIAN_POINT ( 'NONE',  ( 1.787996309160574837, 1.523479866092191548, 1.596893430481533649 ) ) ;
#108526 = CARTESIAN_POINT ( 'NONE',  ( 0.4019237886466816012, 10.42633545031537423, -1.499999999999998668 ) ) ;
#108527 = CARTESIAN_POINT ( 'NONE',  ( 0.9844543725016400293, -1.211084316286781037, 1.480072698922259455 ) ) ;
#108528 = VERTEX_POINT ( 'NONE', #159205 ) ;
#108529 = CARTESIAN_POINT ( 'NONE',  ( 0.6605274321102487800, -0.6603073245880388686, -1.855717402334137622 ) ) ;
#108530 = CARTESIAN_POINT ( 'NONE',  ( 2.595178948467924851, -0.6067665810922833192, 1.844924317596825070 ) ) ;
#108531 = VERTEX_POINT ( 'NONE', #10806 ) ;
#108532 = FACE_OUTER_BOUND ( 'NONE', #149068, .T. ) ;
#108534 = CARTESIAN_POINT ( 'NONE',  ( 6.666864641256595725, 1.379314998728842445, -1.249469950728621326 ) ) ;
#108533 = CARTESIAN_POINT ( 'NONE',  ( -4.630991987519598396, 7.560518531151607213, 1.199719254218452935 ) ) ;
#108535 = CARTESIAN_POINT ( 'NONE',  ( 4.329849954717849947, 6.144853928627882489, 1.599625672291262513 ) ) ;
#108536 = FACE_OUTER_BOUND ( 'NONE', #45774, .T. ) ;
#108537 = CARTESIAN_POINT ( 'NONE',  ( 9.561524646135536543, 12.17819805862340310, -1.599625672291262513 ) ) ;
#108538 = CARTESIAN_POINT ( 'NONE',  ( -5.074494633264801990, 9.142270515442742607, 0.7998128361456291469 ) ) ;
#108539 = CARTESIAN_POINT ( 'NONE',  ( 2.823975127348025804, 1.215230906543849354, -1.823574674616668556 ) ) ;
#108540 = CARTESIAN_POINT ( 'NONE',  ( -10.97010717055062656, 9.799999999999997158, -1.696399592028410952 ) ) ;
#108541 = CARTESIAN_POINT ( 'NONE',  ( 10.99866081003787066, -6.614835951978784934, -0.2118258318330271950 ) ) ;
#108542 = CARTESIAN_POINT ( 'NONE',  ( 8.499999999999980460, 6.200000000000038369, 2.900000000000013678 ) ) ;
#108543 = CARTESIAN_POINT ( 'NONE',  ( 2.807047293222181494, 1.542382716246639474, 0.9765254425028799812 ) ) ;
#108544 = CARTESIAN_POINT ( 'NONE',  ( -9.164948653157990677, 11.71552606681625619, -1.443375672974059665 ) ) ;
#108545 = CARTESIAN_POINT ( 'NONE',  ( -5.730308518391983519, 7.387375129167091714, -1.324551712912255486 ) ) ;
#108546 = CARTESIAN_POINT ( 'NONE',  ( 1.359357947053562156E-15, 0.08000000000000020983, -11.09999999999999964 ) ) ;
#108547 = CARTESIAN_POINT ( 'NONE',  ( 8.106885785967500979, 11.54545161934907682, 1.199719254218460707 ) ) ;
#108548 = CARTESIAN_POINT ( 'NONE',  ( 1.383290355582541542, 1.780271273866357529, -0.7366933121468289825 ) ) ;
#108549 = CARTESIAN_POINT ( 'NONE',  ( 5.717619619964247946, 0.3862620380215216476, -1.923179868201368548 ) ) ;
#108550 = EDGE_CURVE ( 'NONE', #71711, #81797, #115935, .T. ) ;
#108551 = CARTESIAN_POINT ( 'NONE',  ( -1.402160292154681736E-14, 14.81249999999999645, 1.732050807568881190 ) ) ;
#108552 = CARTESIAN_POINT ( 'NONE',  ( -6.418895661066105873, 9.576129806964074120, -1.199719254218440723 ) ) ;
#108553 = CARTESIAN_POINT ( 'NONE',  ( 3.798255590122797898, 7.583048621785260401, -0.7998128361456221525 ) ) ;
#108554 = CARTESIAN_POINT ( 'NONE',  ( 4.775033345069852331, 2.044829088842615494, -0.7888500489584143738 ) ) ;
#108555 = CIRCLE ( 'NONE', #35805, 0.09999999999999999167 ) ;
#108556 = CIRCLE ( 'NONE', #32419, 2.250000000000006661 ) ;
#108557 = CARTESIAN_POINT ( 'NONE',  ( 5.183294799126148433, 4.941598775268944976, 1.040834085586084257E-14 ) ) ;
#108558 = CARTESIAN_POINT ( 'NONE',  ( -1.364853456228725115, 4.017025827590854803, -0.6233480900563461713 ) ) ;
#108559 = CARTESIAN_POINT ( 'NONE',  ( 5.541872263726007830, 1.386227983376321582, 1.537841262885197846 ) ) ;
#108561 = CARTESIAN_POINT ( 'NONE',  ( -1.364683531249997417, 2.571875000341422357, 1.214306433183764966E-14 ) ) ;
#108560 = CARTESIAN_POINT ( 'NONE',  ( -15.75000000000000000, 9.799999999999998934, 0.6999999999999992895 ) ) ;
#108562 = CIRCLE ( 'NONE', #15084, 0.07999999999999979350 ) ;
#108563 = CARTESIAN_POINT ( 'NONE',  ( 5.063244923127927954, -1.278613472530117035, 1.910113253385301801 ) ) ;
#108564 = CARTESIAN_POINT ( 'NONE',  ( 5.938108093105483931, 8.911247961056314892, -1.082531754730537088 ) ) ;
#108566 = CARTESIAN_POINT ( 'NONE',  ( 1.772826578343066117, 3.950000000000009059, 0.4499999999999590994 ) ) ;
#108565 = CARTESIAN_POINT ( 'NONE',  ( 5.722950238744209273, 6.809768379023969587, 1.082531754730549967 ) ) ;
#108567 = CARTESIAN_POINT ( 'NONE',  ( 0.5336625369133874974, -1.625122730996070297, -1.616870241932764074 ) ) ;
#108568 = CARTESIAN_POINT ( 'NONE',  ( -7.694877102302403848, -5.389939693150834543, -7.860745937262087146 ) ) ;
#108569 = CARTESIAN_POINT ( 'NONE',  ( -6.774234028683526532, 7.932303117332766718, 1.199719254218452047 ) ) ;
#108570 = CARTESIAN_POINT ( 'NONE',  ( 4.910071578948462800, 1.337895470842176193, -1.407775065355970412 ) ) ;
#108571 = EDGE_LOOP ( 'NONE', ( #6405, #6003, #144615, #88361, #135615, #175765, #167576, #15753 ) ) ;
#108572 = CARTESIAN_POINT ( 'NONE',  ( 9.693716643646595799, 11.37205284141829686, 1.082531754730548412 ) ) ;
#108573 = EDGE_CURVE ( 'NONE', #23435, #163739, #177603, .T. ) ;
#108574 = ORIENTED_EDGE ( 'NONE', *, *, #98948, .T. ) ;
#108575 = CARTESIAN_POINT ( 'NONE',  ( 4.728717205193702533, 1.314622909153417174, -1.389140896021365368 ) ) ;
#108576 = CARTESIAN_POINT ( 'NONE',  ( 6.194358799569198659, -1.717016665659231167, -0.1635641229304989064 ) ) ;
#108577 = CARTESIAN_POINT ( 'NONE',  ( 5.348842313791752900, -1.825074749614737701, -0.8578464102408298597 ) ) ;
#108579 = CARTESIAN_POINT ( 'NONE',  ( -3.201133666602369310, 6.748756687762456963, -0.7216878364870458196 ) ) ;
#108578 = CARTESIAN_POINT ( 'NONE',  ( -8.666686507633592385, 11.13422023037111330, 1.599625672291269396 ) ) ;
#108580 = CARTESIAN_POINT ( 'NONE',  ( 0.000000000000000000, -1.334374999522042859, -3.793834371823813001 ) ) ;
#108582 = CARTESIAN_POINT ( 'NONE',  ( 6.837169251635001999, -1.579311124772398767, 0.7986344709578310219 ) ) ;
#108581 = CARTESIAN_POINT ( 'NONE',  ( 1.605537313848971026, -2.074692111233501723, 0.2571424261670462452 ) ) ;
#108583 = CARTESIAN_POINT ( 'NONE',  ( 5.502577337681268332, -1.966645332631598908, 0.4444998760482973821 ) ) ;
#108585 = CARTESIAN_POINT ( 'NONE',  ( 3.310744302307960574, 2.072215845705066339, 0.9802597712869900448 ) ) ;
#108584 = CARTESIAN_POINT ( 'NONE',  ( 5.761288931164342486, 5.686201605971993978, -0.7998128361456481317 ) ) ;
#108586 = CARTESIAN_POINT ( 'NONE',  ( 2.290578643201816256, 1.344622755191619445, 1.104862870798990260 ) ) ;
#108587 = CARTESIAN_POINT ( 'NONE',  ( 3.058948843759463188, 0.5191580478346514704, 2.055925682384197373 ) ) ;
#108588 = CARTESIAN_POINT ( 'NONE',  ( 1.154700538379228147, -2.500000000000002220, -1.734723475976807094E-15 ) ) ;
#108589 = CARTESIAN_POINT ( 'NONE',  ( 1.686441086386183619, -0.9581320880991549549, -1.444804011637023322 ) ) ;
#108590 = CARTESIAN_POINT ( 'NONE',  ( -1.360316468750002672, 1.921875000341424666, -3.642919299551294898E-14 ) ) ;
#108591 = CARTESIAN_POINT ( 'NONE',  ( 1.943593235818155351, 1.280450557881509299, 1.350794863662147627 ) ) ;
#108592 = CARTESIAN_POINT ( 'NONE',  ( 2.875608777474625732, -0.2152533142569280078, 2.160498500671267585 ) ) ;
#108593 = CARTESIAN_POINT ( 'NONE',  ( 3.503138892209650024, -0.1435209762444041581, 2.011451614702438828 ) ) ;
#108594 = CARTESIAN_POINT ( 'NONE',  ( 5.187500000000002665, -1.451031289060905172, 1.451031289061322838 ) ) ;
#108595 = CARTESIAN_POINT ( 'NONE',  ( 0.7499999999999902300, 1.764583334016148086, 1.299038105676657340 ) ) ;
#108596 = CARTESIAN_POINT ( 'NONE',  ( 1.008667890995796457, 1.460797969510800876, -1.255919511179462322 ) ) ;
#108597 = CARTESIAN_POINT ( 'NONE',  ( 1.364683531249996529, 14.21354166700806942, 0.7879004041258405033 ) ) ;
#108598 = CARTESIAN_POINT ( 'NONE',  ( 3.146955363149469331, 2.168125099964354874, 0.4830323043785512138 ) ) ;
#108599 = ORIENTED_EDGE ( 'NONE', *, *, #142758, .F. ) ;
#108600 = PLANE ( 'NONE',  #101520 ) ;
#108601 = CARTESIAN_POINT ( 'NONE',  ( -0.7500000000000215383, 0.4416666666666874130, 1.299038105676659116 ) ) ;
#108602 = CARTESIAN_POINT ( 'NONE',  ( 7.507464373665139412, 9.781794407407920389, 1.599625672291281386 ) ) ;
#108603 = CARTESIAN_POINT ( 'NONE',  ( -1.402160292154681736E-14, -0.8031249996585825279, -1.575800808251665908 ) ) ;
#108604 = CARTESIAN_POINT ( 'NONE',  ( 5.941669428368816952, -2.091911387875099670, 0.7476460515099275783 ) ) ;
#108605 = CARTESIAN_POINT ( 'NONE',  ( 5.213317179658601752, -1.656387821537348426, -1.051046178410528942 ) ) ;
#108607 = CARTESIAN_POINT ( 'NONE',  ( -5.395781948558855845, 9.238903340053241209, 0.7216878364870458196 ) ) ;
#108606 = CARTESIAN_POINT ( 'NONE',  ( 9.788623719386617239, 11.48277776311499387, -1.082531754730537088 ) ) ;
#108608 = CARTESIAN_POINT ( 'NONE',  ( -5.064290697676250730, 7.960144884870772763, -1.236948567437242907 ) ) ;
#108609 = CARTESIAN_POINT ( 'NONE',  ( 6.028679731477588177, 2.178036183261321757, 0.6118574502519974478 ) ) ;
#108610 = CARTESIAN_POINT ( 'NONE',  ( -4.340018570150306232, 8.077455741901736985, -0.7216878364870338292 ) ) ;
#108611 = CARTESIAN_POINT ( 'NONE',  ( 2.576693429754982390, 1.349077690114818040, -1.560390594356737104 ) ) ;
#108612 = CARTESIAN_POINT ( 'NONE',  ( -6.663996196316808174, 7.733415969579778171, -1.199719254218446718 ) ) ;
#108613 = VERTEX_POINT ( 'NONE', #164539 ) ;
#108614 = CARTESIAN_POINT ( 'NONE',  ( 1.499999999999987121, 2.077083334016153415, -0.8660254037844262731 ) ) ;
#108615 = CARTESIAN_POINT ( 'NONE',  ( 1.364683531249990311, 3.696875000341416584, 1.214306433183764966E-14 ) ) ;
#108616 = CARTESIAN_POINT ( 'NONE',  ( 4.094877388769967652, 1.581529129216452612, -0.9985332613470513374 ) ) ;
#108617 = CARTESIAN_POINT ( 'NONE',  ( 2.935853622122220674, -1.419245300609776272, -0.9961633832534546595 ) ) ;
#108618 = CARTESIAN_POINT ( 'NONE',  ( -0.02329727741511803188, -2.225753042794619496, -0.5483686822410521744 ) ) ;
#108619 = CARTESIAN_POINT ( 'NONE',  ( 1.378255502416312117, 1.315327575222959622, 1.771799650011764538 ) ) ;
#108620 = CARTESIAN_POINT ( 'NONE',  ( 4.282818888323718376, 1.866831796845986435, -0.9415434926851961039 ) ) ;
#108621 = CARTESIAN_POINT ( 'NONE',  ( 5.806574285656749268, 1.713600856677459205, 0.9136399477176879724 ) ) ;
#108622 = CARTESIAN_POINT ( 'NONE',  ( 0.000000000000000000, -3.600000000000005862, -5.799999999999999822 ) ) ;
#108623 = CARTESIAN_POINT ( 'NONE',  ( 0.3749999999841767684, 2.052068128807281955, -2.222409888604170519E-14 ) ) ;
#108624 = CARTESIAN_POINT ( 'NONE',  ( 0.6685925339881376717, 1.356301626434471164, 1.492253803477984642 ) ) ;
#108625 = ADVANCED_FACE ( 'NONE', ( #81155 ), #150418, .F. ) ;
#108626 = SURFACE_STYLE_FILL_AREA ( #42519 ) ;
#108627 =( NAMED_UNIT ( * ) SI_UNIT ( $, .STERADIAN. ) SOLID_ANGLE_UNIT ( ) );
#108628 = CARTESIAN_POINT ( 'NONE',  ( 6.610000000000006537, 0.002781820520842553934, 2.000159646111852929 ) ) ;
#108629 = CARTESIAN_POINT ( 'NONE',  ( -8.045874094706015001, 11.47427131287732927, -1.199719254218446718 ) ) ;
#108630 = CARTESIAN_POINT ( 'NONE',  ( 5.635385404774530649, 9.726366738878972740, 0.7998128361456462443 ) ) ;
#108631 = CARTESIAN_POINT ( 'NONE',  ( 1.387358672531703974, 7.315968950352358391, 4.254625267140708544 ) ) ;
#108632 = CARTESIAN_POINT ( 'NONE',  ( 3.844227010333609584, 1.817057058749595777, 0.1772887374331885701 ) ) ;
#108633 = CARTESIAN_POINT ( 'NONE',  ( 2.661379449941482012, -1.919611247835448342, -1.088434722066232485 ) ) ;
#108634 = ORIENTED_EDGE ( 'NONE', *, *, #197058, .T. ) ;
#108635 = CARTESIAN_POINT ( 'NONE',  ( -2.984203208339354152, 6.495671153122273722, 0.000000000000000000 ) ) ;
#108636 = CARTESIAN_POINT ( 'NONE',  ( -1.642778471874998480, -1.888541666188708890, 2.845375778867863303 ) ) ;
#108637 = CARTESIAN_POINT ( 'NONE',  ( -8.076906825439122528, 10.44614393447756129, -1.599625672291263179 ) ) ;
#108638 = CARTESIAN_POINT ( 'NONE',  ( 1.476825778181306559, -1.425320297365587408, 1.431352559222300203 ) ) ;
#108639 = CARTESIAN_POINT ( 'NONE',  ( 11.86239285000045740, 9.719999999999982876, 1.812080536912751061 ) ) ;
#108640 = VERTEX_POINT ( 'NONE', #104891 ) ;
#108641 = CARTESIAN_POINT ( 'NONE',  ( -4.821859908315634158, 5.654533310236863564, 1.199719254218452935 ) ) ;
#108642 = CARTESIAN_POINT ( 'NONE',  ( 2.588518228195731741, 1.803668244214111871, 0.4575444346353977898 ) ) ;
#108643 = CARTESIAN_POINT ( 'NONE',  ( 3.083589872104280705, 5.684939719841914929, 1.199719254218450271 ) ) ;
#108644 = LINE ( 'NONE', #21951, #15840 ) ;
#108645 = VERTEX_POINT ( 'NONE', #205555 ) ;
#108646 = CARTESIAN_POINT ( 'NONE',  ( -5.066996723205291708, 6.934582148538044777, 1.599625672291267398 ) ) ;
#108647 = AXIS2_PLACEMENT_3D ( 'NONE', #187554, #191809, #89018 ) ;
#108648 = CARTESIAN_POINT ( 'NONE',  ( -9.182950115157607840, 9.607863310639020327, 0.7998128361456462443 ) ) ;
#108649 = CARTESIAN_POINT ( 'NONE',  ( 4.178209475066913647, -1.049361115903378883, 1.493786327181771068 ) ) ;
#108651 = FACE_OUTER_BOUND ( 'NONE', #2803, .T. ) ;
#108650 = CARTESIAN_POINT ( 'NONE',  ( -3.709037541790315640, 6.484905011134099340, -1.199719254218450271 ) ) ;
#108652 = CARTESIAN_POINT ( 'NONE',  ( 6.489313741793890422, 6.842916442627623219, -0.5960428994750706089 ) ) ;
#108653 = CARTESIAN_POINT ( 'NONE',  ( 0.6843859445029027988, -0.9204285295532282918, -1.469136994349945047 ) ) ;
#108654 = CARTESIAN_POINT ( 'NONE',  ( 5.753808258465379133, 0.7501079416377672837, 1.681592913607635964 ) ) ;
#108655 = CARTESIAN_POINT ( 'NONE',  ( 4.723409996707597536, -0.1167165639803491167, 2.304856601038312913 ) ) ;
#108656 = CARTESIAN_POINT ( 'NONE',  ( 4.366607992053101128, 7.252070536440704096, -1.199719254218448494 ) ) ;
#108657 = CARTESIAN_POINT ( 'NONE',  ( 0.3861014259941424887, -0.9735654513510684227, 1.816333823429964411 ) ) ;
#108658 = CARTESIAN_POINT ( 'NONE',  ( 7.644099680006512187, 7.812537802962739697, 1.040834085586084257E-14 ) ) ;
#108659 = CARTESIAN_POINT ( 'NONE',  ( 5.554211264220430877, 2.030576384096828502, -1.076727444025220803 ) ) ;
#108660 = CARTESIAN_POINT ( 'NONE',  ( -1.432341765624997709, 5.720312500512116038, 1.214306433183764966E-14 ) ) ;
#108661 = CARTESIAN_POINT ( 'NONE',  ( -6.912678218121246942, 9.158153569265168770, 1.599625672291269396 ) ) ;
#108662 = CARTESIAN_POINT ( 'NONE',  ( 5.207814216083940018, -1.861544245658670604, 0.1842191830812092979 ) ) ;
#108664 = CARTESIAN_POINT ( 'NONE',  ( -6.283277845290492714, 6.295188672452495915, -0.7998128361456362523 ) ) ;
#108663 = CARTESIAN_POINT ( 'NONE',  ( 2.338023529656753752, -1.104205016203146705, -1.561194055274425452 ) ) ;
#108665 = CARTESIAN_POINT ( 'NONE',  ( 4.037865812933420173, -1.521084700717803884, -1.599171214764223636 ) ) ;
#108666 = CARTESIAN_POINT ( 'NONE',  ( 4.311780797230674089, -1.305379566919599332, -1.666953740739559819 ) ) ;
#108667 = CARTESIAN_POINT ( 'NONE',  ( -1.225000000000044276, 0.5416666673494865414, -0.7072540797573158011 ) ) ;
#108668 = ADVANCED_FACE ( 'NONE', ( #172015 ), #195130, .T. ) ;
#108669 = CARTESIAN_POINT ( 'NONE',  ( -1.499999999999964029, 7.000000000000000000, 9.886859966642596476 ) ) ;
#108670 = CARTESIAN_POINT ( 'NONE',  ( -0.2108831679770926115, 5.723481173670196043, -2.491210874135452613 ) ) ;
#108671 = CARTESIAN_POINT ( 'NONE',  ( 5.031484404002879884, 6.963427452793765404, 1.443375672974065660 ) ) ;
#108672 = CARTESIAN_POINT ( 'NONE',  ( -5.519577934094894722, 7.532869904567736974, 1.443375672974058777 ) ) ;
#108673 = CARTESIAN_POINT ( 'NONE',  ( 1.958496456072187142, 2.301298802517747877, -0.1708829291464097622 ) ) ;
#108674 = CARTESIAN_POINT ( 'NONE',  ( 2.014041202081144011, 1.956828179156915315, -0.1411808619533050091 ) ) ;
#108675 = CARTESIAN_POINT ( 'NONE',  ( 1.347111479062087616E-15, -9.999999999999994671, -10.99999999999999112 ) ) ;
#108676 = CARTESIAN_POINT ( 'NONE',  ( 6.491093265613332441, 0.1965012520625461223, 2.053163312798581774 ) ) ;
#108677 = CARTESIAN_POINT ( 'NONE',  ( 3.551873057100287223, 5.166937871415542283, 1.443375672974062551 ) ) ;
#108678 = CARTESIAN_POINT ( 'NONE',  ( 4.153529959351897283, 1.954779968807466295, -0.4946301968136583849 ) ) ;
#108679 = CARTESIAN_POINT ( 'NONE',  ( 3.393283585170187688, 7.180857625999046867, 0.7998128361456271485 ) ) ;
#108680 = ORIENTED_EDGE ( 'NONE', *, *, #75612, .F. ) ;
#108681 = CARTESIAN_POINT ( 'NONE',  ( 4.329314735043091389, -1.561880650076686861, -1.275557594027726394 ) ) ;
#108682 = CARTESIAN_POINT ( 'NONE',  ( -9.809487834687324437, 11.40315621434539395, 1.199719254218462483 ) ) ;
#108683 = DIRECTION ( 'NONE',  ( -0.9999980456341538426, 0.000000000000000000, -0.001977050295941298105 ) ) ;
#108684 = CARTESIAN_POINT ( 'NONE',  ( 6.546325832964355662, 5.229711127717882491, -2.448021111374927283 ) ) ;
#108685 = CARTESIAN_POINT ( 'NONE',  ( 2.372313692266983853, 5.711523707712699682, 0.7216878364870438212 ) ) ;
#108686 = CARTESIAN_POINT ( 'NONE',  ( 1.692468234204123734, 1.072632775294654062, -1.887553939074837261 ) ) ;
#108687 = CARTESIAN_POINT ( 'NONE',  ( 4.908934136599710563, 7.884784371745123366, 1.199719254218451159 ) ) ;
#108688 = ADVANCED_FACE ( 'NONE', ( #72351 ), #46677, .T. ) ;
#108690 = CARTESIAN_POINT ( 'NONE',  ( 1.734723475976807094E-15, -3.469446951953614189E-15, -0.2913868168252300994 ) ) ;
#108689 = B_SPLINE_CURVE_WITH_KNOTS ( 'NONE', 3,
 ( #93970, #207683, #139515, #59303 ),
 .UNSPECIFIED., .F., .F.,
 ( 4, 4 ),
 ( 6.034005962835825582E-05, 0.0001895969026200138800 ),
 .UNSPECIFIED. ) ;
#108691 = CARTESIAN_POINT ( 'NONE',  ( 2.547943918863291302, 1.870051909910470878, 0.05015897750767356333 ) ) ;
#108692 = CARTESIAN_POINT ( 'NONE',  ( 0.3157904346527000139, -2.021491663516309156, 0.3995350904514202162 ) ) ;
#108694 = CARTESIAN_POINT ( 'NONE',  ( 6.727182134110222478, 0.005875948494733079785, 1.810970247402940547 ) ) ;
#108693 = CARTESIAN_POINT ( 'NONE',  ( -0.02244404828157658613, 5.719765766439059540, -2.783169749654360814 ) ) ;
#108695 = CARTESIAN_POINT ( 'NONE',  ( -1.364683531250014514, 0.7385416670080887647, -0.7879004041258289570 ) ) ;
#108696 = LINE ( 'NONE', #174724, #135218 ) ;
#108697 = VERTEX_POINT ( 'NONE', #186107 ) ;
#108698 = CARTESIAN_POINT ( 'NONE',  ( 3.492734469894549498, -1.843672829398452784, -0.5074192597756198575 ) ) ;
#108699 = CARTESIAN_POINT ( 'NONE',  ( 3.766244448481158802, -1.188900867318806176, 1.311211162958977328 ) ) ;
#108700 = CARTESIAN_POINT ( 'NONE',  ( 1.488763880571321030, -1.816176428755595706, -0.5988469716494760897 ) ) ;
#108701 = CARTESIAN_POINT ( 'NONE',  ( -3.903858165731105778, 6.641919395739846799, 1.199719254218464037 ) ) ;
#108703 = CARTESIAN_POINT ( 'NONE',  ( -0.1708952380198276444, -1.482394133889615828, -1.213259445456981167 ) ) ;
#108702 = DIRECTION ( 'NONE',  ( 0.000000000000000000, 1.000000000000000000, 0.000000000000000000 ) ) ;
#108704 = CARTESIAN_POINT ( 'NONE',  ( -1.500000000000015099, 0.1291666666666918539, -0.8660254037844383745 ) ) ;
#108705 = CARTESIAN_POINT ( 'NONE',  ( 0.6431357727456864515, -0.2518013131528433757, -2.054909676291870380 ) ) ;
#108706 = CARTESIAN_POINT ( 'NONE',  ( -0.6823417656250246877, -1.136458332991911790, 1.181850606188755259 ) ) ;
#108707 = CARTESIAN_POINT ( 'NONE',  ( 5.787941465827733722, -0.8397648285632768328, 1.671655200917811168 ) ) ;
#108708 = CARTESIAN_POINT ( 'NONE',  ( 1.963248404482214049, 0.3131683437365209710, -1.798463397695612809 ) ) ;
#108709 = EDGE_CURVE ( 'NONE', #101960, #62251, #37740, .T. ) ;
#108711 = CARTESIAN_POINT ( 'NONE',  ( 4.816695983655697511, 8.110494931179941247, 0.8576603160085185529 ) ) ;
#108710 = CARTESIAN_POINT ( 'NONE',  ( 5.338574060078519423, 2.173733305800494175, 0.3801736985692484305 ) ) ;
#108712 = CARTESIAN_POINT ( 'NONE',  ( -1.364683531250014514, -0.2614583329919080157, -0.7879004041258359514 ) ) ;
#108713 = CARTESIAN_POINT ( 'NONE',  ( 3.244635591053147916, -2.031700879476082466, -0.3553325473293292847 ) ) ;
#108715 = CARTESIAN_POINT ( 'NONE',  ( -6.877010230629689858, 9.046264573866535486, 1.599625672291283607 ) ) ;
#108714 = AXIS2_PLACEMENT_3D ( 'NONE', #206825, #207890, #58459 ) ;
#108716 = CARTESIAN_POINT ( 'NONE',  ( 7.567422294721922960, 11.98040977715095323, 0.7998128361456462443 ) ) ;
#108717 = CARTESIAN_POINT ( 'NONE',  ( 11.97185388258315264, 11.37999990720392418, -0.8311143155443054820 ) ) ;
#108718 = EDGE_CURVE ( 'NONE', #177991, #67059, #151941, .T. ) ;
#108719 = CARTESIAN_POINT ( 'NONE',  ( -0.06712591543029376717, -9.995102890834049347, -10.91960056525075018 ) ) ;
#108720 = CARTESIAN_POINT ( 'NONE',  ( 6.749980374757213575, 8.968339418673846097, 1.599625672291268286 ) ) ;
#108721 = CARTESIAN_POINT ( 'NONE',  ( 5.107906530550561541, 0.6527686194882609261, -1.964817160181751010 ) ) ;
#108723 = CARTESIAN_POINT ( 'NONE',  ( 1.364683531249986537, 0.6760416670080884316, 0.7879004041258500513 ) ) ;
#108722 = COLOUR_RGB ( '', 0.31764706, 0.68627451, 0.89019608) ;
#108724 = CARTESIAN_POINT ( 'NONE',  ( 2.073706595668877384, 2.069181010895416950, -0.6253580070983978390 ) ) ;
#108725 = CARTESIAN_POINT ( 'NONE',  ( -4.844715248835366417, 8.098060037232425401, 0.8884674472836263659 ) ) ;
#108727 = CARTESIAN_POINT ( 'NONE',  ( 2.014041202081144011, 1.956828179156915315, -0.1411808619533050091 ) ) ;
#108726 = CARTESIAN_POINT ( 'NONE',  ( 3.545573561795499540, -1.865266050240913520, 0.7750044584247675061 ) ) ;
#108728 = CARTESIAN_POINT ( 'NONE',  ( 6.720655732516679137, 3.688991442244013097, 2.587785764416630219 ) ) ;
#108731 = CARTESIAN_POINT ( 'NONE',  ( 6.982085921357777281, 7.248114451113292667, 1.040834085586084257E-14 ) ) ;
#108730 = CARTESIAN_POINT ( 'NONE',  ( 1.737500000000001155, -2.333333333333333037, 3.009438278150922130 ) ) ;
#108729 = FILL_AREA_STYLE ('',( #126058 ) ) ;
#108732 = CARTESIAN_POINT ( 'NONE',  ( -6.312203035614172286, 9.521931420595302953, -1.199719254218452047 ) ) ;
#108733 = CARTESIAN_POINT ( 'NONE',  ( 1.639861632979456418, 2.010800986640928656, -0.1531718788195315928 ) ) ;
#108735 = CARTESIAN_POINT ( 'NONE',  ( 6.233935805145816467, 2.167428969419796125, 0.3234103439683775894 ) ) ;
#108734 = CARTESIAN_POINT ( 'NONE',  ( -4.771579997005698459, 7.654261532226910525, -1.199719254218452047 ) ) ;
#108736 = DIRECTION ( 'NONE',  ( 0.5773502691896272854, 0.000000000000000000, -0.8164965809277250353 ) ) ;
#108737 = CARTESIAN_POINT ( 'NONE',  ( 5.765855477156511810, 0.5488314196105298359, -1.831976909803390896 ) ) ;
#108738 = CARTESIAN_POINT ( 'NONE',  ( -2.266184231778562541, 5.795632037050281404, 1.040834085586084257E-14 ) ) ;
#108739 = CARTESIAN_POINT ( 'NONE',  ( 5.083944415000174466, 7.914723669933440675, -1.082531754730549078 ) ) ;
#108741 = CARTESIAN_POINT ( 'NONE',  ( 3.058220425488000327, -1.198843740453523266, 1.621196181159669347 ) ) ;
#108740 = CARTESIAN_POINT ( 'NONE',  ( -8.961576348508652146, 10.51788916375733685, -1.082531754730543083 ) ) ;
#108742 = CARTESIAN_POINT ( 'NONE',  ( -0.7499999999999972244, 3.358333333333359150, -1.299038105676652011 ) ) ;
#108743 = CARTESIAN_POINT ( 'NONE',  ( 1.364683531249996529, 14.27604166700806942, 0.7879004041258405033 ) ) ;
#108744 = CARTESIAN_POINT ( 'NONE',  ( 5.684504558281781250, -1.683600953293447944, -0.3737579273616030706 ) ) ;
#108745 = CARTESIAN_POINT ( 'NONE',  ( 6.770317605177710085, 8.992066187497757213, 1.599625672291268286 ) ) ;
#108746 = CARTESIAN_POINT ( 'NONE',  ( 8.581948047770334043, 12.95609712246668899, 0.000000000000000000 ) ) ;
#108747 = CARTESIAN_POINT ( 'NONE',  ( -0.3405876332338036439, 3.079852035184873049, 0.4461735512527613690 ) ) ;
#108748 = CARTESIAN_POINT ( 'NONE',  ( 4.692568346783878575, -0.4079999995015987091, -1.825350503840660110 ) ) ;
#108749 =( BOUNDED_SURFACE ( )  B_SPLINE_SURFACE ( 1, 2, ( 
 ( #39858, #186084, #168777, #188218, #38784, #169843, #156815, #87538, #105967, #71253, #103793, #8402, #74487, #21430, #139504, #121186, #171989, #23581, #189294, #42010, #20382, #137367, #120105, #187155, #104865, #89688, #155739, #40934, #7324, #140593, #73401, #86466, #57168, #206604, #152530, #59292, #176262, #157887, #145918, #77676, #110253, #27863, #210867, #143797, #211930, #95021, #44132, #61429, #194623, #127596, #28937, #192480, #177323, #111319, #62492, #93960, #209794, #161071, #195705, #11602, #142720, #79806, #109193, #9479, #12662, #25719, #160001, #78736, #43080, #175205, #46266, #96091, #174146, #193562, #144860, #162146, #158937, #92892, #63564, #128657, #26787, #112383, #108119, #125451, #207673, #178395, #30007, #13733, #10533, #76606, #129721, #91828, #45205, #75551, #141662, #191413, #208729, #60356, #126519, #97156, #32133, #80884, #115567, #183701, #163211, #116632, #47340, #151222, #113454, #68862, #180513, #649, #131807, #117710, #84068, #182626, #165322, #134981, #14793, #49448, #82996, #197816, #66714, #17980, #181563, #146974, #212991, #132858, #198863, #33191, #149071, #31083, #101386, #99274, #167461, #98214, #150157, #1726, #35309, #65659, #130768, #16916, #50510, #19056, #34249, #48406, #64629, #196763, #114518, #164265, #2790, #15854, #100322, #166388, #81940, #148024, #199938, #67783, #214034, #133933, #51585, #85135, #179459, #52637, #53707, #70990, #87273, #153341, #121994, #105690, #200991, #5991, #139236, #119840, #170650, #169587, #185819, #136034, #54774, #187960, #152277, #4913, #39588, #120921, #21170, #72062, #37450, #7059, #138172, #103528, #137103, #203132, #186894, #69923, #86205, #204182, #55838, #38526, #118765, #36378, #22237, #171718, #23317, #184750, #104603, #88348, #154412, #89425, #155476, #202047, #102455, #205267, #73132, #168521, #20120, #3850, #134623, #83692, #52275, #15484, #281, #65295, #117334, #33880, #200628, #131442, #50142, #118402, #149780, #66353, #167098, #32824, #85837, #18687, #98899, #82626, #132497, #164953, #49086, #213671, #150855 ),
 ( #148712, #2419, #151915, #183333, #184388, #84769, #197445, #68496, #1355, #102088, #166022, #115204, #168157, #36007, #67417, #51211, #199567, #182255, #133558, #19756, #16545, #99957, #53335, #31773, #3488, #201690, #181196, #69558, #34937, #135668, #180147, #97843, #163908, #81570, #147655, #198497, #116264, #101009, #17607, #204892, #136734, #119468, #187594, #203825, #120551, #123769, #38159, #171349, #104232, #202758, #173518, #57609, #186529, #90122, #154045, #22942, #39219, #73855, #74924, #8846, #170278, #20810, #54411, #152974, #89058, #21864, #139950, #155115, #189729, #6699, #185456, #121625, #105311, #41382, #70620, #72775, #169218, #157253, #138874, #56543, #122705, #7766, #188669, #141037, #106409, #55469, #40299, #205976, #172432, #24020, #156189, #107492, #25092, #91192, #207044, #37078, #103157, #86906, #4547, #5610, #87972, #71693, #137806, #2042, #37783, #36701, #8208, #182956, #167783, #18310, #70252, #201317, #102786, #152595, #118030, #34571, #184016, #166719, #52957, #58032, #100643, #202385, #133183, #25525, #199183, #157685, #51907, #86529, #3112, #206407, #169907, #54035, #168844, #9283, #84395, #135304, #20447, #69183, #4181, #103857, #119095, #150482, #68112, #136365, #120172, #185075, #186149, #116957, #190159, #21494, #41814, #35633, #90555, #156618, #124196, #151545, #134249, #74293, #140388, #107927, #173951, #200255, #101710, #19379, #85459, #91633, #50830, #142517, #78543, #194430, #110053, #108987, #13543, #178197, #191216, #76408, #46071, #43938, #47142, #141468, #126317, #61235, #77478, #143597, #95898, #211732, #75355, #210675, #179264, #60162, #160874, #176066, #208526, #10334, #193363, #161951, #175006, #159797, #79613, #45008, #27663, #62303, #192277, #195506, #128462, #93758, #11400, #209589, #127390, #158739, #26592, #112192, #29813, #111118, #207476, #59095, #28738, #145732, #63370, #96965, #177121, #94823, #12468, #144660, #129526, #92693, #113259, #30887, #163013, #125255, #42879, #48212, #167272, #117511, #130580, #15661, #199744, #197617, #200799, #80692, #65467 ) ),
 .UNSPECIFIED., .F., .F., .F. ) 
 B_SPLINE_SURFACE_WITH_KNOTS ( ( 2, 2 ),
 ( 3, 2, 2, 2, 2, 2, 2, 2, 2, 2, 2, 2, 2, 2, 2, 2, 2, 2, 2, 2, 2, 2, 2, 2, 2, 2, 2, 2, 2, 2, 2, 2, 2, 2, 2, 2, 2, 2, 2, 2, 2, 2, 2, 2, 2, 2, 2, 2, 2, 2, 2, 2, 2, 2, 2, 2, 2, 2, 2, 2, 2, 2, 2, 2, 2, 2, 2, 2, 2, 2, 2, 2, 2, 2, 2, 2, 2, 2, 2, 2, 2, 2, 2, 2, 2, 2, 2, 2, 2, 2, 2, 2, 2, 2, 2, 2, 2, 2, 2, 2, 2, 2, 2, 2, 2, 2, 2, 2, 2, 2, 2, 2, 2, 2, 2, 2, 2, 2, 2, 2, 3 ),
 ( 0.000000000000000000, 1.000000000000000000 ),
 ( 0.000000000000000000, 0.008333333333333333218, 0.01666666666666666644, 0.02500000000000000139, 0.03333333333333333287, 0.04166666666666666435, 0.05000000000000000278, 0.05833333333333333426, 0.06666666666666666574, 0.07499999999999999722, 0.08333333333333332871, 0.09166666666666666019, 0.1000000000000000056, 0.1083333333333333370, 0.1166666666666666685, 0.1250000000000000000, 0.1333333333333333315, 0.1416666666666666630, 0.1499999999999999944, 0.1583333333333333259, 0.1666666666666666574, 0.1749999999999999889, 0.1833333333333333204, 0.1916666666666666796, 0.2000000000000000111, 0.2083333333333333426, 0.2166666666666666741, 0.2250000000000000056, 0.2333333333333333370, 0.2416666666666666685, 0.2500000000000000000, 0.2583333333333333592, 0.2666666666666666630, 0.2750000000000000222, 0.2833333333333333259, 0.2916666666666666852, 0.2999999999999999889, 0.3083333333333333481, 0.3166666666666666519, 0.3250000000000000111, 0.3333333333333333148, 0.3416666666666666741, 0.3499999999999999778, 0.3583333333333333370, 0.3666666666666666408, 0.3750000000000000000, 0.3833333333333333592, 0.3916666666666666630, 0.4000000000000000222, 0.4083333333333333259, 0.4166666666666666852, 0.4249999999999999889, 0.4333333333333333481, 0.4416666666666666519, 0.4500000000000000111, 0.4583333333333333148, 0.4666666666666666741, 0.4749999999999999778, 0.4833333333333333370, 0.4916666666666666408, 0.5000000000000000000, 0.5083333333333333037, 0.5166666666666667185, 0.5250000000000000222, 0.5333333333333333259, 0.5416666666666666297, 0.5500000000000000444, 0.5583333333333333481, 0.5666666666666666519, 0.5749999999999999556, 0.5833333333333333703, 0.5916666666666666741, 0.5999999999999999778, 0.6083333333333332815, 0.6166666666666666963, 0.6250000000000000000, 0.6333333333333333037, 0.6416666666666667185, 0.6500000000000000222, 0.6583333333333333259, 0.6666666666666666297, 0.6750000000000000444, 0.6833333333333333481, 0.6916666666666666519, 0.6999999999999999556, 0.7083333333333333703, 0.7166666666666666741, 0.7249999999999999778, 0.7333333333333332815, 0.7416666666666666963, 0.7500000000000000000, 0.7583333333333333037, 0.7666666666666667185, 0.7750000000000000222, 0.7833333333333333259, 0.7916666666666666297, 0.8000000000000000444, 0.8083333333333333481, 0.8166666666666666519, 0.8249999999999999556, 0.8333333333333333703, 0.8416666666666666741, 0.8499999999999999778, 0.8583333333333332815, 0.8666666666666666963, 0.8750000000000000000, 0.8833333333333333037, 0.8916666666666667185, 0.9000000000000000222, 0.9083333333333333259, 0.9166666666666666297, 0.9250000000000000444, 0.9333333333333333481, 0.9416666666666666519, 0.9499999999999999556, 0.9583333333333333703, 0.9666666666666666741, 0.9749999999999999778, 0.9833333333333332815, 0.9916666666666666963, 1.000000000000000000 ),
 .UNSPECIFIED. ) 
 GEOMETRIC_REPRESENTATION_ITEM ( )  RATIONAL_B_SPLINE_SURFACE ( (
 ( 1.000000000000000000, 0.8660254037844387076, 1.000000000000000000, 0.8660254037844387076, 1.000000000000000000, 0.8660254037844387076, 1.000000000000000000, 0.8660254037844387076, 1.000000000000000000, 0.8660254037844387076, 1.000000000000000000, 0.8660254037844387076, 1.000000000000000000, 0.8660254037844387076, 1.000000000000000000, 0.8660254037844387076, 1.000000000000000000, 0.8660254037844387076, 1.000000000000000000, 0.8660254037844387076, 1.000000000000000000, 0.8660254037844387076, 1.000000000000000000, 0.8660254037844387076, 1.000000000000000000, 0.8660254037844387076, 1.000000000000000000, 0.8660254037844387076, 1.000000000000000000, 0.8660254037844387076, 1.000000000000000000, 0.8660254037844387076, 1.000000000000000000, 0.8660254037844387076, 1.000000000000000000, 0.8660254037844387076, 1.000000000000000000, 0.8660254037844387076, 1.000000000000000000, 0.8660254037844387076, 1.000000000000000000, 0.8660254037844387076, 1.000000000000000000, 0.8660254037844387076, 1.000000000000000000, 0.8660254037844387076, 1.000000000000000000, 0.8660254037844387076, 1.000000000000000000, 0.8660254037844387076, 1.000000000000000000, 0.8660254037844387076, 1.000000000000000000, 0.8660254037844387076, 1.000000000000000000, 0.8660254037844387076, 1.000000000000000000, 0.8660254037844387076, 1.000000000000000000, 0.8660254037844387076, 1.000000000000000000, 0.8660254037844387076, 1.000000000000000000, 0.8660254037844387076, 1.000000000000000000, 0.8660254037844387076, 1.000000000000000000, 0.8660254037844387076, 1.000000000000000000, 0.8660254037844387076, 1.000000000000000000, 0.8660254037844387076, 1.000000000000000000, 0.8660254037844387076, 1.000000000000000000, 0.8660254037844387076, 1.000000000000000000, 0.8660254037844387076, 1.000000000000000000, 0.8660254037844387076, 1.000000000000000000, 0.8660254037844387076, 1.000000000000000000, 0.8660254037844387076, 1.000000000000000000, 0.8660254037844387076, 1.000000000000000000, 0.8660254037844387076, 1.000000000000000000, 0.8660254037844387076, 1.000000000000000000, 0.8660254037844387076, 1.000000000000000000, 0.8660254037844387076, 1.000000000000000000, 0.8660254037844387076, 1.000000000000000000, 0.8660254037844387076, 1.000000000000000000, 0.8660254037844387076, 1.000000000000000000, 0.8660254037844387076, 1.000000000000000000, 0.8660254037844387076, 1.000000000000000000, 0.8660254037844387076, 1.000000000000000000, 0.8660254037844387076, 1.000000000000000000, 0.8660254037844387076, 1.000000000000000000, 0.8660254037844387076, 1.000000000000000000, 0.8660254037844387076, 1.000000000000000000, 0.8660254037844387076, 1.000000000000000000, 0.8660254037844387076, 1.000000000000000000, 0.8660254037844387076, 1.000000000000000000, 0.8660254037844387076, 1.000000000000000000, 0.8660254037844387076, 1.000000000000000000, 0.8660254037844387076, 1.000000000000000000, 0.8660254037844387076, 1.000000000000000000, 0.8660254037844387076, 1.000000000000000000, 0.8660254037844387076, 1.000000000000000000, 0.8660254037844387076, 1.000000000000000000, 0.8660254037844387076, 1.000000000000000000, 0.8660254037844387076, 1.000000000000000000, 0.8660254037844387076, 1.000000000000000000, 0.8660254037844387076, 1.000000000000000000, 0.8660254037844387076, 1.000000000000000000, 0.8660254037844387076, 1.000000000000000000, 0.8660254037844387076, 1.000000000000000000, 0.8660254037844387076, 1.000000000000000000, 0.8660254037844387076, 1.000000000000000000, 0.8660254037844387076, 1.000000000000000000, 0.8660254037844387076, 1.000000000000000000, 0.8660254037844387076, 1.000000000000000000, 0.8660254037844387076, 1.000000000000000000, 0.8660254037844387076, 1.000000000000000000, 0.8660254037844387076, 1.000000000000000000, 0.8660254037844387076, 1.000000000000000000, 0.8660254037844387076, 1.000000000000000000, 0.8660254037844387076, 1.000000000000000000, 0.8660254037844387076, 1.000000000000000000, 0.8660254037844387076, 1.000000000000000000, 0.8660254037844387076, 1.000000000000000000, 0.8660254037844387076, 1.000000000000000000, 0.8660254037844387076, 1.000000000000000000, 0.8660254037844387076, 1.000000000000000000, 0.8660254037844387076, 1.000000000000000000, 0.8660254037844387076, 1.000000000000000000, 0.8660254037844387076, 1.000000000000000000, 0.8660254037844387076, 1.000000000000000000, 0.8660254037844387076, 1.000000000000000000, 0.8660254037844387076, 1.000000000000000000, 0.8660254037844387076, 1.000000000000000000, 0.8660254037844387076, 1.000000000000000000, 0.8660254037844387076, 1.000000000000000000, 0.8660254037844387076, 1.000000000000000000, 0.8660254037844387076, 1.000000000000000000, 0.8660254037844387076, 1.000000000000000000, 0.8660254037844387076, 1.000000000000000000, 0.8660254037844387076, 1.000000000000000000, 0.8660254037844387076, 1.000000000000000000, 0.8660254037844387076, 1.000000000000000000, 0.8660254037844387076, 1.000000000000000000, 0.8660254037844387076, 1.000000000000000000, 0.8660254037844387076, 1.000000000000000000, 0.8660254037844387076, 1.000000000000000000, 0.8660254037844387076, 1.000000000000000000, 0.8660254037844387076, 1.000000000000000000, 0.8660254037844387076, 1.000000000000000000, 0.8660254037844387076, 1.000000000000000000, 0.8660254037844387076, 1.000000000000000000, 0.8660254037844387076, 1.000000000000000000, 0.8660254037844387076, 1.000000000000000000, 0.8660254037844387076, 1.000000000000000000, 0.8660254037844387076, 1.000000000000000000),
 ( 1.000000000000000000, 0.8660254037844387076, 1.000000000000000000, 0.8660254037844387076, 1.000000000000000000, 0.8660254037844387076, 1.000000000000000000, 0.8660254037844387076, 1.000000000000000000, 0.8660254037844387076, 1.000000000000000000, 0.8660254037844387076, 1.000000000000000000, 0.8660254037844387076, 1.000000000000000000, 0.8660254037844387076, 1.000000000000000000, 0.8660254037844387076, 1.000000000000000000, 0.8660254037844387076, 1.000000000000000000, 0.8660254037844387076, 1.000000000000000000, 0.8660254037844387076, 1.000000000000000000, 0.8660254037844387076, 1.000000000000000000, 0.8660254037844387076, 1.000000000000000000, 0.8660254037844387076, 1.000000000000000000, 0.8660254037844387076, 1.000000000000000000, 0.8660254037844387076, 1.000000000000000000, 0.8660254037844387076, 1.000000000000000000, 0.8660254037844387076, 1.000000000000000000, 0.8660254037844387076, 1.000000000000000000, 0.8660254037844387076, 1.000000000000000000, 0.8660254037844387076, 1.000000000000000000, 0.8660254037844387076, 1.000000000000000000, 0.8660254037844387076, 1.000000000000000000, 0.8660254037844387076, 1.000000000000000000, 0.8660254037844387076, 1.000000000000000000, 0.8660254037844387076, 1.000000000000000000, 0.8660254037844387076, 1.000000000000000000, 0.8660254037844387076, 1.000000000000000000, 0.8660254037844387076, 1.000000000000000000, 0.8660254037844387076, 1.000000000000000000, 0.8660254037844387076, 1.000000000000000000, 0.8660254037844387076, 1.000000000000000000, 0.8660254037844387076, 1.000000000000000000, 0.8660254037844387076, 1.000000000000000000, 0.8660254037844387076, 1.000000000000000000, 0.8660254037844387076, 1.000000000000000000, 0.8660254037844387076, 1.000000000000000000, 0.8660254037844387076, 1.000000000000000000, 0.8660254037844387076, 1.000000000000000000, 0.8660254037844387076, 1.000000000000000000, 0.8660254037844387076, 1.000000000000000000, 0.8660254037844387076, 1.000000000000000000, 0.8660254037844387076, 1.000000000000000000, 0.8660254037844387076, 1.000000000000000000, 0.8660254037844387076, 1.000000000000000000, 0.8660254037844387076, 1.000000000000000000, 0.8660254037844387076, 1.000000000000000000, 0.8660254037844387076, 1.000000000000000000, 0.8660254037844387076, 1.000000000000000000, 0.8660254037844387076, 1.000000000000000000, 0.8660254037844387076, 1.000000000000000000, 0.8660254037844387076, 1.000000000000000000, 0.8660254037844387076, 1.000000000000000000, 0.8660254037844387076, 1.000000000000000000, 0.8660254037844387076, 1.000000000000000000, 0.8660254037844387076, 1.000000000000000000, 0.8660254037844387076, 1.000000000000000000, 0.8660254037844387076, 1.000000000000000000, 0.8660254037844387076, 1.000000000000000000, 0.8660254037844387076, 1.000000000000000000, 0.8660254037844387076, 1.000000000000000000, 0.8660254037844387076, 1.000000000000000000, 0.8660254037844387076, 1.000000000000000000, 0.8660254037844387076, 1.000000000000000000, 0.8660254037844387076, 1.000000000000000000, 0.8660254037844387076, 1.000000000000000000, 0.8660254037844387076, 1.000000000000000000, 0.8660254037844387076, 1.000000000000000000, 0.8660254037844387076, 1.000000000000000000, 0.8660254037844387076, 1.000000000000000000, 0.8660254037844387076, 1.000000000000000000, 0.8660254037844387076, 1.000000000000000000, 0.8660254037844387076, 1.000000000000000000, 0.8660254037844387076, 1.000000000000000000, 0.8660254037844387076, 1.000000000000000000, 0.8660254037844387076, 1.000000000000000000, 0.8660254037844387076, 1.000000000000000000, 0.8660254037844387076, 1.000000000000000000, 0.8660254037844387076, 1.000000000000000000, 0.8660254037844387076, 1.000000000000000000, 0.8660254037844387076, 1.000000000000000000, 0.8660254037844387076, 1.000000000000000000, 0.8660254037844387076, 1.000000000000000000, 0.8660254037844387076, 1.000000000000000000, 0.8660254037844387076, 1.000000000000000000, 0.8660254037844387076, 1.000000000000000000, 0.8660254037844387076, 1.000000000000000000, 0.8660254037844387076, 1.000000000000000000, 0.8660254037844387076, 1.000000000000000000, 0.8660254037844387076, 1.000000000000000000, 0.8660254037844387076, 1.000000000000000000, 0.8660254037844387076, 1.000000000000000000, 0.8660254037844387076, 1.000000000000000000, 0.8660254037844387076, 1.000000000000000000, 0.8660254037844387076, 1.000000000000000000, 0.8660254037844387076, 1.000000000000000000, 0.8660254037844387076, 1.000000000000000000, 0.8660254037844387076, 1.000000000000000000, 0.8660254037844387076, 1.000000000000000000, 0.8660254037844387076, 1.000000000000000000, 0.8660254037844387076, 1.000000000000000000, 0.8660254037844387076, 1.000000000000000000, 0.8660254037844387076, 1.000000000000000000, 0.8660254037844387076, 1.000000000000000000, 0.8660254037844387076, 1.000000000000000000, 0.8660254037844387076, 1.000000000000000000, 0.8660254037844387076, 1.000000000000000000, 0.8660254037844387076, 1.000000000000000000, 0.8660254037844387076, 1.000000000000000000, 0.8660254037844387076, 1.000000000000000000, 0.8660254037844387076, 1.000000000000000000, 0.8660254037844387076, 1.000000000000000000, 0.8660254037844387076, 1.000000000000000000, 0.8660254037844387076, 1.000000000000000000, 0.8660254037844387076, 1.000000000000000000, 0.8660254037844387076, 1.000000000000000000, 0.8660254037844387076, 1.000000000000000000, 0.8660254037844387076, 1.000000000000000000, 0.8660254037844387076, 1.000000000000000000) ) ) 
 REPRESENTATION_ITEM ( '' )  SURFACE ( )  );
#108750 =( LENGTH_UNIT ( ) NAMED_UNIT ( * ) SI_UNIT ( .MILLI., .METRE. ) );
#108751 = CARTESIAN_POINT ( 'NONE',  ( 0.7607008448355724317, -0.6940761377024067258, -1.950597895851911456 ) ) ;
#108752 = CARTESIAN_POINT ( 'NONE',  ( -11.43209210103587559, 12.44403924016082819, 3.649125173352122609 ) ) ;
#108753 = VERTEX_POINT ( 'NONE', #112410 ) ;
#108754 = CARTESIAN_POINT ( 'NONE',  ( 3.932747076415766596, 6.745899468197171345, 1.199719254218451159 ) ) ;
#108755 = CARTESIAN_POINT ( 'NONE',  ( -11.89942855770814134, 11.37999999999999901, -0.7000000000000009548 ) ) ;
#108756 = CARTESIAN_POINT ( 'NONE',  ( -0.01774202353897573470, -1.183624524064251116, 1.371566177806067932 ) ) ;
#108757 = CARTESIAN_POINT ( 'NONE',  ( 4.190878879955609371, 7.903459436674603822, -0.7216878364870338292 ) ) ;
#108758 = CARTESIAN_POINT ( 'NONE',  ( 0.08191116107305261573, 2.527130371385647667, -1.998427156035398777 ) ) ;
#108759 = ORIENTED_EDGE ( 'NONE', *, *, #4855, .F. ) ;
#108760 = CARTESIAN_POINT ( 'NONE',  ( 7.727784369665023689, 11.95957283134381477, 1.040834085586084257E-14 ) ) ;
#108762 = CARTESIAN_POINT ( 'NONE',  ( 6.726816770674637347, 10.99970333242910669, -0.7998128361456291469 ) ) ;
#108761 = CARTESIAN_POINT ( 'NONE',  ( 0.9241798626423223251, 0.9638202082158978667, 1.708698881219716137 ) ) ;
#108763 = CARTESIAN_POINT ( 'NONE',  ( 5.114804650195723390, 0.1453347504645576271, 1.910168102697987313 ) ) ;
#108764 =( NAMED_UNIT ( * ) PLANE_ANGLE_UNIT ( ) SI_UNIT ( $, .RADIAN. ) );
#108765 = DIRECTION ( 'NONE',  ( 9.436895709313856232E-16, -0.8656921114426506803, -0.5005768354468324022 ) ) ;
#108766 = CIRCLE ( 'NONE', #153693, 0.08000000000000020983 ) ;
#108767 = CARTESIAN_POINT ( 'NONE',  ( 1.224999999999979661, 0.6249999999999866773, -2.775557561562891351E-14 ) ) ;
#108769 = ORIENTED_EDGE ( 'NONE', *, *, #199503, .T. ) ;
#108768 = CARTESIAN_POINT ( 'NONE',  ( 3.226477370372293763, 6.708047998835573900, 0.7216878364870317197 ) ) ;
#108770 = CARTESIAN_POINT ( 'NONE',  ( -8.568389894156720032, 10.05917163368005163, 1.082531754730558626 ) ) ;
#108771 = CARTESIAN_POINT ( 'NONE',  ( 2.606508400632711719, -0.8264410288459265175, -1.997682696722333562 ) ) ;
#108772 = CARTESIAN_POINT ( 'NONE',  ( -3.800028193580205382, 7.655393002477360653, -0.7998128361456481317 ) ) ;
#108773 = CARTESIAN_POINT ( 'NONE',  ( 6.536439455564155843, 8.719208346281938304, 1.443375672974065660 ) ) ;
#108774 = CARTESIAN_POINT ( 'NONE',  ( -3.440018289565379028, 5.036440642624797626, 1.599625672291267398 ) ) ;
#108775 = CARTESIAN_POINT ( 'NONE',  ( 4.893472065931465664, 1.353474861756031267, 1.225258530246610134 ) ) ;
#108776 = CARTESIAN_POINT ( 'NONE',  ( 8.847373858153110504, 13.14833187437462314, 7.638329839124071263 ) ) ;
#108777 = CARTESIAN_POINT ( 'NONE',  ( 1.176956626245349247, -0.04423564266526488348, -1.971012800895243888 ) ) ;
#108778 = CARTESIAN_POINT ( 'NONE',  ( 3.797043250571481732, -0.1924442655423033721, -1.902711443722324258 ) ) ;
#108779 = EDGE_LOOP ( 'NONE', ( #201227, #74341, #109012, #32693 ) ) ;
#108780 = CARTESIAN_POINT ( 'NONE',  ( 0.3999999999999792610, 4.000000000000008882, 0.8338124244295505028 ) ) ;
#108781 = CARTESIAN_POINT ( 'NONE',  ( 4.721133488271325618, -1.758435714881977141, -0.8873337903104687729 ) ) ;
#108782 = EDGE_LOOP ( 'NONE', ( #20239, #59165, #208835, #34637 ) ) ;
#108783 = CARTESIAN_POINT ( 'NONE',  ( 5.935097076209718381, -1.409686562828060152, -1.336055723097711256 ) ) ;
#108784 = ORIENTED_EDGE ( 'NONE', *, *, #121638, .T. ) ;
#108785 = CARTESIAN_POINT ( 'NONE',  ( -5.581116510680924847, 6.540332679663050541, -1.199719254218453823 ) ) ;
#108787 = CARTESIAN_POINT ( 'NONE',  ( 6.240501835383900797, 1.219778281852833546, -1.734492557903525523 ) ) ;
#108786 = CARTESIAN_POINT ( 'NONE',  ( -4.960304097753355457, 6.880383762169266504, 1.599625672291263179 ) ) ;
#108788 = CARTESIAN_POINT ( 'NONE',  ( 6.007671464186812749, 10.02305078494439883, 0.7216878364870317197 ) ) ;
#108790 = VERTEX_POINT ( 'NONE', #194651 ) ;
#108789 = CARTESIAN_POINT ( 'NONE',  ( 3.440010667329951310, -1.141173813254949820, -1.534285795567114974 ) ) ;
#108791 = CARTESIAN_POINT ( 'NONE',  ( -4.379728263269426769, 15.51893462896019038, -11.18122698975924223 ) ) ;
#108792 = CARTESIAN_POINT ( 'NONE',  ( 0.07755575628183573877, -0.002876890934064984216, -2.188974970840869005 ) ) ;
#108793 = CARTESIAN_POINT ( 'NONE',  ( 9.649767104172513044, 4.268299563709507360, -7.133807922836931326 ) ) ;
#108794 = CARTESIAN_POINT ( 'NONE',  ( 5.180342516426402533, 0.9943292982247069478, 1.750330089345548679 ) ) ;
#108795 = CYLINDRICAL_SURFACE ( 'NONE', #93019, 1.500000000000000222 ) ;
#108796 = CARTESIAN_POINT ( 'NONE',  ( 5.795480788678070816, 1.385457615097264394, 1.189071861804301466 ) ) ;
#108797 = CARTESIAN_POINT ( 'NONE',  ( 1.609917502266303480, 0.6029389078928657497, -1.980602105166151095 ) ) ;
#108798 = CARTESIAN_POINT ( 'NONE',  ( -7.063961727919978451, 8.200042423116789436, 1.199719254218450271 ) ) ;
#108799 =( BOUNDED_SURFACE ( )  B_SPLINE_SURFACE ( 3, 3, ( 
 ( #197022, #126784, #193815, #10792, #208986, #192740, #186891, #139232, #56904, #170647 ),
 ( #22233, #154409, #180773, #101383, #103525, #19053, #203128, #88345, #54771, #3847 ),
 ( #205263, #35306, #120918, #55835, #38523, #85132, #121991, #118762, #36374, #151219 ),
 ( #68859, #20117, #136031, #153338, #5988, #204179, #187957, #200988, #171715, #184747 ),
 ( #23314, #169584, #21167, #52634, #155472, #102452, #168518, #86202, #202044, #72884 ),
 ( #25209, #91313, #193041, #157370, #8964, #43629, #141154, #124941, #77162, #190903 ),
 ( #138991, #205012, #42567, #44695, #176807, #188781, #109744, #108670, #27346, #28423 ) ),
 .UNSPECIFIED., .T., .F., .T. ) 
 B_SPLINE_SURFACE_WITH_KNOTS ( ( 4, 3, 4 ),
 ( 4, 1, 1, 1, 1, 1, 1, 4 ),
 ( 0.000000000000000000, 0.5000000000000000000, 1.000000000000000000 ),
 ( 0.000000000000000000, 0.09705918685507786137, 0.1907419858981972138, 0.2602182418918835838, 0.3625179829595637226, 0.5215049497019805802, 0.7338397267804015467, 1.000000000000000000 ),
 .UNSPECIFIED. ) 
 GEOMETRIC_REPRESENTATION_ITEM ( )  RATIONAL_B_SPLINE_SURFACE ( (
 ( 1.000000000000000000, 1.000000000000000000, 1.000000000000000000, 1.000000000000000222, 1.000000000000000222, 0.9999999999999994449, 1.000000000000000444, 0.9999999999999997780, 1.000000000000000000, 1.000000000000000000),
 ( 0.3333333333333333703, 0.3333333333333333703, 0.3333333333333333703, 0.3333333333333334259, 0.3333333333333333703, 0.3333333333333332038, 0.3333333333333335369, 0.3333333333333332038, 0.3333333333333333703, 0.3333333333333333703),
 ( 0.3333333333333333703, 0.3333333333333333703, 0.3333333333333333703, 0.3333333333333334259, 0.3333333333333333703, 0.3333333333333332038, 0.3333333333333335369, 0.3333333333333332038, 0.3333333333333333703, 0.3333333333333333703),
 ( 1.000000000000000000, 1.000000000000000000, 1.000000000000000000, 1.000000000000000222, 1.000000000000000222, 0.9999999999999994449, 1.000000000000000444, 0.9999999999999997780, 1.000000000000000000, 1.000000000000000000),
 ( 0.3333333333333333703, 0.3333333333333333703, 0.3333333333333333703, 0.3333333333333334259, 0.3333333333333333703, 0.3333333333333332038, 0.3333333333333335369, 0.3333333333333332038, 0.3333333333333333703, 0.3333333333333333703),
 ( 0.3333333333333333703, 0.3333333333333333703, 0.3333333333333333703, 0.3333333333333334259, 0.3333333333333333703, 0.3333333333333332038, 0.3333333333333335369, 0.3333333333333332038, 0.3333333333333333703, 0.3333333333333333703),
 ( 1.000000000000000000, 1.000000000000000000, 1.000000000000000000, 1.000000000000000222, 1.000000000000000222, 0.9999999999999994449, 1.000000000000000444, 0.9999999999999997780, 1.000000000000000000, 1.000000000000000000) ) ) 
 REPRESENTATION_ITEM ( '' )  SURFACE ( )  );
#108800 = CARTESIAN_POINT ( 'NONE',  ( -6.152945810502786550, 6.988564382810744213, -0.9301526061148736035 ) ) ;
#108801 = CARTESIAN_POINT ( 'NONE',  ( 0.3282377607281153908, 1.926335450315390885, -1.225000000000010525 ) ) ;
#108802 = CARTESIAN_POINT ( 'NONE',  ( -1.642778471875000035, -2.617708332855375186, -2.845375778867859751 ) ) ;
#108803 = CARTESIAN_POINT ( 'NONE',  ( 5.449487677688982679, 8.445153826357429949, -1.199719254218446718 ) ) ;
#108804 = B_SPLINE_CURVE_WITH_KNOTS ( 'NONE', 3,
 ( #134349, #200352, #114929, #199289, #35734, #184113, #119187, #101809, #4273, #50934, #183055 ),
 .UNSPECIFIED., .F., .F.,
 ( 4, 1, 1, 1, 1, 1, 1, 1, 4 ),
 ( 0.000000000000000000, 0.2254494161556361009, 0.3971188491599597081, 0.5240836380151728813, 0.6154273167216615104, 0.6803253696226415626, 0.7282602231486813293, 0.7688932809586735972, 1.000000000000000000 ),
 .UNSPECIFIED. ) ;
#108805 = CARTESIAN_POINT ( 'NONE',  ( 4.421367491832270957, 6.251624388594711590, 1.443375672974058777 ) ) ;
#108806 = ADVANCED_FACE ( 'NONE', ( #111345 ), #59298, .F. ) ;
#108807 = CARTESIAN_POINT ( 'NONE',  ( 4.227444969362701421, 3.826440640544909400, 1.214306433183764966E-14 ) ) ;
#108808 = CARTESIAN_POINT ( 'NONE',  ( -1.364683531250014514, 11.65104166700806587, -0.7879004041258335089 ) ) ;
#108810 = CARTESIAN_POINT ( 'NONE',  ( -6.526270840131767059, 8.707344961610770540, -1.599625672291271394 ) ) ;
#108809 = CARTESIAN_POINT ( 'NONE',  ( 6.925078400183553029, 0.5781763343528348864, 2.007479843201316783 ) ) ;
#108811 = CARTESIAN_POINT ( 'NONE',  ( 4.377415392590312315, -0.3859441149459389431, -1.690453949067998840 ) ) ;
#108812 = CLOSED_SHELL ( 'NONE', ( #195089, #116761, #41587, #102962, #28510, #128210, #159385, #17251 ) ) ;
#108813 = CARTESIAN_POINT ( 'NONE',  ( -4.874319919312905647, 5.645460313075203018, -1.199719254218446718 ) ) ;
#108814 = CARTESIAN_POINT ( 'NONE',  ( 2.237250781069185734, -0.09733102107959036575, -2.068066387140480522 ) ) ;
#108815 = CARTESIAN_POINT ( 'NONE',  ( 3.445011857661818944, -1.868279436719679110, -0.9960484452814029055 ) ) ;
#108816 = CARTESIAN_POINT ( 'NONE',  ( 7.938462636001388795, 9.220293482545153907, -1.199719254218441611 ) ) ;
#108817 = CARTESIAN_POINT ( 'NONE',  ( -1.201851678989727383E-14, 3.946875000341423689, -1.575800808251660134 ) ) ;
#108818 = CARTESIAN_POINT ( 'NONE',  ( 1.815228950277411712, -1.686530385472130744, -1.016810816036699316 ) ) ;
#108819 = CARTESIAN_POINT ( 'NONE',  ( 5.951559787436734084, 6.118878616701469042, 0.7174803059855124898 ) ) ;
#108821 = DIRECTION ( 'NONE',  ( -0.000000000000000000, -1.000000000000000000, -0.000000000000000000 ) ) ;
#108820 = CARTESIAN_POINT ( 'NONE',  ( -3.475000000000000533, -2.479166666666667851, -2.006292185433948827 ) ) ;
#108822 = CARTESIAN_POINT ( 'NONE',  ( 3.732637569912560682, 0.3354268113090127512, 2.267480163388153169 ) ) ;
#108823 = CARTESIAN_POINT ( 'NONE',  ( 2.051128252772801641, -1.465761996925790900, -1.088229512710245261 ) ) ;
#108824 = CARTESIAN_POINT ( 'NONE',  ( 4.993145711582793744, 9.047363440147082159, -0.7998128361456481317 ) ) ;
#108825 = CARTESIAN_POINT ( 'NONE',  ( 7.415946836550727284, 7.754285518838408109, 0.7216878364870317197 ) ) ;
#108826 = CARTESIAN_POINT ( 'NONE',  ( -6.496328159242330536, 10.73079995242472862, 0.000000000000000000 ) ) ;
#108827 = CARTESIAN_POINT ( 'NONE',  ( 2.566654749391559687, 0.6821283815301434350, 1.894225559998161668 ) ) ;
#108828 = CARTESIAN_POINT ( 'NONE',  ( 2.623818369222921554, 1.924856029493416276, -0.3778354045670463401 ) ) ;
#108829 = CARTESIAN_POINT ( 'NONE',  ( -9.508345801885592863, 9.987491611821676329, 0.7998128361456462443 ) ) ;
#108830 = CARTESIAN_POINT ( 'NONE',  ( -5.201524489137236529, 9.220195670635433771, 0.7998128361456481317 ) ) ;
#108831 = CARTESIAN_POINT ( 'NONE',  ( 0.07536363704233049743, 0.2309889609098912111, -2.177957698420322163 ) ) ;
#108833 = CARTESIAN_POINT ( 'NONE',  ( 3.098275772329066591, -0.5124342443764763333, -1.694037474313156988 ) ) ;
#108832 = CARTESIAN_POINT ( 'NONE',  ( 5.525362607580523111, -1.325732906064909677, -1.616523167544873241 ) ) ;
#108834 = CARTESIAN_POINT ( 'NONE',  ( -6.671583288098545061, 16.00000000000403588, 9.747470831330232954 ) ) ;
#108835 = CARTESIAN_POINT ( 'NONE',  ( 6.667932745306283771, -1.416340830354723135, 1.803254352984103859 ) ) ;
#108836 = CARTESIAN_POINT ( 'NONE',  ( 6.070193552946823168, -1.654735283430305515, -0.5392940629580407208 ) ) ;
#108837 = CARTESIAN_POINT ( 'NONE',  ( 9.101601193475611140, 9.512956235343358102, -0.7998128361456221525 ) ) ;
#108838 = CARTESIAN_POINT ( 'NONE',  ( 6.504485943970635731, -2.231000991611901352, 0.5533298437200293574 ) ) ;
#108839 = CARTESIAN_POINT ( 'NONE',  ( 0.1333692844072585093, 7.629137130509075604, -2.653547345224527287 ) ) ;
#108840 = CARTESIAN_POINT ( 'NONE',  ( 5.325445489366991580, -1.254443461812755789, 1.197174301038748334 ) ) ;
#108841 = CARTESIAN_POINT ( 'NONE',  ( 5.477072320546296780, 2.003985016195033886, 0.8359633449262526828 ) ) ;
#108842 = DIRECTION ( 'NONE',  ( 0.6507913734559712671, -0.7592566023652943530, 0.000000000000000000 ) ) ;
#108843 = CARTESIAN_POINT ( 'NONE',  ( -0.2408018239684434625, -0.007136184528846663787, -2.100252307185761058 ) ) ;
#108844 = CARTESIAN_POINT ( 'NONE',  ( 5.718750000000003553, -0.7852924748296825630, 1.895863743164203141 ) ) ;
#108845 = CARTESIAN_POINT ( 'NONE',  ( 11.07124251632621537, 9.800000000000000711, -0.8054525327832628978 ) ) ;
#108846 = CARTESIAN_POINT ( 'NONE',  ( 3.873980538081963854, 1.069312750484844088, 1.602167800089354222 ) ) ;
#108847 = CARTESIAN_POINT ( 'NONE',  ( -0.7500000000000006661, 11.23958333401613174, -1.299038105676657340 ) ) ;
#108848 = CARTESIAN_POINT ( 'NONE',  ( 6.275645185405086757, 0.3810096023663198661, -2.188332947720336819 ) ) ;
#108849 = ORIENTED_EDGE ( 'NONE', *, *, #156185, .T. ) ;
#108850 = CARTESIAN_POINT ( 'NONE',  ( 1.499999999999989120, 5.045833333333354709, -0.8660254037844323793 ) ) ;
#108851 = CARTESIAN_POINT ( 'NONE',  ( 3.798255590122797898, 7.583048621785260401, -0.7998128361456221525 ) ) ;
#108852 = CARTESIAN_POINT ( 'NONE',  ( 5.282873410819217241, 9.315102745931094219, -0.7998128361456281477 ) ) ;
#108853 = CARTESIAN_POINT ( 'NONE',  ( 2.139591745018020408, 0.003451857093505344976, 2.221473417793240923 ) ) ;
#108854 = SURFACE_STYLE_FILL_AREA ( #191082 ) ;
#108855 = CARTESIAN_POINT ( 'NONE',  ( 5.165293337126522388, 8.969999960048859577, 1.040834085586084257E-14 ) ) ;
#108856 = CARTESIAN_POINT ( 'NONE',  ( -7.795575137733361970, 12.03866206075687018, 0.7216878364870458196 ) ) ;
#108857 = CIRCLE ( 'NONE', #122813, 9.499999999999992895 ) ;
#108858 = CARTESIAN_POINT ( 'NONE',  ( 7.702440666339465558, 8.158804663583751449, -0.7216878364870317197 ) ) ;
#108859 = CARTESIAN_POINT ( 'NONE',  ( 0.2818752512256904597, 1.674885806461807958, -1.122501178855893400 ) ) ;
#108861 = CARTESIAN_POINT ( 'NONE',  ( 5.846154128119951388, -0.9308047640707247661, 1.840808156992862932 ) ) ;
#108860 = CARTESIAN_POINT ( 'NONE',  ( 9.752392566931574081, 10.27221283770866300, -0.7998128361456281477 ) ) ;
#108862 = SURFACE_SIDE_STYLE ('',( #157562 ) ) ;
#108863 = CARTESIAN_POINT ( 'NONE',  ( -3.898132859128961236, 4.506575409527250997, -1.199719254218452047 ) ) ;
#108864 = CARTESIAN_POINT ( 'NONE',  ( 5.343321937117211817, 9.247976336696488886, 0.000000000000000000 ) ) ;
#108865 = CIRCLE ( 'NONE', #205574, 0.08000000000000008493 ) ;
#108866 =( LENGTH_UNIT ( ) NAMED_UNIT ( * ) SI_UNIT ( .MILLI., .METRE. ) );
#108867 = CARTESIAN_POINT ( 'NONE',  ( 0.6823417656249882723, 1.176041667008083325, -1.181850606188749264 ) ) ;
#108869 = B_SPLINE_CURVE_WITH_KNOTS ( 'NONE', 3,
 ( #64834, #114725, #111530, #78946, #177536, #96301, #46472 ),
 .UNSPECIFIED., .F., .F.,
 ( 4, 3, 4 ),
 ( 3.315837474970778393E-05, 0.0009000000035470269054, 0.001929259801299067038 ),
 .UNSPECIFIED. ) ;
#108868 = CARTESIAN_POINT ( 'NONE',  ( 0.9832602892492541269, 1.182927327958797070, 1.316506037215345426 ) ) ;
#108870 = CARTESIAN_POINT ( 'NONE',  ( 0.1939827082095749167, 1.755770691208278889, 0.9913967135185000057 ) ) ;
#108871 = CARTESIAN_POINT ( 'NONE',  ( 6.128409194715155550, 0.1798751216713200540, 1.731140798666473968 ) ) ;
#108872 = CARTESIAN_POINT ( 'NONE',  ( 3.632637656275085281, 0.3374270351050281946, 2.267304333945507011 ) ) ;
#108873 = CARTESIAN_POINT ( 'NONE',  ( -1.402160292154681736E-14, 0.07187500034142156602, 1.575800808251672791 ) ) ;
#108874 = CARTESIAN_POINT ( 'NONE',  ( 2.571990918753517708, -1.761868631437716548, -0.5344257538507578564 ) ) ;
#108875 = CARTESIAN_POINT ( 'NONE',  ( 10.40996301719436090, 11.03937836301526687, 0.000000000000000000 ) ) ;
#108876 = CARTESIAN_POINT ( 'NONE',  ( 11.99904264826913725, 7.001436028495777286, 0.9608145573154694974 ) ) ;
#108877 = CARTESIAN_POINT ( 'NONE',  ( 2.889462524698828361, 1.289687736819044472, 1.292329967842877014 ) ) ;
#108878 = CARTESIAN_POINT ( 'NONE',  ( 3.797500137148449362, 1.423962148579031917, -1.427936706820939872 ) ) ;
#108879 = CARTESIAN_POINT ( 'NONE',  ( -9.236128959407555072, 11.79856975744075598, -1.599625672291263179 ) ) ;
#108881 = DIRECTION ( 'NONE',  ( -0.000000000000000000, -1.000000000000000000, -0.000000000000000000 ) ) ;
#108880 = CARTESIAN_POINT ( 'NONE',  ( 2.694485044408474916, -2.256396476877442492, -0.1672753843019215703 ) ) ;
#108882 = CARTESIAN_POINT ( 'NONE',  ( 5.491282870796595716, 1.858858430755592428, -0.9897807336930256605 ) ) ;
#108883 = CARTESIAN_POINT ( 'NONE',  ( -11.92619526913699879, 13.40000000000000036, -1.328859060402686199 ) ) ;
#108884 = CIRCLE ( 'NONE', #63817, 2.011244508837062295 ) ;
#108885 = CARTESIAN_POINT ( 'NONE',  ( 2.594261239525695206, 0.9781076984213372683, -1.824767828009652426 ) ) ;
#108886 = CARTESIAN_POINT ( 'NONE',  ( 4.059776932288224671, 6.823824623389866950, 1.199719254218462483 ) ) ;
#108887 = CARTESIAN_POINT ( 'NONE',  ( 0.6801582343750056658, 0.5885416670080856338, -1.178068619123862515 ) ) ;
#108888 = CARTESIAN_POINT ( 'NONE',  ( 4.196021508500130004, 1.385991406618786836, 1.604897850144955340 ) ) ;
#108889 = ITEM_DEFINED_TRANSFORMATION ( 'NONE', 'NONE', #173239,  #200407 ) ;
#108890 = CARTESIAN_POINT ( 'NONE',  ( 1.031717895469780988, -1.221320771479022627, -1.489887157414800267 ) ) ;
#108891 = CARTESIAN_POINT ( 'NONE',  ( -5.330290668828105538, 6.247702530834755130, 1.199719254218452935 ) ) ;
#108892 = CARTESIAN_POINT ( 'NONE',  ( 9.108380270282433244, 9.520865158284665952, 1.040834085586084257E-14 ) ) ;
#108893 = CARTESIAN_POINT ( 'NONE',  ( 5.682275777458851707, 6.762314840857718501, 1.082531754730549078 ) ) ;
#108894 = CARTESIAN_POINT ( 'NONE',  ( 0.2466033008277778715, 2.800000000000024691, -1.444539947226808341 ) ) ;
#108895 = CARTESIAN_POINT ( 'NONE',  ( -3.744022975668147790, 7.519777238254810925, -0.7998128361456281477 ) ) ;
#108896 = CARTESIAN_POINT ( 'NONE',  ( 5.818629517237746462, -0.7649446623404360102, -1.977987144599784086 ) ) ;
#108897 = CARTESIAN_POINT ( 'NONE',  ( 1.676933785844336944, -1.999498008410249383, -0.6612845060171600453 ) ) ;
#108898 = CARTESIAN_POINT ( 'NONE',  ( -4.685224601974262271, 7.623789914682047808, -1.199719254218453823 ) ) ;
#108899 = CARTESIAN_POINT ( 'NONE',  ( 8.263858322729371153, 9.599921783727809910, -1.199719254218446718 ) ) ;
#108900 = CARTESIAN_POINT ( 'NONE',  ( 6.244940914744545601, -0.2718465296328761438, -1.840820509183779263 ) ) ;
#108901 = CARTESIAN_POINT ( 'NONE',  ( 6.076025397218672630, 10.24044673006381245, -0.7998128361456291469 ) ) ;
#108902 = FILL_AREA_STYLE ('',( #75266 ) ) ;
#108903 = CARTESIAN_POINT ( 'NONE',  ( -3.984117037569407938, 5.741498858621315371, 1.599625672291270506 ) ) ;
#108904 = CARTESIAN_POINT ( 'NONE',  ( -8.432808358020034589, 10.86136238915529084, 1.443375672974064550 ) ) ;
#108905 = CARTESIAN_POINT ( 'NONE',  ( -3.853720295264455586, 8.531188044730782849, 2.447541241191873773 ) ) ;
#108906 = SURFACE_SIDE_STYLE ('',( #41728 ) ) ;
#108908 = CARTESIAN_POINT ( 'NONE',  ( 3.508209890309890167, 1.962046631884439174, 0.002529298861464468473 ) ) ;
#108907 = CARTESIAN_POINT ( 'NONE',  ( 1.224999999999996980, -0.3750000000000211497, -2.428612866367529932E-14 ) ) ;
#108909 = CARTESIAN_POINT ( 'NONE',  ( 0.5148121308554790554, 1.489681748880047563, -1.566682057046255849 ) ) ;
#108910 = AXIS2_PLACEMENT_3D ( 'NONE', #119979, #152410, #202188 ) ;
#108912 = CARTESIAN_POINT ( 'NONE',  ( -6.070455375431035527, 6.038045056918933895, -0.4763334965118305453 ) ) ;
#108911 = CARTESIAN_POINT ( 'NONE',  ( -4.502189528189771472, 7.410248995266807803, -1.199719254218453823 ) ) ;
#108913 = CARTESIAN_POINT ( 'NONE',  ( -0.6823417656250003738, 1.467708333674752730, -1.181850606188749264 ) ) ;
#108914 = CARTESIAN_POINT ( 'NONE',  ( 2.607021377293942344, -1.721407032317923802, 0.2550150930856145970 ) ) ;
#108915 = CARTESIAN_POINT ( 'NONE',  ( 5.938108093105483931, 8.911247961056314892, -1.082531754730537088 ) ) ;
#108916 = CARTESIAN_POINT ( 'NONE',  ( -11.50790213655337979, 7.746734403679841563, -4.957264960544601529 ) ) ;
#108917 = CARTESIAN_POINT ( 'NONE',  ( 1.809922493048341297, -1.704678386728165185, 1.076150803433255865 ) ) ;
#108918 = CARTESIAN_POINT ( 'NONE',  ( 6.825078400183511640, 3.679815135839346496, 2.758192972206894744 ) ) ;
#108919 = CARTESIAN_POINT ( 'NONE',  ( -4.767627293860968507, 5.591261926706423857, -1.199719254218453823 ) ) ;
#108920 = CARTESIAN_POINT ( 'NONE',  ( 2.131653300961271924, -1.286245803994587877, -1.494167145092902160 ) ) ;
#108921 = AXIS2_PLACEMENT_3D ( 'NONE', #14226, #112897, #196215 ) ;
#108923 = CARTESIAN_POINT ( 'NONE',  ( -6.482206841109545259, 6.735198534148810090, 0.7216878364870257245 ) ) ;
#108922 = CARTESIAN_POINT ( 'NONE',  ( 5.590081826628392925, 1.144292256163012667, 1.532101299821154949 ) ) ;
#108924 = CARTESIAN_POINT ( 'NONE',  ( -5.817857313595549584, 6.920493299683823096, 1.082531754730549078 ) ) ;
#108925 = CARTESIAN_POINT ( 'NONE',  ( 4.850785098639300408, 8.881276058379668825, -0.7998128361456481317 ) ) ;
#108926 = STYLED_ITEM ( 'NONE', ( #205368 ), #156054 ) ;
#108927 = CARTESIAN_POINT ( 'NONE',  ( -4.620296487206990932, 8.612372678375294299, 0.000000000000000000 ) ) ;
#108928 = CARTESIAN_POINT ( 'NONE',  ( 0.9791725360285336022, -1.826886329348556881, -0.8614179918085950183 ) ) ;
#108929 = LINE ( 'NONE', #63308, #4102 ) ;
#108930 = CARTESIAN_POINT ( 'NONE',  ( 5.649573025266686699, -1.814708426832438048, -1.425321367006604056 ) ) ;
#108931 = CARTESIAN_POINT ( 'NONE',  ( 6.777797683793751915, -1.903277019102869616, 0.4755351429900215310 ) ) ;
#108932 = CARTESIAN_POINT ( 'NONE',  ( 2.729291793292155432, 0.1011638768560127188, -1.959297240552673181 ) ) ;
#108933 = CARTESIAN_POINT ( 'NONE',  ( 9.206149998879153529, 10.69926207256923689, 1.199719254218453823 ) ) ;
#108934 = CARTESIAN_POINT ( 'NONE',  ( 0.1588275700346117869, 1.163271727376416376, 1.646837250247008777 ) ) ;
#108935 = ORIENTED_EDGE ( 'NONE', *, *, #30501, .F. ) ;
#108936 = CARTESIAN_POINT ( 'NONE',  ( 0.7786901736592425349, -0.5205582433389954744, -2.052224243718490992 ) ) ;
#108938 = CARTESIAN_POINT ( 'NONE',  ( -7.393273838153706201, 7.519907654134449615, 0.7998128361456341429 ) ) ;
#108937 = CARTESIAN_POINT ( 'NONE',  ( -3.164938793786285842, 5.779846795137578930, -1.199719254218452935 ) ) ;
#108939 = CARTESIAN_POINT ( 'NONE',  ( 1.904012794591736668, 1.364881752761820222, -1.235849761865935870 ) ) ;
#108940 = ORIENTED_EDGE ( 'NONE', *, *, #137329, .F. ) ;
#108941 = CARTESIAN_POINT ( 'NONE',  ( 10.85609235738973588, 9.597193135844154455, 5.125747691056198541 ) ) ;
#108943 = EDGE_CURVE ( 'NONE', #210699, #81951, #140953, .T. ) ;
#108942 = CARTESIAN_POINT ( 'NONE',  ( 3.129257641292593650, 1.918792544363761454, 0.9031103230835100248 ) ) ;
#108944 = CARTESIAN_POINT ( 'NONE',  ( 1.499999999999989120, 4.827083334016149863, -0.8660254037844323793 ) ) ;
#108945 = CARTESIAN_POINT ( 'NONE',  ( 7.832860060393120882, 10.16142270859057462, 1.599625672291281386 ) ) ;
#108946 = CARTESIAN_POINT ( 'NONE',  ( 5.854088466050551887, 10.05179665369283981, 0.7998128361456341429 ) ) ;
#108947 = CARTESIAN_POINT ( 'NONE',  ( 3.919256602636957076, -0.1552153454438681413, 2.055015938418188526 ) ) ;
#108949 = CARTESIAN_POINT ( 'NONE',  ( 1.417261839328866513, -1.023339270300478221, -1.530466495063505628 ) ) ;
#108948 = CARTESIAN_POINT ( 'NONE',  ( -7.609150525767646833, 9.900428251527500834, -1.599625672291263179 ) ) ;
#108950 = CARTESIAN_POINT ( 'NONE',  ( -1.364683531249997417, 5.009375000341425022, 1.214306433183764966E-14 ) ) ;
#108951 = DIRECTION ( 'NONE',  ( 0.000000000000000000, 0.000000000000000000, -1.000000000000000000 ) ) ;
#108952 = CARTESIAN_POINT ( 'NONE',  ( -1.499999999998127498, 8.654187183607668032, 2.562246142702330864 ) ) ;
#108953 = CARTESIAN_POINT ( 'NONE',  ( 2.885543303398817372, 6.439774126353135841, -0.3727371597862367270 ) ) ;
#108954 = CARTESIAN_POINT ( 'NONE',  ( 1.577102763248950046, -2.096353118739826993, -0.6898709473643764856 ) ) ;
#108955 = CARTESIAN_POINT ( 'NONE',  ( 2.355063576532693936, -1.750152493129919717, 1.433722681173225100 ) ) ;
#108956 = CARTESIAN_POINT ( 'NONE',  ( -7.185458225562757484, 11.32685899655781903, 0.7216878364870458196 ) ) ;
#108957 = CARTESIAN_POINT ( 'NONE',  ( 1.968756957844201239, -1.398423508019512651, 1.151565528817798834 ) ) ;
#108958 = CARTESIAN_POINT ( 'NONE',  ( 2.553800400642152635, 1.028702656226655465, 1.615903109786074099 ) ) ;
#108959 = CARTESIAN_POINT ( 'NONE',  ( 4.580570967453869713, 1.276285970795057345, -1.630082184409971324 ) ) ;
#108960 = CARTESIAN_POINT ( 'NONE',  ( -1.201851678989727383E-14, 3.009375000341419248, -1.575800808251660134 ) ) ;
#108961 = CARTESIAN_POINT ( 'NONE',  ( 2.975414797803474176, 1.872564425654202225, -0.6168198417838985925 ) ) ;
#108962 = CARTESIAN_POINT ( 'NONE',  ( 6.516243422921982109, -0.9108434941001318785, -1.697579817862464147 ) ) ;
#108963 = CARTESIAN_POINT ( 'NONE',  ( 4.451927283622527654, 1.870250842541102410, -0.04591718433973044494 ) ) ;
#108965 = CARTESIAN_POINT ( 'NONE',  ( 5.273189713885392926, 7.658326211947664497, -1.220946906274408494 ) ) ;
#108964 = CARTESIAN_POINT ( 'NONE',  ( 1.805729983942544026, 1.920404770136320716, 1.279379207282659969 ) ) ;
#108966 = CARTESIAN_POINT ( 'NONE',  ( 3.701460696238024539, -1.407827198975480032, -1.217257945129922803 ) ) ;
#108967 = CARTESIAN_POINT ( 'NONE',  ( -1.001543065824772872E-14, 4.571875000341418804, 1.575800808251672791 ) ) ;
#108968 = CIRCLE ( 'NONE', #181551, 5.500000000000005329 ) ;
#108969 = CARTESIAN_POINT ( 'NONE',  ( -3.574546055497324737, 7.322054164722185732, 0.7998128361456341429 ) ) ;
#108970 = CARTESIAN_POINT ( 'NONE',  ( 5.099838337034727331, 9.101561826515851550, -0.7998128361456281477 ) ) ;
#108971 = CARTESIAN_POINT ( 'NONE',  ( 11.06389876992412091, 3.829536045110819575, -3.713591040152774081 ) ) ;
#108972 = EDGE_CURVE ( 'NONE', #19630, #97972, #150289, .T. ) ;
#108973 = CARTESIAN_POINT ( 'NONE',  ( 0.5398470734442856189, -1.490880511344143011, -1.487817205855391789 ) ) ;
#108974 = CARTESIAN_POINT ( 'NONE',  ( 1.364683531249990311, 4.196875000341417028, 1.214306433183764966E-14 ) ) ;
#108975 = CARTESIAN_POINT ( 'NONE',  ( 5.905597126736788383, -0.5315564325061740147, 2.095088507090197893 ) ) ;
#108976 = CARTESIAN_POINT ( 'NONE',  ( 2.514065211524143084, -0.6609878990531635745, 2.015050547854141172 ) ) ;
#108977 = CARTESIAN_POINT ( 'NONE',  ( 6.217445935018812264, 1.680332259792745475, 1.120195391490413472 ) ) ;
#108978 = CARTESIAN_POINT ( 'NONE',  ( -1.364683531250014514, -0.01145833299191483488, -0.7879004041258359514 ) ) ;
#108979 = CARTESIAN_POINT ( 'NONE',  ( -5.111060722671894929, 5.065251719313053513, 0.000000000000000000 ) ) ;
#108980 = CARTESIAN_POINT ( 'NONE',  ( 1.265152180075890254, -1.953616520262021039, -0.9254636565915741464 ) ) ;
#108983 = CARTESIAN_POINT ( 'NONE',  ( 2.711267533052988732, 6.106969855296372707, -0.7216878364870267237 ) ) ;
#108982 = CARTESIAN_POINT ( 'NONE',  ( 6.825078400183573812, 7.629137130509070275, 2.455651831298297338 ) ) ;
#108981 = CARTESIAN_POINT ( 'NONE',  ( 5.851225812749518695, 8.984124660586543243, -1.199719254218452047 ) ) ;
#108984 = CARTESIAN_POINT ( 'NONE',  ( -3.332271893908731464, 7.109677319527304640, -0.7998128361456481317 ) ) ;
#108985 = CARTESIAN_POINT ( 'NONE',  ( 5.278529876733943915, -0.4946281652532491524, -1.954780475499573900 ) ) ;
#108987 = CARTESIAN_POINT ( 'NONE',  ( -6.251718229232856139, 8.387033582228697881, -1.443375672974066548 ) ) ;
#108986 = CARTESIAN_POINT ( 'NONE',  ( -7.673551755654729689, 11.89630144833179060, 0.7216878364870458196 ) ) ;
#108988 = CARTESIAN_POINT ( 'NONE',  ( 4.934241560730721510, 4.721313007132757811, 0.000000000000000000 ) ) ;
#108990 = CARTESIAN_POINT ( 'NONE',  ( -1.364683531250010740, 10.88020833367473372, 0.7879004041258445001 ) ) ;
#108989 = CARTESIAN_POINT ( 'NONE',  ( 6.350466702034289312, 0.6732396885240909956, 2.054270918568662729 ) ) ;
#108991 = FACE_OUTER_BOUND ( 'NONE', #78809, .T. ) ;
#108992 = TOROIDAL_SURFACE ( 'NONE', #157335, 9.580000000000001847, 0.08000000000000000167 ) ;
#108994 = CARTESIAN_POINT ( 'NONE',  ( 6.222279831957801655, 1.994873610751910942, 0.2930524845206964879 ) ) ;
#108993 = CARTESIAN_POINT ( 'NONE',  ( -5.219525951136845698, 8.072902128759544382, -1.082531754730543971 ) ) ;
#108995 = CARTESIAN_POINT ( 'NONE',  ( -0.6823417656250212460, 1.113541667008083325, 1.181850606188755259 ) ) ;
#108996 = CARTESIAN_POINT ( 'NONE',  ( 6.883263157960358924, 7.052235917045241997, 2.651962373728885325 ) ) ;
#108997 = SPHERICAL_SURFACE ( 'NONE', #100154, 0.05000000000000000278 ) ;
#108998 = CARTESIAN_POINT ( 'NONE',  ( 2.771755371404661439, 0.9226176164769549493, 1.457180633135872094 ) ) ;
#108999 = CARTESIAN_POINT ( 'NONE',  ( 7.991605200612358573, 8.288237253661408843, 0.7998128361456281477 ) ) ;
#109000 = CARTESIAN_POINT ( 'NONE',  ( 6.378184920586140727, 6.405913593630768510, 0.000000000000000000 ) ) ;
#109001 = CARTESIAN_POINT ( 'NONE',  ( 1.364683531249986537, -0.5739583329919174526, 0.7879004041258500513 ) ) ;
#109002 = CARTESIAN_POINT ( 'NONE',  ( 1.123854678948147834, 1.060202766368176786, -1.416847970540972668 ) ) ;
#109003 = CARTESIAN_POINT ( 'NONE',  ( 2.473293533796361299, -1.752518403998115426, -0.9904139345979168230 ) ) ;
#109004 = SURFACE_SIDE_STYLE ('',( #106857 ) ) ;
#109005 = CARTESIAN_POINT ( 'NONE',  ( 4.155453238874762256, -1.833011353516471154, -1.228491751752130545 ) ) ;
#109006 = VERTEX_POINT ( 'NONE', #95047 ) ;
#109007 = CARTESIAN_POINT ( 'NONE',  ( 1.499999999999987121, -0.7458333333333122539, 0.8660254037844524744 ) ) ;
#109008 = CARTESIAN_POINT ( 'NONE',  ( 9.381879110532285182, 10.04787317181692075, 0.000000000000000000 ) ) ;
#109010 = CARTESIAN_POINT ( 'NONE',  ( 2.407827563459669307, -1.163288551851604513, -1.646826728940099738 ) ) ;
#109009 = CARTESIAN_POINT ( 'NONE',  ( 2.877707679121459083, 0.3088738507561124558, -2.097740099398600400 ) ) ;
#109012 = ORIENTED_EDGE ( 'NONE', *, *, #37586, .T. ) ;
#109011 = CARTESIAN_POINT ( 'NONE',  ( 3.814574336081223649, -0.5739048956562255999, -1.718320587032542202 ) ) ;
#109013 = CARTESIAN_POINT ( 'NONE',  ( 6.496291879603339758, 7.608037276739255006, 1.199719254218452935 ) ) ;
#109014 = ORIENTED_EDGE ( 'NONE', *, *, #41171, .F. ) ;
#109015 = CARTESIAN_POINT ( 'NONE',  ( -4.207966135563104615, 7.175396087857926375, -2.420000000000000373 ) ) ;
#109016 = AXIS2_PLACEMENT_3D ( 'NONE', #85859, #71715, #137828 ) ;
#109017 = CARTESIAN_POINT ( 'NONE',  ( 6.586557105272873969, -1.791547847876047594, -0.3505316570680468979 ) ) ;
#109019 = CARTESIAN_POINT ( 'NONE',  ( 1.534256617913127174, 0.6047330867673149646, 1.817800723622571057 ) ) ;
#109018 = CARTESIAN_POINT ( 'NONE',  ( -3.358669367883384105, 4.941533567329135401, -1.599625672291262513 ) ) ;
#109020 = DIRECTION ( 'NONE',  ( 1.000000000000000000, 1.156482317317871725E-15, 0.000000000000000000 ) ) ;
#109021 = CARTESIAN_POINT ( 'NONE',  ( -1.453605123272271094, 13.24045051524828942, -0.3701785320580647798 ) ) ;
#109022 = AXIS2_PLACEMENT_3D ( 'NONE', #129062, #148428, #195035 ) ;
#109023 = CARTESIAN_POINT ( 'NONE',  ( -1.364683531250000748, 2.321875000341422357, 1.214306433183764966E-14 ) ) ;
#109024 = CARTESIAN_POINT ( 'NONE',  ( 0.000000000000000000, 4.000000000000003553, 0.000000000000000000 ) ) ;
#109025 = CARTESIAN_POINT ( 'NONE',  ( 7.349928672384120176, 7.747540670635879145, 0.7216878364870267237 ) ) ;
#109026 = CARTESIAN_POINT ( 'NONE',  ( -4.936577329151611515, 7.813071746435248599, 1.082531754730549967 ) ) ;
#109027 = CARTESIAN_POINT ( 'NONE',  ( -5.413448473606448985, 9.537716662508005427, 0.000000000000000000 ) ) ;
#109028 = CARTESIAN_POINT ( 'NONE',  ( 2.619513681940002670, 1.793805257907291395, 1.130712135851599687 ) ) ;
#109030 = CARTESIAN_POINT ( 'NONE',  ( -9.986107380900749675, 5.615474669794299878, -5.966265754238714969 ) ) ;
#109029 = CARTESIAN_POINT ( 'NONE',  ( -0.1298852118744100725, 7.629137130509058728, -2.326516543997098729 ) ) ;
#109031 = CARTESIAN_POINT ( 'NONE',  ( 4.956303624527079066, 0.7517850369052423432, 1.822569506419220220 ) ) ;
#109032 = CARTESIAN_POINT ( 'NONE',  ( 6.275647926998929371, 0.3200337115364471074, -1.885262484646982095 ) ) ;
#109033 = ORIENTED_EDGE ( 'NONE', *, *, #68466, .T. ) ;
#109034 = CARTESIAN_POINT ( 'NONE',  ( 6.192584684491233560, 1.567513771475435247, -1.423521977300482577 ) ) ;
#109035 = CARTESIAN_POINT ( 'NONE',  ( -0.5973138996857457750, 6.735707300253057639, -3.614276400337344874 ) ) ;
#109036 = CARTESIAN_POINT ( 'NONE',  ( 1.891162872569674080, 0.2007839719405465906, 2.060584128686280714 ) ) ;
#109037 = CARTESIAN_POINT ( 'NONE',  ( 3.187375889530741802, -0.7864489302777454283, 1.775747734548535961 ) ) ;
#109038 = ORIENTED_EDGE ( 'NONE', *, *, #8106, .T. ) ;
#109039 = CARTESIAN_POINT ( 'NONE',  ( 6.042093733545556233, 7.078139439671806699, -1.199719254218452047 ) ) ;
#109040 = CARTESIAN_POINT ( 'NONE',  ( 6.821687566331318564, 7.987665577921906568, 1.199719254218452935 ) ) ;
#109042 = CARTESIAN_POINT ( 'NONE',  ( 5.656776405399742025, 7.622658444431597680, -1.599625672291262513 ) ) ;
#109041 = CARTESIAN_POINT ( 'NONE',  ( 3.257844248621785788, 0.9402718649541740303, 1.867333078124802315 ) ) ;
#109043 = CARTESIAN_POINT ( 'NONE',  ( 5.383996397958233260, 5.453953017138946535, -0.7216878364870458196 ) ) ;
#109045 = ORIENTED_EDGE ( 'NONE', *, *, #81110, .T. ) ;
#109044 = CARTESIAN_POINT ( 'NONE',  ( 0.6096459265214678735, -0.6533943968328138618, 1.689718745909152053 ) ) ;
#109046 = CARTESIAN_POINT ( 'NONE',  ( 5.848300530743933301, 2.204158087718602221, 0.1119919437090263481 ) ) ;
#109047 = CARTESIAN_POINT ( 'NONE',  ( 3.017802228139008225, 6.452510944783090174, -0.1818790228878484905 ) ) ;
#109048 = CARTESIAN_POINT ( 'NONE',  ( 3.329339556154627289, 0.05228039400686017302, 2.206313527657398854 ) ) ;
#109049 = CARTESIAN_POINT ( 'NONE',  ( 7.584896871841365851, 10.93646455286856956, -1.199719254218446718 ) ) ;
#109050 = CARTESIAN_POINT ( 'NONE',  ( 3.158686601859607812, 6.628958768904106513, -0.7216878364870269458 ) ) ;
#109051 = CARTESIAN_POINT ( 'NONE',  ( 3.422422624566554994, -0.7774026117220147469, -1.747318718686732275 ) ) ;
#109052 = CARTESIAN_POINT ( 'NONE',  ( 9.154780037725547714, 11.70366268214508487, 1.599625672291279388 ) ) ;
#109053 = CARTESIAN_POINT ( 'NONE',  ( 5.389151899530504330, 0.1487064154041470299, 2.065066873896327593 ) ) ;
#109054 = CIRCLE ( 'NONE', #160796, 11.09999999999999964 ) ;
#109056 = CARTESIAN_POINT ( 'NONE',  ( 3.081113354808207916, -0.1575343947536785305, -2.156009052512488200 ) ) ;
#109055 = CARTESIAN_POINT ( 'NONE',  ( -3.054546515950523400, 6.451825606165701998, 0.6676900015689657408 ) ) ;
#109057 = CARTESIAN_POINT ( 'NONE',  ( 5.126606437771586755, 0.1607948393855564151, 2.185736094377451089 ) ) ;
#109058 = VERTEX_POINT ( 'NONE', #59322 ) ;
#109059 = VERTEX_POINT ( 'NONE', #192507 ) ;
#109060 = CARTESIAN_POINT ( 'NONE',  ( 9.911173986789782120, 11.52179005846497972, -1.199719254218440723 ) ) ;
#109061 = CARTESIAN_POINT ( 'NONE',  ( 0.4304495291404202839, 3.052659083096553871, -0.4198826858263793871 ) ) ;
#109062 = CARTESIAN_POINT ( 'NONE',  ( 4.450808633097254052, 7.987047222781193057, -2.500000000000000444 ) ) ;
#109063 = ADVANCED_FACE ( 'NONE', ( #11629 ), #112178, .F. ) ;
#109064 = CARTESIAN_POINT ( 'NONE',  ( 3.901714345682657292, 7.774026846596938434, 0.7998128361456271485 ) ) ;
#109065 = CARTESIAN_POINT ( 'NONE',  ( 1.001543065824772753E-15, -2.559374999522041172, 3.793834371823810780 ) ) ;
#109067 = CARTESIAN_POINT ( 'NONE',  ( -7.673551755654729689, 11.89630144833179060, 0.7216878364870458196 ) ) ;
#109066 = AXIS2_PLACEMENT_3D ( 'NONE', #2885, #22341, #35406 ) ;
#109068 = CARTESIAN_POINT ( 'NONE',  ( 6.574778147984297938, 6.635272358928617997, -0.7998128361456481317 ) ) ;
#109069 = CARTESIAN_POINT ( 'NONE',  ( 5.489151832033660305, 0.1466973765328460355, 2.065091666743318122 ) ) ;
#109070 = CARTESIAN_POINT ( 'NONE',  ( 4.072816532378962684, -1.798017144868354178, -0.6922151418781684606 ) ) ;
#109071 = CARTESIAN_POINT ( 'NONE',  ( 0.4566579290818244541, -1.899626807963299635, -0.6766942018802262204 ) ) ;
#109072 = CARTESIAN_POINT ( 'NONE',  ( -8.462260433223891098, 13.02438760540324481, -0.7998128361456281477 ) ) ;
#109073 = CARTESIAN_POINT ( 'NONE',  ( 7.452141709366786770, 8.723195411463290583, 1.199719254218452047 ) ) ;
#109074 = CARTESIAN_POINT ( 'NONE',  ( -4.811125034100962594, 6.783301700437176507, -1.284903130169626539 ) ) ;
#109075 = CARTESIAN_POINT ( 'NONE',  ( 5.172688686914132639, 1.361056241693802349, -1.423677202773800721 ) ) ;
#109076 = CARTESIAN_POINT ( 'NONE',  ( 6.720655732516684466, -0.007268404184076341853, 2.273772995263834140 ) ) ;
#109077 = CARTESIAN_POINT ( 'NONE',  ( 4.793472150574508817, 1.354911484294840429, 1.223852735664505698 ) ) ;
#109079 = EDGE_CURVE ( 'NONE', #40760, #63091, #71722, .T. ) ;
#109078 = AXIS2_PLACEMENT_3D ( 'NONE', #53050, #134345, #203540 ) ;
#109080 = CARTESIAN_POINT ( 'NONE',  ( 6.780486220610169035, 9.003929572168926754, -1.443375672974078761 ) ) ;
#109081 = CARTESIAN_POINT ( 'NONE',  ( 4.826339496340538382, 4.733076955259818419, 1.040834085586084257E-14 ) ) ;
#109082 = CARTESIAN_POINT ( 'NONE',  ( -6.317173229324657413, 6.334733287159020954, 0.000000000000000000 ) ) ;
#109083 = CARTESIAN_POINT ( 'NONE',  ( 5.564695703766185275, 5.456842840674144490, 0.000000000000000000 ) ) ;
#109084 = ORIENTED_EDGE ( 'NONE', *, *, #81005, .T. ) ;
#109086 = CARTESIAN_POINT ( 'NONE',  ( 5.959245303985257536, -1.698412939339728700, 1.080668751846917797 ) ) ;
#109085 = CARTESIAN_POINT ( 'NONE',  ( 2.788419073117563762, 1.577926727847511312, -0.9486480243563880643 ) ) ;
#109087 = CARTESIAN_POINT ( 'NONE',  ( 0.5272844384777974902, 2.272924705895418285, -0.3403917945235325204 ) ) ;
#109088 = CARTESIAN_POINT ( 'NONE',  ( 5.242999579849755953, -0.2363135928187160284, -1.947375393322479109 ) ) ;
#109089 = CARTESIAN_POINT ( 'NONE',  ( -4.218558352146454915, 8.073401844146177453, 1.040834085586084257E-14 ) ) ;
#109090 = CARTESIAN_POINT ( 'NONE',  ( -7.011678565220742065, -6.606405293530505318, 6.580818069394644532 ) ) ;
#109091 = CARTESIAN_POINT ( 'NONE',  ( -3.541704441667874903, 5.155074486744371853, -1.599625672291256295 ) ) ;
#109092 = CARTESIAN_POINT ( 'NONE',  ( 0.7485892145711986467, -2.054541080789675789, -0.2550698046258002005 ) ) ;
#109093 = CARTESIAN_POINT ( 'NONE',  ( -4.125423880308188629, 8.035021303660014880, -0.7998128361456481317 ) ) ;
#109095 = CARTESIAN_POINT ( 'NONE',  ( 0.4966798268824790252, 1.557709316500059726, -1.035497600327957235 ) ) ;
#109094 = CARTESIAN_POINT ( 'NONE',  ( 1.610996488345920907, -0.2524672473064055733, 2.075362222853482930 ) ) ;
#109096 = CARTESIAN_POINT ( 'NONE',  ( 1.423203639035979906, 0.8144988626696235690, 1.844428818423976546 ) ) ;
#109097 = EDGE_LOOP ( 'NONE', ( #150170, #159202 ) ) ;
#109098 = CARTESIAN_POINT ( 'NONE',  ( -0.6823417656250212460, 4.613541667008086655, 1.181850606188767472 ) ) ;
#109099 = B_SPLINE_CURVE_WITH_KNOTS ( 'NONE', 3,
 ( #15307, #115026, #198322, #146429, #81395, #100834 ),
 .UNSPECIFIED., .F., .F.,
 ( 4, 2, 4 ),
 ( 0.000000000000000000, 0.0003141588434155108628, 0.0006283176868310217256 ),
 .UNSPECIFIED. ) ;
#109100 = CARTESIAN_POINT ( 'NONE',  ( 1.909305195714078307, -0.8207579233160157139, -1.534770245041901182 ) ) ;
#109101 = CARTESIAN_POINT ( 'NONE',  ( 3.811813743736467419, 7.598866467667865443, 1.040834085586084257E-14 ) ) ;
#109103 = CARTESIAN_POINT ( 'NONE',  ( 1.522028533774268277, 8.691231065131713507, 2.524624912498933504 ) ) ;
#109102 = DIRECTION ( 'NONE',  ( 1.561251128379126077E-17, 1.301042606982605475E-17, 1.000000000000000000 ) ) ;
#109104 = CARTESIAN_POINT ( 'NONE',  ( 2.666273504311657661, -1.189765394598929937, 1.249106299861786118 ) ) ;
#109105 = CARTESIAN_POINT ( 'NONE',  ( 2.859115728684503477, 0.3189004193784421015, -2.168101852914063876 ) ) ;
#109106 = CARTESIAN_POINT ( 'NONE',  ( 4.793709216081707858, 1.633822259641436903, 1.483752339651790653 ) ) ;
#109107 = CARTESIAN_POINT ( 'NONE',  ( -10.82993273518205690, 5.589502548902120616, -6.507125152095314391 ) ) ;
#109108 = CARTESIAN_POINT ( 'NONE',  ( 2.237404288245536943, -0.1031769000767470690, -2.168708286310920386 ) ) ;
#109109 = CARTESIAN_POINT ( 'NONE',  ( 1.523764310407935030, -1.012771255265769943, -1.518815351243132383 ) ) ;
#109110 = CARTESIAN_POINT ( 'NONE',  ( 3.749298086285374865, 0.2552367968642406115, -2.101811201404654827 ) ) ;
#109111 = DIRECTION ( 'NONE',  ( 0.000000000000000000, 0.000000000000000000, -1.000000000000000000 ) ) ;
#109112 = ADVANCED_FACE ( 'NONE', ( #91855, #46294 ), #144886, .T. ) ;
#109113 = ORIENTED_EDGE ( 'NONE', *, *, #67371, .F. ) ;
#109115 = CARTESIAN_POINT ( 'NONE',  ( 1.364683531249988757, 1.446875000341421469, 0.000000000000000000 ) ) ;
#109114 = CARTESIAN_POINT ( 'NONE',  ( 3.650172380179962150, 0.8259502761284505112, 2.138564905064809896 ) ) ;
#109116 = LINE ( 'NONE', #92819, #167852 ) ;
#109117 = CARTESIAN_POINT ( 'NONE',  ( 4.111146893441827821, 5.819424013814004759, 1.599625672291267398 ) ) ;
#109118 = CARTESIAN_POINT ( 'NONE',  ( 6.358078514681034576, 0.8530912398192547208, -2.051143523256500067 ) ) ;
#109119 = CARTESIAN_POINT ( 'NONE',  ( -5.965224400332865606, 7.022145224218852455, 1.082531754730549967 ) ) ;
#109120 = CARTESIAN_POINT ( 'NONE',  ( 2.724825686666657809, 6.122787701178987518, 0.000000000000000000 ) ) ;
#109121 = AXIS2_PLACEMENT_3D ( 'NONE', #2238, #197265, #48905 ) ;
#109122 = CARTESIAN_POINT ( 'NONE',  ( -7.524412065460066579, 7.880828285899290186, 0.7216878364870317197 ) ) ;
#109124 = B_SPLINE_CURVE_WITH_KNOTS ( 'NONE', 3,
 ( #114794, #127889, #48677, #193840, #46549, #162430, #146196, #115855 ),
 .UNSPECIFIED., .F., .F.,
 ( 4, 2, 2, 4 ),
 ( 0.001893943459172981250, 0.002262838117583250517, 0.002447285446788384933, 0.002631732775993519350 ),
 .UNSPECIFIED. ) ;
#109123 = CARTESIAN_POINT ( 'NONE',  ( -0.5000000000000455191, 3.999999999999955147, 0.4499999999999521605 ) ) ;
#109125 = ORIENTED_EDGE ( 'NONE', *, *, #200070, .F. ) ;
#109126 = CARTESIAN_POINT ( 'NONE',  ( 4.447888798048591497, -1.802416534049579910, -0.9041112711936499791 ) ) ;
#109128 = CARTESIAN_POINT ( 'NONE',  ( 3.784078317859154605, -1.224626257592566159, -1.659553996539532283 ) ) ;
#109127 = CARTESIAN_POINT ( 'NONE',  ( 6.449928391799196525, 8.548002428564306143, -1.599625672291262513 ) ) ;
#109129 = CARTESIAN_POINT ( 'NONE',  ( -3.673896439623323129, 4.156855427197417185, 1.000000000000009548 ) ) ;
#109130 = EDGE_CURVE ( 'NONE', #2289, #1199, #61455, .T. ) ;
#109131 = CARTESIAN_POINT ( 'NONE',  ( 4.001064729364292916, 6.721640380016713934, -1.082531754730548412 ) ) ;
#109132 = CARTESIAN_POINT ( 'NONE',  ( -3.285556943750000514, -3.288541666188709023, -1.896917185911906500 ) ) ;
#109133 = CARTESIAN_POINT ( 'NONE',  ( 0.6823417656249917140, 5.592708333674749177, 1.181850606188765695 ) ) ;
#109134 = CARTESIAN_POINT ( 'NONE',  ( 6.580031370938625557, -2.148343778048496411, -0.4316624935760752790 ) ) ;
#109135 = CARTESIAN_POINT ( 'NONE',  ( 4.026017654026761150, -1.753031021560845559, 0.9963007555989014108 ) ) ;
#109136 = CARTESIAN_POINT ( 'NONE',  ( 2.454439063956286304, -1.602943312447857593, -0.9057913635923324769 ) ) ;
#109137 = CARTESIAN_POINT ( 'NONE',  ( 5.686755365928134687, 8.721966129303114101, 1.199719254218462483 ) ) ;
#109138 = CARTESIAN_POINT ( 'NONE',  ( 6.176747059734421619, -1.734417727105644680, -0.5698399933231483860 ) ) ;
#109139 = CARTESIAN_POINT ( 'NONE',  ( -0.1219072497536327904, -0.5225375287686329084, -2.247936139081475382 ) ) ;
#109140 = CARTESIAN_POINT ( 'NONE',  ( -7.552055258011950656, 8.769484874890757453, 1.199719254218462483 ) ) ;
#109142 = CARTESIAN_POINT ( 'NONE',  ( -4.522526758610270647, 7.433975764090723359, -1.199719254218453823 ) ) ;
#109141 = CARTESIAN_POINT ( 'NONE',  ( 6.139586942761116717, -1.633760600410700592, -1.565427815648293031 ) ) ;
#109143 = CARTESIAN_POINT ( 'NONE',  ( 1.823018060162405085, 1.965545597939293954, 0.7568914254860066304 ) ) ;
#109144 = CARTESIAN_POINT ( 'NONE',  ( -6.017840079619296567, 8.114175741012878973, -1.599625672291271394 ) ) ;
#109145 = CARTESIAN_POINT ( 'NONE',  ( 6.577677080924314801, 10.82570702772039262, 1.040834085586084257E-14 ) ) ;
#109146 = CARTESIAN_POINT ( 'NONE',  ( 6.156811153937166381, 10.19704708965311468, 0.000000000000000000 ) ) ;
#109147 = CARTESIAN_POINT ( 'NONE',  ( 8.378074386687003994, 18.20815134976857053, 15.76159487570644124 ) ) ;
#109148 = CARTESIAN_POINT ( 'NONE',  ( -7.888146445052511169, 8.097259028849730811, 1.040834085586084257E-14 ) ) ;
#109149 = CARTESIAN_POINT ( 'NONE',  ( 1.499999999999959588, 7.193113254731348327, -10.88798745763944353 ) ) ;
#109150 = CARTESIAN_POINT ( 'NONE',  ( 7.036318535368067728, 10.19249347702934294, -1.082531754730537976 ) ) ;
#109151 = CARTESIAN_POINT ( 'NONE',  ( 4.037917249208685000, 7.776151245443112536, -0.4343759663945709892 ) ) ;
#109152 = CARTESIAN_POINT ( 'NONE',  ( -6.084912014434944894, 5.993485526462540847, -0.7998128361456291469 ) ) ;
#109154 = CARTESIAN_POINT ( 'NONE',  ( 3.305138010220570521, -0.4367349056570711263, -2.177900917948209614 ) ) ;
#109153 = CARTESIAN_POINT ( 'NONE',  ( 2.021885665735908333, -0.4598567139443253682, 2.069992740399699382 ) ) ;
#109155 = CARTESIAN_POINT ( 'NONE',  ( 0.1357705729100426029, -2.015811560716780360, 0.8986578214904348272 ) ) ;
#109156 = CARTESIAN_POINT ( 'NONE',  ( -6.448838341955544173, 7.552674816150118708, 1.199719254218452047 ) ) ;
#109157 = CARTESIAN_POINT ( 'NONE',  ( 6.308621549060418054, 6.254479983525607523, 0.7998128361456341429 ) ) ;
#109158 = CARTESIAN_POINT ( 'NONE',  ( 4.703538834289092030, -1.515240342570793430, -1.246145567450624991 ) ) ;
#109159 = CARTESIAN_POINT ( 'NONE',  ( 9.348510611822643313, 10.86534945433664134, 1.199719254218453823 ) ) ;
#109160 = CARTESIAN_POINT ( 'NONE',  ( -5.485560113408387117, 6.267152048184752466, 0.9985905309092910631 ) ) ;
#109161 = DIRECTION ( 'NONE',  ( 0.5994789404140892231, -6.777585655618907357E-14, -0.8003905296791067325 ) ) ;
#109162 = CARTESIAN_POINT ( 'NONE',  ( 1.364683531249986537, 0.8635416670080893198, 0.7879004041258500513 ) ) ;
#109163 = CARTESIAN_POINT ( 'NONE',  ( -4.584065335196305213, 6.441438539186039591, 1.443375672974058777 ) ) ;
#109165 = ORIENTED_EDGE ( 'NONE', *, *, #136379, .F. ) ;
#109164 = CARTESIAN_POINT ( 'NONE',  ( -5.992340707560165569, 8.014150130285418783, 1.443375672974064550 ) ) ;
#109166 = CARTESIAN_POINT ( 'NONE',  ( 3.849942018323779358, -1.464806807754112539, -1.533599281611098597 ) ) ;
#109167 = CARTESIAN_POINT ( 'NONE',  ( -5.448397627845328550, 7.449826213943242514, 1.599625672291263179 ) ) ;
#109168 = CARTESIAN_POINT ( 'NONE',  ( 4.452137864729129646, 2.161286467946467837, -0.05003489268536746859 ) ) ;
#109169 = CARTESIAN_POINT ( 'NONE',  ( 4.317794123949899365, 1.129187743159822288, -1.454283868005897151 ) ) ;
#109170 = CARTESIAN_POINT ( 'NONE',  ( -5.471750928372196121, 6.276313537582185909, 1.010767274114855008 ) ) ;
#109171 = CARTESIAN_POINT ( 'NONE',  ( -1.201851678989727383E-14, 1.634375000341421025, 1.575800808251672791 ) ) ;
#109172 = CARTESIAN_POINT ( 'NONE',  ( 6.281193118957388855, 1.205677877666534892, 1.255287683557136491 ) ) ;
#109173 = CARTESIAN_POINT ( 'NONE',  ( 6.727182134110203826, 0.5859025467632031914, 1.963451964196837984 ) ) ;
#109174 = CARTESIAN_POINT ( 'NONE',  ( 4.392478581147586603, 4.226905887534702977, -0.7216878364870188411 ) ) ;
#109175 = CARTESIAN_POINT ( 'NONE',  ( 11.84668730067608777, 13.50634727754795250, -1.400000000000001910 ) ) ;
#109176 = CARTESIAN_POINT ( 'NONE',  ( 3.713887418366210280, -2.130098009959373151, 0.3673708613747132534 ) ) ;
#109177 = ORIENTED_EDGE ( 'NONE', *, *, #133456, .F. ) ;
#109178 = CARTESIAN_POINT ( 'NONE',  ( 5.677111188754776272, -0.9039728708103295096, -1.802140534545144890 ) ) ;
#109179 = CARTESIAN_POINT ( 'NONE',  ( -8.310784975052682100, 10.71900177569337487, -1.443375672974058777 ) ) ;
#109180 = CARTESIAN_POINT ( 'NONE',  ( 3.854492016355787420, 0.7758605394001509836, 2.017853709245204463 ) ) ;
#109181 = CARTESIAN_POINT ( 'NONE',  ( 3.321511454083085457, -1.900871985879136528, 0.5222822307265824193 ) ) ;
#109182 = AXIS2_PLACEMENT_3D ( 'NONE', #171362, #22956, #155128 ) ;
#109183 = DIRECTION ( 'NONE',  ( 0.000000000000000000, 7.254698431504986582E-17, -1.000000000000000000 ) ) ;
#109184 = CARTESIAN_POINT ( 'NONE',  ( 1.308152564336163115, -0.5581994038030186900, 2.238931160296030232 ) ) ;
#109185 = CARTESIAN_POINT ( 'NONE',  ( 2.038423305949757847, 2.037923218716758633, 0.3053300769366319445 ) ) ;
#109186 = CARTESIAN_POINT ( 'NONE',  ( 4.739756017840593749, 1.937102985688110568, 0.1393878014490906314 ) ) ;
#109189 = ORIENTED_EDGE ( 'NONE', *, *, #103866, .F. ) ;
#109188 = DIRECTION ( 'NONE',  ( 0.000000000000000000, 0.000000000000000000, 1.000000000000000000 ) ) ;
#109187 = CARTESIAN_POINT ( 'NONE',  ( -7.931156673870055407, 11.23647130528163096, 1.082531754730549967 ) ) ;
#109190 = B_SPLINE_CURVE_WITH_KNOTS ( 'NONE', 3,
 ( #174116, #91797, #157854, #171957, #9448, #189265, #173034 ),
 .UNSPECIFIED., .F., .F.,
 ( 4, 3, 4 ),
 ( 5.085429910792683232E-15, 2.761892602843915009E-05, 5.460426739256992639E-05 ),
 .UNSPECIFIED. ) ;
#109191 = CARTESIAN_POINT ( 'NONE',  ( -4.932134020321308654, 8.976183133675331050, 0.7998128361456291469 ) ) ;
#109192 = DIRECTION ( 'NONE',  ( 0.6507913734559640506, -0.7592566023653004592, 0.000000000000000000 ) ) ;
#109194 = ORIENTED_EDGE ( 'NONE', *, *, #191290, .T. ) ;
#109193 = CARTESIAN_POINT ( 'NONE',  ( -4.197131071882288289, 7.054347462908075350, -1.199719254218455378 ) ) ;
#109195 = CARTESIAN_POINT ( 'NONE',  ( -6.195713011320783892, 10.17215624660883577, -0.7216878364870267237 ) ) ;
#109196 = CARTESIAN_POINT ( 'NONE',  ( 1.958336283151569157, 2.200835622443702011, -0.1624582802550941507 ) ) ;
#109197 = CARTESIAN_POINT ( 'NONE',  ( 0.000000000000000000, -0.5468749995220422155, -3.793834371823813001 ) ) ;
#109198 = CARTESIAN_POINT ( 'NONE',  ( 6.895372015613538075, -1.753720159772365284, 0.8792710811909019153 ) ) ;
#109199 = CARTESIAN_POINT ( 'NONE',  ( -0.02919842301648319441, 0.2290444945237135044, -2.107092690553781456 ) ) ;
#109200 = CARTESIAN_POINT ( 'NONE',  ( -1.499999999999997780, 4.181250000682819490, 1.214306433183764966E-14 ) ) ;
#109202 = CARTESIAN_POINT ( 'NONE',  ( -4.140749582569956289, 7.233010276137757266, -0.9217035184944754045 ) ) ;
#109201 = CARTESIAN_POINT ( 'NONE',  ( 0.1749903794560644099, 4.092791488633133135, -2.510332109122221045 ) ) ;
#109203 = CARTESIAN_POINT ( 'NONE',  ( 5.876868881424701208, 1.699447150514224125, -0.7087742222662285485 ) ) ;
#109204 = ORIENTED_EDGE ( 'NONE', *, *, #61776, .F. ) ;
#109205 = CARTESIAN_POINT ( 'NONE',  ( 1.224999999999994982, 2.666666667349464781, 0.7072540797572857141 ) ) ;
#109206 = UNCERTAINTY_MEASURE_WITH_UNIT (LENGTH_MEASURE( 1.000000000000000082E-05 ), #79686, 'distance_accuracy_value', 'NONE');
#109207 = CARTESIAN_POINT ( 'NONE',  ( -7.152089726408780379, 8.302858421353754181, -1.199719254218446718 ) ) ;
#109208 = DIRECTION ( 'NONE',  ( 3.330669073875478989E-16, -3.330669073875478989E-16, -1.000000000000000000 ) ) ;
#109210 = EDGE_CURVE ( 'NONE', #108613, #205532, #47367, .T. ) ;
#109209 = CARTESIAN_POINT ( 'NONE',  ( 6.275647701495586261, 0.3610785225884837746, -2.089460823871174266 ) ) ;
#109211 = CARTESIAN_POINT ( 'NONE',  ( 11.92008656065780947, 6.690339256190793726, -0.9868697903839722674 ) ) ;
#109212 = CARTESIAN_POINT ( 'NONE',  ( 3.662674053986138656, 7.424870162959149589, 0.7998128361456321445 ) ) ;
#109213 = CARTESIAN_POINT ( 'NONE',  ( 0.3915709625425906615, 1.526647161510179318, 1.384594130533061129 ) ) ;
#109216 = CARTESIAN_POINT ( 'NONE',  ( 4.317794123949899365, 1.129187743159822288, -1.454283868005897151 ) ) ;
#109215 = CARTESIAN_POINT ( 'NONE',  ( 1.398636348511049565, 0.3583461405318502102, 1.826042456754966681 ) ) ;
#109214 = CARTESIAN_POINT ( 'NONE',  ( -10.44512553078396344, 5.055828132299228450, 5.909874117198688381 ) ) ;
#109217 = CARTESIAN_POINT ( 'NONE',  ( 7.470706336329915764, 8.674577799595093452, -1.199719254218441611 ) ) ;
#109218 = CARTESIAN_POINT ( 'NONE',  ( -4.428767733937130302, 15.51888673063479196, 11.16163516131764233 ) ) ;
#109219 = CARTESIAN_POINT ( 'NONE',  ( -4.932134020321308654, 8.976183133675331050, 0.7998128361456291469 ) ) ;
#109221 = VERTEX_POINT ( 'NONE', #63591 ) ;
#109220 = CARTESIAN_POINT ( 'NONE',  ( -6.534012848836717957, -6.583711766989042147, -7.055786748303233935 ) ) ;
#109222 = CIRCLE ( 'NONE', #198933, 2.000000000000006217 ) ;
#109223 = CARTESIAN_POINT ( 'NONE',  ( 4.811249113497881424, 1.919052844561389692, 1.089612025192594258 ) ) ;
#109224 = CARTESIAN_POINT ( 'NONE',  ( 6.186863813140405455, -0.3229369685709322924, -2.239133911541963506 ) ) ;
#109225 = CARTESIAN_POINT ( 'NONE',  ( -4.256897045010916258, 7.910204285913967404, 0.7216878364870317197 ) ) ;
#109226 = CARTESIAN_POINT ( 'NONE',  ( -0.08783152977152529350, -1.912005390248720627, -0.04503566501021933483 ) ) ;
#109227 = CARTESIAN_POINT ( 'NONE',  ( 6.139839150192680783, 1.910077931696544384, -0.1482136438759658337 ) ) ;
#109228 = CARTESIAN_POINT ( 'NONE',  ( 3.389175213736273840, 6.897862149426906342, 0.7216878364870233931 ) ) ;
#109229 = CARTESIAN_POINT ( 'NONE',  ( 0.07536363704230969462, 1.333366039338843789, -2.397125032416930424 ) ) ;
#109230 = CARTESIAN_POINT ( 'NONE',  ( 5.777967262743825216, 1.883199444611630469, -0.3313529498064629042 ) ) ;
#109231 = CARTESIAN_POINT ( 'NONE',  ( 11.41157692552970815, 12.34089662913000573, -3.404533818002362100 ) ) ;
#109232 = CARTESIAN_POINT ( 'NONE',  ( 1.217418975555501826, -1.825842229346545498, 0.4062821374252246764 ) ) ;
#109233 = CARTESIAN_POINT ( 'NONE',  ( 2.378138974734815392, -2.011451771401792321, -0.1435188914247695346 ) ) ;
#109235 = CARTESIAN_POINT ( 'NONE',  ( 4.143269384990833970, -1.832638288540566318, 1.037631460274644812 ) ) ;
#109234 = CARTESIAN_POINT ( 'NONE',  ( -9.189729191964438826, 9.615772233580322848, 1.040834085586084257E-14 ) ) ;
#109236 = CARTESIAN_POINT ( 'NONE',  ( 8.620286740190458374, 8.951422706510690830, 1.040834085586084257E-14 ) ) ;
#109238 = CARTESIAN_POINT ( 'NONE',  ( -8.690940161559884913, 10.09818392903003748, 1.199719254218462483 ) ) ;
#109237 = CARTESIAN_POINT ( 'NONE',  ( 1.499999999999987121, -0.2458333333333099502, 0.8660254037844524744 ) ) ;
#109239 = FACE_OUTER_BOUND ( 'NONE', #122049, .T. ) ;
#109240 = CARTESIAN_POINT ( 'NONE',  ( 2.689718276569666333, 1.916506935140523726, -0.6377304922457660563 ) ) ;
#109241 = CARTESIAN_POINT ( 'NONE',  ( -1.364683531250012516, 3.030208333674755394, 0.7879004041258379498 ) ) ;
#109242 = VECTOR ( 'NONE', #54935, 1000.000000000000000 ) ;
#109243 = EDGE_CURVE ( 'NONE', #111689, #205992, #49473, .T. ) ;
#109244 = CARTESIAN_POINT ( 'NONE',  ( 10.24960094225127172, 11.06021530882240356, -0.7216878364870257245 ) ) ;
#109245 = CARTESIAN_POINT ( 'NONE',  ( 4.253314833958360630, -1.794556715717060769, -1.204719293387515267 ) ) ;
#109246 = CARTESIAN_POINT ( 'NONE',  ( -0.9311234436981496998, -1.634380368602566636, 3.475000000000000977 ) ) ;
#109247 = CARTESIAN_POINT ( 'NONE',  ( -1.499999999999997780, 5.650000000000023448, 1.214306433183764966E-14 ) ) ;
#109249 = CARTESIAN_POINT ( 'NONE',  ( -9.493819324367761325, -9.279866070759378971, 0.3645580569638187662 ) ) ;
#109248 = CARTESIAN_POINT ( 'NONE',  ( 6.912678218121202534, 9.158153569265168770, 1.599625672291268286 ) ) ;
#109250 = CARTESIAN_POINT ( 'NONE',  ( 9.205623113554628034, 9.842241175342985926, 0.7216878364870458196 ) ) ;
#109252 = LINE ( 'NONE', #195758, #107589 ) ;
#109251 = CARTESIAN_POINT ( 'NONE',  ( 2.471331864234734610, 1.938535094165691142, 0.9779774689679074928 ) ) ;
#109254 = CARTESIAN_POINT ( 'NONE',  ( 0.9426144736941791669, -1.451487892885485742, -1.132780452900377099 ) ) ;
#109253 = CARTESIAN_POINT ( 'NONE',  ( -5.246642258808529746, 9.064907035344523578, 0.000000000000000000 ) ) ;
#109255 = CARTESIAN_POINT ( 'NONE',  ( -1.201851678989727383E-14, 2.571875000341417472, 1.575800808251672791 ) ) ;
#109256 = CARTESIAN_POINT ( 'NONE',  ( 1.575987392057216940, -1.168677030305173004, 1.853764812240476623 ) ) ;
#109257 = CARTESIAN_POINT ( 'NONE',  ( 6.266000345369230118, 6.920845220647411367, 0.8521018698646137812 ) ) ;
#109258 = CARTESIAN_POINT ( 'NONE',  ( 3.221791447092836602, -2.180992460559240786, 0.6016781482265749492 ) ) ;
#109259 = CARTESIAN_POINT ( 'NONE',  ( -7.881367368245678406, 8.089350105908421185, 0.7998128361456602331 ) ) ;
#109260 = CARTESIAN_POINT ( 'NONE',  ( -1.001543065824772872E-14, 5.134375000341421469, 1.575800808251672791 ) ) ;
#109261 = CARTESIAN_POINT ( 'NONE',  ( 5.028717893731355026, 7.888467461587344687, 1.094519599958807765 ) ) ;
#109262 = CARTESIAN_POINT ( 'NONE',  ( 1.500000000000001332, 12.37499999999999645, 0.000000000000000000 ) ) ;
#109263 = CARTESIAN_POINT ( 'NONE',  ( 7.024532985656141371, 7.367912369453226695, 0.7216878364870328300 ) ) ;
#109264 = CARTESIAN_POINT ( 'NONE',  ( 4.393649985211129483, -0.6784793013954493190, 1.634714195790587077 ) ) ;
#109265 = CARTESIAN_POINT ( 'NONE',  ( 9.759171643738394408, 10.28012176064996197, 0.000000000000000000 ) ) ;
#109266 = CARTESIAN_POINT ( 'NONE',  ( 0.5343771797220103759, 1.082321145649869587, -1.806417116151628477 ) ) ;
#109268 = CARTESIAN_POINT ( 'NONE',  ( 1.499999999999989120, 1.525000000000019451, 0.000000000000000000 ) ) ;
#109267 = CARTESIAN_POINT ( 'NONE',  ( -1.402160292154681736E-14, 10.17187500034139447, 1.575800808251682339 ) ) ;
#109269 = CARTESIAN_POINT ( 'NONE',  ( -4.472210567661380587, 6.310941310395290493, 1.599625672291270506 ) ) ;
#109270 = CARTESIAN_POINT ( 'NONE',  ( 6.064077406165095496, -1.076301619396256237, 1.704949653848472302 ) ) ;
#109271 = ORIENTED_EDGE ( 'NONE', *, *, #124727, .F. ) ;
#109272 = CARTESIAN_POINT ( 'NONE',  ( 7.958272981541723468, 8.386999354661243800, 1.040834085586084257E-14 ) ) ;
#109273 = EDGE_CURVE ( 'NONE', #5447, #201551, #108766, .T. ) ;
#109274 = CARTESIAN_POINT ( 'NONE',  ( 10.40996301719436090, 11.03937836301526687, 0.000000000000000000 ) ) ;
#109275 = CARTESIAN_POINT ( 'NONE',  ( 3.977312496258199825, 1.761605600429091201, -0.6297503393934977822 ) ) ;
#109276 = CARTESIAN_POINT ( 'NONE',  ( 3.907136544319700810, -1.695332804699274387, 1.187946514627869821 ) ) ;
#109277 = CARTESIAN_POINT ( 'NONE',  ( -6.604230223188181093, 6.877559146573883453, 0.7216878364870317197 ) ) ;
#109278 = CARTESIAN_POINT ( 'NONE',  ( -1.500000000000008216, 10.78125000068279249, 3.469446951953614189E-15 ) ) ;
#109279 = CARTESIAN_POINT ( 'NONE',  ( 7.456094412511537151, 10.78619501698377370, 1.199719254218460707 ) ) ;
#109280 = CARTESIAN_POINT ( 'NONE',  ( -4.342209589451060836, 5.574336833734898633, -1.249999994511378887 ) ) ;
#109281 = CARTESIAN_POINT ( 'NONE',  ( 6.587282531393223728, 8.778525268082516320, 1.599625672291268286 ) ) ;
#109282 = CARTESIAN_POINT ( 'NONE',  ( -5.814151116872314340, 5.955800188500202985, -0.1636420086626904635 ) ) ;
#109283 = CARTESIAN_POINT ( 'NONE',  ( -1.364683531250010295, 5.301041667008085767, -0.7879004041258300672 ) ) ;
#109284 = CARTESIAN_POINT ( 'NONE',  ( 3.771884902471400292, -1.933230903833718539, 0.3329965046865584477 ) ) ;
#109285 = CARTESIAN_POINT ( 'NONE',  ( 2.548203688163702463, 1.844428314090811538, -0.8144999995377337765 ) ) ;
#109286 = CARTESIAN_POINT ( 'NONE',  ( -4.496464221587651799, 5.274905009054215554, 1.199719254218452935 ) ) ;
#109287 = CARTESIAN_POINT ( 'NONE',  ( -4.889337272013151825, 4.909234758358784312, -0.4031905389056227307 ) ) ;
#109288 = CARTESIAN_POINT ( 'NONE',  ( 0.6142526126209290060, 1.294576594435635108, -1.350420462534522859 ) ) ;
#109289 = CARTESIAN_POINT ( 'NONE',  ( -0.6823417656249969321, 3.467708333674754506, -1.181850606188749264 ) ) ;
#109290 = CARTESIAN_POINT ( 'NONE',  ( 2.883067256526872235, -1.861736025891271407, -0.7665772676846579481 ) ) ;
#109292 = CARTESIAN_POINT ( 'NONE',  ( 3.462624114536147157, -2.041159069107215007, -0.5622701121768166610 ) ) ;
#109291 = CARTESIAN_POINT ( 'NONE',  ( -5.233084105194862445, 9.049089189461916760, 0.7216878364870458196 ) ) ;
#109293 = FACE_OUTER_BOUND ( 'NONE', #205359, .T. ) ;
#109294 = CARTESIAN_POINT ( 'NONE',  ( 4.949704645232674061, 1.531818663031824013, 1.392983054852282132 ) ) ;
#109295 = CARTESIAN_POINT ( 'NONE',  ( 2.911969131885072670, 6.619324097166378706, 0.000000000000000000 ) ) ;
#109297 = CARTESIAN_POINT ( 'NONE',  ( 11.89839339040395139, 13.82877468403908772, 1.560885614203548100 ) ) ;
#109296 = CARTESIAN_POINT ( 'NONE',  ( 0.5563344311030217204, -1.511574431613523117, 1.444666882759609194 ) ) ;
#109299 = VERTEX_POINT ( 'NONE', #133957 ) ;
#109298 = CARTESIAN_POINT ( 'NONE',  ( 5.174738384962677351, -1.719472664011096219, -0.6136495084824307167 ) ) ;
#109300 = CARTESIAN_POINT ( 'NONE',  ( 9.576136569953906275, 10.06658084123472641, 0.000000000000000000 ) ) ;
#109301 = CARTESIAN_POINT ( 'NONE',  ( 4.816739869979735467, 5.096136759539821703, 0.7457829957396797660 ) ) ;
#109302 = CARTESIAN_POINT ( 'NONE',  ( 11.57394138716773213, 8.953477593029530723, 4.723522898263817993 ) ) ;
#109303 = CARTESIAN_POINT ( 'NONE',  ( -10.77299012366456310, 5.423410747438590640, 6.621146351739780833 ) ) ;
#109304 = CARTESIAN_POINT ( 'NONE',  ( -1.364683531250000748, 11.67187500034139802, 0.000000000000000000 ) ) ;
#109305 = CARTESIAN_POINT ( 'NONE',  ( 6.305323439471717251, 1.661359358424657318, -0.9468341723649562613 ) ) ;
#109306 = CARTESIAN_POINT ( 'NONE',  ( -9.657485491635913633, 10.16148791653038330, 1.040834085586084257E-14 ) ) ;
#109307 = CARTESIAN_POINT ( 'NONE',  ( 7.332262146892202459, 7.448727347662698506, -0.7998128361456281477 ) ) ;
#109308 = CARTESIAN_POINT ( 'NONE',  ( 1.360316468749975805, 2.776041667008103175, 0.7853790794158820310 ) ) ;
#109309 = CARTESIAN_POINT ( 'NONE',  ( 3.158686601859607368, 6.628958768904106513, -0.7216878364870267237 ) ) ;
#109310 = CARTESIAN_POINT ( 'NONE',  ( -15.75000000000000000, 12.69999999999999929, -0.7000000000000009548 ) ) ;
#109311 = EDGE_CURVE ( 'NONE', #107614, #138769, #181359, .T. ) ;
#109312 = CARTESIAN_POINT ( 'NONE',  ( 3.174580523894166006, 6.855427711185178019, 0.7998128361456341429 ) ) ;
#109313 = VERTEX_POINT ( 'NONE', #165346 ) ;
#109314 = CARTESIAN_POINT ( 'NONE',  ( -6.557303570864871034, 7.679217583210999010, -1.199719254218452047 ) ) ;
#109315 = CARTESIAN_POINT ( 'NONE',  ( 11.00023875073173762, -5.574346042903139953, 0.04317804960740431047 ) ) ;
#109317 = CARTESIAN_POINT ( 'NONE',  ( 6.668631453075247073, 8.873432343378178544, -1.599625672291281386 ) ) ;
#109316 = DIRECTION ( 'NONE',  ( 0.000000000000000000, -1.000000000000000000, -0.000000000000000000 ) ) ;
#109318 = CIRCLE ( 'NONE', #47123, 0.07999999999999993228 ) ;
#109319 = DIRECTION ( 'NONE',  ( 0.000000000000000000, 0.000000000000000000, -1.000000000000000000 ) ) ;
#109320 = CARTESIAN_POINT ( 'NONE',  ( -0.1399997263889819765, 0.7174702203470960660, -2.082715917450683740 ) ) ;
#109321 =( BOUNDED_CURVE ( )  B_SPLINE_CURVE ( 2, ( #197952, #14923, #81016, #147105, #213129, #146047, #130901 ),
 .UNSPECIFIED., .F., .T. ) 
 B_SPLINE_CURVE_WITH_KNOTS ( ( 3, 2, 2, 3 ),
 ( 0.2250000000000001998, 0.2291666666666669072, 0.2333333333333336701, 0.2375000000000003775 ),
 .UNSPECIFIED. ) 
 CURVE ( )  GEOMETRIC_REPRESENTATION_ITEM ( )  RATIONAL_B_SPLINE_CURVE ( ( 0.9999999999999937828, 0.8660254037844449249, 1.000000000000000000, 0.8660254037844387076, 1.000000000000000000, 0.8660254037844261621, 1.000000000000012434 ) ) 
 REPRESENTATION_ITEM ( '' )  );
#109322 = CARTESIAN_POINT ( 'NONE',  ( -5.910991785878170646, 7.919243054989755670, -1.443375672974059665 ) ) ;
#109323 = AXIS2_PLACEMENT_3D ( 'NONE', #106268, #9771, #75844 ) ;
#109324 = CARTESIAN_POINT ( 'NONE',  ( 4.844340958784499662, 4.546152628203684820, 0.7998128361456341429 ) ) ;
#109325 = CARTESIAN_POINT ( 'NONE',  ( 2.535944157116743369, 1.207843060446149197, 1.555523554018751309 ) ) ;
#109326 = CARTESIAN_POINT ( 'NONE',  ( 3.216422893352603563, 1.967893637826668263, 0.4390085219014849827 ) ) ;
#109327 = CARTESIAN_POINT ( 'NONE',  ( -8.667740277838301921, 9.006785167099828016, -0.7998128361456291469 ) ) ;
#109328 = CARTESIAN_POINT ( 'NONE',  ( 6.827182134110219458, 3.682144966263278363, 2.702925436647874324 ) ) ;
#109329 = CARTESIAN_POINT ( 'NONE',  ( 3.222796723461582413, 0.05406831605479084368, 2.190948157972896659 ) ) ;
#109330 = FILL_AREA_STYLE_COLOUR ( '', #60541 ) ;
#109331 = CARTESIAN_POINT ( 'NONE',  ( 1.834862671528534994, 0.1865727292883790633, 1.917327306167202261 ) ) ;
#109332 = CARTESIAN_POINT ( 'NONE',  ( -9.182950115157607840, 9.607863310639020327, 0.7998128361456462443 ) ) ;
#109333 = CARTESIAN_POINT ( 'NONE',  ( -1.040834085586084257E-14, -7.473374494045017968, -9.579665964948867796 ) ) ;
#109334 = CARTESIAN_POINT ( 'NONE',  ( 0.2333540202161402677, 0.7093705336200817335, -2.128223931541360248 ) ) ;
#109335 = ADVANCED_FACE ( 'NONE', ( #115592 ), #50533, .F. ) ;
#109336 = CARTESIAN_POINT ( 'NONE',  ( 6.109920781252839994, 10.27999134477033216, 1.040834085586084257E-14 ) ) ;
#109337 = CARTESIAN_POINT ( 'NONE',  ( 5.335297142177534369, 6.183267073083954735, -1.199719254218452047 ) ) ;
#109338 = CARTESIAN_POINT ( 'NONE',  ( -6.717748655458910534, -7.473374494057226869, 6.717748655460332508 ) ) ;
#109339 = CARTESIAN_POINT ( 'NONE',  ( 4.394251184604957672, 8.140727125432173139, -0.7216878364870357165 ) ) ;
#109340 = VERTEX_POINT ( 'NONE', #197840 ) ;
#109342 = CARTESIAN_POINT ( 'NONE',  ( 2.684242053459008570, 1.078846248543659403, 1.699430804756915547 ) ) ;
#109341 = CARTESIAN_POINT ( 'NONE',  ( 5.495603940606402560, -1.841430844871448258, 0.006098274996368944698 ) ) ;
#109343 = CARTESIAN_POINT ( 'NONE',  ( 4.148081960540086932, -0.2207414774363871957, -2.287749835899715034 ) ) ;
#109345 = CARTESIAN_POINT ( 'NONE',  ( 3.379601846096703888, -1.794663673993960540, 0.4920686967917423105 ) ) ;
#109344 = CARTESIAN_POINT ( 'NONE',  ( -0.02880301295722554472, 4.079423595021631321, -2.828475351696632778 ) ) ;
#109346 = CARTESIAN_POINT ( 'NONE',  ( 8.039058738260216330, 8.343599714250547805, -0.7998128361456341429 ) ) ;
#109347 = CARTESIAN_POINT ( 'NONE',  ( -0.1290005225502918740, 6.946858002156244716, -2.769053915224591211 ) ) ;
#109348 = CARTESIAN_POINT ( 'NONE',  ( 6.310809538426106258, -0.5167911955388967415, -1.841158844219364044 ) ) ;
#109349 = CARTESIAN_POINT ( 'NONE',  ( -6.320072162264675164, 10.52516795595079557, 0.7998128361456481317 ) ) ;
#109350 = CARTESIAN_POINT ( 'NONE',  ( -6.319508997745553636, 6.545384383557486530, 0.7216878364870257245 ) ) ;
#109351 = CARTESIAN_POINT ( 'NONE',  ( 5.442948297640814559, -1.648798800320664615, -1.285478093666903687 ) ) ;
#109352 = CARTESIAN_POINT ( 'NONE',  ( 6.805829924380114804, 8.002851668940699881, 1.082531754730558626 ) ) ;
#109353 = CARTESIAN_POINT ( 'NONE',  ( -11.01135777277262129, 13.39999999999998259, 1.399999999999998579 ) ) ;
#109354 = DIRECTION ( 'NONE',  ( 0.3162277660168376636, 0.9486832980505138790, 0.000000000000000000 ) ) ;
#109355 = CARTESIAN_POINT ( 'NONE',  ( 5.672382752830540831, -1.089361703149527072, 1.337344134918318606 ) ) ;
#109356 = CARTESIAN_POINT ( 'NONE',  ( -5.063080299699540987, 7.994345218703034384, 1.199719254218464037 ) ) ;
#109357 = CARTESIAN_POINT ( 'NONE',  ( 1.213026639236804316, 1.670944716536880259, 0.4636423645143650241 ) ) ;
#109358 = SURFACE_STYLE_FILL_AREA ( #43241 ) ;
#109359 = CARTESIAN_POINT ( 'NONE',  ( -1.001543065824772872E-14, 5.493750000682816825, 1.732050807568877637 ) ) ;
#109360 = AXIS2_PLACEMENT_3D ( 'NONE', #107082, #176299, #206639 ) ;
#109361 = DIRECTION ( 'NONE',  ( 0.000000000000000000, 0.000000000000000000, -1.000000000000000000 ) ) ;
#109362 = CARTESIAN_POINT ( 'NONE',  ( 5.946172770594575496, -0.9833217254726284162, 1.935730195829394429 ) ) ;
#109363 = CARTESIAN_POINT ( 'NONE',  ( 4.090329635444483358, -1.806102819543849769, -0.2658631594732660530 ) ) ;
#109364 = CARTESIAN_POINT ( 'NONE',  ( 2.026150138982992566, 1.004015975608811173, 1.685199498757394831 ) ) ;
#109365 = LINE ( 'NONE', #206776, #196275 ) ;
#109366 = DIRECTION ( 'NONE',  ( 0.000000000000000000, 1.000000000000000000, 0.000000000000000000 ) ) ;
#109367 = CARTESIAN_POINT ( 'NONE',  ( 6.428537391173986038, 10.65171072301167854, 0.7998128361456462443 ) ) ;
#109368 = CARTESIAN_POINT ( 'NONE',  ( 2.420699464796825850, -0.8139657014685426351, -1.958238820914718792 ) ) ;
#109369 = CARTESIAN_POINT ( 'NONE',  ( -3.389175213736311587, 4.977123720824209840, 1.443375672974064550 ) ) ;
#109370 = SURFACE_SIDE_STYLE ('',( #43252 ) ) ;
#109371 = AXIS2_PLACEMENT_3D ( 'NONE', #149498, #36794, #152690 ) ;
#109372 = CARTESIAN_POINT ( 'NONE',  ( -5.289711001425910553, 6.400709951683444920, -1.138330407662338617 ) ) ;
#109373 = CARTESIAN_POINT ( 'NONE',  ( 0.6200890622066607127, 2.048230590617374336, -0.3001980380039070972 ) ) ;
#109375 = CARTESIAN_POINT ( 'NONE',  ( 0.7500000000000006661, 13.44791666734946389, -1.299038105676657340 ) ) ;
#109374 = CARTESIAN_POINT ( 'NONE',  ( -10.62413147216588527, 4.107683970518822392, 5.580188593819120690 ) ) ;
#109377 = ORIENTED_EDGE ( 'NONE', *, *, #202242, .T. ) ;
#109376 = CARTESIAN_POINT ( 'NONE',  ( 3.229344874888330441, 2.008827177783510720, 0.9482931344305007837 ) ) ;
#109378 = CARTESIAN_POINT ( 'NONE',  ( 0.7394344266866456072, 2.295659475925112769, -0.1205738325454289578 ) ) ;
#109380 = CARTESIAN_POINT ( 'NONE',  ( 6.508646177561060675, 0.6413444998595011493, 1.960425241914983907 ) ) ;
#109379 = CARTESIAN_POINT ( 'NONE',  ( 4.142179624174931796, 4.791296635414242111, 1.199719254218464037 ) ) ;
#109382 = CARTESIAN_POINT ( 'NONE',  ( 1.737499999999999378, -1.166666666666666519, -3.009438278150925683 ) ) ;
#109381 = CARTESIAN_POINT ( 'NONE',  ( 3.542423274920540432, 7.354853930707762721, -1.734723475976807094E-15 ) ) ;
#109383 = ADVANCED_FACE ( 'NONE', ( #181586 ), #14818, .F. ) ;
#109384 = CARTESIAN_POINT ( 'NONE',  ( 0.2329586101569527945, 7.629137130509077380, -2.445728209250570107 ) ) ;
#109385 = CARTESIAN_POINT ( 'NONE',  ( 6.058133912487986272, -1.297239342979487509, 1.306937132449899508 ) ) ;
#109386 = CIRCLE ( 'NONE', #15902, 0.07999999999999946043 ) ;
#109387 = EDGE_CURVE ( 'NONE', #205391, #98224, #149632, .T. ) ;
#109388 = CARTESIAN_POINT ( 'NONE',  ( -0.2104748580754408904, 1.337026610731705700, -2.356057411969681326 ) ) ;
#109389 = CARTESIAN_POINT ( 'NONE',  ( 3.029983902540707152, 0.9595516922606081023, -1.432977992855663185 ) ) ;
#109390 = CARTESIAN_POINT ( 'NONE',  ( 1.710173085450257702, 1.157096902994741772, -1.651345047625000229 ) ) ;
#109391 = CARTESIAN_POINT ( 'NONE',  ( 2.918861131495727790, -1.545587104802835565, -1.701642145805809303 ) ) ;
#109392 = CARTESIAN_POINT ( 'NONE',  ( 2.390224264847177871, -0.9692217175977213550, 2.044435098530998474 ) ) ;
#109393 = CARTESIAN_POINT ( 'NONE',  ( 4.916683514525310272, 1.453009998446822992, -1.524801812277425839 ) ) ;
#109394 = CARTESIAN_POINT ( 'NONE',  ( -5.614485009834902840, 9.564333254867113610, 0.7216878364870267237 ) ) ;
#109395 = ORIENTED_EDGE ( 'NONE', *, *, #49580, .F. ) ;
#109396 = CARTESIAN_POINT ( 'NONE',  ( 3.303702144000867591, -1.767878013958000150, 0.08340844992380143375 ) ) ;
#109398 = CARTESIAN_POINT ( 'NONE',  ( 6.128533286225700039, 0.2205342988230532264, 2.281768524910554596 ) ) ;
#109397 = CARTESIAN_POINT ( 'NONE',  ( 4.217995187182922656, 6.014356699837137832, 1.443375672974058777 ) ) ;
#109399 = CARTESIAN_POINT ( 'NONE',  ( 4.839718430358881385, 1.836437689789902628, 0.1323948491315785347 ) ) ;
#109400 = CARTESIAN_POINT ( 'NONE',  ( -4.924636110261798372, 6.768494766770632332, 1.599625672291267398 ) ) ;
#109401 = CARTESIAN_POINT ( 'NONE',  ( 4.161989969270883272, 7.799479364217271282, 0.7216878364870317197 ) ) ;
#109402 = CARTESIAN_POINT ( 'NONE',  ( 1.499999999999989120, 3.504166666666683749, 0.8660254037844524744 ) ) ;
#109403 = CARTESIAN_POINT ( 'NONE',  ( 4.857479518068650748, 2.167902099161696849, -0.3196092617779102696 ) ) ;
#109404 = CARTESIAN_POINT ( 'NONE',  ( -4.485049888022365927, 4.126979712314507331, 0.7998128361456341429 ) ) ;
#109405 = CARTESIAN_POINT ( 'NONE',  ( -11.41381675112453387, 12.69999999999999929, -3.704697986577184299 ) ) ;
#109406 = CARTESIAN_POINT ( 'NONE',  ( 4.984861949208964305, 1.980195279717174905, 0.6042863919064264122 ) ) ;
#109407 = LINE ( 'NONE', #56317, #66040 ) ;
#109408 =( BOUNDED_CURVE ( )  B_SPLINE_CURVE ( 3, ( #193911, #78031, #74847, #160355 ),
 .UNSPECIFIED., .F., .T. ) 
 B_SPLINE_CURVE_WITH_KNOTS ( ( 4, 4 ),
 ( 4.148111545443840420, 4.712388980384622172 ),
 .UNSPECIFIED. ) 
 CURVE ( )  GEOMETRIC_REPRESENTATION_ITEM ( )  RATIONAL_B_SPLINE_CURVE ( ( 1.000000000000000000, 0.9736414627471743355, 0.9736414627471743355, 1.000000000000000000 ) ) 
 REPRESENTATION_ITEM ( '' )  );
#109409 = CARTESIAN_POINT ( 'NONE',  ( -1.364683531249997417, 5.259375000341425022, 1.214306433183764966E-14 ) ) ;
#109410 = CARTESIAN_POINT ( 'NONE',  ( 3.123571566491334384, -1.856553849623356234, 0.5141669907481066781 ) ) ;
#109411 = CARTESIAN_POINT ( 'NONE',  ( 1.364683531249997417, 10.48437500034139802, 2.602085213965210642E-15 ) ) ;
#109412 = CARTESIAN_POINT ( 'NONE',  ( -2.629918611371007575, 6.012062780000711371, 0.7216878364870317197 ) ) ;
#109413 = CARTESIAN_POINT ( 'NONE',  ( -0.1047794747230318818, -2.156939676625940994, -0.5310815526072456549 ) ) ;
#109414 = ORIENTED_EDGE ( 'NONE', *, *, #61884, .T. ) ;
#109416 = SURFACE_SIDE_STYLE ('',( #125670 ) ) ;
#109415 = CARTESIAN_POINT ( 'NONE',  ( -3.634994582239682526, 6.294558541704648569, 1.082531754730549967 ) ) ;
#109417 = CARTESIAN_POINT ( 'NONE',  ( 3.167801447087334576, 6.847518788243868393, -0.7998128361456291469 ) ) ;
#109418 = FACE_OUTER_BOUND ( 'NONE', #43983, .T. ) ;
#109419 = CARTESIAN_POINT ( 'NONE',  ( 3.946537740505243974, 2.817530495244580102, -0.7749999999999935829 ) ) ;
#109420 = CARTESIAN_POINT ( 'NONE',  ( -6.302510697806719797, 6.525553010488573058, -0.1636245105971004254 ) ) ;
#109421 = CARTESIAN_POINT ( 'NONE',  ( 1.855835942623608181, -0.6640040153468586004, 1.846199708051485588 ) ) ;
#109422 = CARTESIAN_POINT ( 'NONE',  ( 1.364683531249986537, 0.9260416670080896528, 0.7879004041258500513 ) ) ;
#109423 = DIRECTION ( 'NONE',  ( 1.000000000000000000, -0.000000000000000000, -0.000000000000000000 ) ) ;
#109424 = CARTESIAN_POINT ( 'NONE',  ( 6.021922112293466967, 1.933069186966931863, -0.3339256516061983038 ) ) ;
#109425 = CARTESIAN_POINT ( 'NONE',  ( -8.890396042259075315, 11.39521468743417998, -1.599625672291263179 ) ) ;
#109426 = CARTESIAN_POINT ( 'NONE',  ( -6.548225005276122168, 6.741943382351338165, 0.7216878364870317197 ) ) ;
#109427 = CARTESIAN_POINT ( 'NONE',  ( 6.754756207809571755, -1.674487575904315406, 1.366813541845832924 ) ) ;
#109429 = EDGE_LOOP ( 'NONE', ( #82077, #65670, #92246, #120235, #175802, #8517, #183043, #142472, #199707, #34887, #62591, #152036, #140868, #129329, #174008, #205612, #61652, #727, #5557, #57064, #2907, #48961, #43452, #106383, #87678, #176161, #124131, #62352 ) ) ;
#109428 = CARTESIAN_POINT ( 'NONE',  ( -0.4382560683119312572, -5.200000000000007283, -10.99126615174919230 ) ) ;
#109430 = CARTESIAN_POINT ( 'NONE',  ( -1.001543065824772872E-14, 4.821875000341419693, 1.575800808251672791 ) ) ;
#109431 = CARTESIAN_POINT ( 'NONE',  ( 6.678986255646885972, -0.09454399199107686724, -1.969188304806670287 ) ) ;
#109432 = CARTESIAN_POINT ( 'NONE',  ( 6.573613466494099278, 1.281508381366827765, -1.168108599551227478 ) ) ;
#109434 = CARTESIAN_POINT ( 'NONE',  ( 2.736070936638954176, 2.175344985778558726, 0.2654339622269741295 ) ) ;
#109433 = CARTESIAN_POINT ( 'NONE',  ( 0.6801582343749900117, 0.05729166700808169255, -1.178068619123848526 ) ) ;
#109435 = CARTESIAN_POINT ( 'NONE',  ( 4.753107839025799031, -1.856540859070819005, 1.370308287008913606 ) ) ;
#109436 = CARTESIAN_POINT ( 'NONE',  ( 6.098915436037096960, 1.687290577560787375, -1.182889608693861394 ) ) ;
#109437 = CARTESIAN_POINT ( 'NONE',  ( 1.816251609031571457, 1.811968324836669142, 0.6989759121980871903 ) ) ;
#109438 = CARTESIAN_POINT ( 'NONE',  ( -6.209271164934474285, 6.346497235286081562, 1.040834085586084257E-14 ) ) ;
#109439 = PRODUCT_DEFINITION_SHAPE ( 'NONE', 'NONE',  #26565 ) ;
#109440 = CARTESIAN_POINT ( 'NONE',  ( -6.775478006741587400, -7.217909409563576517, -6.775478006741549208 ) ) ;
#109441 = CARTESIAN_POINT ( 'NONE',  ( 5.607717026683647354, 1.607092460389969446, 1.383685132418293495 ) ) ;
#109442 = CARTESIAN_POINT ( 'NONE',  ( 2.672500184003968382, 1.427937546361924381, 1.423961308954827754 ) ) ;
#109443 = CARTESIAN_POINT ( 'NONE',  ( -5.219525951136850139, 7.112532914458205013, -1.443375672974051449 ) ) ;
#109444 = CARTESIAN_POINT ( 'NONE',  ( 11.41381675112453564, 12.56994333910006567, -3.704697986577182522 ) ) ;
#109445 = CARTESIAN_POINT ( 'NONE',  ( 8.561083932025322696, 12.07534945641652158, -1.199719254218446718 ) ) ;
#109446 = CARTESIAN_POINT ( 'NONE',  ( 11.94654170777226021, 12.44825673841064173, -1.134972293687621647 ) ) ;
#109447 = CARTESIAN_POINT ( 'NONE',  ( -5.237192476628793614, 9.332084666034067055, 0.7998128361456291469 ) ) ;
#109450 = AXIS2_PLACEMENT_3D ( 'NONE', #204010, #55657, #186717 ) ;
#109449 = CARTESIAN_POINT ( 'NONE',  ( -4.956387674247580755, 7.940146832334256111, 1.199719254218452935 ) ) ;
#109448 = CARTESIAN_POINT ( 'NONE',  ( -4.745581203565001793, 8.305819929356548670, 0.7838639097331673300 ) ) ;
#109451 = CARTESIAN_POINT ( 'NONE',  ( -4.613268803136618246, 8.378775596900176481, 0.2107346534404584415 ) ) ;
#109452 = EDGE_LOOP ( 'NONE', ( #76823, #119153, #542, #198372 ) ) ;
#109453 = CARTESIAN_POINT ( 'NONE',  ( 5.823136237661057812, -0.05295972098229295016, 2.060385759621866431 ) ) ;
#109454 = CARTESIAN_POINT ( 'NONE',  ( -6.251718229232856139, 8.387033582228697881, -1.443375672974066548 ) ) ;
#109455 = UNCERTAINTY_MEASURE_WITH_UNIT (LENGTH_MEASURE( 1.000000000000000082E-05 ), #90516, 'distance_accuracy_value', 'NONE');
#109456 = CARTESIAN_POINT ( 'NONE',  ( -3.391510981712833939, 7.108513245306943062, 0.7998128361456341429 ) ) ;
#109457 = CARTESIAN_POINT ( 'NONE',  ( -4.328202132483162323, 7.418225535201088405, 1.151854025577046636 ) ) ;
#109458 = CARTESIAN_POINT ( 'NONE',  ( 5.110023566311792997, -0.7249756751233800145, 1.885263354437803240 ) ) ;
#109459 = CARTESIAN_POINT ( 'NONE',  ( -0.7500000000000215383, 1.441666666666688190, 1.299038105676659116 ) ) ;
#109461 = CARTESIAN_POINT ( 'NONE',  ( 8.975134502566660899, 10.53370701015836275, -1.082531754730543083 ) ) ;
#109460 = CARTESIAN_POINT ( 'NONE',  ( -4.817943484809863008, 6.714296380401858499, 1.599625672291263179 ) ) ;
#109462 = CARTESIAN_POINT ( 'NONE',  ( 6.714312387265682247, 8.856450423275211037, 1.599625672291281386 ) ) ;
#109463 = CARTESIAN_POINT ( 'NONE',  ( 3.959881651031765593, 2.045548025627259126, -0.2503382637644557263 ) ) ;
#109464 = CARTESIAN_POINT ( 'NONE',  ( 2.690077459517980163, 1.704938782060089864, 1.076316768488336351 ) ) ;
#109465 = ORIENTED_EDGE ( 'NONE', *, *, #15404, .F. ) ;
#109466 = DIRECTION ( 'NONE',  ( 0.000000000000000000, 1.000000000000000000, -8.546850786086437571E-32 ) ) ;
#109467 = CARTESIAN_POINT ( 'NONE',  ( 5.027376032568989572, 4.759693547618927489, 0.7998128361456341429 ) ) ;
#109469 = ORIENTED_EDGE ( 'NONE', *, *, #114198, .T. ) ;
#109468 = CARTESIAN_POINT ( 'NONE',  ( -0.3088250840613139814, 7.211283896344582445, -2.083830622148103995 ) ) ;
#109470 = CARTESIAN_POINT ( 'NONE',  ( 2.565779641467882399, 1.620934753846922982, -1.198676126143098486 ) ) ;
#109471 = CARTESIAN_POINT ( 'NONE',  ( 1.991909005812149358, -0.4902695928585449892, -1.774584731258487036 ) ) ;
#109472 = CARTESIAN_POINT ( 'NONE',  ( 0.8038796212130067120, 1.889748380504801650, 1.324265523043531845 ) ) ;
#109473 = CARTESIAN_POINT ( 'NONE',  ( 5.248941747146098180, 6.152795455539095570, -1.199719254218452047 ) ) ;
#109474 = CARTESIAN_POINT ( 'NONE',  ( 3.936934155531632396, 0.3128429973590241553, 2.138701728237289768 ) ) ;
#109475 = CARTESIAN_POINT ( 'NONE',  ( 9.745613490124728884, 10.26430391476735338, 0.7998128361456462443 ) ) ;
#109476 = CARTESIAN_POINT ( 'NONE',  ( -7.088215381846223906, 7.164006121775713609, 0.7998128361456341429 ) ) ;
#109477 = CARTESIAN_POINT ( 'NONE',  ( 3.585630231873372598, 1.460649136416993121, -1.774545834528557409 ) ) ;
#109478 = VERTEX_POINT ( 'NONE', #18007 ) ;
#109479 = AXIS2_PLACEMENT_3D ( 'NONE', #71599, #105213, #27130 ) ;
#109480 = CARTESIAN_POINT ( 'NONE',  ( 0.000000000000000000, 4.518459255872631530, 11.92000000000000348 ) ) ;
#109481 = CARTESIAN_POINT ( 'NONE',  ( 0.8306673739700667358, 0.1335802410974036292, 1.865940672528036304 ) ) ;
#109482 = CARTESIAN_POINT ( 'NONE',  ( 5.752796013432011080, -1.554615333184097059, 1.212288997074702834 ) ) ;
#109483 = AXIS2_PLACEMENT_3D ( 'NONE', #3509, #102108, #168179 ) ;
#109485 = CARTESIAN_POINT ( 'NONE',  ( 8.880227426826634129, 11.38335130276301754, 1.443375672974076540 ) ) ;
#109484 = CARTESIAN_POINT ( 'NONE',  ( 0.6823417656249899377, 3.676041667008085767, -1.181850606188754593 ) ) ;
#109487 = CARTESIAN_POINT ( 'NONE',  ( 0.9618826090718561872, 0.4271145061440981272, -2.164990749644220447 ) ) ;
#109486 = CARTESIAN_POINT ( 'NONE',  ( -6.575868197828002693, 7.630599971342813426, 1.199719254218450271 ) ) ;
#109488 = DIRECTION ( 'NONE',  ( -0.000000000000000000, 1.000000000000000000, -0.000000000000000000 ) ) ;
#109489 = CARTESIAN_POINT ( 'NONE',  ( 4.710568305744190276, 7.583081225755162968, 1.199719254218462483 ) ) ;
#109490 = CARTESIAN_POINT ( 'NONE',  ( -4.577849422908604637, 8.492574760035358494, -0.7998128361456281477 ) ) ;
#109491 = CARTESIAN_POINT ( 'NONE',  ( 6.539320575229230492, 2.428701779328062749, 2.485127258459709054 ) ) ;
#109492 = CARTESIAN_POINT ( 'NONE',  ( 5.243030984088811408, -1.691212405323471835, 1.012918505260449464 ) ) ;
#109493 = CARTESIAN_POINT ( 'NONE',  ( 4.037936217472848810, -1.589972691411502659, -1.672771819537349325 ) ) ;
#109494 = CARTESIAN_POINT ( 'NONE',  ( 3.397386871994355850, -1.821155587584430302, 0.9682287363927607471 ) ) ;
#109495 = CARTESIAN_POINT ( 'NONE',  ( 7.293923454472091450, 7.611924906413328529, 0.7216878364870317197 ) ) ;
#109496 = CARTESIAN_POINT ( 'NONE',  ( 6.215487077222150880, 6.216099443039444949, 0.000000000000000000 ) ) ;
#109497 = CARTESIAN_POINT ( 'NONE',  ( 4.441177836928239309, 7.339068688795062911, 1.199719254218452047 ) ) ;
#109498 = CARTESIAN_POINT ( 'NONE',  ( 0.6823417656249882723, 2.488541667008084435, -1.181850606188749264 ) ) ;
#109499 = CARTESIAN_POINT ( 'NONE',  ( -11.07790593930098311, 12.30000000000000071, -0.7000000000000009548 ) ) ;
#109500 = CARTESIAN_POINT ( 'NONE',  ( 6.277061933002785032, 7.385955679000473673, 1.082531754730558626 ) ) ;
#109501 = CARTESIAN_POINT ( 'NONE',  ( 5.002462566363424123, 2.165002515946230499, 0.1647018997421762776 ) ) ;
#109503 = CARTESIAN_POINT ( 'NONE',  ( 3.684953445348177148, 1.336164438771630714, 1.267087564277062484 ) ) ;
#109502 = CARTESIAN_POINT ( 'NONE',  ( -4.636525346193588248, 4.511627113421689650, 0.7216878364870317197 ) ) ;
#109505 = CARTESIAN_POINT ( 'NONE',  ( 11.86239285000045562, 12.29999999999998472, 1.812080536912751061 ) ) ;
#109504 = CARTESIAN_POINT ( 'NONE',  ( -1.833030277982346634, 0.000000000000000000, -2.499999999999998668 ) ) ;
#109506 = CARTESIAN_POINT ( 'NONE',  ( 5.390230798962840630, -0.5317533105795355652, -2.125930911514521959 ) ) ;
#109507 = CARTESIAN_POINT ( 'NONE',  ( 0.000000000000000000, 0.000000000000000000, 0.000000000000000000 ) ) ;
#109508 = CARTESIAN_POINT ( 'NONE',  ( 0.7555949320777423095, -1.911880202960547948, -1.209378468041100607 ) ) ;
#109509 = CARTESIAN_POINT ( 'NONE',  ( -4.074744958279661766, 7.716589449174610316, -0.6783282581392232613 ) ) ;
#109510 = DIRECTION ( 'NONE',  ( 0.5000000000000003331, 0.000000000000000000, 0.8660254037844383745 ) ) ;
#109511 = CARTESIAN_POINT ( 'NONE',  ( 6.148788998471866662, 7.076870205577955986, 1.084632487400632339 ) ) ;
#109512 = CARTESIAN_POINT ( 'NONE',  ( -3.634994581795317536, 7.254927755487573293, 0.000000000000000000 ) ) ;
#109513 = CARTESIAN_POINT ( 'NONE',  ( 4.936577329151614180, 4.931964103531220722, -0.7216878364870458196 ) ) ;
#109514 = CARTESIAN_POINT ( 'NONE',  ( 0.4613126893583847643, 1.751520745650859912, -0.2531317886874852041 ) ) ;
#109515 = AXIS2_PLACEMENT_3D ( 'NONE', #4485, #49025, #19696 ) ;
#109516 = CARTESIAN_POINT ( 'NONE',  ( 5.233069312805943341, 1.860886824452904653, 0.7683393057746935595 ) ) ;
#109517 = CARTESIAN_POINT ( 'NONE',  ( 5.686755365928134687, 8.721966129303114101, 1.199719254218462483 ) ) ;
#109518 = CARTESIAN_POINT ( 'NONE',  ( 4.559663772078708988, 0.4639327178320976630, -2.054050964449795291 ) ) ;
#109519 = CARTESIAN_POINT ( 'NONE',  ( 2.970226572681373689, -1.887729772399210804, -0.3245638568863758455 ) ) ;
#109520 = CARTESIAN_POINT ( 'NONE',  ( 4.207107738942202246, 3.802713871720993399, 1.214306433183764966E-14 ) ) ;
#109521 = CARTESIAN_POINT ( 'NONE',  ( 4.387129405986627262, 0.09430581837475923712, 1.967405897498993195 ) ) ;
#109523 = ADVANCED_FACE ( 'NONE', ( #33215 ), #179487, .T. ) ;
#109522 = CARTESIAN_POINT ( 'NONE',  ( 5.748308766347858700, 0.9917722086787251756, -1.759414076857076514 ) ) ;
#109524 = CARTESIAN_POINT ( 'NONE',  ( 1.551402291579254022, 0.5461136009352780540, -1.789155053659279071 ) ) ;
#109527 = EDGE_LOOP ( 'NONE', ( #166998, #195526 ) ) ;
#109526 = CARTESIAN_POINT ( 'NONE',  ( 1.582132296805271787, 0.9858968508435607125, 1.638552900098678045 ) ) ;
#109525 = CARTESIAN_POINT ( 'NONE',  ( 4.652814366283819503, -1.382804000779764619, 1.030830748262304253 ) ) ;
#109529 = CARTESIAN_POINT ( 'NONE',  ( 3.538314903486612817, 7.071858454135611538, 1.040834085586084257E-14 ) ) ;
#109528 = CARTESIAN_POINT ( 'NONE',  ( 1.858336453454629611, 2.200810804183956026, -0.1644699235988852648 ) ) ;
#109530 = CIRCLE ( 'NONE', #206221, 0.07999999999999989064 ) ;
#109531 = CARTESIAN_POINT ( 'NONE',  ( 1.364683531249990311, 2.696875000341415696, 1.214306433183764966E-14 ) ) ;
#109532 = CARTESIAN_POINT ( 'NONE',  ( 6.320756440275016708, -1.388331291134708767, 1.386421665916007795 ) ) ;
#109534 = EDGE_CURVE ( 'NONE', #39288, #109538, #179518, .T. ) ;
#109533 = CARTESIAN_POINT ( 'NONE',  ( 7.239163954692881653, 10.53310948286200599, -1.199719254218441611 ) ) ;
#109535 = CARTESIAN_POINT ( 'NONE',  ( 11.78331023100045627, 11.29999999999998117, 1.799999999999999600 ) ) ;
#109536 = DIRECTION ( 'NONE',  ( -0.000000000000000000, -1.000000000000000000, -0.000000000000000000 ) ) ;
#109537 = CARTESIAN_POINT ( 'NONE',  ( -0.3396678349899239224, 2.756311866119263154, -2.043018440765232313 ) ) ;
#109538 = VERTEX_POINT ( 'NONE', #79834 ) ;
#109539 = CARTESIAN_POINT ( 'NONE',  ( -10.76345817711984587, -5.427673425445469491, 0.4370932794886463468 ) ) ;
#109540 = ORIENTED_EDGE ( 'NONE', *, *, #107896, .T. ) ;
#109541 = CARTESIAN_POINT ( 'NONE',  ( 2.084514231050747401, 1.193861083872927109, -1.691280048542340708 ) ) ;
#109542 = CARTESIAN_POINT ( 'NONE',  ( -1.500000000000013101, 2.629166666666687746, -0.8660254037844313801 ) ) ;
#109543 = CARTESIAN_POINT ( 'NONE',  ( 5.612185521052973414, 8.634967976948757951, -1.199719254218440723 ) ) ;
#109544 = CARTESIAN_POINT ( 'NONE',  ( -8.213542131780492639, 8.476887330032372603, 1.040834085586084257E-14 ) ) ;
#109545 = CARTESIAN_POINT ( 'NONE',  ( 3.067887898442204442, 6.801229324816399746, 0.7998128361456271485 ) ) ;
#109546 = CARTESIAN_POINT ( 'NONE',  ( 0.3287785284849250034, 1.391158174000119097, -1.464406657780653820 ) ) ;
#109547 = CARTESIAN_POINT ( 'NONE',  ( -3.090895833791289071, 6.549869539491048442, 1.040834085586084257E-14 ) ) ;
#109548 = CARTESIAN_POINT ( 'NONE',  ( -1.402160292154681736E-14, 2.446875000341416584, -1.575800808251660134 ) ) ;
#109550 = CARTESIAN_POINT ( 'NONE',  ( 2.846322183865124700, 5.408127416896231665, -1.199719254218446718 ) ) ;
#109549 = CARTESIAN_POINT ( 'NONE',  ( 0.000000000000000000, -0.5000000000000004441, 0.000000000000000000 ) ) ;
#109551 = CARTESIAN_POINT ( 'NONE',  ( 5.958361200765043719, 1.524811557412728114, 1.319025083221535333 ) ) ;
#109552 = CARTESIAN_POINT ( 'NONE',  ( 4.944510238519550072, -1.383032091829504928, 1.325833103116050626 ) ) ;
#109553 = PRESENTATION_STYLE_ASSIGNMENT (( #143086 ) ) ;
#109554 = CARTESIAN_POINT ( 'NONE',  ( 2.613028500285840661, -0.2118117899099076218, 2.181281865515646068 ) ) ;
#109555 = CARTESIAN_POINT ( 'NONE',  ( -1.500000000000001110, 10.55208333401613530, 0.8660254037844418162 ) ) ;
#109556 = CARTESIAN_POINT ( 'NONE',  ( -0.7500000000000006661, 0.1395833340161536928, -1.299038105676652011 ) ) ;
#109557 = CARTESIAN_POINT ( 'NONE',  ( 5.713144883995101786, 1.643398218655172105, -1.162588118691459949 ) ) ;
#109558 = CARTESIAN_POINT ( 'NONE',  ( 1.793074957647671663, -0.09724762972821224261, -1.910064080951429100 ) ) ;
#109559 = CARTESIAN_POINT ( 'NONE',  ( -6.555530967407501741, 7.606873202518897870, 1.199719254218450271 ) ) ;
#109561 = CARTESIAN_POINT ( 'NONE',  ( 0.06993570063764525946, -0.9480199632962028611, 1.779638758220257522 ) ) ;
#109560 = CARTESIAN_POINT ( 'NONE',  ( -3.795919822146293754, 4.491289883001181593, -1.082531754730549967 ) ) ;
#109562 = CARTESIAN_POINT ( 'NONE',  ( 1.364683531250000303, 10.06770833367473017, -0.7879004041258355073 ) ) ;
#109564 = CARTESIAN_POINT ( 'NONE',  ( -5.121948170912633991, 9.197632976031879792, -0.7998128361456362523 ) ) ;
#109563 = CARTESIAN_POINT ( 'NONE',  ( 3.896100387133538234, -0.6578992572023834029, -1.984587938432079257 ) ) ;
#109566 = ORIENTED_EDGE ( 'NONE', *, *, #135294, .T. ) ;
#109565 = CARTESIAN_POINT ( 'NONE',  ( 1.904884197260014567, 1.431573929998239958, 0.9616530215695131556 ) ) ;
#109567 = CARTESIAN_POINT ( 'NONE',  ( 6.521762860236213655, -0.4636855090699961712, 2.076960040381255812 ) ) ;
#109568 = CARTESIAN_POINT ( 'NONE',  ( 4.476163270806094552, 8.373940915915776273, 0.7998128361456462443 ) ) ;
#109569 = CARTESIAN_POINT ( 'NONE',  ( -0.2233545620225162176, 13.28207115425022877, 1.458379360998039997 ) ) ;
#109570 = CARTESIAN_POINT ( 'NONE',  ( 0.4671467121175364445, 1.705069321186868159, 0.9702857188121425391 ) ) ;
#109571 = CYLINDRICAL_SURFACE ( 'NONE', #102180, 1.250000000000000000 ) ;
#109572 = CARTESIAN_POINT ( 'NONE',  ( 4.632082037363250748, 8.555846143565791095, -0.7998128361456231517 ) ) ;
#109573 = CARTESIAN_POINT ( 'NONE',  ( 4.650083499807244891, 5.295740330745369207, 2.420000000000010587 ) ) ;
#109574 = ORIENTED_EDGE ( 'NONE', *, *, #163044, .T. ) ;
#109575 = CARTESIAN_POINT ( 'NONE',  ( 2.982852160962686128, -1.674641624487639424, -0.6911452858660637188 ) ) ;
#109576 = ORIENTED_EDGE ( 'NONE', *, *, #97896, .T. ) ;
#109577 = CARTESIAN_POINT ( 'NONE',  ( 4.325214697959421706, 5.004837554829479451, 1.199719254218462483 ) ) ;
#109578 = VERTEX_POINT ( 'NONE', #163236 ) ;
#109579 = CARTESIAN_POINT ( 'NONE',  ( 5.574337433874081427, 6.532423756721743580, -1.199719254218452047 ) ) ;
#109580 = CARTESIAN_POINT ( 'NONE',  ( 4.248556108744420357, 1.777317977963272178, 0.3491261437693141123 ) ) ;
#109581 = CARTESIAN_POINT ( 'NONE',  ( 6.539320575229287336, 7.629137130509086262, 2.596737603865982624 ) ) ;
#109582 = CARTESIAN_POINT ( 'NONE',  ( -1.115562610750309283E-14, 9.093750000682799595, 1.500000000000001554 ) ) ;
#109583 = CARTESIAN_POINT ( 'NONE',  ( 4.128212683569056018, 7.424016784313646866, 0.7064205832574363964 ) ) ;
#109584 = CARTESIAN_POINT ( 'NONE',  ( 3.982723974049819482, 1.766592268715084790, 0.5855280163863920695 ) ) ;
#109585 = CARTESIAN_POINT ( 'NONE',  ( 1.370553398973891390, -0.2825970708170088552, -1.894525755544463008 ) ) ;
#109586 = CARTESIAN_POINT ( 'NONE',  ( 0.6920833903016985200, -1.811158644599793810, -0.2285449354127722099 ) ) ;
#109587 = CARTESIAN_POINT ( 'NONE',  ( 1.408835580989207914, 4.237373208279807457, 0.5203893312692566830 ) ) ;
#109588 = CARTESIAN_POINT ( 'NONE',  ( -10.79318656363365569, 4.699712429332246089, -5.142077722257549333 ) ) ;
#109589 = CARTESIAN_POINT ( 'NONE',  ( 5.542547785767838242, 7.428594929708664196, 1.247761615041423244 ) ) ;
#109590 = CARTESIAN_POINT ( 'NONE',  ( 7.322143911241490777, 14.00158514652465591, 10.35507522492528132 ) ) ;
#109591 = LINE ( 'NONE', #126920, #143473 ) ;
#109592 = DIRECTION ( 'NONE',  ( 0.6250000204279239080, -1.312437604053124089E-08, -0.7806247334443706665 ) ) ;
#109593 = CARTESIAN_POINT ( 'NONE',  ( 7.863365906246055914, 10.19701286208565705, -1.443375672974057666 ) ) ;
#109594 = CARTESIAN_POINT ( 'NONE',  ( 5.840667653085179545, -1.920577060998058583, -0.4351772876184378247 ) ) ;
#109595 = CARTESIAN_POINT ( 'NONE',  ( -3.255929445576174697, 6.950334786480840243, -0.7998128361456281477 ) ) ;
#109596 = CARTESIAN_POINT ( 'NONE',  ( 0.000000000000000000, 9.799999999999998934, 0.000000000000000000 ) ) ;
#109597 = B_SPLINE_CURVE_WITH_KNOTS ( 'NONE', 3,
 ( #1442, #67507, #203915, #171442, #88061, #76076 ),
 .UNSPECIFIED., .F., .F.,
 ( 4, 2, 4 ),
 ( 0.001916662113439827810, 0.002237152494173779652, 0.002557642874907731494 ),
 .UNSPECIFIED. ) ;
#109598 = CARTESIAN_POINT ( 'NONE',  ( 0.5157159539815784344, -1.120044586405210207, -1.765097889335610404 ) ) ;
#109599 = CARTESIAN_POINT ( 'NONE',  ( 6.448874621594486989, 10.67543749183559143, 0.7998128361456462443 ) ) ;
#109600 = CARTESIAN_POINT ( 'NONE',  ( 5.579104889113781773, -0.04751220352695872257, -1.925958990430853612 ) ) ;
#109601 = CARTESIAN_POINT ( 'NONE',  ( -5.018489415352746619, 9.006654751220198207, 0.7998128361456481317 ) ) ;
#109602 = CARTESIAN_POINT ( 'NONE',  ( 1.131563826228650038, -1.154680578942975044, -1.414029504508321100 ) ) ;
#109603 = CARTESIAN_POINT ( 'NONE',  ( 2.491098823239074278, -0.3784457004711218042, -2.174036671264235387 ) ) ;
#109604 = EDGE_CURVE ( 'NONE', #85120, #36225, #145943, .T. ) ;
#109605 = CARTESIAN_POINT ( 'NONE',  ( 11.94980361490430099, 12.59667875264130288, 1.099999952233555733 ) ) ;
#109606 =( BOUNDED_CURVE ( )  B_SPLINE_CURVE ( 3, ( #72222, #56003, #10436, #208627 ),
 .UNSPECIFIED., .F., .T. ) 
 B_SPLINE_CURVE_WITH_KNOTS ( ( 4, 4 ),
 ( 1.570796326794897668, 2.415429946053228250 ),
 .UNSPECIFIED. ) 
 CURVE ( )  GEOMETRIC_REPRESENTATION_ITEM ( )  RATIONAL_B_SPLINE_CURVE ( ( 1.000000000000000000, 0.9414278581755111119, 0.9414278581755111119, 1.000000000000000000 ) ) 
 REPRESENTATION_ITEM ( '' )  );
#109607 = CARTESIAN_POINT ( 'NONE',  ( 6.842638217859555283, -1.930751226189564962, -0.3875045943893626887 ) ) ;
#109608 = CARTESIAN_POINT ( 'NONE',  ( 2.981904208038600679, -1.913756795454506721, -0.3294587723015156011 ) ) ;
#109609 = CIRCLE ( 'NONE', #9179, 4.624999999999993783 ) ;
#109610 = EDGE_LOOP ( 'NONE', ( #154860, #198781, #203207, #84593 ) ) ;
#109611 = CARTESIAN_POINT ( 'NONE',  ( 0.5091384654962345380, 2.010518347751136137, 0.1511200514899835312 ) ) ;
#109613 = CARTESIAN_POINT ( 'NONE',  ( 6.948144928891270666, -0.7966579434352799582, 1.680504273975716334 ) ) ;
#109612 = CARTESIAN_POINT ( 'NONE',  ( -5.875479466675803231, 7.948088359245467416, -1.599625672291271394 ) ) ;
#109614 = CARTESIAN_POINT ( 'NONE',  ( 4.224247379109608680, 7.085983154673295203, -1.199719254218452047 ) ) ;
#109615 = LINE ( 'NONE', #175620, #14627 ) ;
#109616 = CARTESIAN_POINT ( 'NONE',  ( 10.18233705906309972, 11.83814697611718714, 1.199719254218450271 ) ) ;
#109617 = CARTESIAN_POINT ( 'NONE',  ( -5.066996723205291708, 6.934582148538044777, 1.599625672291267398 ) ) ;
#109618 = CARTESIAN_POINT ( 'NONE',  ( -5.562588163356775972, 9.711712967216715953, 0.7998128361456291469 ) ) ;
#109619 = CARTESIAN_POINT ( 'NONE',  ( 2.911879292414458309, -1.082406496695037301, -1.905547650945007776 ) ) ;
#109620 = CARTESIAN_POINT ( 'NONE',  ( 3.307826292054301121, 4.882216645528547616, -1.443375672974057666 ) ) ;
#109621 = CARTESIAN_POINT ( 'NONE',  ( -11.33772463945037146, 19.00000000000000000, 3.679999999999999272 ) ) ;
#109622 = LINE ( 'NONE', #207030, #30393 ) ;
#109624 = EDGE_CURVE ( 'NONE', #147312, #12172, #115207, .T. ) ;
#109623 = CARTESIAN_POINT ( 'NONE',  ( 2.385134503015675200, 1.669401249834654433, -0.7394980648879890817 ) ) ;
#109625 = CARTESIAN_POINT ( 'NONE',  ( 4.406036734316882253, 6.163462161501578329, -1.443375672974051449 ) ) ;
#109626 = CARTESIAN_POINT ( 'NONE',  ( -4.451154503988200339, 4.087435097607984957, 1.214306433183764966E-14 ) ) ;
#109627 = CARTESIAN_POINT ( 'NONE',  ( -5.797436685056675643, 7.335035436452395530, -1.304849551618554981 ) ) ;
#109628 = CARTESIAN_POINT ( 'NONE',  ( 0.3870735955438693310, 1.000000000000000888, -11.88799243440807274 ) ) ;
#109629 = CARTESIAN_POINT ( 'NONE',  ( 8.372323551638698902, 9.726464550788689323, 1.199719254218462483 ) ) ;
#109630 = CARTESIAN_POINT ( 'NONE',  ( 0.9614038661405551744, 0.3767496340168969837, -1.889141571593662805 ) ) ;
#109631 = CARTESIAN_POINT ( 'NONE',  ( 5.242999579849755953, -0.2363135928187160284, -1.947375393322479109 ) ) ;
#109632 = CARTESIAN_POINT ( 'NONE',  ( 0.7500000000000006661, 14.83333333333333748, 1.299038105676657340 ) ) ;
#109633 = CARTESIAN_POINT ( 'NONE',  ( -8.050844288416501016, 8.287073179441051707, 1.040834085586084257E-14 ) ) ;
#109634 = CARTESIAN_POINT ( 'NONE',  ( 5.606460214450851964, 6.499623990736163037, 1.199719254218462483 ) ) ;
#109635 = CARTESIAN_POINT ( 'NONE',  ( 4.652002595327206613, 0.8389548150543740812, 2.024815518666116088 ) ) ;
#109636 = AXIS2_PLACEMENT_3D ( 'NONE', #138399, #188189, #204418 ) ;
#109637 = VECTOR ( 'NONE', #203515, 1000.000000000000000 ) ;
#109638 = CARTESIAN_POINT ( 'NONE',  ( 0.000000000000000000, 0.000000000000000000, 0.000000000000000000 ) ) ;
#109639 = CARTESIAN_POINT ( 'NONE',  ( 3.590741003927795827, 2.018730135711533258, 0.4582614309688318177 ) ) ;
#109641 = CARTESIAN_POINT ( 'NONE',  ( -1.364683531250000748, 1.321875000341421469, 0.000000000000000000 ) ) ;
#109640 = FILL_AREA_STYLE ('',( #209167 ) ) ;
#109642 = ORIENTED_EDGE ( 'NONE', *, *, #55681, .F. ) ;
#109643 = CARTESIAN_POINT ( 'NONE',  ( 3.920743334446879835, -1.585418671752996334, -1.664648107385821030 ) ) ;
#109644 = CARTESIAN_POINT ( 'NONE',  ( 7.131225611108088280, 9.342849184424693476, 1.443375672974076540 ) ) ;
#109645 = CARTESIAN_POINT ( 'NONE',  ( 4.258669648468268676, 7.982548666606070320, 0.7216878364870257245 ) ) ;
#109647 = EDGE_CURVE ( 'NONE', #73672, #160219, #208685, .T. ) ;
#109646 = CARTESIAN_POINT ( 'NONE',  ( -11.43204722947019825, 13.65592754026171818, 3.649275849833181429 ) ) ;
#109648 = CARTESIAN_POINT ( 'NONE',  ( -7.273023059088104425, 7.449891421883056530, 0.000000000000000000 ) ) ;
#109649 = CARTESIAN_POINT ( 'NONE',  ( 4.453030731839799472, 0.4239971928432215154, -1.894948383050964580 ) ) ;
#109650 = ORIENTED_EDGE ( 'NONE', *, *, #29015, .F. ) ;
#109651 = CARTESIAN_POINT ( 'NONE',  ( 9.286972035236624734, 11.85788667924133399, -1.443375672974058777 ) ) ;
#109652 = ADVANCED_FACE ( 'NONE', ( #170677 ), #135244, .T. ) ;
#109653 = VERTEX_POINT ( 'NONE', #151246 ) ;
#109654 = CARTESIAN_POINT ( 'NONE',  ( 5.238497809344139000, 1.134185964801931679, -1.539638564045166857 ) ) ;
#109655 = CARTESIAN_POINT ( 'NONE',  ( 5.983370841356476788, 1.591773204597257463, -0.6646525218769030463 ) ) ;
#109656 = CARTESIAN_POINT ( 'NONE',  ( 4.118375227313908482, 1.978554835517082555, 0.3886342876525810119 ) ) ;
#109658 = CARTESIAN_POINT ( 'NONE',  ( -2.862179826260718762, 6.353310540697199471, 0.000000000000000000 ) ) ;
#109657 = CARTESIAN_POINT ( 'NONE',  ( -7.641992139597101108, 12.06740792950531649, 0.7998128361456481317 ) ) ;
#109659 = CARTESIAN_POINT ( 'NONE',  ( -3.285556943750000514, -3.726041666188710799, -1.896917185911906500 ) ) ;
#109661 = CARTESIAN_POINT ( 'NONE',  ( 0.1625042017948316320, -1.577765994087614310, -0.8020051908347087810 ) ) ;
#109660 = CARTESIAN_POINT ( 'NONE',  ( 1.236401392562349155, 0.4093969531599008227, 2.049976805931138735 ) ) ;
#109662 = CARTESIAN_POINT ( 'NONE',  ( 5.994767569012836361, -2.000857541758268354, 0.2496038112331094849 ) ) ;
#109664 = CARTESIAN_POINT ( 'NONE',  ( 3.416269409239420352, 1.454353297360365449, -1.771818544839237175 ) ) ;
#109663 = CARTESIAN_POINT ( 'NONE',  ( 3.400062661977048428, 7.188766548940353829, -1.734723475976807094E-15 ) ) ;
#109665 = CARTESIAN_POINT ( 'NONE',  ( 1.675334203684273771, -0.9328193774022232043, 1.469000774227617434 ) ) ;
#109666 = DIRECTION ( 'NONE',  ( -1.000000000000000000, 0.000000000000000000, 0.000000000000000000 ) ) ;
#109667 = CARTESIAN_POINT ( 'NONE',  ( 0.6140417155099803237, 0.5521904297083098934, -1.643632271941943612 ) ) ;
#109668 = CARTESIAN_POINT ( 'NONE',  ( -1.360316468750062846, 1.401041667008104508, -0.7853790794158941324 ) ) ;
#109669 = CARTESIAN_POINT ( 'NONE',  ( 2.136937089482681795, -0.08731620468203694918, -1.859122327218107218 ) ) ;
#109670 = CARTESIAN_POINT ( 'NONE',  ( 2.102231420249685456, 0.8322404413585123839, -2.005527090382641653 ) ) ;
#109671 = CARTESIAN_POINT ( 'NONE',  ( 3.010954138651841916, 0.05432569772663429358, 2.015980714967258614 ) ) ;
#109672 = CARTESIAN_POINT ( 'NONE',  ( 3.968750000000002665, 0.7852924748297764879, -1.895863743164168724 ) ) ;
#109673 = CARTESIAN_POINT ( 'NONE',  ( 1.499999999999987121, 2.077083334016153415, -0.8660254037844262731 ) ) ;
#109674 = CARTESIAN_POINT ( 'NONE',  ( 6.621714856310891406, -1.867994803139013005, 0.4708039761674199797 ) ) ;
#109675 = CARTESIAN_POINT ( 'NONE',  ( -1.364683531250014514, 14.08854166700806942, -0.7879004041258335089 ) ) ;
#109676 = CARTESIAN_POINT ( 'NONE',  ( 3.340272282456987263, -1.325889367010645969, -1.782164031402436954 ) ) ;
#109677 = ORIENTED_EDGE ( 'NONE', *, *, #53503, .T. ) ;
#109678 = FILL_AREA_STYLE_COLOUR ( '', #137215 ) ;
#109679 = CARTESIAN_POINT ( 'NONE',  ( 9.399880572976245574, 9.860948844760784482, 0.7998128361456462443 ) ) ;
#109680 = CARTESIAN_POINT ( 'NONE',  ( -1.364683531250014514, -0.9697916663252473812, 0.7879004041258379498 ) ) ;
#109681 = CARTESIAN_POINT ( 'NONE',  ( 0.03034698492793227315, -2.177136498186870384, 0.4399771670399817425 ) ) ;
#109682 = CARTESIAN_POINT ( 'NONE',  ( 4.510177812457000002, 1.961482754637720927, -0.04604004567236585910 ) ) ;
#109684 = CARTESIAN_POINT ( 'NONE',  ( -5.531363484695544841, 8.436712584578003771, 1.082531754730548412 ) ) ;
#109683 = CARTESIAN_POINT ( 'NONE',  ( 3.195971524519376494, 4.751719416737803847, -1.599625672291262513 ) ) ;
#109685 = CARTESIAN_POINT ( 'NONE',  ( -1.350180276725266415, 4.245934212466626612, -0.3120814641734330208 ) ) ;
#109686 = CARTESIAN_POINT ( 'NONE',  ( 5.589262808440923713, 1.998987879104210608, -1.059483486058722779 ) ) ;
#109687 = CARTESIAN_POINT ( 'NONE',  ( 2.594246270321644676, 0.9746516854327008650, -1.817902028900773459 ) ) ;
#109688 = CARTESIAN_POINT ( 'NONE',  ( -6.013204822860843457, 6.974159367214481264, -1.199719254218446718 ) ) ;
#109689 = ORIENTED_EDGE ( 'NONE', *, *, #102711, .T. ) ;
#109690 = CARTESIAN_POINT ( 'NONE',  ( -1.201851678989727383E-14, 2.743750000682820378, 1.732050807568877637 ) ) ;
#109691 = CARTESIAN_POINT ( 'NONE',  ( 3.971829172498120286, 1.036919360001643531, 1.556626693588740062 ) ) ;
#109692 = CARTESIAN_POINT ( 'NONE',  ( 2.144752260294139568, 0.7423094788623717522, 1.567400511497107018 ) ) ;
#109693 = CARTESIAN_POINT ( 'NONE',  ( 6.005464345382193869, -2.175231771021503668, 0.2666438670960933344 ) ) ;
#109694 = CARTESIAN_POINT ( 'NONE',  ( 1.044295067165665669, 0.8929887407379886177, -2.018210024696056148 ) ) ;
#109695 = CARTESIAN_POINT ( 'NONE',  ( 3.625982885822197410, -1.285997354380935098, -1.737435825693343094 ) ) ;
#109696 = CARTESIAN_POINT ( 'NONE',  ( 6.052673674419667194, -1.666704710846309112, -0.9964068823852706425 ) ) ;
#109697 = STYLED_ITEM ( 'NONE', ( #102386 ), #143536 ) ;
#109698 = CARTESIAN_POINT ( 'NONE',  ( 8.917979296484501717, 14.68769155229934142, 8.032863906691817490 ) ) ;
#109699 = CARTESIAN_POINT ( 'NONE',  ( -4.318600669050631780, 4.999583595936801572, -2.500000000000000444 ) ) ;
#109700 = CARTESIAN_POINT ( 'NONE',  ( 0.6801582343749865700, 2.307291667008083635, -1.178068619123879834 ) ) ;
#109701 = CYLINDRICAL_SURFACE ( 'NONE', #145356, 0.2500000000000574540 ) ;
#109702 = CARTESIAN_POINT ( 'NONE',  ( -7.967387826325084355, 12.44703623068796361, 0.7998128361456481317 ) ) ;
#109703 = CARTESIAN_POINT ( 'NONE',  ( 6.795661308947685164, 8.951357498570873261, -1.599625672291262513 ) ) ;
#109704 = CARTESIAN_POINT ( 'NONE',  ( -1.499999999999946709, 7.750000000000000000, 15.75000000000000711 ) ) ;
#109705 = CARTESIAN_POINT ( 'NONE',  ( 3.738726038629454074, 0.2694068579384528150, 1.805578518607708016 ) ) ;
#109706 = ADVANCED_FACE ( 'NONE', ( #187988 ), #123107, .T. ) ;
#109707 = CARTESIAN_POINT ( 'NONE',  ( 1.975870009618452050, 2.111717515986545113, -0.6407313945460398896 ) ) ;
#109708 = ORIENTED_EDGE ( 'NONE', *, *, #32460, .F. ) ;
#109709 = CARTESIAN_POINT ( 'NONE',  ( -5.275531169048922386, 5.327410250078064458, -0.7216878364870338292 ) ) ;
#109710 = CARTESIAN_POINT ( 'NONE',  ( 3.285556943749998737, -3.142708332855375986, -1.896917185911906500 ) ) ;
#109711 = CARTESIAN_POINT ( 'NONE',  ( -6.995117189646935962, 10.24838825697502109, 1.199719254218453823 ) ) ;
#109712 = CARTESIAN_POINT ( 'NONE',  ( 0.8967469923133252196, -1.971478154887895684, -0.4383870506769834141 ) ) ;
#109713 = CARTESIAN_POINT ( 'NONE',  ( 0.9617728337494994006, -1.673954878106189703, -1.301583125534570673 ) ) ;
#109714 = CARTESIAN_POINT ( 'NONE',  ( 0.000000000000000000, 9.001999999999998892, 0.000000000000000000 ) ) ;
#109715 = CARTESIAN_POINT ( 'NONE',  ( -6.310394152517827315, 6.326824364217716656, 0.7998128361456281477 ) ) ;
#109716 = CARTESIAN_POINT ( 'NONE',  ( 2.412761291957177701, -1.442071615443579091, 1.176286876380010726 ) ) ;
#109717 = CARTESIAN_POINT ( 'NONE',  ( 2.706824224222692088, 6.309712028235118453, 0.7998128361456362523 ) ) ;
#109718 = CARTESIAN_POINT ( 'NONE',  ( 6.117814597332064785, 0.2004318333163370436, 2.006446488866588496 ) ) ;
#109719 = ORIENTED_EDGE ( 'NONE', *, *, #125104, .T. ) ;
#109720 = CARTESIAN_POINT ( 'NONE',  ( -9.267161690140662600, 10.77044237904097734, -1.199719254218441611 ) ) ;
#109721 = CARTESIAN_POINT ( 'NONE',  ( 3.879382553896340013, 1.718498013671100777, -0.6167319420108534622 ) ) ;
#109724 = VERTEX_POINT ( 'NONE', #185845 ) ;
#109723 = CARTESIAN_POINT ( 'NONE',  ( -4.976004696740268685, 6.814476922186354813, -1.450531527366223372 ) ) ;
#109722 = CARTESIAN_POINT ( 'NONE',  ( -3.467853430045390706, 7.267855778353407459, 0.7998128361456352531 ) ) ;
#109725 = CARTESIAN_POINT ( 'NONE',  ( 6.053423048675670159, 7.145495228771222784, -1.160209803801291795 ) ) ;
#109726 = CARTESIAN_POINT ( 'NONE',  ( 6.485703859413265882, 1.880147802650249611, 0.7282652505391642439 ) ) ;
#109727 = CARTESIAN_POINT ( 'NONE',  ( 6.369096972855497363, 1.760372669148374758, -0.5393517311068628528 ) ) ;
#109728 = CARTESIAN_POINT ( 'NONE',  ( 2.972313222866368676, 6.545497292499366182, 0.5012468031770876964 ) ) ;
#109729 = CARTESIAN_POINT ( 'NONE',  ( 4.196143101376831552, -0.8852276965729001246, 2.131346054819768909 ) ) ;
#109730 = CARTESIAN_POINT ( 'NONE',  ( 4.908934136599710563, 7.884784371745123366, 1.199719254218451159 ) ) ;
#109731 = CARTESIAN_POINT ( 'NONE',  ( 6.749309733681256418, -1.731629633356733589, -1.293610171197785652 ) ) ;
#109732 = CARTESIAN_POINT ( 'NONE',  ( 6.120616281565444794, 9.228137197546649517, -1.199719254218440723 ) ) ;
#109733 = CARTESIAN_POINT ( 'NONE',  ( 1.892034919678585281, -0.5197426219408564085, -1.871140422112322232 ) ) ;
#109734 = CARTESIAN_POINT ( 'NONE',  ( 5.255319057710332586, -2.280117823540278366, -0.2889680969316887893 ) ) ;
#109735 = CARTESIAN_POINT ( 'NONE',  ( 0.000000000000000000, 1.899999999999999023, 0.000000000000000000 ) ) ;
#109736 = CARTESIAN_POINT ( 'NONE',  ( -7.774674742793745708, 8.035151719539642912, 0.7998128361456341429 ) ) ;
#109737 = CARTESIAN_POINT ( 'NONE',  ( 4.082764389539480732, -0.1829629792115642917, -1.861669828791753467 ) ) ;
#109740 = CARTESIAN_POINT ( 'NONE',  ( -5.123001941117347080, 7.070197912760590064, 1.599625672291263179 ) ) ;
#109739 = CARTESIAN_POINT ( 'NONE',  ( -1.500000000000013101, 1.660416667349487119, -0.8660254037844313801 ) ) ;
#109738 = CARTESIAN_POINT ( 'NONE',  ( 2.373185085050379506, -1.665764800640230803, -0.9392108107411781814 ) ) ;
#109741 = CARTESIAN_POINT ( 'NONE',  ( 4.108205984530819421, -2.201057848371779535, 0.1611738814469021175 ) ) ;
#109742 = CARTESIAN_POINT ( 'NONE',  ( 1.224999999999949241, 0.4583333340161501734, -0.7072540797573277915 ) ) ;
#109743 = CARTESIAN_POINT ( 'NONE',  ( 6.983263157960398537, 3.691045885609476773, 2.560325512483021981 ) ) ;
#109744 = CARTESIAN_POINT ( 'NONE',  ( -0.2108831679770924727, 4.091978752061476321, -2.452067053820900622 ) ) ;
#109745 = CARTESIAN_POINT ( 'NONE',  ( 5.194182247366869731, 7.153241603385088965, 1.443375672974064550 ) ) ;
#109746 = CARTESIAN_POINT ( 'NONE',  ( -5.682275777458886346, 7.722684055159061423, 1.443375672974058777 ) ) ;
#109747 = CARTESIAN_POINT ( 'NONE',  ( 1.880087831454971603, -1.058004756265405799, 1.663231189906771990 ) ) ;
#109748 = CARTESIAN_POINT ( 'NONE',  ( 2.520946605012349018, 1.507388781920895759, -1.747272692061818011 ) ) ;
#109749 = CARTESIAN_POINT ( 'NONE',  ( 2.875390130891414042, -0.1950805366632331617, 1.952157403750237163 ) ) ;
#109750 = DIRECTION ( 'NONE',  ( -1.000000000000000000, 7.387867266669436732E-31, -0.000000000000000000 ) ) ;
#109751 = CARTESIAN_POINT ( 'NONE',  ( 6.244999159755385776, -0.2970413431409227312, -2.040939473721150144 ) ) ;
#109752 = CARTESIAN_POINT ( 'NONE',  ( 3.795919822146273326, 5.451659097302528068, -1.443375672974051449 ) ) ;
#109753 = CARTESIAN_POINT ( 'NONE',  ( 3.889861467948489082, -2.010801299972611478, 0.1531677096566556595 ) ) ;
#109754 = CARTESIAN_POINT ( 'NONE',  ( 3.542423274920540432, 7.354853930707762721, -1.734723475976807094E-15 ) ) ;
#109755 = ORIENTED_EDGE ( 'NONE', *, *, #3537, .F. ) ;
#109756 = CARTESIAN_POINT ( 'NONE',  ( -4.874313559192080092, 4.961021341527962036, 0.5169845646830675268 ) ) ;
#109757 = CARTESIAN_POINT ( 'NONE',  ( 0.000000000000000000, 15.50000000000019362, 0.000000000000000000 ) ) ;
#109758 = CARTESIAN_POINT ( 'NONE',  ( -3.023105066167347310, 5.702484939155337607, 2.500000000000011102 ) ) ;
#109759 = CARTESIAN_POINT ( 'NONE',  ( 9.748476143425788720, 11.33197590787365172, -1.199719254218440723 ) ) ;
#109761 = AXIS2_PLACEMENT_3D ( 'NONE', #160173, #141836, #60530 ) ;
#109760 = CARTESIAN_POINT ( 'NONE',  ( 2.430757386254971841, -1.338474561058100143, 1.709278666203792652 ) ) ;
#109762 = LINE ( 'NONE', #144372, #41262 ) ;
#109763 = CARTESIAN_POINT ( 'NONE',  ( -4.369858682569394581, 14.55265096709559280, -11.13738628252537310 ) ) ;
#109764 = CARTESIAN_POINT ( 'NONE',  ( -11.88237951145550042, 9.843193473787149372, -0.9087114598430712231 ) ) ;
#109765 = CARTESIAN_POINT ( 'NONE',  ( 2.881944908259078453, -0.9649329312324153030, 1.602325162460143559 ) ) ;
#109766 = CARTESIAN_POINT ( 'NONE',  ( 6.134075720976177593, 1.071308383804179476, -1.877395391766012445 ) ) ;
#109767 = EDGE_CURVE ( 'NONE', #95692, #45033, #153174, .T. ) ;
#109769 = CARTESIAN_POINT ( 'NONE',  ( 6.727182134110203826, 7.053687134213418197, 2.309100590371661710 ) ) ;
#109768 = CARTESIAN_POINT ( 'NONE',  ( -11.33772463945037146, 13.50902469614650414, -3.600000000000000977 ) ) ;
#109770 = CARTESIAN_POINT ( 'NONE',  ( -1.364683531250014514, 0.9885416670080898749, -0.7879004041258289570 ) ) ;
#109771 = CARTESIAN_POINT ( 'NONE',  ( -1.364417678870916806, 4.013935251703865781, 0.6242711042719457648 ) ) ;
#109772 = CARTESIAN_POINT ( 'NONE',  ( 1.805181101471531546, 1.663141274854248230, -0.9436981260437929953 ) ) ;
#109773 = CARTESIAN_POINT ( 'NONE',  ( 3.959615635602866668, 1.756445048235187212, -0.2166398133998989062 ) ) ;
#109774 = CARTESIAN_POINT ( 'NONE',  ( 2.068876254944008508, -1.477226179422253871, 1.214308343151893510 ) ) ;
#109775 = CARTESIAN_POINT ( 'NONE',  ( -6.078132937628113908, 5.985576603521232109, 1.040834085586084257E-14 ) ) ;
#109776 = CARTESIAN_POINT ( 'NONE',  ( 0.1279635871501626776, 1.910768599467532081, 0.1380287717926073077 ) ) ;
#109777 = CARTESIAN_POINT ( 'NONE',  ( 1.499999999999985123, -0.7041666666666481778, -0.8660254037844323793 ) ) ;
#109778 = CARTESIAN_POINT ( 'NONE',  ( 1.328672132201724532, -1.314895749051579132, 1.599177317581280455 ) ) ;
#109779 = CARTESIAN_POINT ( 'NONE',  ( 0.7499999999999920064, 5.483333333333353821, 1.299038105676669330 ) ) ;
#109780 = ADVANCED_FACE ( 'NONE', ( #73159 ), #180846, .T. ) ;
#109781 = CARTESIAN_POINT ( 'NONE',  ( 5.225416543158964977, -1.776039340814106637, 0.5876355328483380269 ) ) ;
#109782 = CARTESIAN_POINT ( 'NONE',  ( 1.347985785199314668, 1.823511463271022093, 0.09156768404049858701 ) ) ;
#109784 = CARTESIAN_POINT ( 'NONE',  ( 4.909045613421183063, 8.010784895652180992, 0.9812996480243344477 ) ) ;
#109783 = CARTESIAN_POINT ( 'NONE',  ( 5.531908139154323223, -1.397534428995873546, -1.707979418440738195 ) ) ;
#109785 = CARTESIAN_POINT ( 'NONE',  ( -0.6823417656249969321, 5.530208333674756283, -1.181850606188749264 ) ) ;
#109786 = CARTESIAN_POINT ( 'NONE',  ( 2.734894939886590937, -1.973151212864039605, -0.6010335745895727388 ) ) ;
#109787 = ADVANCED_FACE ( 'NONE', ( #21197 ), #135006, .T. ) ;
#109788 = CARTESIAN_POINT ( 'NONE',  ( -8.389798128758148010, 8.682519326506312751, 0.7998128361456462443 ) ) ;
#109789 = PLANE ( 'NONE',  #57458 ) ;
#109790 = CARTESIAN_POINT ( 'NONE',  ( 9.887974103068218668, 10.43039129653476493, 0.7998128361456462443 ) ) ;
#109791 = CARTESIAN_POINT ( 'NONE',  ( 1.350180276725264639, 3.454065787533412646, -0.3120814641734592776 ) ) ;
#109792 = CARTESIAN_POINT ( 'NONE',  ( 0.5796411875719498230, 2.017120475678677582, -0.7774783797904263327 ) ) ;
#109793 = CARTESIAN_POINT ( 'NONE',  ( 5.481239241674765950, 9.616805891921051952, -0.7998128361456481317 ) ) ;
#109794 = AXIS2_PLACEMENT_3D ( 'NONE', #165488, #98363, #196921 ) ;
#109795 = ORIENTED_EDGE ( 'NONE', *, *, #93697, .F. ) ;
#109796 = CARTESIAN_POINT ( 'NONE',  ( 5.371561628297467195, -0.3073141173523045167, 2.047320497149993646 ) ) ;
#109797 = CARTESIAN_POINT ( 'NONE',  ( -0.6823417656250246877, 0.1135416670080893753, 1.181850606188755259 ) ) ;
#109798 = CARTESIAN_POINT ( 'NONE',  ( 2.987745815084281276, 1.526290923294726820, 1.530918043534036599 ) ) ;
#109799 = CARTESIAN_POINT ( 'NONE',  ( -4.756313517479579644, 8.198030745052275137, 0.7332552394410801755 ) ) ;
#109800 = CARTESIAN_POINT ( 'NONE',  ( 3.633467297704314980, -0.1462457305761339643, 2.014424004083538833 ) ) ;
#109801 = CARTESIAN_POINT ( 'NONE',  ( 6.720655732516649827, 0.5547967289194677409, 2.325046546815363602 ) ) ;
#109803 = CARTESIAN_POINT ( 'NONE',  ( 7.998947442382716488, 9.394822106610419610, -1.082531754730543083 ) ) ;
#109802 = CARTESIAN_POINT ( 'NONE',  ( 1.737499999999999378, -1.866666666666665808, -3.009438278150925683 ) ) ;
#109804 = CARTESIAN_POINT ( 'NONE',  ( -5.582925393777276035, 9.735439736040634173, 0.7998128361456291469 ) ) ;
#109805 = CARTESIAN_POINT ( 'NONE',  ( 1.780482797753998092, -0.5424726148271253878, -1.942096288550937411 ) ) ;
#109807 = CARTESIAN_POINT ( 'NONE',  ( 6.444889499930222421, -1.758869480593090673, -1.307235502039267860 ) ) ;
#109806 = CARTESIAN_POINT ( 'NONE',  ( -3.716906668440817185, 7.488141546489591072, 0.7998128361456341429 ) ) ;
#109808 = CARTESIAN_POINT ( 'NONE',  ( -1.001543065824772872E-14, 5.243750000682815937, 1.732050807568877637 ) ) ;
#109809 = CARTESIAN_POINT ( 'NONE',  ( 4.535362393419643645, -0.08824616237496610283, 1.910463848342446980 ) ) ;
#109810 = CARTESIAN_POINT ( 'NONE',  ( -11.94980361723156292, 12.59761943414563312, 1.099999926404457984 ) ) ;
#109811 = CARTESIAN_POINT ( 'NONE',  ( 6.127922243252466039, 6.251590159990418449, 1.040834085586084257E-14 ) ) ;
#109813 = CARTESIAN_POINT ( 'NONE',  ( 3.567982607561688280, -0.9913820634350967165, 1.755780237201590488 ) ) ;
#109812 = CARTESIAN_POINT ( 'NONE',  ( -9.124274191872640216, 10.70770331434866485, -1.082531754730537976 ) ) ;
#109814 = CARTESIAN_POINT ( 'NONE',  ( 0.6823417656249934904, 13.25520833367473195, 1.181850606188764807 ) ) ;
#109815 = CARTESIAN_POINT ( 'NONE',  ( 5.649328262929842914, -1.362134112713381029, -1.057878908126141715 ) ) ;
#109816 = CARTESIAN_POINT ( 'NONE',  ( 6.526270840131753737, 8.707344961610770540, -1.599625672291283607 ) ) ;
#109817 = CARTESIAN_POINT ( 'NONE',  ( 9.327646496521982300, 11.90534021740758064, -1.443375672974057666 ) ) ;
#109818 = CARTESIAN_POINT ( 'NONE',  ( 0.000000000000000000, 8.500000000000000000, 0.000000000000000000 ) ) ;
#109819 = CARTESIAN_POINT ( 'NONE',  ( 3.954256261376987602, 0.6707706173689140794, 1.746330409709492937 ) ) ;
#109820 = DIRECTION ( 'NONE',  ( 0.000000000000000000, 0.000000000000000000, -1.000000000000000000 ) ) ;
#109821 = AXIS2_PLACEMENT_3D ( 'NONE', #111887, #124946, #65941 ) ;
#109822 = CARTESIAN_POINT ( 'NONE',  ( 0.9716355300813659390, -0.3074278181635254903, 2.047203142020392441 ) ) ;
#109823 = CARTESIAN_POINT ( 'NONE',  ( 1.734723475976807094E-15, -7.105553651663779391, 0.000000000000000000 ) ) ;
#109824 = ORIENTED_EDGE ( 'NONE', *, *, #58248, .T. ) ;
#109825 = CARTESIAN_POINT ( 'NONE',  ( 6.445981706654077215, -1.189238676736432465, -1.366527308926633211 ) ) ;
#109826 = CARTESIAN_POINT ( 'NONE',  ( 4.523580528814945545, 5.306540700819438960, 1.199719254218452047 ) ) ;
#109827 =( LENGTH_UNIT ( ) NAMED_UNIT ( * ) SI_UNIT ( .MILLI., .METRE. ) );
#109828 = CARTESIAN_POINT ( 'NONE',  ( 0.2635251908490592876, 0.5682291949154983923, -1.720254828205844966 ) ) ;
#109829 = CARTESIAN_POINT ( 'NONE',  ( 6.509323147892504657, 6.766834225395614411, 0.000000000000000000 ) ) ;
#109830 = CARTESIAN_POINT ( 'NONE',  ( 1.607015867998825343, 0.9165151389911689872, 1.199999999999999734 ) ) ;
#109831 = VERTEX_POINT ( 'NONE', #137128 ) ;
#109832 = TOROIDAL_SURFACE ( 'NONE', #33526, 0.8300000000000010703, 0.08000000000000000167 ) ;
#109834 = CARTESIAN_POINT ( 'NONE',  ( 6.753933077901968396, 11.03133902419432566, 0.7998128361456462443 ) ) ;
#109833 = CARTESIAN_POINT ( 'NONE',  ( 0.8538673084422104820, -0.7095216264049221122, 1.829241926910141203 ) ) ;
#109835 = CARTESIAN_POINT ( 'NONE',  ( 4.868704338522531039, -0.2386889102116992178, -1.900620109961237203 ) ) ;
#109836 = CARTESIAN_POINT ( 'NONE',  ( -6.482157434489847603, 6.770256554395555959, 0.2388210531332583819 ) ) ;
#109837 = CARTESIAN_POINT ( 'NONE',  ( 4.365362273920238678, 7.076377838673507448, 1.082531754730558626 ) ) ;
#109838 = CARTESIAN_POINT ( 'NONE',  ( -7.863365906246054138, 11.15738207638699464, -1.082531754730543971 ) ) ;
#109839 = AXIS2_PLACEMENT_3D ( 'NONE', #186274, #85584, #150609 ) ;
#109840 = CARTESIAN_POINT ( 'NONE',  ( 1.920999885407469243, 2.016935458891587096, 0.7782144962657986387 ) ) ;
#109841 = CARTESIAN_POINT ( 'NONE',  ( -4.309512724297390740, 6.121127159803966933, 1.599625672291270506 ) ) ;
#109842 = CARTESIAN_POINT ( 'NONE',  ( 7.024532985656136930, 8.328281583754568729, 1.082531754730549967 ) ) ;
#109843 = CARTESIAN_POINT ( 'NONE',  ( -3.898132859128961236, 4.506575409527250997, -1.199719254218452047 ) ) ;
#109844 = CARTESIAN_POINT ( 'NONE',  ( 4.875911338656576888, 1.051942333337583468, 1.491839654383666947 ) ) ;
#109845 = EDGE_CURVE ( 'NONE', #179060, #81951, #56934, .T. ) ;
#109846 = CARTESIAN_POINT ( 'NONE',  ( 11.18441447305199077, 7.671075215653008428, 3.641562284844301889 ) ) ;
#109847 = CARTESIAN_POINT ( 'NONE',  ( 0.7726555735236986244, -1.854786837065467653, -0.6681536526091761408 ) ) ;
#109848 = CARTESIAN_POINT ( 'NONE',  ( 3.867365959033176814, -1.592763314076732106, -1.058159689705892692 ) ) ;
#109849 = ORIENTED_EDGE ( 'NONE', *, *, #147025, .T. ) ;
#109850 = CARTESIAN_POINT ( 'NONE',  ( 10.38614328979769041, 3.507114751586604129, 5.996442624206595795 ) ) ;
#109851 = CARTESIAN_POINT ( 'NONE',  ( 3.666418788940009943, -0.7958718277518551654, -1.801768233320384605 ) ) ;
#109852 = VERTEX_POINT ( 'NONE', #189063 ) ;
#109853 = CARTESIAN_POINT ( 'NONE',  ( 5.864781425808283544, 0.1387459415673809593, -1.937151248970377271 ) ) ;
#109854 = ORIENTED_EDGE ( 'NONE', *, *, #122294, .T. ) ;
#109855 = CARTESIAN_POINT ( 'NONE',  ( -5.641074431737709283, 8.738948049406083385, -1.199719254218452047 ) ) ;
#109857 = CARTESIAN_POINT ( 'NONE',  ( 6.504144398916748671, -0.9053081408615070158, 1.915699539216948688 ) ) ;
#109856 = CARTESIAN_POINT ( 'NONE',  ( -5.743814354044916470, 6.730146830254374990, -1.199719254218453823 ) ) ;
#109858 = CARTESIAN_POINT ( 'NONE',  ( 5.953438849732186178, 8.999410187112612647, -1.082531754730548412 ) ) ;
#109859 = CARTESIAN_POINT ( 'NONE',  ( 4.283787348595206268, 1.854039900284172315, -0.4678174759695231666 ) ) ;
#109860 = DIRECTION ( 'NONE',  ( 0.000000000000000000, 1.000000000000000000, 0.000000000000000000 ) ) ;
#109861 = CARTESIAN_POINT ( 'NONE',  ( 4.593150236022219428E-15, -8.011313137147251240, -11.00000000000000178 ) ) ;
#109862 = FILL_AREA_STYLE_COLOUR ( '', #23612 ) ;
#109863 = CARTESIAN_POINT ( 'NONE',  ( 5.110025693318159590, -0.7223781944584523051, 1.879196401790662607 ) ) ;
#109864 = CARTESIAN_POINT ( 'NONE',  ( 11.86145016429273191, 12.69999999999999929, 1.099999999999996758 ) ) ;
#109866 = CARTESIAN_POINT ( 'NONE',  ( 5.630092293170263495, 2.014432788975322630, 0.09412139267171715229 ) ) ;
#109865 = CARTESIAN_POINT ( 'NONE',  ( 6.656878040733529289, -1.407521694628325770, 1.162499734694094844 ) ) ;
#109867 = DIRECTION ( 'NONE',  ( 3.347138415753902517E-16, 0.6000000000000018652, 0.7999999999999984901 ) ) ;
#109868 = CARTESIAN_POINT ( 'NONE',  ( 1.398975865466948632, 0.4019745351953528112, 2.030794141931663521 ) ) ;
#109869 = CARTESIAN_POINT ( 'NONE',  ( -8.839552966430023417, 9.415159337030921449, -0.7216878364870267237 ) ) ;
#109870 = CARTESIAN_POINT ( 'NONE',  ( -5.163927922758308142, 7.774463771048841565, -1.174891720174384480 ) ) ;
#109871 = CARTESIAN_POINT ( 'NONE',  ( 8.014278199453780616, 8.522615118883788199, 0.000000000000000000 ) ) ;
#109872 = CARTESIAN_POINT ( 'NONE',  ( 1.642778471875000035, -3.026041666188708401, -2.845375778867859751 ) ) ;
#109873 = CARTESIAN_POINT ( 'NONE',  ( 5.961834861707224320, 7.978559976790334574, -1.599625672291262513 ) ) ;
#109874 = CARTESIAN_POINT ( 'NONE',  ( -7.334597915313094241, 9.580116872663850813, 1.040834085586084257E-14 ) ) ;
#109875 = CARTESIAN_POINT ( 'NONE',  ( 4.231553341240963384, 7.950912974840849579, -0.7216878364870357165 ) ) ;
#109876 = DIRECTION ( 'NONE',  ( 0.000000000000000000, -1.000000000000000000, 0.000000000000000000 ) ) ;
#109877 = CARTESIAN_POINT ( 'NONE',  ( -0.6823417656250039265, 11.38020833367473017, -1.181850606188755259 ) ) ;
#109878 = CARTESIAN_POINT ( 'NONE',  ( -3.490334480514268645, 6.159475096320226939, -1.199719254218452935 ) ) ;
#109880 = CARTESIAN_POINT ( 'NONE',  ( -6.119526231721793330, 8.232809585132461194, 1.599625672291263179 ) ) ;
#109879 = SURFACE_STYLE_FILL_AREA ( #192100 ) ;
#109881 = CARTESIAN_POINT ( 'NONE',  ( 4.043420308529748652, -1.281227996783333989, 1.168826672502675912 ) ) ;
#109882 = CARTESIAN_POINT ( 'NONE',  ( -3.795392936821753604, 6.515376628678959392, -1.199719254218452047 ) ) ;
#109883 = CARTESIAN_POINT ( 'NONE',  ( 2.975506508543227291, -0.2074491501150333705, 2.059866449969804503 ) ) ;
#109884 = CARTESIAN_POINT ( 'NONE',  ( 3.058335788041772307, -1.258934183635691095, 1.702155058717010672 ) ) ;
#109885 = CARTESIAN_POINT ( 'NONE',  ( 8.911787042884274257, 9.291506392986812912, 0.7998128361456462443 ) ) ;
#109886 = CARTESIAN_POINT ( 'NONE',  ( 0.6823417656249899377, 3.926041667008085767, -1.181850606188754593 ) ) ;
#109887 = CARTESIAN_POINT ( 'NONE',  ( 0.5144232481557647896, 0.7485027850700550767, 1.821871385004094845 ) ) ;
#109888 = CARTESIAN_POINT ( 'NONE',  ( 5.639836874842681702, 6.325236607244836051, 1.140081021588116084 ) ) ;
#109889 = CARTESIAN_POINT ( 'NONE',  ( 3.036663219780971978, 6.486598156479028709, -0.7216878364870267237 ) ) ;
#109891 = CARTESIAN_POINT ( 'NONE',  ( 0.000000000000000000, 4.000000000000003553, 0.000000000000000000 ) ) ;
#109890 = CARTESIAN_POINT ( 'NONE',  ( 1.001543065824772753E-15, -2.012499999999999289, 4.012584370867899430 ) ) ;
#109892 = CARTESIAN_POINT ( 'NONE',  ( 3.627152717534872561, -2.118219197452147373, 0.8765883884584676489 ) ) ;
#109894 = ADVANCED_FACE ( 'NONE', ( #118792 ), #86232, .T. ) ;
#109893 = CARTESIAN_POINT ( 'NONE',  ( 1.101864800459760207, -1.825872481749410525, -0.002338443969775172437 ) ) ;
#109895 = CARTESIAN_POINT ( 'NONE',  ( 3.779479514802902340, 0.2291398179169491789, -1.898525689255560422 ) ) ;
#109896 = CARTESIAN_POINT ( 'NONE',  ( 5.611095471209277541, 7.639640364534566075, 1.599625672291268286 ) ) ;
#109897 = CARTESIAN_POINT ( 'NONE',  ( 7.578644679914718019, 7.944099669429731669, 0.7216878364870317197 ) ) ;
#109898 = CARTESIAN_POINT ( 'NONE',  ( -9.267161690140662600, 10.77044237904097734, -1.199719254218441611 ) ) ;
#109899 = CARTESIAN_POINT ( 'NONE',  ( 1.933841784273998332, -1.951746473714164321, 0.4931059669559466063 ) ) ;
#109900 = CARTESIAN_POINT ( 'NONE',  ( 2.008577182894935476, 0.6104510041588117053, 1.864461945915835583 ) ) ;
#109901 = CARTESIAN_POINT ( 'NONE',  ( -8.158255747121117452, 10.54105100977322174, 1.599625672291295375 ) ) ;
#109902 = CARTESIAN_POINT ( 'NONE',  ( -6.551614543901706611, 8.666636272683888365, 1.599625672291283607 ) ) ;
#109904 = EDGE_CURVE ( 'NONE', #111991, #36461, #89695, .T. ) ;
#109903 = FACE_OUTER_BOUND ( 'NONE', #59666, .T. ) ;
#109906 = CARTESIAN_POINT ( 'NONE',  ( 3.625649997064513297, -1.053871202854910871, -1.421704988934450409 ) ) ;
#109905 = CARTESIAN_POINT ( 'NONE',  ( 4.470703160837229184, 0.0002547659985942945528, -2.090823719324691687 ) ) ;
#109907 = CARTESIAN_POINT ( 'NONE',  ( -8.752560967067513076, 14.99999998465384365, 9.356054886187056496 ) ) ;
#109908 = CARTESIAN_POINT ( 'NONE',  ( 5.982448691606671254, -0.3306924304021444661, -2.268186543139012024 ) ) ;
#109909 = CARTESIAN_POINT ( 'NONE',  ( 5.138483783005516337, -1.490010379379594241, 0.8989716238894971401 ) ) ;
#109910 = CARTESIAN_POINT ( 'NONE',  ( 7.079328764629950754, 11.41096732537697633, 0.7998128361456462443 ) ) ;
#109911 = CARTESIAN_POINT ( 'NONE',  ( 1.499999999999990896, 4.025000000000021672, 1.214306433183764966E-14 ) ) ;
#109912 = CARTESIAN_POINT ( 'NONE',  ( 5.378194026956880869, -0.2521426391564468572, 1.715267145961799411 ) ) ;
#109913 = CARTESIAN_POINT ( 'NONE',  ( 6.180164126497881938, -1.200935631872475540, -1.808625420649534021 ) ) ;
#109914 = CARTESIAN_POINT ( 'NONE',  ( 5.417547566918786472, 6.138612003838852971, 1.022798779415410753 ) ) ;
#109915 = CARTESIAN_POINT ( 'NONE',  ( 6.403528931544730796, -1.954801056786956259, 0.4946215565981848528 ) ) ;
#109916 = CARTESIAN_POINT ( 'NONE',  ( 5.218750000000002665, -0.7852924748297095414, 1.895863743164193371 ) ) ;
#109917 = CARTESIAN_POINT ( 'NONE',  ( -1.201851678989727383E-14, 5.618750000682818602, -1.732050807568863648 ) ) ;
#109918 = CARTESIAN_POINT ( 'NONE',  ( 3.557566385928968788, 0.4691178692100838599, -1.868274323828737371 ) ) ;
#109919 = CARTESIAN_POINT ( 'NONE',  ( -1.500000000000015099, 11.01041666734946389, -0.8660254037844309360 ) ) ;
#109920 = CARTESIAN_POINT ( 'NONE',  ( 0.6455721646590365514, 0.1693206843514388493, 2.214916916779915201 ) ) ;
#109921 = ORIENTED_EDGE ( 'NONE', *, *, #183326, .F. ) ;
#109922 = CARTESIAN_POINT ( 'NONE',  ( -1.500000000000011324, 4.879166666666690411, -0.8660254037844313801 ) ) ;
#109923 = CARTESIAN_POINT ( 'NONE',  ( 6.471319392424407901, 6.444294134116939077, 0.7998128361456341429 ) ) ;
#109924 = CARTESIAN_POINT ( 'NONE',  ( 7.169564303528210836, 7.258913197071374945, -0.7998128361456281477 ) ) ;
#109925 = CARTESIAN_POINT ( 'NONE',  ( 2.069254833283964867, -1.714886923611224745, 1.411838272681579687 ) ) ;
#109926 = CARTESIAN_POINT ( 'NONE',  ( 4.382186172716248329, 4.009346271119131444, 0.09521571495261728357 ) ) ;
#109927 = CARTESIAN_POINT ( 'NONE',  ( 8.107412671292042461, 9.521364873671299023, 1.082531754730558626 ) ) ;
#109928 = CARTESIAN_POINT ( 'NONE',  ( -8.880227426826648340, 11.38335130276301754, 1.443375672974064550 ) ) ;
#109929 = EDGE_CURVE ( 'NONE', #112883, #157004, #56420, .T. ) ;
#109930 = CARTESIAN_POINT ( 'NONE',  ( 6.211043768836170820, 9.299949259400630552, 1.082531754730549967 ) ) ;
#109931 = STYLED_ITEM ( 'NONE', ( #165783 ), #202122 ) ;
#109932 = CARTESIAN_POINT ( 'NONE',  ( 0.6510177983308338412, 0.9963039324867200008, 1.753029211773032392 ) ) ;
#109934 = CARTESIAN_POINT ( 'NONE',  ( 5.424308963177657539, 1.013736099364664911, 1.796294033555500658 ) ) ;
#109933 = CARTESIAN_POINT ( 'NONE',  ( 8.106885785967500979, 11.54545161934907682, 1.199719254218460707 ) ) ;
#109935 = CARTESIAN_POINT ( 'NONE',  ( -11.86239285000045918, 9.719999999999998863, -1.812080536912752837 ) ) ;
#109936 = CARTESIAN_POINT ( 'NONE',  ( -4.613852347352193739, 4.277249248199312071, 1.214306433183764966E-14 ) ) ;
#109937 = CARTESIAN_POINT ( 'NONE',  ( -2.019980081995991661, 3.974415841077574285, 11.36314192354172192 ) ) ;
#109938 = CARTESIAN_POINT ( 'NONE',  ( -1.402160292154681736E-14, 1.446875000341420137, -1.575800808251659024 ) ) ;
#109939 = CARTESIAN_POINT ( 'NONE',  ( 0.1921619543209041325, -0.3744425218715953796, -1.735604558297418443 ) ) ;
#109940 = CARTESIAN_POINT ( 'NONE',  ( 6.416678112323896954, -1.140949303232444478, -1.306061676789990855 ) ) ;
#109941 = CARTESIAN_POINT ( 'NONE',  ( 5.794438198198100132, 1.417746085458403638, -1.009241466377588603 ) ) ;
#109942 = CARTESIAN_POINT ( 'NONE',  ( 2.613130667218881431, -0.2215951064345271782, 2.281621536969838271 ) ) ;
#109943 = CARTESIAN_POINT ( 'NONE',  ( -0.6823417656250246877, -0.4489583329919111243, 1.181850606188755259 ) ) ;
#109944 = CARTESIAN_POINT ( 'NONE',  ( 2.501689010688646242, -0.7045654096689784041, -1.701190496055771550 ) ) ;
#109945 = CARTESIAN_POINT ( 'NONE',  ( 9.921869487102386032, 10.46993591124128997, 0.000000000000000000 ) ) ;
#109946 = CARTESIAN_POINT ( 'NONE',  ( -9.604686356149276349, 3.999999999999997335, 7.193747284969079558 ) ) ;
#109947 = CARTESIAN_POINT ( 'NONE',  ( 2.608196206841297826, -0.6965810133783244540, -1.687657492251873226 ) ) ;
#109948 = CARTESIAN_POINT ( 'NONE',  ( 4.254529844270301453, 1.955172953530256219, -0.4926405443339901269 ) ) ;
#109949 = CARTESIAN_POINT ( 'NONE',  ( -3.348500752450953577, 4.929670182657964084, 1.443375672974062551 ) ) ;
#109950 = CARTESIAN_POINT ( 'NONE',  ( 4.407809338218622308, 8.156544971314787063, 0.000000000000000000 ) ) ;
#109951 = CARTESIAN_POINT ( 'NONE',  ( 5.649480931864863109, -1.658039504894607719, -1.298324887859639842 ) ) ;
#109952 = CARTESIAN_POINT ( 'NONE',  ( -7.223796917982883592, 7.322184580601816428, -0.7998128361456291469 ) ) ;
#109953 = CARTESIAN_POINT ( 'NONE',  ( 7.591119599213490332, 13.85210394378908028, 8.823496455125575011 ) ) ;
#109954 = CARTESIAN_POINT ( 'NONE',  ( 2.189971326302230903, -1.350648006375281929, -1.569233719104834890 ) ) ;
#109955 = CARTESIAN_POINT ( 'NONE',  ( 3.181359600701000989, 6.863336634126477875, 0.000000000000000000 ) ) ;
#109956 = CARTESIAN_POINT ( 'NONE',  ( 1.360316468750004448, 0.2968750003413955785, -6.938893903907228378E-15 ) ) ;
#109957 = CARTESIAN_POINT ( 'NONE',  ( 4.705793326368500118, 1.571798730262342181, 1.423547657546264000 ) ) ;
#109958 = ITEM_DEFINED_TRANSFORMATION ( 'NONE', 'NONE', #14249,  #200407 ) ;
#109959 = CARTESIAN_POINT ( 'NONE',  ( 1.295397306693826467, 1.458444760659328265, 1.258811869801695682 ) ) ;
#109960 = ORIENTED_EDGE ( 'NONE', *, *, #35190, .T. ) ;
#109961 = CARTESIAN_POINT ( 'NONE',  ( -4.950662367645459305, 5.804802846121667415, -1.199719254218453823 ) ) ;
#109962 = CARTESIAN_POINT ( 'NONE',  ( 7.560643217915098191, 11.97250085420964716, -0.7998128361456291469 ) ) ;
#109963 = CARTESIAN_POINT ( 'NONE',  ( 5.844973620822844218, 6.952128991449046502, 1.082531754730549967 ) ) ;
#109964 = CARTESIAN_POINT ( 'NONE',  ( -1.737500000000000266, -0.7145833323774185564, -3.009438278150923907 ) ) ;
#109965 = CARTESIAN_POINT ( 'NONE',  ( -6.064574784014443942, 5.969758757638621738, -0.7998128361456291469 ) ) ;
#109966 = CARTESIAN_POINT ( 'NONE',  ( 5.730757696090861941, 1.422813033107739988, -1.572628729999878905 ) ) ;
#109967 = CARTESIAN_POINT ( 'NONE',  ( 1.993330679213504153, 1.832751758872013914, -1.037179240317965823 ) ) ;
#109968 = CARTESIAN_POINT ( 'NONE',  ( -5.991777542596674166, 5.955104985976372944, 0.000000000000000000 ) ) ;
#109969 = CARTESIAN_POINT ( 'NONE',  ( 7.079328764629950754, 11.41096732537697633, 0.7998128361456462443 ) ) ;
#109970 = CARTESIAN_POINT ( 'NONE',  ( 5.910971410920907942, -1.467885462018687415, 1.143791174867914373 ) ) ;
#109971 = CARTESIAN_POINT ( 'NONE',  ( 5.764187864104357573, 9.876636274763768597, 1.040834085586084257E-14 ) ) ;
#109972 = CARTESIAN_POINT ( 'NONE',  ( -0.4340096093344613104, 3.986747911422942714, -0.4851708347456849535 ) ) ;
#109973 = CARTESIAN_POINT ( 'NONE',  ( -7.932929277771797238, 8.427708043588125975, 0.000000000000000000 ) ) ;
#109975 = CARTESIAN_POINT ( 'NONE',  ( -2.103486388414573138, 5.605817886458954291, 1.040834085586084257E-14 ) ) ;
#109974 = AXIS2_PLACEMENT_3D ( 'NONE', #126834, #29252, #94273 ) ;
#109976 = CARTESIAN_POINT ( 'NONE',  ( -1.817552723627640532, 2.511586290612293659, 2.499391979724955526 ) ) ;
#109977 = FILL_AREA_STYLE_COLOUR ( '', #74680 ) ;
#109979 = CARTESIAN_POINT ( 'NONE',  ( 2.242563829109287088, -1.923402688547710904, -0.3857071251459272543 ) ) ;
#109978 = CARTESIAN_POINT ( 'NONE',  ( -3.355169270512988773E-14, -0.4375000000000020539, 1.414508159514561436 ) ) ;
#109980 = CARTESIAN_POINT ( 'NONE',  ( 1.376082401959723089, 1.288024388040419632, 1.735935173841046675 ) ) ;
#109982 = CARTESIAN_POINT ( 'NONE',  ( -5.854914268151548917, 6.175991412503675448, 0.9282606102084377531 ) ) ;
#109981 = CARTESIAN_POINT ( 'NONE',  ( -6.123442655227560927, 7.173046514967467147, 1.199719254218452047 ) ) ;
#109983 = CARTESIAN_POINT ( 'NONE',  ( 1.364683531249988535, 2.363541667008088432, 0.7879004041258500513 ) ) ;
#109984 = CARTESIAN_POINT ( 'NONE',  ( 2.934579196337202323, 0.9245653808827180020, 1.466514439666162684 ) ) ;
#109985 = CARTESIAN_POINT ( 'NONE',  ( 2.026944798790380364, -1.135751832872053058, -1.318713242574782507 ) ) ;
#109986 = CARTESIAN_POINT ( 'NONE',  ( 6.317736394288140822, 7.433409217166723870, 1.082531754730558626 ) ) ;
#109987 = CARTESIAN_POINT ( 'NONE',  ( -12.65133343644925823, 8.691152131673410608, 1.253321570098529181 ) ) ;
#109988 = AXIS2_PLACEMENT_3D ( 'NONE', #102214, #52400, #117462 ) ;
#109989 = CARTESIAN_POINT ( 'NONE',  ( -0.08814328694728679192, -9.915773547069447247, -10.99964701288570623 ) ) ;
#109990 = CARTESIAN_POINT ( 'NONE',  ( -5.093022980588950865, 5.970890227889075419, -1.199719254218453823 ) ) ;
#109991 = CARTESIAN_POINT ( 'NONE',  ( 1.182427310604698079, -1.922956083944601158, -0.4339701177692931178 ) ) ;
#109993 = CARTESIAN_POINT ( 'NONE',  ( -4.651856103264620401, 8.441266197201775512, 0.000000000000000000 ) ) ;
#109992 = CARTESIAN_POINT ( 'NONE',  ( 5.291234991620994421, -0.05314252713351996088, -1.911838368980276925 ) ) ;
#109994 = CARTESIAN_POINT ( 'NONE',  ( -4.923019175093582334, 8.757623114335565617, 0.7216878364870267237 ) ) ;
#109995 = CARTESIAN_POINT ( 'NONE',  ( 5.176180785367283654, 9.260904359562321275, -0.7998128361456481317 ) ) ;
#109996 = CARTESIAN_POINT ( 'NONE',  ( -7.445362632559989535, 8.715286488521982733, 1.199719254218452047 ) ) ;
#109997 = CARTESIAN_POINT ( 'NONE',  ( 1.102219918440990876, -0.9059408578524772437, 1.805149201161629025 ) ) ;
#109998 = CARTESIAN_POINT ( 'NONE',  ( -0.3000000000000155320, 3.999999999999955147, 1.007084189318345757 ) ) ;
#109999 = CARTESIAN_POINT ( 'NONE',  ( 5.895647473559280982, 1.742329625737188525, 1.513132890121783536 ) ) ;
#110000 = CARTESIAN_POINT ( 'NONE',  ( 5.371523934717264304, -0.2895824386080196322, 1.940264742196501802 ) ) ;
#110001 = CARTESIAN_POINT ( 'NONE',  ( 3.537899350542179189, 1.241011212050652901, 1.519374649786103149 ) ) ;
#110002 = CARTESIAN_POINT ( 'NONE',  ( 7.425061681778431399, 11.81432239538354345, 0.7998128361456462443 ) ) ;
#110003 = CARTESIAN_POINT ( 'NONE',  ( 0.7740648250077889481, 1.777010169924503558, -0.9530137779002674225 ) ) ;
#110004 = ORIENTED_EDGE ( 'NONE', *, *, #209722, .F. ) ;
#110005 = CARTESIAN_POINT ( 'NONE',  ( 1.675176079212177260, 1.839371217556123650, -1.048680071690030413 ) ) ;
#110007 = CARTESIAN_POINT ( 'NONE',  ( -8.681298431451969222, 9.022603012982438386, 1.040834085586084257E-14 ) ) ;
#110006 = CARTESIAN_POINT ( 'NONE',  ( -3.490334480514268645, 6.159475096320226939, -1.199719254218452935 ) ) ;
#110008 = CARTESIAN_POINT ( 'NONE',  ( 2.273173984786102775, 1.132353773513800510, 1.451651336590239927 ) ) ;
#110009 = ORIENTED_EDGE ( 'NONE', *, *, #65319, .T. ) ;
#110010 = CARTESIAN_POINT ( 'NONE',  ( 11.57758243856749303, 8.192336405874874217, -2.990131717548606627 ) ) ;
#110011 = CARTESIAN_POINT ( 'NONE',  ( 3.269896953881154644, 0.5115095171020591636, -2.057881918134551125 ) ) ;
#110012 = CARTESIAN_POINT ( 'NONE',  ( -1.201851678989727383E-14, 3.868750000682817713, -1.732050807568863648 ) ) ;
#110013 = CARTESIAN_POINT ( 'NONE',  ( 6.913768267964901071, 10.15348118167935709, -1.199719254218441611 ) ) ;
#110014 = CARTESIAN_POINT ( 'NONE',  ( 7.014364370223726830, 9.276787413384745662, -1.599625672291269396 ) ) ;
#110015 = CARTESIAN_POINT ( 'NONE',  ( 3.163408073613428684, 0.3057118896435347954, -2.037866251177067323 ) ) ;
#110017 = CARTESIAN_POINT ( 'NONE',  ( 0.02850758872123548837, -1.683968158181762043, 0.7450552726024004535 ) ) ;
#110016 = CARTESIAN_POINT ( 'NONE',  ( -8.538937818508475885, 8.856515631215026829, 1.040834085586084257E-14 ) ) ;
#110018 = CARTESIAN_POINT ( 'NONE',  ( -0.6823417656249969321, 4.717708333674755394, -1.181850606188749264 ) ) ;
#110019 =( BOUNDED_CURVE ( )  B_SPLINE_CURVE ( 2, ( #29396, #95489, #147412, #13121, #131217, #94414, #161535 ),
 .UNSPECIFIED., .F., .T. ) 
 B_SPLINE_CURVE_WITH_KNOTS ( ( 3, 2, 2, 3 ),
 ( 0.2375000000000003775, 0.2416666666666670293, 0.2458333333333336257, 0.2500000000000002776 ),
 .UNSPECIFIED. ) 
 CURVE ( )  GEOMETRIC_REPRESENTATION_ITEM ( )  RATIONAL_B_SPLINE_CURVE ( ( 0.9999999999999874545, 0.8660254037844512531, 1.000000000000000000, 0.8660254037844387076, 1.000000000000000000, 0.8660254037844298258, 1.000000000000008882 ) ) 
 REPRESENTATION_ITEM ( '' )  );
#110020 = CARTESIAN_POINT ( 'NONE',  ( -0.1007326007326104361, -9.919999999999998153, -10.99953876047306167 ) ) ;
#110021 = CARTESIAN_POINT ( 'NONE',  ( 0.2939702064862387276, 1.638257335637434364, 1.478849500172851217 ) ) ;
#110022 = CARTESIAN_POINT ( 'NONE',  ( 2.478104529052836291, 1.390129537188329101, 1.784895063601476428 ) ) ;
#110023 = CARTESIAN_POINT ( 'NONE',  ( -8.514157279702027736, 10.95626946445095307, -1.443375672974059665 ) ) ;
#110024 = CARTESIAN_POINT ( 'NONE',  ( 2.671877653990344381, 1.802496804585513868, -0.1814095246875074008 ) ) ;
#110025 = CARTESIAN_POINT ( 'NONE',  ( 3.239363768214057249, 0.4605203156026844158, -1.859431460922003509 ) ) ;
#110026 = CARTESIAN_POINT ( 'NONE',  ( 3.912603064140641074, 0.7423916865902054907, 1.932869565047180549 ) ) ;
#110027 = CARTESIAN_POINT ( 'NONE',  ( 0.6823417656249899377, 2.405208333674753618, 1.181850606188767472 ) ) ;
#110028 = EDGE_CURVE ( 'NONE', #118348, #169237, #90884, .T. ) ;
#110029 = CARTESIAN_POINT ( 'NONE',  ( 3.010573890873136094, 1.429054271512670615, -1.358355385302984164 ) ) ;
#110030 = PRODUCT_RELATED_PRODUCT_CATEGORY ( 'part', '', ( #157772 ) ) ;
#110031 = CARTESIAN_POINT ( 'NONE',  ( 6.709608095207008738, -0.4227469423600908605, 1.886647698053174116 ) ) ;
#110032 = CARTESIAN_POINT ( 'NONE',  ( 2.711613914024712191, -1.850561042518297672, 0.2725550856255419818 ) ) ;
#110034 = CARTESIAN_POINT ( 'NONE',  ( 4.708029738644283313, 8.352945002179891887, -0.6661931671527853149 ) ) ;
#110033 = CARTESIAN_POINT ( 'NONE',  ( 2.069360784497351613, -2.110879405061675929, -0.9329422106417961658 ) ) ;
#110035 = CARTESIAN_POINT ( 'NONE',  ( 2.681907113330802339, -1.068898278170841598, -1.523273593526828673 ) ) ;
#110036 = CARTESIAN_POINT ( 'NONE',  ( 1.364683531249988535, 2.363541667008088432, 0.7879004041258500513 ) ) ;
#110037 = CARTESIAN_POINT ( 'NONE',  ( 6.408646180098039657, 0.6432782940990633413, 1.959889192978042205 ) ) ;
#110038 = CARTESIAN_POINT ( 'NONE',  ( -4.192495815123836955, 5.914331089109674089, -1.599625672291256295 ) ) ;
#110039 = CARTESIAN_POINT ( 'NONE',  ( 7.610204295972345712, 7.772993188256215547, 0.7998128361456341429 ) ) ;
#110040 = CARTESIAN_POINT ( 'NONE',  ( -1.500343415223059695, 3.249252082317366508, -0.07855322731632197186 ) ) ;
#110041 = CARTESIAN_POINT ( 'NONE',  ( 0.6101635361662772761, -2.095732242510168764, 0.2083838208960953620 ) ) ;
#110042 = CARTESIAN_POINT ( 'NONE',  ( -0.6823417656249969321, 4.030208333674754506, -1.181850606188749264 ) ) ;
#110043 = CARTESIAN_POINT ( 'NONE',  ( 5.817692603468245238, -2.110333850551704415, 0.4673072906974176655 ) ) ;
#110044 = CARTESIAN_POINT ( 'NONE',  ( 6.639320575229294086, 0.002105643433562148347, 2.003388605011639179 ) ) ;
#110045 = CARTESIAN_POINT ( 'NONE',  ( 0.6823417656249864960, -1.073958332991911568, -1.181850606188749264 ) ) ;
#110046 = CARTESIAN_POINT ( 'NONE',  ( -5.097502569058221411, 6.009803087731781623, -1.082531754730544860 ) ) ;
#110049 = CARTESIAN_POINT ( 'NONE',  ( 4.528060117284240071, 5.345453560662148718, 1.082531754730560403 ) ) ;
#110048 = FACE_OUTER_BOUND ( 'NONE', #208598, .T. ) ;
#110047 = CARTESIAN_POINT ( 'NONE',  ( 6.363572996767764778, 8.517530811019446091, -1.599625672291283607 ) ) ;
#110050 = CARTESIAN_POINT ( 'NONE',  ( -0.2409995289980038091, -0.004801160710915519658, -2.000252362011435636 ) ) ;
#110051 = CARTESIAN_POINT ( 'NONE',  ( 4.346888830327386266, -1.803415170841724979, -0.9023466997552240798 ) ) ;
#110053 = CARTESIAN_POINT ( 'NONE',  ( -5.763624699140874164, 8.777960344756069233, -1.082531754730549967 ) ) ;
#110052 = CARTESIAN_POINT ( 'NONE',  ( -9.978437869977959451, 10.74385839117019614, -0.7216878364870267237 ) ) ;
#110054 = DIRECTION ( 'NONE',  ( -0.6483454320283799088, 0.000000000000000000, 0.7613463080411786432 ) ) ;
#110056 = CARTESIAN_POINT ( 'NONE',  ( -1.364683531250010740, 11.13020833367473372, 0.7879004041258445001 ) ) ;
#110055 = CARTESIAN_POINT ( 'NONE',  ( 5.612251347527116963, -0.9680786960581324596, -1.932885698521320528 ) ) ;
#110057 = LINE ( 'NONE', #96969, #72360 ) ;
#110058 = CARTESIAN_POINT ( 'NONE',  ( -10.94893285264089577, 5.391538659128299216, 4.806406785934876247 ) ) ;
#110060 = CARTESIAN_POINT ( 'NONE',  ( 6.415638736316127577, -1.319241173714128745, -1.525034172108488573 ) ) ;
#110059 = CARTESIAN_POINT ( 'NONE',  ( -7.334597914868743018, 7.659378443542744996, -0.7216878364870267237 ) ) ;
#110061 = CARTESIAN_POINT ( 'NONE',  ( 0.6823417656249899377, 1.405208333674752508, 1.181850606188755259 ) ) ;
#110062 = CARTESIAN_POINT ( 'NONE',  ( 6.883263157960367806, 2.959656548886806515, 2.506466465954690914 ) ) ;
#110063 = CARTESIAN_POINT ( 'NONE',  ( 0.7500000000000006661, 8.666666666666669627, -1.299038105676657340 ) ) ;
#110064 = CARTESIAN_POINT ( 'NONE',  ( 1.664246808422519486, -1.221613929703774915, 1.218001262086549907 ) ) ;
#110065 = CARTESIAN_POINT ( 'NONE',  ( 6.994027139803230320, 9.253060644560830994, -1.599625672291267398 ) ) ;
#110066 = CARTESIAN_POINT ( 'NONE',  ( 5.611095471209277541, 7.639640364534566075, 1.599625672291268286 ) ) ;
#110067 = CARTESIAN_POINT ( 'NONE',  ( -0.6823417656250246877, -0.8864583329919115684, 1.181850606188755259 ) ) ;
#110068 = CARTESIAN_POINT ( 'NONE',  ( 1.282078435845935616, -1.724974465617232999, -0.3947418589646100040 ) ) ;
#110069 = CARTESIAN_POINT ( 'NONE',  ( 2.209637070578834628, 1.557646164037255643, 1.275278917823706948 ) ) ;
#110070 = CARTESIAN_POINT ( 'NONE',  ( 4.225739626866775289, -2.112672615930260900, 0.6375689414055001336 ) ) ;
#110071 = AXIS2_PLACEMENT_3D ( 'NONE', #62917, #96524, #129085 ) ;
#110072 = CARTESIAN_POINT ( 'NONE',  ( 5.401315523140023167, -1.865749354952720207, 1.109950958716971803 ) ) ;
#110073 = ORIENTED_EDGE ( 'NONE', *, *, #187963, .F. ) ;
#110074 = CARTESIAN_POINT ( 'NONE',  ( 0.7499999999999885647, -1.016666666666644847, 1.299038105676657340 ) ) ;
#110075 = CARTESIAN_POINT ( 'NONE',  ( 8.717529583462654941, 9.272798723569005475, 0.7216878364870458196 ) ) ;
#110077 = CARTESIAN_POINT ( 'NONE',  ( 3.005482631727268039, -1.942536929278560365, 0.5405117225928540714 ) ) ;
#110076 = CARTESIAN_POINT ( 'NONE',  ( 3.281995766809755466, 2.068381274212594878, -0.4664580258975092875 ) ) ;
#110079 = ORIENTED_EDGE ( 'NONE', *, *, #83031, .T. ) ;
#110078 = CARTESIAN_POINT ( 'NONE',  ( 3.357467859903106255, -1.375039365347962450, -1.179588011891503418 ) ) ;
#110080 = CARTESIAN_POINT ( 'NONE',  ( 4.552505719138623341, 8.533283448962240669, 0.7998128361456341429 ) ) ;
#110081 = ORIENTED_EDGE ( 'NONE', *, *, #153081, .F. ) ;
#110082 = CARTESIAN_POINT ( 'NONE',  ( -10.23203630735456393, -6.594478602028840619, 1.760317133499380763E-15 ) ) ;
#110083 = CARTESIAN_POINT ( 'NONE',  ( 3.960953433486789521, 7.772862772376584850, -0.7998128361456221525 ) ) ;
#110084 = CARTESIAN_POINT ( 'NONE',  ( 6.129513044595952032, -1.717388127611047421, 0.6198453807191862674 ) ) ;
#110086 = CARTESIAN_POINT ( 'NONE',  ( 1.200237320533149799, 1.284028115529710190, -1.421911532115504029 ) ) ;
#110085 = CARTESIAN_POINT ( 'NONE',  ( -3.415764635639130020, 6.072476943965863683, 1.199719254218462483 ) ) ;
#110088 = AXIS2_PLACEMENT_3D ( 'NONE', #204051, #202998, #186763 ) ;
#110087 = AXIS2_PLACEMENT_3D ( 'NONE', #157258, #143174, #61875 ) ;
#110089 = CYLINDRICAL_SURFACE ( 'NONE', #2774, 2.000000000000000000 ) ;
#110090 = DIRECTION ( 'NONE',  ( 0.000000000000000000, 1.000000000000000000, 0.000000000000000000 ) ) ;
#110091 = CARTESIAN_POINT ( 'NONE',  ( 1.364683531249986537, 1.717708333674749399, -0.7879004041258239610 ) ) ;
#110092 = DIRECTION ( 'NONE',  ( 0.000000000000000000, 0.000000000000000000, 1.000000000000000000 ) ) ;
#110093 = CARTESIAN_POINT ( 'NONE',  ( -9.318531651294266638, 9.766041769465124034, -0.7998128361456291469 ) ) ;
#110094 = CARTESIAN_POINT ( 'NONE',  ( 5.752838164830007983, -1.706859214253673152, 1.326403591387192771 ) ) ;
#110095 = CARTESIAN_POINT ( 'NONE',  ( -4.665414256878301025, 6.536345614481700927, -1.443375672974066548 ) ) ;
#110096 = CARTESIAN_POINT ( 'NONE',  ( -7.747558435566414659, 8.003516027774422170, -0.7998128361456362523 ) ) ;
#110097 = CARTESIAN_POINT ( 'NONE',  ( 3.498385214435925317, -1.041973313016024472, 1.846846941210858351 ) ) ;
#110099 = CARTESIAN_POINT ( 'NONE',  ( -10.28823555840286552, 6.680969737303435352, 5.325637450257892702 ) ) ;
#110098 = CARTESIAN_POINT ( 'NONE',  ( -0.1296875068448125057, 1.390030859318210688, -2.083197486262199138 ) ) ;
#110100 = CARTESIAN_POINT ( 'NONE',  ( 4.165272970243100836, 0.2446167658484849627, -1.956081580383911778 ) ) ;
#110101 = CARTESIAN_POINT ( 'NONE',  ( 6.170165192347925931, 1.906784905861274693, -0.1475879885542986936 ) ) ;
#110102 = ORIENTED_EDGE ( 'NONE', *, *, #5141, .F. ) ;
#110103 = CARTESIAN_POINT ( 'NONE',  ( 5.700440484604645697, 1.420036636931173657, -1.570746850784213056 ) ) ;
#110104 = FACE_OUTER_BOUND ( 'NONE', #52112, .T. ) ;
#110105 = CARTESIAN_POINT ( 'NONE',  ( 0.2388460773940295212, -2.007853281042128568, -0.5044432775610437902 ) ) ;
#110106 = CARTESIAN_POINT ( 'NONE',  ( 2.888542945859973177, 1.665235949713929076, -0.9988640340363763581 ) ) ;
#110107 = VERTEX_POINT ( 'NONE', #156581 ) ;
#110108 = DIRECTION ( 'NONE',  ( -1.000000000000000000, 0.000000000000000000, 0.000000000000000000 ) ) ;
#110109 = CARTESIAN_POINT ( 'NONE',  ( 6.363572996767764778, 8.517530811019446091, -1.599625672291283607 ) ) ;
#110111 = CARTESIAN_POINT ( 'NONE',  ( 7.332262146892202459, 7.448727347662698506, -0.7998128361456281477 ) ) ;
#110110 = CARTESIAN_POINT ( 'NONE',  ( 4.136730066327800159, -1.819077861029708032, 1.030257495502053589 ) ) ;
#110112 = CARTESIAN_POINT ( 'NONE',  ( 5.031484404002889654, 6.003058238492422483, 1.082531754730549078 ) ) ;
#110114 = ORIENTED_EDGE ( 'NONE', *, *, #211811, .F. ) ;
#110113 = CARTESIAN_POINT ( 'NONE',  ( 0.3283783949157508819, 1.250606878306897984, -1.310747381600821049 ) ) ;
#110115 = CARTESIAN_POINT ( 'NONE',  ( 5.285833163787800437, 1.479997892162683071, 1.637210856327932618 ) ) ;
#110116 = DIRECTION ( 'NONE',  ( -0.6507913734559641616, -0.7592566023653004592, 0.000000000000000000 ) ) ;
#110117 = CARTESIAN_POINT ( 'NONE',  ( 3.223846859376262142, -2.127229092858519799, 0.5869343725257711863 ) ) ;
#110118 = CARTESIAN_POINT ( 'NONE',  ( 6.611572464958476836, 10.86525164242692298, 0.7998128361456462443 ) ) ;
#110119 = CARTESIAN_POINT ( 'NONE',  ( 7.015401035077362124, 6.062865449010541141, -2.437084766375293921 ) ) ;
#110120 = CARTESIAN_POINT ( 'NONE',  ( 1.699719973799845185, 1.319605273547658220, 1.384218846220357291 ) ) ;
#110121 = CARTESIAN_POINT ( 'NONE',  ( 8.615316546479974136, 12.13862083994696839, 1.199719254218450271 ) ) ;
#110122 = CARTESIAN_POINT ( 'NONE',  ( 5.283670394142272464, -1.967056725255760474, 0.6460906113585005439 ) ) ;
#110124 = CARTESIAN_POINT ( 'NONE',  ( 2.307699607974790901, -0.4742087202370263155, 2.108885336910087283 ) ) ;
#110123 = CARTESIAN_POINT ( 'NONE',  ( 9.620326184871647257, -9.190313392136383541, -0.3418113563954068290 ) ) ;
#110125 = CARTESIAN_POINT ( 'NONE',  ( 4.985950990042907094, -2.174969566330759996, -0.2684501861200879747 ) ) ;
#110126 = EDGE_LOOP ( 'NONE', ( #16384, #16371, #206054, #33306 ) ) ;
#110127 = CARTESIAN_POINT ( 'NONE',  ( 8.940712233207955606, 12.51824914112961729, 1.199719254218450271 ) ) ;
#110128 = AXIS2_PLACEMENT_3D ( 'NONE', #153987, #5555, #172374 ) ;
#110129 = DIRECTION ( 'NONE',  ( 1.000000000000000000, -0.000000000000000000, -0.000000000000000000 ) ) ;
#110130 = CARTESIAN_POINT ( 'NONE',  ( -0.4138605925103633898, 8.005950907165120256, 1.999879544075660043 ) ) ;
#110131 = CARTESIAN_POINT ( 'NONE',  ( 5.761288931164342486, 5.686201605971993978, -0.7998128361456481317 ) ) ;
#110132 = CARTESIAN_POINT ( 'NONE',  ( -3.285556943750000070, -2.996874999522041616, 0.000000000000000000 ) ) ;
#110133 = CARTESIAN_POINT ( 'NONE',  ( -2.979759899953417612, 6.698413326579433225, 0.7998128361456352531 ) ) ;
#110134 = CARTESIAN_POINT ( 'NONE',  ( -9.490344339885981029, 10.17441593939621924, -0.7216878364870267237 ) ) ;
#110135 = CARTESIAN_POINT ( 'NONE',  ( 4.549643065837591038, 7.465611455855944101, -1.199719254218452047 ) ) ;
#110136 = CARTESIAN_POINT ( 'NONE',  ( 5.981320602565292965, -0.05662044862421274777, 2.069665677200482445 ) ) ;
#110137 = CARTESIAN_POINT ( 'NONE',  ( 4.670489471188726149, -1.257041717089462773, 1.459967279689990960 ) ) ;
#110138 = CARTESIAN_POINT ( 'NONE',  ( -0.1234324464992678227, -0.4448297287729073846, -1.973926538189611835 ) ) ;
#110139 = CARTESIAN_POINT ( 'NONE',  ( -2.331034670843834533E-15, -6.465328379374287948, 10.58872653680447407 ) ) ;
#110140 = CARTESIAN_POINT ( 'NONE',  ( 5.473741331615251227, 7.409117525016355010, -1.599625672291262513 ) ) ;
#110141 = CARTESIAN_POINT ( 'NONE',  ( 4.715651637508523564, 0.4355733895117944177, -1.920488317121961108 ) ) ;
#110142 = CARTESIAN_POINT ( 'NONE',  ( -0.01142137120296871262, -0.4863542539808898280, -2.144715426241408984 ) ) ;
#110143 = CARTESIAN_POINT ( 'NONE',  ( 4.195794211080963620, -0.6966935528937776567, 1.687730213881050600 ) ) ;
#110144 = CARTESIAN_POINT ( 'NONE',  ( 5.221298555038576872, 9.105615724271411082, 0.000000000000000000 ) ) ;
#110145 = CARTESIAN_POINT ( 'NONE',  ( 3.023105065722948126, 6.470780310077995701, 0.7216878364870338292 ) ) ;
#110146 = CARTESIAN_POINT ( 'NONE',  ( -6.631873415740034083, 7.766215735565355160, 1.199719254218452047 ) ) ;
#110147 = CARTESIAN_POINT ( 'NONE',  ( 4.878955176071345434, 6.785476686873604280, -1.599625672291269396 ) ) ;
#110148 = VERTEX_POINT ( 'NONE', #206370 ) ;
#110150 = CARTESIAN_POINT ( 'NONE',  ( 5.625249212676971311, 1.777412282398885823, 0.9453524948108845694 ) ) ;
#110149 = CARTESIAN_POINT ( 'NONE',  ( 2.946635061770470632, -1.506786691049965432, -1.057933238436038925 ) ) ;
#110151 = CARTESIAN_POINT ( 'NONE',  ( 0.6326644773376333131, 0.2229630159884201934, -2.287572974657641645 ) ) ;
#110152 = CARTESIAN_POINT ( 'NONE',  ( 5.858247074779933783, -1.961936380223072263, -0.003592477671530979431 ) ) ;
#110153 = CARTESIAN_POINT ( 'NONE',  ( -4.880045225915050189, 7.780804299287790826, 1.199719254218464037 ) ) ;
#110154 = FACE_OUTER_BOUND ( 'NONE', #105331, .T. ) ;
#110155 = CARTESIAN_POINT ( 'NONE',  ( -2.272963308585411735, 5.803540959991587478, 0.7998128361456341429 ) ) ;
#110157 = ADVANCED_FACE ( 'NONE', ( #74259 ), #59791, .F. ) ;
#110156 = CARTESIAN_POINT ( 'NONE',  ( 0.2212536527127808295, -1.848710500310095872, -0.9322282823912150240 ) ) ;
#110158 = CARTESIAN_POINT ( 'NONE',  ( -5.795184315198522285, 5.725746220678519904, -0.7998128361456362523 ) ) ;
#110160 = CARTESIAN_POINT ( 'NONE',  ( 0.3384655940862451029, 0.3152513238553408814, 1.843739016257638141 ) ) ;
#110159 = CARTESIAN_POINT ( 'NONE',  ( 1.083664105429899216, -0.9366695517310281716, 1.869248094466950949 ) ) ;
#110161 = CARTESIAN_POINT ( 'NONE',  ( 0.07074886611255049029, 8.280404612018074317, -2.000278354478734588 ) ) ;
#110162 = ORIENTED_EDGE ( 'NONE', *, *, #160909, .T. ) ;
#110163 = CARTESIAN_POINT ( 'NONE',  ( -0.2104748580754426390, 2.865278511227668634, -2.591885361450113834 ) ) ;
#110164 = CARTESIAN_POINT ( 'NONE',  ( 1.715945410011958217, 1.623988859063689949, 0.6264298892959454523 ) ) ;
#110165 = AXIS2_PLACEMENT_3D ( 'NONE', #79852, #211971, #18028 ) ;
#110166 = CARTESIAN_POINT ( 'NONE',  ( 4.961394147597008697, 7.875711374583454827, -1.199719254218452047 ) ) ;
#110168 = FACE_OUTER_BOUND ( 'NONE', #131043, .T. ) ;
#110167 = FACE_OUTER_BOUND ( 'NONE', #208265, .T. ) ;
#110169 = CARTESIAN_POINT ( 'NONE',  ( 2.789346554370454534, 1.219787599184172233, 1.219827592095571456 ) ) ;
#110170 = CARTESIAN_POINT ( 'NONE',  ( 2.261505105119133052, 2.148611799745976381, -0.4309092228176118478 ) ) ;
#110171 = CARTESIAN_POINT ( 'NONE',  ( 4.776106669258010307, 1.268914099295117781, 1.805409367619143390 ) ) ;
#110172 = CARTESIAN_POINT ( 'NONE',  ( -10.52626310920980757, 3.679096435225583939, -5.196420034295205603 ) ) ;
#110173 = CARTESIAN_POINT ( 'NONE',  ( 2.413135165516873126, -1.680682958684741823, 1.374403011902309402 ) ) ;
#110174 = CARTESIAN_POINT ( 'NONE',  ( 0.6272434487209905818, -1.734552980249819631, 0.5698080454362154379 ) ) ;
#110175 = CARTESIAN_POINT ( 'NONE',  ( 3.204427616716760685, 1.339657272674670718, -1.639694800048612899 ) ) ;
#110176 = CARTESIAN_POINT ( 'NONE',  ( 6.639320575229255894, 7.053084031878349869, 2.494893166485531388 ) ) ;
#110177 = ORIENTED_EDGE ( 'NONE', *, *, #63333, .T. ) ;
#110178 = AXIS2_PLACEMENT_3D ( 'NONE', #184266, #21745, #66230 ) ;
#110180 = CARTESIAN_POINT ( 'NONE',  ( -1.364683531250012516, 1.592708333674756727, 0.7879004041258379498 ) ) ;
#110179 = CARTESIAN_POINT ( 'NONE',  ( 4.072042370276293788, -1.319783315292190284, 1.874172932857321339 ) ) ;
#110181 = CARTESIAN_POINT ( 'NONE',  ( 3.029357257649615054, 5.621668336311468117, -1.199719254218446718 ) ) ;
#110182 = CARTESIAN_POINT ( 'NONE',  ( 5.778047442595251937, 2.188849720005956900, -0.3775064732549227586 ) ) ;
#110183 = CARTESIAN_POINT ( 'NONE',  ( -6.236387472606145010, 9.259240570473746601, -1.082531754730538864 ) ) ;
#110184 = CARTESIAN_POINT ( 'NONE',  ( 3.389175213736292047, 5.937492935125556315, 1.082531754730558626 ) ) ;
#110185 = CARTESIAN_POINT ( 'NONE',  ( -6.439759776366783761, 8.536139043893143707, 1.443375672974078761 ) ) ;
#110186 = EDGE_CURVE ( 'NONE', #61426, #177833, #48758, .T. ) ;
#110187 = CARTESIAN_POINT ( 'NONE',  ( 3.933273961740298752, 5.682181936820735579, 1.443375672974058777 ) ) ;
#110188 = EDGE_LOOP ( 'NONE', ( #144450, #579, #88888, #91658 ) ) ;
#110189 = CARTESIAN_POINT ( 'NONE',  ( 3.920546200773936896, -1.392545040883992336, -1.458557299768625581 ) ) ;
#110191 = CARTESIAN_POINT ( 'NONE',  ( 1.657159287258206604, 1.688608613550081516, -1.184165042645689558 ) ) ;
#110190 = CARTESIAN_POINT ( 'NONE',  ( 6.796715079152391148, 6.823922435299587974, 0.7998128361456341429 ) ) ;
#110192 = CARTESIAN_POINT ( 'NONE',  ( 11.94105721237523277, 19.00000000000000000, -1.187919463087249827 ) ) ;
#110193 = CARTESIAN_POINT ( 'NONE',  ( 4.895902867866261055, 4.884510565364971413, -0.7216878364870458196 ) ) ;
#110194 = CARTESIAN_POINT ( 'NONE',  ( 1.642778471875001811, -2.792708332855376785, 2.845375778867859751 ) ) ;
#110195 = CARTESIAN_POINT ( 'NONE',  ( 0.6823417656249899377, 5.676041667008087543, -1.181850606188754593 ) ) ;
#110196 = CARTESIAN_POINT ( 'NONE',  ( 5.191441776010862874, -0.7909675746368143301, 2.043907961996515699 ) ) ;
#110197 = CARTESIAN_POINT ( 'NONE',  ( 2.672500184003968382, 1.427937546361924381, 1.423961308954827754 ) ) ;
#110198 = CARTESIAN_POINT ( 'NONE',  ( 1.821575194732877545, 1.059174331173462935, -1.505913648122420900 ) ) ;
#110199 = CARTESIAN_POINT ( 'NONE',  ( 5.282873410819217241, 9.315102745931094219, -0.7998128361456281477 ) ) ;
#110200 = CARTESIAN_POINT ( 'NONE',  ( 0.1117072452763347851, -0.7311285168369995313, -1.561089762993218999 ) ) ;
#110201 =( BOUNDED_CURVE ( )  B_SPLINE_CURVE ( 2, ( #78959, #76827, #74711, #140814, #42229, #173293, #94184 ),
 .UNSPECIFIED., .F., .T. ) 
 B_SPLINE_CURVE_WITH_KNOTS ( ( 3, 2, 2, 3 ),
 ( 0.3750000000000002776, 0.3833333333333334703, 0.3916666666666665519, 0.3999999999999997446 ),
 .UNSPECIFIED. ) 
 CURVE ( )  GEOMETRIC_REPRESENTATION_ITEM ( )  RATIONAL_B_SPLINE_CURVE ( ( 0.9999999999999955591, 0.8660254037844431485, 1.000000000000000000, 0.8660254037844387076, 1.000000000000000000, 0.8660254037844431485, 0.9999999999999955591 ) ) 
 REPRESENTATION_ITEM ( '' )  );
#110202 = CARTESIAN_POINT ( 'NONE',  ( -6.367525699912501835, 10.58053041653993098, -0.7998128361456291469 ) ) ;
#110204 = CARTESIAN_POINT ( 'NONE',  ( -4.305596300791617814, 7.180890229968955651, 1.199719254218452935 ) ) ;
#110203 = CARTESIAN_POINT ( 'NONE',  ( 5.313438862022389131, -0.3376633510823018880, 2.237075724153537504 ) ) ;
#110205 = CARTESIAN_POINT ( 'NONE',  ( 1.471456325463766479, 0.1532790705911575568, -2.100547924479207129 ) ) ;
#110206 = CARTESIAN_POINT ( 'NONE',  ( -4.936050443827081580, 7.916420063510339666, 1.199719254218452935 ) ) ;
#110207 = APPLICATION_CONTEXT ( 'automotive_design' ) ;
#110208 = CARTESIAN_POINT ( 'NONE',  ( 8.762647353133951711, 9.117510088278095282, 1.040834085586084257E-14 ) ) ;
#110209 = CARTESIAN_POINT ( 'NONE',  ( 7.485510208076452621, 7.905719128943566432, 0.000000000000000000 ) ) ;
#110210 = CARTESIAN_POINT ( 'NONE',  ( 8.378074386687003994, 29.50815134976859255, 15.76159487570644835 ) ) ;
#110211 = CARTESIAN_POINT ( 'NONE',  ( -7.985916173649233230, 9.275655943134292869, -1.199719254218446718 ) ) ;
#110212 = UNCERTAINTY_MEASURE_WITH_UNIT (LENGTH_MEASURE( 1.000000000000000082E-05 ), #176099, 'distance_accuracy_value', 'NONE');
#110213 = CARTESIAN_POINT ( 'NONE',  ( 3.009410498757215446, 6.662729348525398443, 0.6539756689588872574 ) ) ;
#110214 = CARTESIAN_POINT ( 'NONE',  ( 7.741342523278705201, 9.094283034322399928, 1.082531754730558626 ) ) ;
#110215 = CARTESIAN_POINT ( 'NONE',  ( 4.230803266364135951, 7.299989629454814555, -0.8951707687023923166 ) ) ;
#110216 = CARTESIAN_POINT ( 'NONE',  ( -7.673551755654729689, 11.89630144833179060, 0.7216878364870458196 ) ) ;
#110218 = CARTESIAN_POINT ( 'NONE',  ( 3.146955363149469331, 2.168125099964354874, 0.4830323043785512138 ) ) ;
#110217 = CARTESIAN_POINT ( 'NONE',  ( 1.810938747355747447, -0.5704394276861005642, -2.042344090522000055 ) ) ;
#110219 = CARTESIAN_POINT ( 'NONE',  ( -0.02244404828157658613, -0.004869073801674199918, -2.189079685368473527 ) ) ;
#110220 = CARTESIAN_POINT ( 'NONE',  ( -4.599959256786493533, 8.588645909551377855, 0.000000000000000000 ) ) ;
#110221 = CARTESIAN_POINT ( 'NONE',  ( 4.137209430464448445, 7.978494768850520558, 1.040834085586084257E-14 ) ) ;
#110222 = CARTESIAN_POINT ( 'NONE',  ( 4.404711838702720428, 0.5211615849865286476, 1.891323523724611766 ) ) ;
#110223 = CARTESIAN_POINT ( 'NONE',  ( 9.565441069641300587, 11.11843498845840905, -1.199719254218440723 ) ) ;
#110224 = CARTESIAN_POINT ( 'NONE',  ( -5.505981461394960697, 6.253680794909101337, 0.9796770575781436063 ) ) ;
#110225 = CARTESIAN_POINT ( 'NONE',  ( -2.081668171172168513E-14, 6.487495393664096888, 3.100011470320013451 ) ) ;
#110226 = CARTESIAN_POINT ( 'NONE',  ( 1.364683531249986537, 0.6135416670080880985, 0.7879004041258500513 ) ) ;
#110227 = CARTESIAN_POINT ( 'NONE',  ( -5.641601317062259646, 5.754492089426966217, -0.7216878364870338292 ) ) ;
#110229 = ORIENTED_EDGE ( 'NONE', *, *, #95445, .T. ) ;
#110228 = CARTESIAN_POINT ( 'NONE',  ( -7.592202833972775622, 8.920286730132099606, 1.082531754730558626 ) ) ;
#110230 = CARTESIAN_POINT ( 'NONE',  ( 2.935903058640790597, -2.042584291827519660, 0.5695675404085094318 ) ) ;
#110231 = CARTESIAN_POINT ( 'NONE',  ( -3.949167883330528372, 7.829389307186077396, 1.214306433183764966E-14 ) ) ;
#110232 = CARTESIAN_POINT ( 'NONE',  ( 4.153314892778156242, -1.795761387672462961, -1.203114871582221079 ) ) ;
#110233 = CARTESIAN_POINT ( 'NONE',  ( 3.614658571667620279, -0.1319153736358945894, 1.836568937333193485 ) ) ;
#110234 = CARTESIAN_POINT ( 'NONE',  ( -4.208837953572873047, 7.367755930811632936, 0.8315943877991900379 ) ) ;
#110235 = CARTESIAN_POINT ( 'NONE',  ( -0.6823417656250003738, 0.2802083336747515641, -1.181850606188749264 ) ) ;
#110236 = CARTESIAN_POINT ( 'NONE',  ( 5.454937174282652457, 0.3337844340769695606, -1.707832357695503234 ) ) ;
#110237 = DIRECTION ( 'NONE',  ( -1.276756478318932585E-15, 1.000000000000000000, -1.665334536937738262E-16 ) ) ;
#110238 = CARTESIAN_POINT ( 'NONE',  ( 4.202664430556257713, 4.965825259479493603, 1.082531754730560403 ) ) ;
#110239 = LINE ( 'NONE', #191397, #170635 ) ;
#110240 = CARTESIAN_POINT ( 'NONE',  ( 3.098656953246520906, -0.6260995091542166380, -2.069055637940686143 ) ) ;
#110241 = CARTESIAN_POINT ( 'NONE',  ( 5.659529772124847646, -0.4871306767523299608, -1.956261131662299535 ) ) ;
#110242 = CARTESIAN_POINT ( 'NONE',  ( -8.148087131688692253, 10.52918762510205042, -1.443375672974058777 ) ) ;
#110243 = CIRCLE ( 'NONE', #203514, 0.07999999999999907185 ) ;
#110244 = CARTESIAN_POINT ( 'NONE',  ( 2.536181837661064087, 1.019768383293401248, -1.906060392209196763 ) ) ;
#110245 = CARTESIAN_POINT ( 'NONE',  ( 3.901606001822624403, -0.5752225463674947026, 1.885544661340606165 ) ) ;
#110246 = CARTESIAN_POINT ( 'NONE',  ( 0.1874131419884322858, 1.628132678060219884, 1.467219630700428157 ) ) ;
#110247 = CARTESIAN_POINT ( 'NONE',  ( 4.897963269493502025, -0.6577025220009655726, -1.827417481390420928 ) ) ;
#110250 = ORIENTED_EDGE ( 'NONE', *, *, #47118, .F. ) ;
#110249 = DIRECTION ( 'NONE',  ( 0.9998757926790049488, 0.01538962834598772353, 0.003399787332178825280 ) ) ;
#110248 = CARTESIAN_POINT ( 'NONE',  ( -8.310784975052682100, 10.71900177569337487, -1.443375672974058777 ) ) ;
#110251 = CARTESIAN_POINT ( 'NONE',  ( -4.769436176957319695, 8.786368983084006601, 0.7998128361456281477 ) ) ;
#110252 = CARTESIAN_POINT ( 'NONE',  ( 11.84104725192634966, 9.990164625485805416, 1.443823348526939165 ) ) ;
#110254 = ORIENTED_EDGE ( 'NONE', *, *, #5825, .F. ) ;
#110253 = CARTESIAN_POINT ( 'NONE',  ( -4.950662367645459305, 5.804802846121667415, -1.199719254218453823 ) ) ;
#110255 = CARTESIAN_POINT ( 'NONE',  ( -9.449669878600625239, 10.12696240122997082, -0.7216878364870267237 ) ) ;
#110256 = CARTESIAN_POINT ( 'NONE',  ( 2.415298318263587873, 1.970979330149217335, 0.9926799514654092160 ) ) ;
#110257 = CARTESIAN_POINT ( 'NONE',  ( 1.001543065824772753E-15, -0.7218749995220414828, 3.793834371823811669 ) ) ;
#110258 = CARTESIAN_POINT ( 'NONE',  ( 6.737165023268617325, -0.09304339776683606678, -1.959646862056351857 ) ) ;
#110259 = CARTESIAN_POINT ( 'NONE',  ( 1.364683531249988535, 5.217708333674750065, -0.7879004041258300672 ) ) ;
#110260 = CARTESIAN_POINT ( 'NONE',  ( -1.201851678989727383E-14, 4.368750000682820378, -1.732050807568863648 ) ) ;
#110261 = CARTESIAN_POINT ( 'NONE',  ( 5.178766244632133642, 6.659365504414815895, -1.397763381526682336 ) ) ;
#110263 = DIRECTION ( 'NONE',  ( 0.000000000000000000, 0.000000000000000000, 1.000000000000000000 ) ) ;
#110262 = CARTESIAN_POINT ( 'NONE',  ( -1.806654366501805775, 0.000000000000000000, 2.420000000000000373 ) ) ;
#110264 = CARTESIAN_POINT ( 'NONE',  ( 5.120983416928425846, -1.747193932927636029, 0.5808180576658967809 ) ) ;
#110265 = ORIENTED_EDGE ( 'NONE', *, *, #194628, .F. ) ;
#110266 = CARTESIAN_POINT ( 'NONE',  ( -1.360316468750032870, -1.088541666325267165, 0.7853790794158641564 ) ) ;
#110267 = CARTESIAN_POINT ( 'NONE',  ( -7.751511138711140170, 10.06651563329490529, -1.599625672291263179 ) ) ;
#110268 = CARTESIAN_POINT ( 'NONE',  ( -0.8666125166525048273, -3.171907292983330183E-14, 0.9704771928531863434 ) ) ;
#110269 = CARTESIAN_POINT ( 'NONE',  ( 6.433838290133602200, -2.056603270127650429, 0.5165238393732355382 ) ) ;
#110270 = DIRECTION ( 'NONE',  ( 0.000000000000000000, -1.000000000000000000, 0.000000000000000000 ) ) ;
#110271 = CARTESIAN_POINT ( 'NONE',  ( 5.443762371086860341, 6.309809840144842141, 1.199719254218462483 ) ) ;
#110272 = CARTESIAN_POINT ( 'NONE',  ( 6.169226111886771946, 0.1559856310293654957, -2.054958193847939096 ) ) ;
#110275 = CARTESIAN_POINT ( 'NONE',  ( 4.229911503591711863, 1.806553461410321582, 0.3548724298726435022 ) ) ;
#110274 = CARTESIAN_POINT ( 'NONE',  ( 2.383057912469242812, -0.003606268183664260163, 1.861241884763777499 ) ) ;
#110273 = CARTESIAN_POINT ( 'NONE',  ( 3.847109862837356786, 4.045599327266925727, -0.8077998227820462063 ) ) ;
#110276 = CARTESIAN_POINT ( 'NONE',  ( 6.825640269476072497, 10.05066518344239412, 1.199719254218460707 ) ) ;
#110277 = CARTESIAN_POINT ( 'NONE',  ( -9.568394635526177083, 14.89572081425755812, -7.242253469718477277 ) ) ;
#110278 = CARTESIAN_POINT ( 'NONE',  ( -7.957709816578236506, 8.248692638954882028, 0.7998128361456341429 ) ) ;
#110280 = VERTEX_POINT ( 'NONE', #63069 ) ;
#110279 = CARTESIAN_POINT ( 'NONE',  ( 0.000000000000000000, 1.000000000000000888, 0.000000000000000000 ) ) ;
#110281 = CARTESIAN_POINT ( 'NONE',  ( 4.283934280384479543, 1.440456688004333019, 1.672026782002330458 ) ) ;
#110282 = CARTESIAN_POINT ( 'NONE',  ( 5.870491743106223126, -1.441790217864300283, 1.743476569090945061 ) ) ;
#110283 = CARTESIAN_POINT ( 'NONE',  ( -5.585596099150193616, 6.579245539505756746, -1.082531754730544860 ) ) ;
#110284 = CARTESIAN_POINT ( 'NONE',  ( 5.959207022242491547, -1.525490245149653701, 0.9768169865009832531 ) ) ;
#110285 = CARTESIAN_POINT ( 'NONE',  ( 6.333208386676280277, -1.543085173044305591, -1.135110930932172746 ) ) ;
#110286 = DIRECTION ( 'NONE',  ( -0.6507913734559640506, -0.7592566023653004592, 0.000000000000000000 ) ) ;
#110287 = ADVANCED_FACE ( 'NONE', ( #129237 ), #163062, .T. ) ;
#110288 = CARTESIAN_POINT ( 'NONE',  ( 6.403191318657627029, 1.556466930477506505, 1.037356966126230517 ) ) ;
#110289 = CARTESIAN_POINT ( 'NONE',  ( 5.953752735127215701, -1.388294428863137586, -1.315342447896154843 ) ) ;
#110290 = CARTESIAN_POINT ( 'NONE',  ( 0.000000000000000000, 9.000000000000000000, 2.080000000000000071 ) ) ;
#110291 = CARTESIAN_POINT ( 'NONE',  ( 1.111929834214450796, -0.8377583890188080584, -1.672643128629976772 ) ) ;
#110292 = CARTESIAN_POINT ( 'NONE',  ( 0.8312679839070147292, -1.592664559859976237, -1.236796411087807801 ) ) ;
#110293 = EDGE_CURVE ( 'NONE', #167139, #47238, #92505, .T. ) ;
#110295 = CARTESIAN_POINT ( 'NONE',  ( 4.459663826605764214, 0.4620033958209149305, -2.054602365452788071 ) ) ;
#110294 = CARTESIAN_POINT ( 'NONE',  ( -9.073431116043565225, 11.60875560684942265, -1.599625672291263179 ) ) ;
#110296 = CARTESIAN_POINT ( 'NONE',  ( 8.072990401933337168, 11.50590700464255356, -1.199719254218446718 ) ) ;
#110298 = CARTESIAN_POINT ( 'NONE',  ( -7.340850106795412167, 10.65174332698158643, 1.199719254218453823 ) ) ;
#110297 = CARTESIAN_POINT ( 'NONE',  ( -0.7500000000000006661, -0.8916666666666448471, -1.299038105676652011 ) ) ;
#110299 = DIRECTION ( 'NONE',  ( 0.000000000000000000, 0.000000000000000000, -1.000000000000000000 ) ) ;
#110300 = CARTESIAN_POINT ( 'NONE',  ( 3.375264624815476289, -1.783316433176849625, -0.9482593927577113169 ) ) ;
#110301 = CARTESIAN_POINT ( 'NONE',  ( -0.6823417656250212460, 3.301041667008085323, 1.181850606188767472 ) ) ;
#110302 = CARTESIAN_POINT ( 'NONE',  ( 9.571693261567954636, 12.19006144329456731, 1.443375672974076540 ) ) ;
#110303 = CARTESIAN_POINT ( 'NONE',  ( 4.868538603872567982, -1.416007186031362330, 1.633285015310452115 ) ) ;
#110304 = CARTESIAN_POINT ( 'NONE',  ( 6.620655732516627090, 7.629137130509076492, 2.426260288887295502 ) ) ;
#110305 = CARTESIAN_POINT ( 'NONE',  ( -1.201851678989727383E-14, 5.587500000000021672, -1.732050807568863648 ) ) ;
#110307 = CARTESIAN_POINT ( 'NONE',  ( -9.590670562336521598, -9.593477663480378226, 0.1674057773689523465 ) ) ;
#110306 = CARTESIAN_POINT ( 'NONE',  ( 7.452141709366786770, 8.723195411463290583, 1.199719254218452047 ) ) ;
#110308 = CARTESIAN_POINT ( 'NONE',  ( 9.395437264145964917, 10.06369101769952934, -0.7216878364870257245 ) ) ;
#110310 = CARTESIAN_POINT ( 'NONE',  ( 8.571448334701180727, 14.94795601790086437, -8.335953519237410347 ) ) ;
#110309 = CARTESIAN_POINT ( 'NONE',  ( 0.4499840099862363330, 1.609255455985519445, 1.457649523623653298 ) ) ;
#110312 = CARTESIAN_POINT ( 'NONE',  ( 0.9602180038516641147, -1.664555262390180257, -0.7873027242753791732 ) ) ;
#110311 = CARTESIAN_POINT ( 'NONE',  ( -6.453317930424837812, 7.591587675992828466, 1.082531754730549967 ) ) ;
#110313 = CARTESIAN_POINT ( 'NONE',  ( 1.364683531249988535, 1.863541667008086211, 0.7879004041258500513 ) ) ;
#110314 = CARTESIAN_POINT ( 'NONE',  ( 1.804482060849887270, 1.621174160030929068, -1.474864209862189579 ) ) ;
#110315 = DIRECTION ( 'NONE',  ( 1.000000000000000000, 0.000000000000000000, 0.000000000000000000 ) ) ;
#110316 = CARTESIAN_POINT ( 'NONE',  ( 2.378104638162964246, 1.391771292293322082, 1.783738300129237508 ) ) ;
#110317 = CARTESIAN_POINT ( 'NONE',  ( -6.775324078527193983, 8.927630729746953264, -1.599625672291263179 ) ) ;
#110319 = AXIS2_PLACEMENT_3D ( 'NONE', #6798, #154151, #106512 ) ;
#110318 = CARTESIAN_POINT ( 'NONE',  ( 0.6823417656249899377, 4.988541667008086655, -1.181850606188754593 ) ) ;
#110320 = CARTESIAN_POINT ( 'NONE',  ( 5.094250900851895025, 7.824382189606214233, 1.140223938556598871 ) ) ;
#110321 = CARTESIAN_POINT ( 'NONE',  ( -1.500000000000008216, 12.99999999999999822, 3.469446951953614189E-15 ) ) ;
#110322 = CARTESIAN_POINT ( 'NONE',  ( 6.536439455564155843, 8.719208346281938304, 1.443375672974065660 ) ) ;
#110323 = CARTESIAN_POINT ( 'NONE',  ( 4.639784515242838303, 0.7573303825321504590, -1.599664492173937358 ) ) ;
#110324 = B_SPLINE_CURVE_WITH_KNOTS ( 'NONE', 3,
 ( #166582, #51777, #117894, #124325, #10466, #159935, #141596, #190285, #125380, #77609, #76540, #191346, #9414, #139434, #59222, #44068 ),
 .UNSPECIFIED., .F., .F.,
 ( 4, 3, 3, 3, 3, 4 ),
 ( 0.000000000000000000, 2.209015272824978271E-05, 5.594181769345698359E-05, 8.979300607464787737E-05, 0.0001236442050441801050, 0.0001574956163004470730 ),
 .UNSPECIFIED. ) ;
#110325 = CARTESIAN_POINT ( 'NONE',  ( 10.09812548408005384, 10.67556790771522124, -0.7998128361456281477 ) ) ;
#110326 = CARTESIAN_POINT ( 'NONE',  ( 0.6750070354940709283, -1.982970624965023410, -0.7094951434080811747 ) ) ;
#110329 = ADVANCED_FACE ( 'NONE', ( #178972 ), #180028, .F. ) ;
#110328 = CARTESIAN_POINT ( 'NONE',  ( 0.7499999999999885647, 0.8166666666666877461, -1.299038105676652899 ) ) ;
#110327 = CARTESIAN_POINT ( 'NONE',  ( 1.364683531249997417, 10.48437500034139802, 2.602085213965210642E-15 ) ) ;
#110330 = CIRCLE ( 'NONE', #13316, 0.1000000000000000333 ) ;
#110331 = CARTESIAN_POINT ( 'NONE',  ( -6.120580001926503755, 6.105374521861167914, -0.7998128361456362523 ) ) ;
#110332 = CARTESIAN_POINT ( 'NONE',  ( 5.958611281643053204, -1.915606116362132072, -0.6298603123368745615 ) ) ;
#110334 = ORIENTED_EDGE ( 'NONE', *, *, #132306, .T. ) ;
#110333 = CARTESIAN_POINT ( 'NONE',  ( 5.045072953846708508, 0.1408599011454790551, 1.806194821104394777 ) ) ;
#110335 = CARTESIAN_POINT ( 'NONE',  ( 10.26082332744404368, 10.86538205830655279, -0.7998128361456281477 ) ) ;
#110336 = CARTESIAN_POINT ( 'NONE',  ( 3.238977024203249400, -1.650389259550872456, 0.8806316622528218563 ) ) ;
#110337 = CARTESIAN_POINT ( 'NONE',  ( 4.856339096887199780, -2.069677458173447171, -0.05615216265978521804 ) ) ;
#110338 = CARTESIAN_POINT ( 'NONE',  ( -5.411112705185557203, 9.327065566109540740, 0.7216878364870267237 ) ) ;
#110339 = DIRECTION ( 'NONE',  ( -1.276756478318932585E-15, 1.000000000000000000, -1.665334536937738262E-16 ) ) ;
#110340 = CARTESIAN_POINT ( 'NONE',  ( 8.320953590485093088, 10.73086516036454618, 1.599625672291281386 ) ) ;
#110341 = CARTESIAN_POINT ( 'NONE',  ( -1.523896559881120938, 8.692074762372739016, 2.522933744808692147 ) ) ;
#110342 = CARTESIAN_POINT ( 'NONE',  ( 5.993586425693011144, 9.150212042353954800, -1.199719254218452047 ) ) ;
#110343 = EDGE_CURVE ( 'NONE', #58157, #192481, #97726, .T. ) ;
#110344 = CARTESIAN_POINT ( 'NONE',  ( -4.911139836396910319, 4.690354089464431553, -0.3431232535803417916 ) ) ;
#110345 = CARTESIAN_POINT ( 'NONE',  ( 1.364683531249990311, 5.676041667008088432, 0.7879004041258500513 ) ) ;
#110346 = CARTESIAN_POINT ( 'NONE',  ( 3.648837080137564470, -0.3802854374791163616, -1.924481129451253603 ) ) ;
#110347 = CARTESIAN_POINT ( 'NONE',  ( 1.177110994959302825, -0.9039684864705423983, -1.802142742073430171 ) ) ;
#110348 = CARTESIAN_POINT ( 'NONE',  ( -4.065465959251405081, 5.836405933916976707, -1.599625672291271394 ) ) ;
#110349 = CARTESIAN_POINT ( 'NONE',  ( 6.760712154708803823, 11.03924794713562818, 1.040834085586084257E-14 ) ) ;
#110350 = CARTESIAN_POINT ( 'NONE',  ( 0.9834252619641962179, 1.251819791611600285, 1.390119989509101650 ) ) ;
#110351 = CARTESIAN_POINT ( 'NONE',  ( 1.364683531249990311, 3.634375000341416584, 1.214306433183764966E-14 ) ) ;
#110352 = CARTESIAN_POINT ( 'NONE',  ( 2.970950383256478755, -1.521771678934441097, 1.318087423592265717 ) ) ;
#110354 = CARTESIAN_POINT ( 'NONE',  ( 3.339577153505444151, 0.5119293057267596536, -2.054306502313862470 ) ) ;
#110353 = CARTESIAN_POINT ( 'NONE',  ( -5.097502569058207200, 8.890910730635814829, -0.7216878364870207285 ) ) ;
#110355 = CARTESIAN_POINT ( 'NONE',  ( 6.825078400183551608, 0.5660753733540256905, 2.196387875007102419 ) ) ;
#110356 = CARTESIAN_POINT ( 'NONE',  ( 5.441872305809390298, 1.387781221417656141, 1.536568222347669987 ) ) ;
#110357 = CARTESIAN_POINT ( 'NONE',  ( 5.996449078994045223, 10.21788403546024782, 0.7998128361456331437 ) ) ;
#110359 = CARTESIAN_POINT ( 'NONE',  ( 11.84668729410370602, 13.50620512324527134, 1.399999999999998357 ) ) ;
#110358 = CARTESIAN_POINT ( 'NONE',  ( 6.615180898807764720, -2.028213694748048024, 0.5066274125750843682 ) ) ;
#110361 = ORIENTED_EDGE ( 'NONE', *, *, #140329, .F. ) ;
#110360 = CARTESIAN_POINT ( 'NONE',  ( 5.051681782491273864, 0.5714109786712183725, -1.733901259708306331 ) ) ;
#110362 = CARTESIAN_POINT ( 'NONE',  ( 9.250740883225924804, 9.686952540052077509, 1.040834085586084257E-14 ) ) ;
#110363 = CARTESIAN_POINT ( 'NONE',  ( 6.639320575229281651, -0.0007625845807879281287, 2.103388539994067497 ) ) ;
#110364 = CARTESIAN_POINT ( 'NONE',  ( 10.81010058466664425, 10.31570469300483950, 6.498163104334348183 ) ) ;
#110365 = CARTESIAN_POINT ( 'NONE',  ( 6.721690211428396289, -2.142211831252617493, 0.5295551626897446740 ) ) ;
#110366 = CARTESIAN_POINT ( 'NONE',  ( -1.402160292154681736E-14, 11.73437500034140335, 1.575800808251682339 ) ) ;
#110367 = CARTESIAN_POINT ( 'NONE',  ( 4.969353466749234727, -1.617520173792227567, -1.019718193788564209 ) ) ;
#110368 = CARTESIAN_POINT ( 'NONE',  ( -9.429859533504656000, 10.96025652963230534, -1.199719254218441611 ) ) ;
#110369 = CIRCLE ( 'NONE', #93007, 0.07999999999999998779 ) ;
#110370 = CARTESIAN_POINT ( 'NONE',  ( 6.388916700537700777, 8.476822122092563916, 1.599625672291281386 ) ) ;
#110371 = CARTESIAN_POINT ( 'NONE',  ( -1.360316468750048857, 2.651041667008094294, -0.7853790794159161148 ) ) ;
#110372 = CARTESIAN_POINT ( 'NONE',  ( 3.294268137996273715, 5.826768013428865522, -1.082531754730543971 ) ) ;
#110373 = DIRECTION ( 'NONE',  ( 0.000000000000000000, 0.000000000000000000, -1.000000000000000000 ) ) ;
#110374 = CARTESIAN_POINT ( 'NONE',  ( 4.147904930777053245, 6.926640621626830807, -1.199719254218452047 ) ) ;
#110375 = ORIENTED_EDGE ( 'NONE', *, *, #208819, .F. ) ;
#110376 = CARTESIAN_POINT ( 'NONE',  ( 8.064677165291193717, -5.223431457505076203, -7.446209719563348983 ) ) ;
#110377 = CARTESIAN_POINT ( 'NONE',  ( -0.02299388927992032997, 5.724334336916190757, -2.505015335112478425 ) ) ;
#110378 = CARTESIAN_POINT ( 'NONE',  ( 4.857564175446106525, 8.889184981320973122, 0.7998128361456331437 ) ) ;
#110379 = CARTESIAN_POINT ( 'NONE',  ( -0.3870735955438814879, 1.000000000000000888, 11.88799243440809050 ) ) ;
#110380 = VECTOR ( 'NONE', #21081, 1000.000000000000000 ) ;
#110381 = CARTESIAN_POINT ( 'NONE',  ( -5.865985541149716376, 7.193105608424513520, 1.152625159504708119 ) ) ;
#110382 = CARTESIAN_POINT ( 'NONE',  ( -5.368665641331555882, 8.246898433986675769, 1.082531754730548412 ) ) ;
#110383 = CARTESIAN_POINT ( 'NONE',  ( 2.659370686574860976, 6.254349567645977714, -0.7998128361456291469 ) ) ;
#110384 = CARTESIAN_POINT ( 'NONE',  ( 2.395301122324170695, -1.761490415372953589, 0.8809153588016715997 ) ) ;
#110385 = CARTESIAN_POINT ( 'NONE',  ( 3.532827515057835654, -1.646827434736859441, 1.163287548526056980 ) ) ;
#110386 = CARTESIAN_POINT ( 'NONE',  ( -8.019811557683421910, 9.315200557840817908, 1.199719254218462483 ) ) ;
#110387 = CARTESIAN_POINT ( 'NONE',  ( 5.391302360089590628, 6.318882837306503575, -1.199719254218452047 ) ) ;
#110388 = CARTESIAN_POINT ( 'NONE',  ( 6.827182134110205247, 2.955377424523279117, 2.541486622063714673 ) ) ;
#110389 = CARTESIAN_POINT ( 'NONE',  ( 3.398540877415173966, 1.727514402264049620, -1.348270469230819391 ) ) ;
#110390 = FACE_BOUND ( 'NONE', #74488, .T. ) ;
#110391 = CARTESIAN_POINT ( 'NONE',  ( 1.782126058915745936, -1.032679515686143024, 1.626040290554785717 ) ) ;
#110392 = CARTESIAN_POINT ( 'NONE',  ( -9.104463846776669200, 10.58062822844965645, -1.199719254218441611 ) ) ;
#110393 = FILL_AREA_STYLE ('',( #191552 ) ) ;
#110394 = CARTESIAN_POINT ( 'NONE',  ( 0.2333540202161610289, 0.003568502611739353923, -2.045944795905803471 ) ) ;
#110395 = CARTESIAN_POINT ( 'NONE',  ( 3.770576118376306241, 6.452737000530752276, 1.082531754730549078 ) ) ;
#110396 = CARTESIAN_POINT ( 'NONE',  ( 7.313733799568044702, 10.62010763521636214, 1.199719254218460707 ) ) ;
#110397 = CARTESIAN_POINT ( 'NONE',  ( -6.520158902580853066, 5.290451655908523065, -2.438235897557453846 ) ) ;
#110398 = CARTESIAN_POINT ( 'NONE',  ( 4.407809338218622308, 8.156544971314787063, 0.000000000000000000 ) ) ;
#110399 = EDGE_LOOP ( 'NONE', ( #13338, #121596, #88589, #130605, #148939, #153979 ) ) ;
#110401 = CARTESIAN_POINT ( 'NONE',  ( 2.649090073008007362, 0.2487567141898557876, 1.997615136964459470 ) ) ;
#110400 = CARTESIAN_POINT ( 'NONE',  ( 6.321814700078944860, 1.054209175812788502, -1.509406368332133930 ) ) ;
#110402 = CARTESIAN_POINT ( 'NONE',  ( 4.745672437882476835, -2.227950070917711134, -0.5642311211754289513 ) ) ;
#110404 = CARTESIAN_POINT ( 'NONE',  ( 1.709564315929460232, 0.5465817987246027743, -1.778839887662834185 ) ) ;
#110403 = CARTESIAN_POINT ( 'NONE',  ( -0.1288028175206907822, -0.008968661790493319408, -2.273875003271645934 ) ) ;
#110405 = CARTESIAN_POINT ( 'NONE',  ( -1.642778471874998480, -2.151041666188707957, 2.845375778867863303 ) ) ;
#110406 = CARTESIAN_POINT ( 'NONE',  ( -4.613268803136618246, 8.378775596900176481, 0.2107346534404584415 ) ) ;
#110407 = CARTESIAN_POINT ( 'NONE',  ( 5.449440537890920311, -1.726199344983204265, 0.8234401749890255529 ) ) ;
#110408 = CARTESIAN_POINT ( 'NONE',  ( -6.723954117373590833, 9.932031339322813679, -1.199719254218440723 ) ) ;
#110409 = EDGE_CURVE ( 'NONE', #12777, #211051, #120939, .T. ) ;
#110410 = CARTESIAN_POINT ( 'NONE',  ( -5.533136088152923904, 6.588318536667425285, 1.082531754730549078 ) ) ;
#110412 = CARTESIAN_POINT ( 'NONE',  ( 3.906994808788874174, 1.604092888448312326, 0.9621832354540849064 ) ) ;
#110411 = CARTESIAN_POINT ( 'NONE',  ( 5.003505698738024421, -2.080571448108500476, 0.2061593518874194064 ) ) ;
#110413 = CARTESIAN_POINT ( 'NONE',  ( 6.100805936469477331, 9.101062111647635788, -1.082531754730537088 ) ) ;
#110414 = VECTOR ( 'NONE', #97170, 1000.000000000000000 ) ;
#110415 = DIRECTION ( 'NONE',  ( -1.000000000000000000, 0.000000000000000000, -5.551115123125765446E-17 ) ) ;
#110416 = FACE_OUTER_BOUND ( 'NONE', #210072, .T. ) ;
#110417 = CARTESIAN_POINT ( 'NONE',  ( 5.760297821273290708, 0.7050700890500715134, 1.574392225784694066 ) ) ;
#110418 = CARTESIAN_POINT ( 'NONE',  ( -4.740547266272593596, 8.682388910626682943, -0.7998128361456281477 ) ) ;
#110419 = CARTESIAN_POINT ( 'NONE',  ( 1.670155932360503970, 1.196126419257515838, 1.255837360413303738 ) ) ;
#110420 = CARTESIAN_POINT ( 'NONE',  ( -11.84668730067608244, 11.00636224908218530, -1.400000000000002132 ) ) ;
#110421 = CARTESIAN_POINT ( 'NONE',  ( 6.539320575229233157, 0.001224430076711413356, 2.103502572931112091 ) ) ;
#110422 = CARTESIAN_POINT ( 'NONE',  ( 6.315638730379727228, -1.320822524126588515, -1.523799118890494020 ) ) ;
#110423 = CARTESIAN_POINT ( 'NONE',  ( 6.157114316693172995, 1.779627781583184909, -1.243356570269833483 ) ) ;
#110424 = CARTESIAN_POINT ( 'NONE',  ( 4.898959864523320107, 1.516061528642864253, -1.016892643307308441 ) ) ;
#110425 = CARTESIAN_POINT ( 'NONE',  ( 2.061309051315598051, 1.628117514333087934, 1.094105149622534467 ) ) ;
#110426 = CARTESIAN_POINT ( 'NONE',  ( 0.2283145101530216492, 2.111890517744571927, 0.1509969543822299032 ) ) ;
#110427 = CARTESIAN_POINT ( 'NONE',  ( -8.319899820280397762, 12.85830022363583147, -0.7998128361456281477 ) ) ;
#110428 = CARTESIAN_POINT ( 'NONE',  ( 9.074484886248265880, 9.481320543578137361, 0.7998128361456462443 ) ) ;
#110429 = CARTESIAN_POINT ( 'NONE',  ( 2.561320117580662803, -1.761587792986643475, 1.180070990429403555 ) ) ;
#110430 = CARTESIAN_POINT ( 'NONE',  ( -3.714570900464290393, 5.356752022006865843, 1.443375672974064550 ) ) ;
#110431 =( GEOMETRIC_REPRESENTATION_CONTEXT ( 3 ) GLOBAL_UNCERTAINTY_ASSIGNED_CONTEXT ( ( #34205 ) ) GLOBAL_UNIT_ASSIGNED_CONTEXT ( ( #105597, #120830, #20031 ) ) REPRESENTATION_CONTEXT ( 'NONE', 'WORKASPACE' ) );
#110432 = DIRECTION ( 'NONE',  ( 1.000000000000000000, 0.000000000000000000, 0.000000000000000000 ) ) ;
#110433 = CARTESIAN_POINT ( 'NONE',  ( -5.662059632048889846, 6.153064387560178261, -0.8011038117717106388 ) ) ;
#110434 = CARTESIAN_POINT ( 'NONE',  ( 6.983263157960363010, -0.009046620988246899253, 2.153544821522495489 ) ) ;
#110436 = CARTESIAN_POINT ( 'NONE',  ( -0.7500000000000006661, 14.23958333401613352, -1.299038105676657340 ) ) ;
#110435 = CARTESIAN_POINT ( 'NONE',  ( -9.869385822740339265, 3.553052390425875284, 6.766708219044660133 ) ) ;
#110438 = VERTEX_POINT ( 'NONE', #76377 ) ;
#110437 = CARTESIAN_POINT ( 'NONE',  ( 3.809420206217276395, 1.876102094647231988, -1.189034995700769981 ) ) ;
#110439 = CARTESIAN_POINT ( 'NONE',  ( 1.214008909562364069, 2.217199183031343779, 0.6065299581617057401 ) ) ;
#110441 = CARTESIAN_POINT ( 'NONE',  ( 5.225460488781804358, 0.2076664479006613828, -2.052122333454815539 ) ) ;
#110440 = CARTESIAN_POINT ( 'NONE',  ( 4.356247428692526569, 3.976710176429713250, 0.7998128361456341429 ) ) ;
#110443 = CARTESIAN_POINT ( 'NONE',  ( -3.475000000000000533, -2.829166666666666607, -2.006292185433948827 ) ) ;
#110442 = CARTESIAN_POINT ( 'NONE',  ( 3.705121118284530279, 7.544668081299086282, -1.734723475976807094E-15 ) ) ;
#110444 = CARTESIAN_POINT ( 'NONE',  ( 0.2329586101569320611, 0.7537478099126624365, -1.931748487665209124 ) ) ;
#110445 = CARTESIAN_POINT ( 'NONE',  ( 5.882333747326812023, -0.2767177626767613474, -1.820229446528654371 ) ) ;
#110446 = CARTESIAN_POINT ( 'NONE',  ( 0.000000000000000000, 0.5000000000000004441, 0.000000000000000000 ) ) ;
#110447 = CARTESIAN_POINT ( 'NONE',  ( 4.542145155778077203, 5.257923088951247159, -1.199719254218452047 ) ) ;
#110448 = CARTESIAN_POINT ( 'NONE',  ( -0.1104750535120025690, -0.004616138082884356161, -2.103378236956428893 ) ) ;
#110449 = CARTESIAN_POINT ( 'NONE',  ( 2.432253191915220825, 1.672178088080849223, 0.4220979471536658867 ) ) ;
#110450 = CARTESIAN_POINT ( 'NONE',  ( 1.217982839071569012, 0.9896824804975332679, -1.756856037137773940 ) ) ;
#110451 = CARTESIAN_POINT ( 'NONE',  ( 3.041888879667261403, -1.739239095176773775, 1.503071639953108773 ) ) ;
#110452 = CARTESIAN_POINT ( 'NONE',  ( 2.847247395794590297, -1.882567391055539385, 1.254484791939513899 ) ) ;
#110453 = CARTESIAN_POINT ( 'NONE',  ( 5.391282926306558032, 1.858022621660906371, -0.9916069233004040084 ) ) ;
#110454 = CARTESIAN_POINT ( 'NONE',  ( -6.943184063974178422, 8.233374508458908281, -1.082531754730549967 ) ) ;
#110455 = CARTESIAN_POINT ( 'NONE',  ( 3.356489944714312834, -1.342140201951192102, 1.153657164820639958 ) ) ;
#110457 = CARTESIAN_POINT ( 'NONE',  ( 6.005493137707444973, -2.275576565988911337, 0.2767016799969032603 ) ) ;
#110456 = CARTESIAN_POINT ( 'NONE',  ( 5.519577934094864524, 5.612131475965050242, 0.7216878364870328300 ) ) ;
#110458 = CARTESIAN_POINT ( 'NONE',  ( 4.576008823784957436, -1.786506429242448624, -0.4446734633927542091 ) ) ;
#110459 = CARTESIAN_POINT ( 'NONE',  ( -3.276266675996675204, 6.974061555304760240, -0.7998128361456281477 ) ) ;
#110460 = UNCERTAINTY_MEASURE_WITH_UNIT (LENGTH_MEASURE( 1.000000000000000082E-05 ), #176010, 'distance_accuracy_value', 'NONE');
#110461 = CARTESIAN_POINT ( 'NONE',  ( 5.680503174001485078, 6.689970460165617361, -1.082531754730543083 ) ) ;
#110462 = CARTESIAN_POINT ( 'NONE',  ( 0.7499999999999902300, 3.233333333333352044, 1.299038105676669330 ) ) ;
#110463 = CARTESIAN_POINT ( 'NONE',  ( 4.681673494351117348, -1.034495392153191418, 1.931897795048514554 ) ) ;
#110464 = CARTESIAN_POINT ( 'NONE',  ( -5.447678794592645701, 5.250046769979851646, 0.000000000000000000 ) ) ;
#110465 = FACE_OUTER_BOUND ( 'NONE', #48726, .T. ) ;
#110466 = CARTESIAN_POINT ( 'NONE',  ( 4.949704645232674061, 1.531818663031824013, 1.392983054852282132 ) ) ;
#110467 = CARTESIAN_POINT ( 'NONE',  ( -1.499999999999993339, 10.64264068711930733, 1.232676135170975238E-14 ) ) ;
#110468 = CARTESIAN_POINT ( 'NONE',  ( 0.6823417656249899377, 4.926041667008086655, -1.181850606188754593 ) ) ;
#110469 = CARTESIAN_POINT ( 'NONE',  ( 3.510301166856438115, -0.7815644168660453861, -1.761018089871415393 ) ) ;
#110470 = CARTESIAN_POINT ( 'NONE',  ( -1.364683531250010295, 9.130208333674731946, 0.7879004041258445001 ) ) ;
#110471 = CARTESIAN_POINT ( 'NONE',  ( -2.494337075234348777, 5.853884321174607663, -0.7216878364870267237 ) ) ;
#110472 = CARTESIAN_POINT ( 'NONE',  ( 0.0006278483607258588750, -1.039594266688011137, 1.963129682597685166 ) ) ;
#110473 = ORIENTED_EDGE ( 'NONE', *, *, #95445, .F. ) ;
#110475 = FACE_OUTER_BOUND ( 'NONE', #38621, .T. ) ;
#110474 = CARTESIAN_POINT ( 'NONE',  ( 1.499999999999990674, 8.226407212580426176, -3.114167208185174118 ) ) ;
#110476 = CARTESIAN_POINT ( 'NONE',  ( 4.650610384687404952, 5.384465856012134566, 1.199719254218462483 ) ) ;
#110477 = CARTESIAN_POINT ( 'NONE',  ( -4.161989969715295778, 4.726297878971393196, 2.500000000000011102 ) ) ;
#110478 =( LENGTH_UNIT ( ) NAMED_UNIT ( * ) SI_UNIT ( .MILLI., .METRE. ) );
#110479 = AXIS2_PLACEMENT_3D ( 'NONE', #104661, #185874, #154474 ) ;
#110480 = DIRECTION ( 'NONE',  ( 0.000000000000000000, 0.000000000000000000, -1.000000000000000000 ) ) ;
#110481 = CARTESIAN_POINT ( 'NONE',  ( 5.192409644353875642, 5.160158794608717514, 1.040834085586084257E-14 ) ) ;
#110482 = CARTESIAN_POINT ( 'NONE',  ( 1.099968687278202406, 0.7983322178258808188, -1.792280776234014050 ) ) ;
#110483 = CARTESIAN_POINT ( 'NONE',  ( 0.6823417656249882723, 1.488541667008083547, -1.181850606188749264 ) ) ;
#110484 = AXIS2_PLACEMENT_3D ( 'NONE', #63724, #93060, #12824 ) ;
#110485 = CARTESIAN_POINT ( 'NONE',  ( 5.928642344448160628, 2.082074431819755045, 0.5810635428650026135 ) ) ;
#110486 = CARTESIAN_POINT ( 'NONE',  ( 5.406682003534418079, 0.5678430586343993225, 1.877905798087247335 ) ) ;
#110487 = CARTESIAN_POINT ( 'NONE',  ( -8.123306592882240551, 12.62894145833798376, 0.000000000000000000 ) ) ;
#110488 = CARTESIAN_POINT ( 'NONE',  ( -6.385527161912131433, 6.552129231760014605, 0.7216878364870317197 ) ) ;
#110489 = CARTESIAN_POINT ( 'NONE',  ( 5.735289742212391850, -1.956171686333206816, 0.9202595734885756773 ) ) ;
#110491 = EDGE_LOOP ( 'NONE', ( #79343, #113394, #92564, #44316 ) ) ;
#110490 = CARTESIAN_POINT ( 'NONE',  ( -0.1368885365587547698, -5.294776013890321487, -10.99935770452674610 ) ) ;
#110492 = CARTESIAN_POINT ( 'NONE',  ( 1.364683531249988535, 4.363541667008090208, 0.7879004041258500513 ) ) ;
#110493 = CARTESIAN_POINT ( 'NONE',  ( 6.608667082420285332, 1.462428336960637676, -1.322156044359092064 ) ) ;
#110494 = CARTESIAN_POINT ( 'NONE',  ( 6.134130222960958889, 0.1235499018571624141, -1.729521282446895070 ) ) ;
#110496 = CARTESIAN_POINT ( 'NONE',  ( 2.525153347276567484, -2.043736813514348771, 0.7916865192442237298 ) ) ;
#110495 = CARTESIAN_POINT ( 'NONE',  ( 1.360316468749953600, 0.4947916670081083934, 0.7853790794158861388 ) ) ;
#110497 = CARTESIAN_POINT ( 'NONE',  ( 4.401628477801726724, 1.850755835686506590, 1.378093606121533199 ) ) ;
#110498 = CARTESIAN_POINT ( 'NONE',  ( 5.378222296270031677, -1.148346438381561363, 1.710960936357192264 ) ) ;
#110499 = CARTESIAN_POINT ( 'NONE',  ( 1.570153368812776229, -1.843976851262040029, -0.6092462720258711162 ) ) ;
#110500 = CARTESIAN_POINT ( 'NONE',  ( -7.171900071504754060, 7.469564292951421436, -0.7216878364870267237 ) ) ;
#110501 = CARTESIAN_POINT ( 'NONE',  ( 5.589586000038863745, 5.798386900100804375, -0.7226491117988718127 ) ) ;
#110502 = CARTESIAN_POINT ( 'NONE',  ( 5.045234882716379765, 0.1584239314957915090, 2.114765283346302205 ) ) ;
#110503 = CARTESIAN_POINT ( 'NONE',  ( 2.180314765559120183, 1.560501322096979449, 1.277041908422072991 ) ) ;
#110504 = CARTESIAN_POINT ( 'NONE',  ( -5.870317324592812191, 7.871789516823500144, -1.443375672974051449 ) ) ;
#110505 = CARTESIAN_POINT ( 'NONE',  ( 5.210101597250164751, -2.196594437182074255, 0.2116553293704941940 ) ) ;
#110506 = CARTESIAN_POINT ( 'NONE',  ( -6.770317605177755382, 8.992066187497757213, 1.599625672291269396 ) ) ;
#110507 = CARTESIAN_POINT ( 'NONE',  ( -1.501780004532949908, -3.122141865171504271, -3.051664013761996141 ) ) ;
#110508 = CARTESIAN_POINT ( 'NONE',  ( 0.08226035653636187828, -1.769965142718381124, -0.4472663993063328847 ) ) ;
#110509 = CARTESIAN_POINT ( 'NONE',  ( -7.761116589180078407, 8.019333873657032541, 0.000000000000000000 ) ) ;
#110511 = CARTESIAN_POINT ( 'NONE',  ( 5.843201017809841247, 5.919415396974013532, 1.040834085586084257E-14 ) ) ;
#110510 = CARTESIAN_POINT ( 'NONE',  ( -5.773448424614897156, 7.353550462951784716, 1.313087523158409153 ) ) ;
#110512 = CARTESIAN_POINT ( 'NONE',  ( -4.810269800901881609, 8.163507479013537349, 0.8607707128150362541 ) ) ;
#110513 = ORIENTED_EDGE ( 'NONE', *, *, #15140, .T. ) ;
#110514 = CARTESIAN_POINT ( 'NONE',  ( 4.750885258907265651, -1.656392207783722315, 1.226022070186979063 ) ) ;
#110515 = CARTESIAN_POINT ( 'NONE',  ( 4.033527471555918176, 7.762610268090422316, -0.4095974594184521034 ) ) ;
#110516 = CARTESIAN_POINT ( 'NONE',  ( 0.1980946632348811465, -8.057097448493964365, 9.531438498077058341 ) ) ;
#110517 = CARTESIAN_POINT ( 'NONE',  ( -4.904298879841297421, 6.744767997946721216, 1.599625672291267398 ) ) ;
#110518 = CARTESIAN_POINT ( 'NONE',  ( -3.654804927335652209, 6.421633627603656080, 1.199719254218452935 ) ) ;
#110519 = CARTESIAN_POINT ( 'NONE',  ( 4.688151973431080144, 1.164670015804763370, 1.649827500200540253 ) ) ;
#110521 = VERTEX_POINT ( 'NONE', #19636 ) ;
#110520 = CARTESIAN_POINT ( 'NONE',  ( 1.499999999999987121, 0.7541666666666868579, 0.8660254037844524744 ) ) ;
#110523 = CARTESIAN_POINT ( 'NONE',  ( 8.256552361042350796, 12.57646882128404187, 1.040834085586084257E-14 ) ) ;
#110522 = CARTESIAN_POINT ( 'NONE',  ( -3.983063267364693960, 7.868933921892603323, -0.7998128361456481317 ) ) ;
#110524 = CARTESIAN_POINT ( 'NONE',  ( 5.635385404774530649, 9.726366738878972740, 0.7998128361456462443 ) ) ;
#110525 = CARTESIAN_POINT ( 'NONE',  ( 4.082927109850850833, -0.2000173336921743650, -2.051146848037002979 ) ) ;
#110526 = CARTESIAN_POINT ( 'NONE',  ( 3.094375128876575065, -0.3905979561782264575, 1.978050703236901686 ) ) ;
#110527 = EDGE_LOOP ( 'NONE', ( #163041, #39203, #39600, #166467 ) ) ;
#110528 = CARTESIAN_POINT ( 'NONE',  ( 6.727182134110194944, 2.413774403037728167, 2.569658639860139093 ) ) ;
#110529 = CARTESIAN_POINT ( 'NONE',  ( 3.948449050077836642, 5.629609863222681199, 1.599625672291267398 ) ) ;
#110531 = ORIENTED_EDGE ( 'NONE', *, *, #63733, .F. ) ;
#110530 = CARTESIAN_POINT ( 'NONE',  ( -6.071018923869249129, 10.30488218781460574, 0.7998128361456291469 ) ) ;
#110532 = CARTESIAN_POINT ( 'NONE',  ( 2.864611068004913275, -0.6351033500862738324, 1.913510180259501592 ) ) ;
#110533 = CARTESIAN_POINT ( 'NONE',  ( 2.079791654855645877, -1.805462111169679584, -0.3597937517794968509 ) ) ;
#110534 = CARTESIAN_POINT ( 'NONE',  ( 0.7687468715882056491, 1.142267183891092053, 2.005099294460314319 ) ) ;
#110535 = CARTESIAN_POINT ( 'NONE',  ( 5.761288931164342486, 5.686201605971993978, -0.7998128361456481317 ) ) ;
#110536 = ADVANCED_FACE ( 'NONE', ( #34815 ), #191194, .T. ) ;
#110537 = CARTESIAN_POINT ( 'NONE',  ( 2.513140823169751847, 1.929641211675875878, 0.9743453106897670413 ) ) ;
#110538 = CARTESIAN_POINT ( 'NONE',  ( -6.226218857173722476, 8.287007971501239467, 1.599625672291283607 ) ) ;
#110539 = EDGE_CURVE ( 'NONE', #20115, #210323, #132375, .T. ) ;
#110540 = VERTEX_POINT ( 'NONE', #165903 ) ;
#110541 = CARTESIAN_POINT ( 'NONE',  ( 1.498681428038322050, 1.531199225506232553, -1.074333469806128427 ) ) ;
#110542 = CARTESIAN_POINT ( 'NONE',  ( 5.612177202991157188, -0.8859793764278474093, -1.761228054870385806 ) ) ;
#110544 = CARTESIAN_POINT ( 'NONE',  ( 8.392133896734662812, 10.81390885098904420, 1.443375672974076540 ) ) ;
#110543 = CARTESIAN_POINT ( 'NONE',  ( -0.6823417656249969321, 3.717708333674754506, -1.181850606188749264 ) ) ;
#110546 = CARTESIAN_POINT ( 'NONE',  ( 0.3115100037339203487, 1.922317768103290803, 1.083863418116323807 ) ) ;
#110545 = CARTESIAN_POINT ( 'NONE',  ( -7.335124800193271177, 8.516399340768996851, -1.199719254218452935 ) ) ;
#110547 = CARTESIAN_POINT ( 'NONE',  ( 6.777786256569462431, -2.009253640576996514, 0.4989836931604470505 ) ) ;
#110548 = CARTESIAN_POINT ( 'NONE',  ( 7.169564303528210836, 7.258913197071374945, -0.7998128361456281477 ) ) ;
#110549 = CARTESIAN_POINT ( 'NONE',  ( -5.545448523189368650, 6.428443684264421698, -1.199719254218446718 ) ) ;
#110550 = CARTESIAN_POINT ( 'NONE',  ( 6.639320575229251453, 6.034321252505787214, 2.798156424428144717 ) ) ;
#110551 = CARTESIAN_POINT ( 'NONE',  ( 5.383651750111712708, 1.323420565077202182, 1.461416689776244615 ) ) ;
#110552 = CARTESIAN_POINT ( 'NONE',  ( 6.293224362130668936, -0.1031327824093461465, -2.017302584901353946 ) ) ;
#110553 = CARTESIAN_POINT ( 'NONE',  ( 0.7499999999999867883, 0.09791666734948467621, -1.299038105676652899 ) ) ;
#110554 = CARTESIAN_POINT ( 'NONE',  ( 4.301628547034565209, 1.852045629758605649, 1.376555262909467947 ) ) ;
#110555 = EDGE_CURVE ( 'NONE', #55041, #57699, #164835, .T. ) ;
#110556 = CARTESIAN_POINT ( 'NONE',  ( 1.463816541924748638, -0.5049463793320208005, 1.999668334691290683 ) ) ;
#110557 = CARTESIAN_POINT ( 'NONE',  ( 7.076992996653421741, 10.23994701519558781, -1.082531754730537976 ) ) ;
#110558 = CARTESIAN_POINT ( 'NONE',  ( 4.746236293235721604, 7.694970221153795364, 1.199719254218451159 ) ) ;
#110559 = CARTESIAN_POINT ( 'NONE',  ( 5.761288931164342486, 5.686201605971993978, -0.7998128361456481317 ) ) ;
#110560 = CARTESIAN_POINT ( 'NONE',  ( -1.364683531250012516, 2.551041667008089320, -0.7879004041258289570 ) ) ;
#110561 = CARTESIAN_POINT ( 'NONE',  ( -0.7616041399369541942, 14.48136325226530019, 12.01010946711977567 ) ) ;
#110562 = CARTESIAN_POINT ( 'NONE',  ( 4.812781342726850653, 8.558735966582574406, 0.7216878364870438212 ) ) ;
#110563 = CARTESIAN_POINT ( 'NONE',  ( 4.826735082517537023, -1.421624449711873295, 1.641102681368050487 ) ) ;
#110565 = CARTESIAN_POINT ( 'NONE',  ( 4.423293856316495187, -1.136390847421838490, -1.448631019334602144 ) ) ;
#110564 = CARTESIAN_POINT ( 'NONE',  ( -4.473827502829599290, 4.321812962830357208, 0.7216878364870317197 ) ) ;
#110567 = DIRECTION ( 'NONE',  ( 0.000000000000000000, -0.000000000000000000, -1.000000000000000000 ) ) ;
#110566 = DIRECTION ( 'NONE',  ( 0.000000000000000000, -1.000000000000000000, 0.000000000000000000 ) ) ;
#110568 = CARTESIAN_POINT ( 'NONE',  ( 5.812113132715003516, 1.472855484078567700, -1.623034594306454137 ) ) ;
#110569 = CARTESIAN_POINT ( 'NONE',  ( -11.01135777277262306, 11.00623004977699715, -1.400000000000002132 ) ) ;
#110570 = CARTESIAN_POINT ( 'NONE',  ( 6.051720714260678591, 0.6634699467917944959, -2.163057363297292035 ) ) ;
#110571 = CARTESIAN_POINT ( 'NONE',  ( -4.038790540952651220, 7.763523381248250033, -0.5490930765432913141 ) ) ;
#110572 = CARTESIAN_POINT ( 'NONE',  ( 11.43204722947019825, 11.15592754026173949, -3.649275849833183649 ) ) ;
#110573 = CARTESIAN_POINT ( 'NONE',  ( 5.275877007301786215, 7.772378248882220397, 1.293907329011657614 ) ) ;
#110574 = CIRCLE ( 'NONE', #79276, 1.250000000000000888 ) ;
#110575 = CARTESIAN_POINT ( 'NONE',  ( -4.462041952228944730, 7.259447140025469203, -1.082531754730549967 ) ) ;
#110576 = CARTESIAN_POINT ( 'NONE',  ( -3.059603515650958450, 6.244770895048625370, 0.7153734454320024305 ) ) ;
#110577 = CARTESIAN_POINT ( 'NONE',  ( 0.5492016079408028606, 0.5613503750152969429, -1.678537049539428727 ) ) ;
#110578 = CARTESIAN_POINT ( 'NONE',  ( 5.725249205227378013, 1.776381904961796154, 0.9470739834369249488 ) ) ;
#110579 = CARTESIAN_POINT ( 'NONE',  ( 6.993308306550549247, 7.053281200597435685, 1.040834085586084257E-14 ) ) ;
#110580 = CARTESIAN_POINT ( 'NONE',  ( 3.944438254296574797, 2.095630017474863660, 0.2083849179023259668 ) ) ;
#110581 = CARTESIAN_POINT ( 'NONE',  ( 1.933070621186453897, -1.539717990624125621, -1.139454883405303098 ) ) ;
#110582 = FACE_OUTER_BOUND ( 'NONE', #170941, .T. ) ;
#110583 = CARTESIAN_POINT ( 'NONE',  ( 2.963290904843593587, 1.662405373943407261, 1.055889934586044188 ) ) ;
#110584 = CARTESIAN_POINT ( 'NONE',  ( 5.291273337336410698, -0.05367003302336400411, -2.019259759236047280 ) ) ;
#110585 = CARTESIAN_POINT ( 'NONE',  ( 2.184254540302111636, -1.834043650784190405, -0.3674020703766100460 ) ) ;
#110588 = ORIENTED_EDGE ( 'NONE', *, *, #32218, .F. ) ;
#110587 = CARTESIAN_POINT ( 'NONE',  ( 1.634869402278725348, 1.785593253932623803, 0.6852637533772619749 ) ) ;
#110586 = CARTESIAN_POINT ( 'NONE',  ( 4.582452686631489414, -1.674003568303910949, -0.4152789331205719026 ) ) ;
#110590 = CARTESIAN_POINT ( 'NONE',  ( 5.517805331081858888, 5.539787095791365523, 1.040834085586084257E-14 ) ) ;
#110589 = CARTESIAN_POINT ( 'NONE',  ( 1.471597369358583318, 0.1596246592955492538, -2.201166978212334424 ) ) ;
#110591 = CARTESIAN_POINT ( 'NONE',  ( 1.364683531249988535, 1.926041667008086211, 0.7879004041258500513 ) ) ;
#110593 = AXIS2_PLACEMENT_3D ( 'NONE', #139314, #176075, #91642 ) ;
#110592 = CARTESIAN_POINT ( 'NONE',  ( 6.913768267964901071, 10.15348118167935709, -1.199719254218441611 ) ) ;
#110594 = CARTESIAN_POINT ( 'NONE',  ( 11.52469724861194145, 12.22000006648768711, -3.346365485506883175 ) ) ;
#110595 = SURFACE_STYLE_FILL_AREA ( #95372 ) ;
#110596 = CARTESIAN_POINT ( 'NONE',  ( 3.019342412789784547, 6.452475500722323787, 0.1501914610189964416 ) ) ;
#110597 = CYLINDRICAL_SURFACE ( 'NONE', #78664, 0.04999999999999991257 ) ;
#110598 =( BOUNDED_SURFACE ( )  B_SPLINE_SURFACE ( 3, 2, ( 
 ( #152156, #83939, #167340 ),
 ( #164148, #185695, #49334 ),
 ( #33072, #147902, #101257 ),
 ( #34128, #118646, #35180 ) ),
 .UNSPECIFIED., .F., .F., .T. ) 
 B_SPLINE_SURFACE_WITH_KNOTS ( ( 4, 4 ),
 ( 3, 3 ),
 ( 1.570796326794896114, 2.200856270471036158 ),
 ( 0.000000000000000000, 1.000000000000000000 ),
 .UNSPECIFIED. ) 
 GEOMETRIC_REPRESENTATION_ITEM ( )  RATIONAL_B_SPLINE_SURFACE ( (
 ( 1.000000000000000000, 0.7071067811865475727, 1.000000000000000000),
 ( 1.000000000000000000, 0.7517196685950601198, 1.000000000000000000),
 ( 1.000000000000000000, 0.7917671131335182189, 1.000000000000000000),
 ( 1.000000000000000000, 0.8226529996948372947, 1.000000000000000000) ) ) 
 REPRESENTATION_ITEM ( '' )  SURFACE ( )  );
#110599 = VERTEX_POINT ( 'NONE', #68372 ) ;
#110600 = CARTESIAN_POINT ( 'NONE',  ( 1.943885480841448965, 1.426152643941134501, 1.501071833787496645 ) ) ;
#110601 = CARTESIAN_POINT ( 'NONE',  ( -1.500000000000011324, 3.420833333333355597, 0.8660254037844403729 ) ) ;
#110602 = CARTESIAN_POINT ( 'NONE',  ( 5.717788096661236885, 7.693838750903348789, 1.599625672291267398 ) ) ;
#110603 = CARTESIAN_POINT ( 'NONE',  ( -5.554036483092550824, 9.631459663583308739, -0.7998128361456231517 ) ) ;
#110604 = CARTESIAN_POINT ( 'NONE',  ( 3.366167277942881064, 7.149221934233827014, -0.7998128361456362523 ) ) ;
#110606 = EDGE_CURVE ( 'NONE', #66261, #115079, #4405, .T. ) ;
#110605 = CARTESIAN_POINT ( 'NONE',  ( -0.02277885239688070759, -1.805142470748948513, -0.9059449988992168690 ) ) ;
#110607 = DIRECTION ( 'NONE',  ( -0.04529798058948708572, 0.000000000000000000, -0.9989735196462988798 ) ) ;
#110608 = CARTESIAN_POINT ( 'NONE',  ( 1.364683531249990311, 2.634375000341422801, 1.214306433183764966E-14 ) ) ;
#110609 = EDGE_CURVE ( 'NONE', #50012, #94238, #28020, .T. ) ;
#110610 = CARTESIAN_POINT ( 'NONE',  ( 4.142179624174931796, 4.791296635414242111, 1.199719254218464037 ) ) ;
#110611 = CARTESIAN_POINT ( 'NONE',  ( 4.868517441940229951, -0.5404072756688070855, 1.942244311778835497 ) ) ;
#110612 = CARTESIAN_POINT ( 'NONE',  ( 5.278507882932355955, -0.4720989235634742154, -1.856488224439522439 ) ) ;
#110613 = DIRECTION ( 'NONE',  ( 0.000000000000000000, -1.000000000000000000, 0.000000000000000000 ) ) ;
#110614 = CARTESIAN_POINT ( 'NONE',  ( 2.894263506066748093, -0.6386881658498286818, -2.096408367471907841 ) ) ;
#110615 = CARTESIAN_POINT ( 'NONE',  ( 0.2335667940002684184, 0.001055507091213009818, -2.153566573614831281 ) ) ;
#110616 = CARTESIAN_POINT ( 'NONE',  ( -1.500000000000013101, 1.202083334016148974, 0.8660254037844403729 ) ) ;
#110617 = CARTESIAN_POINT ( 'NONE',  ( 5.554944837187737683, 0.3969321943368699368, 1.973527061375530023 ) ) ;
#110618 = CARTESIAN_POINT ( 'NONE',  ( -7.718669524881690336, 7.899535955317097624, 0.7998128361456462443 ) ) ;
#110620 = CARTESIAN_POINT ( 'NONE',  ( 6.345324880664913181, 0.3618513607092630480, -2.085922816363374288 ) ) ;
#110619 = CARTESIAN_POINT ( 'NONE',  ( -2.792616454734997866, 6.201876930592042925, 0.7216878364870317197 ) ) ;
#110621 = CARTESIAN_POINT ( 'NONE',  ( 1.364683531249997417, 9.296875000341403350, 2.602085213965210642E-15 ) ) ;
#110623 = CARTESIAN_POINT ( 'NONE',  ( -7.119966945832006289, 8.335658187339330283, 1.199719254218452047 ) ) ;
#110622 = CARTESIAN_POINT ( 'NONE',  ( 3.140259756110568734, 0.5104685904834010968, 2.027328384984484533 ) ) ;
#110625 = ORIENTED_EDGE ( 'NONE', *, *, #54063, .F. ) ;
#110624 = CARTESIAN_POINT ( 'NONE',  ( 1.535739282219195978, 0.8544175402723229729, -1.498188246372294863 ) ) ;
#110626 = CARTESIAN_POINT ( 'NONE',  ( 6.170199167347634628, 2.114832956739281400, -0.1575216572810705096 ) ) ;
#110627 = CARTESIAN_POINT ( 'NONE',  ( 4.798696304233017074, 7.685897223992134819, -1.199719254218452047 ) ) ;
#110628 = DIRECTION ( 'NONE',  ( -1.207943261119674327E-30, -2.168404344971008079E-15, 1.000000000000000000 ) ) ;
#110629 = CARTESIAN_POINT ( 'NONE',  ( 7.712222144929244294, -6.293595771080967793, 7.712222144929218537 ) ) ;
#110630 = CARTESIAN_POINT ( 'NONE',  ( 6.709229400517491726, -7.621055083280683817, -6.726126798030838572 ) ) ;
#110631 = CARTESIAN_POINT ( 'NONE',  ( 5.282873410819217241, 9.315102745931094219, -0.7998128361456281477 ) ) ;
#110632 = LINE ( 'NONE', #176634, #158461 ) ;
#110633 = CARTESIAN_POINT ( 'NONE',  ( 1.769862606763368706, 1.806619053477545700, -0.1335387089566111574 ) ) ;
#110634 = CARTESIAN_POINT ( 'NONE',  ( -5.205440912643032547, 8.160432600470439723, 1.199719254218452047 ) ) ;
#110635 = ORIENTED_EDGE ( 'NONE', *, *, #162793, .F. ) ;
#110636 = CARTESIAN_POINT ( 'NONE',  ( 3.192055101013606233, 5.811482486902795230, -1.199719254218446718 ) ) ;
#110637 = VERTEX_POINT ( 'NONE', #136613 ) ;
#110638 = CARTESIAN_POINT ( 'NONE',  ( 5.571474780572990504, 5.464751763615448787, 0.7998128361456352531 ) ) ;
#110639 = CARTESIAN_POINT ( 'NONE',  ( 3.141053669680595739, 0.04696373034178760036, 1.811039086309898627 ) ) ;
#110640 = CARTESIAN_POINT ( 'NONE',  ( -1.499999999999963141, 7.750000000000000000, -10.99818166789402518 ) ) ;
#110641 = FILL_AREA_STYLE_COLOUR ( '', #90314 ) ;
#110642 = CARTESIAN_POINT ( 'NONE',  ( 4.034853869772982549, 7.546986718285443985, 0.4065704115671017749 ) ) ;
#110643 = AXIS2_PLACEMENT_3D ( 'NONE', #146823, #177165, #77521 ) ;
#110644 = CARTESIAN_POINT ( 'NONE',  ( 3.596024570820981037, 0.8385914878215626755, -1.661501840750801540 ) ) ;
#110645 = CARTESIAN_POINT ( 'NONE',  ( 1.651812010259229968, 0.9862763539280462455, 1.642055979085883299 ) ) ;
#110646 = CARTESIAN_POINT ( 'NONE',  ( 0.5338675855391886715, 0.9430634504648884864, -1.562995807167219642 ) ) ;
#110647 = DIRECTION ( 'NONE',  ( 1.000000000000000000, 0.000000000000000000, 0.000000000000000000 ) ) ;
#110648 = CARTESIAN_POINT ( 'NONE',  ( -0.4461809497497640775, 3.122791860410086606, 1.949595486268987043 ) ) ;
#110649 = CARTESIAN_POINT ( 'NONE',  ( 5.234661009243278151, 7.693064604033777343, 1.208367059251337361 ) ) ;
#110650 = DIRECTION ( 'NONE',  ( 1.993562223070362833E-14, -1.000000000000000000, 2.190074022720978955E-12 ) ) ;
#110651 = CARTESIAN_POINT ( 'NONE',  ( -4.311129659465605002, 4.131998812239033647, 0.7216878364870317197 ) ) ;
#110652 = CARTESIAN_POINT ( 'NONE',  ( 6.778713617152772208, 10.85232362007950258, -0.7216878364870267237 ) ) ;
#110653 = CARTESIAN_POINT ( 'NONE',  ( 5.489095164188675824, 0.1408790922432824055, 1.964433151921646470 ) ) ;
#110654 = CARTESIAN_POINT ( 'NONE',  ( -5.037017762676898158, 5.835274463666530131, -1.199719254218446718 ) ) ;
#110655 = FACE_OUTER_BOUND ( 'NONE', #46342, .T. ) ;
#110656 = CARTESIAN_POINT ( 'NONE',  ( 0.2872076490801517279, 1.550519377178682268, 1.402564467939530823 ) ) ;
#110657 = CARTESIAN_POINT ( 'NONE',  ( 7.365103760721646076, 9.615707025640515937, 1.599625672291281386 ) ) ;
#110658 = CARTESIAN_POINT ( 'NONE',  ( 5.051747076446268636, 0.6043308924107357871, -1.829198057362067198 ) ) ;
#110659 = CARTESIAN_POINT ( 'NONE',  ( -6.043183783389232566, 8.073467052085995022, 1.599625672291269396 ) ) ;
#110660 = CARTESIAN_POINT ( 'NONE',  ( 0.8678470384533981674, 0.8956018474440343713, 1.590720368640268001 ) ) ;
#110661 = CARTESIAN_POINT ( 'NONE',  ( 2.245003380770736801, 0.4850519687749441644, 2.152760086278446394 ) ) ;
#110662 = CARTESIAN_POINT ( 'NONE',  ( -6.170096473061220443, 6.976792551583999469, 0.9111270007488531109 ) ) ;
#110663 = LINE ( 'NONE', #179864, #22848 ) ;
#110664 = CARTESIAN_POINT ( 'NONE',  ( 0.4847283499135228713, 1.883623918205453718, 0.5753430019505183513 ) ) ;
#110665 = CARTESIAN_POINT ( 'NONE',  ( 2.331498104393217474, 0.9136196428927362279, -1.713718834741830177 ) ) ;
#110666 = ORIENTED_EDGE ( 'NONE', *, *, #98746, .F. ) ;
#110667 = CARTESIAN_POINT ( 'NONE',  ( 0.8079699768257715409, -1.730602710733687877, 1.034004433739174500 ) ) ;
#110669 = CARTESIAN_POINT ( 'NONE',  ( 5.823074758751579871, -1.681767765412798710, -0.7970822532109583802 ) ) ;
#110668 = CARTESIAN_POINT ( 'NONE',  ( -4.606738333593328072, 8.596554832492683929, 0.7998128361456281477 ) ) ;
#110670 = CARTESIAN_POINT ( 'NONE',  ( 3.739016502318667445, 7.584212696005614873, 0.7998128361456271485 ) ) ;
#110671 = CARTESIAN_POINT ( 'NONE',  ( -11.55950211276791251, 13.88000000000000078, -3.221476510067115662 ) ) ;
#110672 = CARTESIAN_POINT ( 'NONE',  ( 8.536830278099042602, 13.11138575775759563, -0.7998128361456352531 ) ) ;
#110673 = CARTESIAN_POINT ( 'NONE',  ( -3.879604511804807032, 7.677955697080923514, 0.7998128361456341429 ) ) ;
#110674 = CARTESIAN_POINT ( 'NONE',  ( -8.100070429521727178, 8.414780020722290033, 0.7998128361456341429 ) ) ;
#110675 = CARTESIAN_POINT ( 'NONE',  ( 1.804482060849887270, 1.621174160030929068, -1.474864209862189579 ) ) ;
#110676 = CARTESIAN_POINT ( 'NONE',  ( 4.541618270897912701, 4.400902192243413502, 1.214306433183764966E-14 ) ) ;
#110677 = CARTESIAN_POINT ( 'NONE',  ( 6.502017186205484300, 9.743381262951846367, -1.199719254218452047 ) ) ;
#110678 = CARTESIAN_POINT ( 'NONE',  ( 0.000000000000000000, 4.099999999999999645, 0.000000000000000000 ) ) ;
#110679 = CARTESIAN_POINT ( 'NONE',  ( 2.560947663861262491, -1.588335953301520220, -0.9000364273514869229 ) ) ;
#110680 = CARTESIAN_POINT ( 'NONE',  ( -2.676845263694313637, 5.210404343363602919, -1.199719254218446718 ) ) ;
#110681 = CARTESIAN_POINT ( 'NONE',  ( -3.846762897975357198, 5.510976019103107859, -1.599625672291256295 ) ) ;
#110682 =( BOUNDED_CURVE ( )  B_SPLINE_CURVE ( 2, ( #113829, #177700, #94335, #95405, #129028, #161457, #114878, #93270, #78052 ),
 .UNSPECIFIED., .F., .T. ) 
 B_SPLINE_CURVE_WITH_KNOTS ( ( 3, 2, 2, 2, 3 ),
 ( 0.5156250000000002220, 0.5208333333333333703, 0.5312500000000000000, 0.5416666666666666297, 0.5468749999999997780 ),
 .UNSPECIFIED. ) 
 CURVE ( )  GEOMETRIC_REPRESENTATION_ITEM ( )  RATIONAL_B_SPLINE_CURVE ( ( 0.9330127018922194093, 0.9330127018922221849, 1.000000000000000000, 0.8660254037844387076, 1.000000000000000000, 0.8660254037844387076, 1.000000000000000000, 0.9330127018922221849, 0.9330127018922194093 ) ) 
 REPRESENTATION_ITEM ( '' )  );
#110683 =( GEOMETRIC_REPRESENTATION_CONTEXT ( 3 ) GLOBAL_UNCERTAINTY_ASSIGNED_CONTEXT ( ( #57143 ) ) GLOBAL_UNIT_ASSIGNED_CONTEXT ( ( #178346, #11553, #162093 ) ) REPRESENTATION_CONTEXT ( 'NONE', 'WORKASPACE' ) );
#110684 = CARTESIAN_POINT ( 'NONE',  ( -5.577377183731011101, 7.510248947172004641, -1.348340355397449342 ) ) ;
#110685 = DIRECTION ( 'NONE',  ( 0.000000000000000000, 0.000000000000000000, 1.000000000000000000 ) ) ;
#110686 = CARTESIAN_POINT ( 'NONE',  ( 9.459838494033030898, 12.05956421450382088, 1.599625672291281386 ) ) ;
#110687 = CARTESIAN_POINT ( 'NONE',  ( 1.506341009219732907, -0.6927896466909737594, -1.797792356224122923 ) ) ;
#110688 = CARTESIAN_POINT ( 'NONE',  ( 5.119951393648711324, 1.940949770148656661, -0.2839766199017114690 ) ) ;
#110689 = CARTESIAN_POINT ( 'NONE',  ( -6.364663046611467756, 9.512858423433634414, 1.199719254218452047 ) ) ;
#110690 = CARTESIAN_POINT ( 'NONE',  ( 3.974511587100456822, 7.788680618259193444, 1.040834085586084257E-14 ) ) ;
#110691 = CARTESIAN_POINT ( 'NONE',  ( 4.845371438081495619, 0.6875289519675978900, -2.081009137124201658 ) ) ;
#110692 = CARTESIAN_POINT ( 'NONE',  ( -11.94105721237523099, 10.90000000000000036, 1.187919463087248273 ) ) ;
#110693 = CARTESIAN_POINT ( 'NONE',  ( 3.555589372526322123, 1.629040189086952362, 1.277421477176057474 ) ) ;
#110694 = CARTESIAN_POINT ( 'NONE',  ( 1.364683531249986537, 1.967708333674750731, -0.7879004041258239610 ) ) ;
#110695 = ORIENTED_EDGE ( 'NONE', *, *, #87971, .T. ) ;
#110696 = CARTESIAN_POINT ( 'NONE',  ( 3.709890859234076466, 2.183183022688690578, 0.7197655052363950423 ) ) ;
#110698 = ORIENTED_EDGE ( 'NONE', *, *, #51647, .F. ) ;
#110697 = CARTESIAN_POINT ( 'NONE',  ( 6.643132081016111634, 9.733775946952057723, 1.082531754730558626 ) ) ;
#110700 = CARTESIAN_POINT ( 'NONE',  ( 1.642778471875000035, -1.276041666188710400, -2.845375778867859751 ) ) ;
#110699 = CARTESIAN_POINT ( 'NONE',  ( 4.258669648468278446, 7.022179452304728287, 1.082531754730549078 ) ) ;
#110701 = CARTESIAN_POINT ( 'NONE',  ( 0.000000000000000000, -3.600000000000005862, 0.000000000000000000 ) ) ;
#110702 = CARTESIAN_POINT ( 'NONE',  ( -9.951069066757307624, 4.531349380723807663, -6.628891310175081486 ) ) ;
#110703 = CARTESIAN_POINT ( 'NONE',  ( 4.119036135373352003, -1.858019016064060169, 0.5647323716678387395 ) ) ;
#110704 = ORIENTED_EDGE ( 'NONE', *, *, #119125, .F. ) ;
#110705 = CARTESIAN_POINT ( 'NONE',  ( 7.578644679914694926, 11.78557652663510424, 0.7216878364870438212 ) ) ;
#110706 = VERTEX_POINT ( 'NONE', #17487 ) ;
#110707 = CARTESIAN_POINT ( 'NONE',  ( 4.992401499097729456, -1.057410677138232780, 1.593263788312593743 ) ) ;
#110708 = CARTESIAN_POINT ( 'NONE',  ( 6.457991230880992362, 1.719707694194565484, -0.1327171722449934921 ) ) ;
#110709 = CARTESIAN_POINT ( 'NONE',  ( 4.698454014923811428, 1.387101836239763131, -1.463925544105355803 ) ) ;
#110710 = CARTESIAN_POINT ( 'NONE',  ( 4.446711195602238043, 6.210915699667824974, -1.443375672974051449 ) ) ;
#110711 = CARTESIAN_POINT ( 'NONE',  ( 2.315298440750997777, 1.971968782506158924, 0.9909306302095726160 ) ) ;
#110713 = CARTESIAN_POINT ( 'NONE',  ( -11.94105721237522921, 12.57259609010266921, 1.187919463087244720 ) ) ;
#110712 = CARTESIAN_POINT ( 'NONE',  ( -8.631737353394710155, 13.22211067893587533, 1.040834085586084257E-14 ) ) ;
#110715 = CARTESIAN_POINT ( 'NONE',  ( 0.4437791967034719343, 1.764639887404760188, 0.1366099650685937694 ) ) ;
#110714 = CARTESIAN_POINT ( 'NONE',  ( 1.886780952650327636, 1.818441039422484806, -1.031378756152110610 ) ) ;
#110716 = CARTESIAN_POINT ( 'NONE',  ( 6.100232455412330168, -0.2440331339308223768, 2.001510902166554473 ) ) ;
#110718 = CARTESIAN_POINT ( 'NONE',  ( 3.521668038933927658, -1.364967583988693889, -1.841414078927001041 ) ) ;
#110717 = CARTESIAN_POINT ( 'NONE',  ( 4.037295881819344956, 7.932205305423046582, -0.7998128361456362523 ) ) ;
#110719 = CARTESIAN_POINT ( 'NONE',  ( 0.6029369919973374126, -1.732405018438128552, 0.1659646143751663805 ) ) ;
#110720 = COLOUR_RGB ( '', 0.66274510, 0.83137255, 0.94901961) ;
#110721 = CARTESIAN_POINT ( 'NONE',  ( 2.812858766682566181, -0.6196351552101020399, -2.028021595557969015 ) ) ;
#110722 = DIRECTION ( 'NONE',  ( 4.440892098500637009E-16, 0.8656921114426514574, 0.5005768354468314030 ) ) ;
#110723 = CARTESIAN_POINT ( 'NONE',  ( 1.317307599089176939, -1.370793471230176808, 1.061547382435957587 ) ) ;
#110724 = CARTESIAN_POINT ( 'NONE',  ( 1.360316468749971808, 1.026041667008142921, 0.7853790794158540534 ) ) ;
#110725 = CARTESIAN_POINT ( 'NONE',  ( -11.94980361058168938, 13.40000000000000036, -1.100000000000000311 ) ) ;
#110726 = CARTESIAN_POINT ( 'NONE',  ( 1.205810543264747681, -1.711434635494583967, -1.335908126413299923 ) ) ;
#110727 = CARTESIAN_POINT ( 'NONE',  ( 3.626185617424378282, 2.007256095728218614, 0.1928357053486499662 ) ) ;
#110728 = CARTESIAN_POINT ( 'NONE',  ( 5.281250000000004441, 0.7852924748302615443, 1.895863743163964665 ) ) ;
#110729 = CARTESIAN_POINT ( 'NONE',  ( -1.201851678989727383E-14, 1.993750000682816381, 1.732050807568877637 ) ) ;
#110730 = CARTESIAN_POINT ( 'NONE',  ( 6.358035567807713839, 1.921127907539350810, -0.1446545421508997620 ) ) ;
#110731 = CARTESIAN_POINT ( 'NONE',  ( 1.364683531250000303, 13.00520833367473550, -0.7879004041258355073 ) ) ;
#110732 = CARTESIAN_POINT ( 'NONE',  ( 3.182088186068011915, 2.166492470972399165, -0.4902054615175278629 ) ) ;
#110733 = ORIENTED_EDGE ( 'NONE', *, *, #73531, .F. ) ;
#110734 = DIRECTION ( 'NONE',  ( 0.000000000000000000, 1.000000000000000000, 0.000000000000000000 ) ) ;
#110735 = CARTESIAN_POINT ( 'NONE',  ( 0.7499999999999867883, -0.6833333333333135862, -1.299038105676652899 ) ) ;
#110736 = CARTESIAN_POINT ( 'NONE',  ( 6.916630921265960019, 11.22115317478565188, 0.7998128361456462443 ) ) ;
#110737 = FACE_OUTER_BOUND ( 'NONE', #73981, .T. ) ;
#110738 = CARTESIAN_POINT ( 'NONE',  ( 5.759256982813394821, 1.713166593665109705, -0.3060214249656545982 ) ) ;
#110739 = CARTESIAN_POINT ( 'NONE',  ( 4.141029529442549872, -0.1900441490861082827, -1.952618137025011746 ) ) ;
#110741 = CARTESIAN_POINT ( 'NONE',  ( -6.561783159334141580, 7.718130443053708767, -1.082531754730544860 ) ) ;
#110740 = CARTESIAN_POINT ( 'NONE',  ( 3.846762897975340767, 5.510976019103107859, -1.599625672291256295 ) ) ;
#110743 = EDGE_CURVE ( 'NONE', #74942, #159480, #100890, .T. ) ;
#110742 = CONICAL_SURFACE ( 'NONE', #162486, 10.92874649719719571, 0.04746665426984499059 ) ;
#110744 = CARTESIAN_POINT ( 'NONE',  ( -1.412279214364694724, 4.224281623699000399, 0.5092244867763746630 ) ) ;
#110745 = CARTESIAN_POINT ( 'NONE',  ( 6.274757189715042927, -2.145364790639526564, -0.7184590933012062752 ) ) ;
#110746 = CARTESIAN_POINT ( 'NONE',  ( 1.996602216506689453, 2.039906831610329263, 0.3049752315822819027 ) ) ;
#110747 = CARTESIAN_POINT ( 'NONE',  ( -7.100719765255177229, 9.307259030929609267, -1.599625672291263179 ) ) ;
#110748 = ORIENTED_EDGE ( 'NONE', *, *, #2128, .F. ) ;
#110749 = CARTESIAN_POINT ( 'NONE',  ( 0.7499999999999902300, 1.514583334016148086, 1.299038105676657340 ) ) ;
#110750 = CARTESIAN_POINT ( 'NONE',  ( 3.866346082213562685, -1.258301477641217803, 1.384200088751494251 ) ) ;
#110751 = CARTESIAN_POINT ( 'NONE',  ( 2.109626794357027268, 0.001117226762978317921, 1.734343004219033757 ) ) ;
#110752 = CARTESIAN_POINT ( 'NONE',  ( 6.374583145400191775, -0.1054333438532777389, -2.189162923280890904 ) ) ;
#110753 = CARTESIAN_POINT ( 'NONE',  ( 1.307976841356368602, -0.5351398426680589182, 2.140771676462468687 ) ) ;
#110754 = CARTESIAN_POINT ( 'NONE',  ( 4.276362541559985075, -1.246951984143488623, 1.765614359104182629 ) ) ;
#110755 = CARTESIAN_POINT ( 'NONE',  ( 5.121012332258009891, -1.843477085030984286, 0.6107378676363499626 ) ) ;
#110756 = CARTESIAN_POINT ( 'NONE',  ( 6.678970768140332304, -0.09217866350584583146, -1.868372134486769420 ) ) ;
#110757 = CARTESIAN_POINT ( 'NONE',  ( 0.01034996896555614825, -0.2601230917365888740, -1.999999999999999556 ) ) ;
#110758 = CARTESIAN_POINT ( 'NONE',  ( -0.4170821662629227156, 3.033599471985643170, 0.4170821662629036752 ) ) ;
#110759 = CARTESIAN_POINT ( 'NONE',  ( 6.825078400183575589, -0.005632053428735600553, 2.144262460745151255 ) ) ;
#110760 = CARTESIAN_POINT ( 'NONE',  ( 5.801407773674092105, 1.352156682446105984, -1.496049708713815374 ) ) ;
#110761 = CARTESIAN_POINT ( 'NONE',  ( -8.503988664269602538, 10.94440607977979063, 1.599625672291269396 ) ) ;
#110762 = CARTESIAN_POINT ( 'NONE',  ( 6.123478934866503742, 10.29580919065294431, 0.7998128361456462443 ) ) ;
#110763 = DIRECTION ( 'NONE',  ( -7.387867266669436732E-31, -1.000000000000000000, 8.546850786086437571E-32 ) ) ;
#110764 = CARTESIAN_POINT ( 'NONE',  ( 3.211362085483655981, -0.3553965070040401852, 1.790585553824732390 ) ) ;
#110765 = CARTESIAN_POINT ( 'NONE',  ( 2.274722540679521288, -1.357913018379176995, 1.739418515187239223 ) ) ;
#110766 = ORIENTED_EDGE ( 'NONE', *, *, #196345, .F. ) ;
#110767 = CARTESIAN_POINT ( 'NONE',  ( -3.946832114909637479, 7.618738210787614484, 0.7216878364870338292 ) ) ;
#110768 = CARTESIAN_POINT ( 'NONE',  ( 3.285556943750000514, -1.451041666188708890, 1.896917185911906500 ) ) ;
#110769 = CARTESIAN_POINT ( 'NONE',  ( -8.532158741701643123, 8.848606708273724308, 0.7998128361456462443 ) ) ;
#110770 = CARTESIAN_POINT ( 'NONE',  ( 1.160422406460089428, 2.017671146822976880, 0.09473317391113857122 ) ) ;
#110771 = CARTESIAN_POINT ( 'NONE',  ( 0.9441710812277158693, -1.348169866081018853, -1.636719737310005973 ) ) ;
#110772 = EDGE_CURVE ( 'NONE', #10371, #7674, #146255, .T. ) ;
#110773 = CARTESIAN_POINT ( 'NONE',  ( -1.000000000000017097, 8.600000000000013856, -0.3999999999999858113 ) ) ;
#110774 = CARTESIAN_POINT ( 'NONE',  ( -4.261005416444848315, 8.193199762486115034, 0.7998128361456352531 ) ) ;
#110775 = CARTESIAN_POINT ( 'NONE',  ( 2.289708051090312058, -1.211253549455925338, -1.412920978024762908 ) ) ;
#110776 = CARTESIAN_POINT ( 'NONE',  ( 3.842846474469570062, 6.570739089268092137, -1.199719254218452047 ) ) ;
#110777 = CARTESIAN_POINT ( 'NONE',  ( 0.3038912542124502236, -0.5749842496362895794, 2.083749421223294540 ) ) ;
#110778 = CARTESIAN_POINT ( 'NONE',  ( 5.766250055133458119, 1.862018000461727052, -0.7743128548072516493 ) ) ;
#110779 = ORIENTED_EDGE ( 'NONE', *, *, #129965, .F. ) ;
#110780 = CARTESIAN_POINT ( 'NONE',  ( -9.917953063596627317, 11.52969898140628047, -1.199719254218441611 ) ) ;
#110781 = CARTESIAN_POINT ( 'NONE',  ( 3.967279163243800255, 0.2216459979678051528, -1.812115712870238537 ) ) ;
#110784 = ORIENTED_EDGE ( 'NONE', *, *, #179909, .F. ) ;
#110783 = CARTESIAN_POINT ( 'NONE',  ( -5.249217764984337009, 6.599847349967512322, -1.403262209131036053 ) ) ;
#110782 = CARTESIAN_POINT ( 'NONE',  ( -4.118644803501354978, 8.027112380718707030, 0.7998128361456352531 ) ) ;
#110785 = CARTESIAN_POINT ( 'NONE',  ( 5.355371708033295874, 7.701368364266228284, 1.317571137710125351 ) ) ;
#110786 = CARTESIAN_POINT ( 'NONE',  ( 5.993517489292202960, 1.942244631591660164, 0.5404061186519912852 ) ) ;
#110787 = CARTESIAN_POINT ( 'NONE',  ( 6.263598714517844890, 0.9507720431706818687, 1.576509192756641697 ) ) ;
#110788 = CARTESIAN_POINT ( 'NONE',  ( 2.987092767191504183, 6.445738828830674727, 0.3863172271417950054 ) ) ;
#110789 = CARTESIAN_POINT ( 'NONE',  ( 4.213705752388523962, -0.3967513169967327724, 2.273188601971836142 ) ) ;
#110790 = CARTESIAN_POINT ( 'NONE',  ( 6.150558962454855561, 7.204682206732687000, 1.199719254218452047 ) ) ;
#110791 = CARTESIAN_POINT ( 'NONE',  ( 5.413408226029434722, -0.3230527293765028674, 2.137217106551466905 ) ) ;
#110792 = CARTESIAN_POINT ( 'NONE',  ( 7.332262146892202459, 7.448727347662698506, -0.7998128361456281477 ) ) ;
#110793 = CARTESIAN_POINT ( 'NONE',  ( 2.542442122522000414, -1.613304532933591995, 1.080848972723145618 ) ) ;
#110794 = CARTESIAN_POINT ( 'NONE',  ( 4.728017916497640805, -2.050086588643835750, -1.039272215941482225 ) ) ;
#110795 = CARTESIAN_POINT ( 'NONE',  ( -6.749980374757255319, 8.968339418673846097, 1.599625672291269396 ) ) ;
#110796 = CARTESIAN_POINT ( 'NONE',  ( 4.610133579271312954, -0.8000244862099057386, -1.691074300901610261 ) ) ;
#110797 = VERTEX_POINT ( 'NONE', #184264 ) ;
#110800 = CARTESIAN_POINT ( 'NONE',  ( -3.772911886352873445, 7.623757310712140800, 0.7998128361456352531 ) ) ;
#110799 = CARTESIAN_POINT ( 'NONE',  ( -1.402160292154681736E-14, -0.1312499993171854229, -1.732050807568870754 ) ) ;
#110798 = CARTESIAN_POINT ( 'NONE',  ( 2.021601768330282045, -0.4154675118966509317, 1.866563793090275203 ) ) ;
#110801 = CARTESIAN_POINT ( 'NONE',  ( 3.914836437932368796, 1.561248537261412883, -1.560010120355350471 ) ) ;
#110802 = CARTESIAN_POINT ( 'NONE',  ( -1.608462485352074145, 8.735270501766109419, -2.463594439587580176 ) ) ;
#110803 = CARTESIAN_POINT ( 'NONE',  ( 5.356880090730863131, 7.343055753976412525, 1.443375672974064550 ) ) ;
#110804 = CARTESIAN_POINT ( 'NONE',  ( -5.600926855776882540, 8.588146194164741232, -1.082531754730549967 ) ) ;
#110805 = CARTESIAN_POINT ( 'NONE',  ( 1.458210469330342374, 0.7952313087857125762, 1.804010633499957272 ) ) ;
#110806 = CARTESIAN_POINT ( 'NONE',  ( 1.765117381242779615, -1.630797578202509701, 1.632866094832433834 ) ) ;
#110808 = ADVANCED_FACE ( 'NONE', ( #3370 ), #185161, .T. ) ;
#110807 = CARTESIAN_POINT ( 'NONE',  ( 2.787496613063783713, -1.831585881375777713, 0.7034878451678548972 ) ) ;
#110809 = CARTESIAN_POINT ( 'NONE',  ( -5.906512197408906317, 6.919960980845699439, -1.199719254218453823 ) ) ;
#110810 = CARTESIAN_POINT ( 'NONE',  ( 5.928601196466630086, -1.312702821215183002, 1.590880328853358394 ) ) ;
#110811 = CARTESIAN_POINT ( 'NONE',  ( 4.094199201646931741, 4.839282492418613302, -1.082531754730543083 ) ) ;
#110812 = CARTESIAN_POINT ( 'NONE',  ( 6.039231080244466199, 6.010467446565510130, 0.7998128361456352531 ) ) ;
#110813 = ORIENTED_EDGE ( 'NONE', *, *, #16190, .T. ) ;
#110814 = CARTESIAN_POINT ( 'NONE',  ( -10.63367255181986160, 11.30037282007833532, 1.040834085586084257E-14 ) ) ;
#110815 = CARTESIAN_POINT ( 'NONE',  ( 6.484567079770447329, -6.583980363594976737, 7.100579091573052004 ) ) ;
#110816 = CARTESIAN_POINT ( 'NONE',  ( 8.550388431712704573, 13.12720360364021133, 0.000000000000000000 ) ) ;
#110817 = CARTESIAN_POINT ( 'NONE',  ( 1.973704989461112946, -0.2689809023317759618, 2.154309762211854107 ) ) ;
#110818 = CARTESIAN_POINT ( 'NONE',  ( -0.4019237886466933696, 12.30133545031537423, 1.500000000000005995 ) ) ;
#110819 = CARTESIAN_POINT ( 'NONE',  ( 6.650326532587140349, -8.038658175288279750, 6.784185045882107801 ) ) ;
#110820 = CARTESIAN_POINT ( 'NONE',  ( -9.976233718008073126, 4.600059191775173417, -6.670817322401115135 ) ) ;
#110821 = CARTESIAN_POINT ( 'NONE',  ( 2.811613793402362393, -1.850737340378521223, 0.2705540153197931730 ) ) ;
#110822 = CARTESIAN_POINT ( 'NONE',  ( 0.2103215893997134323, -0.8792329509940269849, -1.862182962916396844 ) ) ;
#110823 = CARTESIAN_POINT ( 'NONE',  ( 6.727182134110222478, 3.706444386917655986, 2.325533714637216143 ) ) ;
#110824 = CARTESIAN_POINT ( 'NONE',  ( -1.364683531249997417, 5.821875000341418804, 1.214306433183764966E-14 ) ) ;
#110825 =( NAMED_UNIT ( * ) PLANE_ANGLE_UNIT ( ) SI_UNIT ( $, .RADIAN. ) );
#110826 = EDGE_CURVE ( 'NONE', #146356, #42660, #52348, .T. ) ;
#110827 = CARTESIAN_POINT ( 'NONE',  ( 1.717294761138322690, 1.590556852780611097, 1.061263400373997134 ) ) ;
#110828 = B_SPLINE_CURVE_WITH_KNOTS ( 'NONE', 3,
 ( #118016, #104921, #85445, #201303, #134234, #151530, #52943, #204505, #119080, #185061 ),
 .UNSPECIFIED., .F., .F.,
 ( 4, 2, 2, 2, 4 ),
 ( 0.000000000000000000, 0.0002021113321160290582, 0.0004042226642320581164, 0.0006063339963480871746, 0.0008084453284641167749 ),
 .UNSPECIFIED. ) ;
#110829 =( GEOMETRIC_REPRESENTATION_CONTEXT ( 3 ) GLOBAL_UNCERTAINTY_ASSIGNED_CONTEXT ( ( #23023 ) ) GLOBAL_UNIT_ASSIGNED_CONTEXT ( ( #88293, #153280, #42769 ) ) REPRESENTATION_CONTEXT ( 'NONE', 'WORKASPACE' ) );
#110830 = CARTESIAN_POINT ( 'NONE',  ( 4.451851733873055217, 1.769451340447548038, -0.04442182319205205399 ) ) ;
#110831 = CARTESIAN_POINT ( 'NONE',  ( 2.332540574144434053, 1.247770424613745543, -1.449200414897835687 ) ) ;
#110832 = CARTESIAN_POINT ( 'NONE',  ( -4.055860508782465068, 7.883587693554856557, 1.040834085586084257E-14 ) ) ;
#110834 = CARTESIAN_POINT ( 'NONE',  ( 6.609000000000045283, 0.005669918681758949128, 1.900160851458796651 ) ) ;
#110833 = DIRECTION ( 'NONE',  ( -1.000000000000000000, 1.250471828332832423E-35, 1.561251128379126077E-17 ) ) ;
#110835 = CARTESIAN_POINT ( 'NONE',  ( 1.499999999999987121, -0.7458333333333122539, 0.8660254037844524744 ) ) ;
#110836 = CARTESIAN_POINT ( 'NONE',  ( 0.9771079587245214970, 1.912259438035465386, 0.7939916666956441382 ) ) ;
#110837 = CARTESIAN_POINT ( 'NONE',  ( 0.7499999999999902300, 5.816666666666685082, -1.299038105676658228 ) ) ;
#110838 = CARTESIAN_POINT ( 'NONE',  ( 4.961713530105988923, 1.850188064717460223, -0.2750520410098392654 ) ) ;
#110839 = CARTESIAN_POINT ( 'NONE',  ( 2.015964598666186269, -0.8597642540715648707, -1.610575774528985704 ) ) ;
#110841 = CARTESIAN_POINT ( 'NONE',  ( 4.631618433768171172, 8.327536854573105884, -0.3785340233409782984 ) ) ;
#110840 = CARTESIAN_POINT ( 'NONE',  ( 4.371826309796801979, 2.140994599346605742, -0.5347268394074317088 ) ) ;
#110842 = CARTESIAN_POINT ( 'NONE',  ( 1.364683531249988535, 5.467708333674750953, -0.7879004041258300672 ) ) ;
#110843 = CARTESIAN_POINT ( 'NONE',  ( 2.488800817111187946, 2.000174138640842258, 0.5034198422354563274 ) ) ;
#110844 = CARTESIAN_POINT ( 'NONE',  ( -7.153898609505128015, 11.49796547773133604, 0.7998128361456481317 ) ) ;
#110845 = FACE_OUTER_BOUND ( 'NONE', #162283, .T. ) ;
#110846 = CARTESIAN_POINT ( 'NONE',  ( 9.215791728987056786, 11.77484298861683598, -1.599625672291262513 ) ) ;
#110847 = CARTESIAN_POINT ( 'NONE',  ( 1.367350270964193593, 3.416621234749356528, -0.2578043790911870858 ) ) ;
#110848 = CARTESIAN_POINT ( 'NONE',  ( 5.397027666691686321, 8.454226823519094935, 1.199719254218451159 ) ) ;
#110849 = ORIENTED_EDGE ( 'NONE', *, *, #185104, .T. ) ;
#110850 = CARTESIAN_POINT ( 'NONE',  ( 5.934052368846653991, 1.230181698326970885, 1.665117723180092213 ) ) ;
#110851 = CARTESIAN_POINT ( 'NONE',  ( -1.402160292154681736E-14, 0.5093750003414236893, -1.575800808251659024 ) ) ;
#110852 = CARTESIAN_POINT ( 'NONE',  ( 2.829541668879275829, -2.018026287816252040, 0.7751260729957699658 ) ) ;
#110853 = CARTESIAN_POINT ( 'NONE',  ( -4.629329830860687167, 8.351765225447314478, -0.3187335059142253346 ) ) ;
#110855 = EDGE_CURVE ( 'NONE', #55540, #23435, #111663, .T. ) ;
#110854 = CARTESIAN_POINT ( 'NONE',  ( 3.387372106552827944, 0.04729818973902254198, -2.019286085025721267 ) ) ;
#110856 = CARTESIAN_POINT ( 'NONE',  ( -2.460826785407703721, 8.202405370174460586, 2.499999999999999112 ) ) ;
#110857 = EDGE_LOOP ( 'NONE', ( #106454, #198691, #179313, #7811 ) ) ;
#110858 = EDGE_CURVE ( 'NONE', #96195, #94484, #54288, .T. ) ;
#110861 = CARTESIAN_POINT ( 'NONE',  ( 7.673551755654734130, 9.015193805427763607, -1.082531754730537976 ) ) ;
#110860 = CARTESIAN_POINT ( 'NONE',  ( 3.475000000000000533, -1.954166666666666163, 2.006292185433948827 ) ) ;
#110859 = CARTESIAN_POINT ( 'NONE',  ( 9.899039292889495911, 2.972657967447090321, 6.161878781005994732 ) ) ;
#110862 = CARTESIAN_POINT ( 'NONE',  ( -3.973948422136970748, 6.690004688251493192, -1.082531754730546636 ) ) ;
#110863 = CARTESIAN_POINT ( 'NONE',  ( 0.8136858238772455287, -1.282993010278702606, -1.555696519147983459 ) ) ;
#110865 = CARTESIAN_POINT ( 'NONE',  ( 5.899973326018036701, -0.7874313895239596350, -2.045375389432432467 ) ) ;
#110864 = CARTESIAN_POINT ( 'NONE',  ( -3.581325132304157943, 7.329963087663487364, -0.7998128361456281477 ) ) ;
#110866 =( BOUNDED_CURVE ( )  B_SPLINE_CURVE ( 3, ( #9706, #191639, #73645, #172227 ),
 .UNSPECIFIED., .F., .T. ) 
 B_SPLINE_CURVE_WITH_KNOTS ( ( 4, 4 ),
 ( 4.712388980384771386, 5.718907872238673029 ),
 .UNSPECIFIED. ) 
 CURVE ( )  GEOMETRIC_REPRESENTATION_ITEM ( )  RATIONAL_B_SPLINE_CURVE ( ( 1.000000000000000000, 0.9173434942194497177, 0.9173434942194497177, 1.000000000000000000 ) ) 
 REPRESENTATION_ITEM ( '' )  );
#110867 = CARTESIAN_POINT ( 'NONE',  ( 1.499999999999989120, 4.535416667349484676, 0.8660254037844524744 ) ) ;
#110868 = CARTESIAN_POINT ( 'NONE',  ( 5.080287894202283994, 0.9478536798121822704, 1.660923459347658282 ) ) ;
#110869 = CARTESIAN_POINT ( 'NONE',  ( -4.277761160311629673, 4.949475094240346706, 1.199719254218462483 ) ) ;
#110870 = CARTESIAN_POINT ( 'NONE',  ( 6.954969613686092345, 7.216478758829655504, -0.7216878364870257245 ) ) ;
#110872 = CARTESIAN_POINT ( 'NONE',  ( 3.216422893352603563, 1.967893637826668263, 0.4390085219014849827 ) ) ;
#110871 = CARTESIAN_POINT ( 'NONE',  ( -9.476786185827959841, 10.15859809299519334, 0.7216878364870438212 ) ) ;
#110873 = CARTESIAN_POINT ( 'NONE',  ( -1.364683531250000748, 13.67187500034139980, 0.000000000000000000 ) ) ;
#110874 = CARTESIAN_POINT ( 'NONE',  ( -3.332271893908731464, 7.109677319527304640, -0.7998128361456481317 ) ) ;
#110875 = CARTESIAN_POINT ( 'NONE',  ( 5.455954713372185516, 1.722626330383254745, -0.08824682005538657392 ) ) ;
#110876 = CARTESIAN_POINT ( 'NONE',  ( 7.523848900940885542, 7.742521570711348389, 0.7998128361456291469 ) ) ;
#110877 = CARTESIAN_POINT ( 'NONE',  ( 3.816783937446950770, 4.411668334231586996, 1.199719254218464037 ) ) ;
#110878 = CARTESIAN_POINT ( 'NONE',  ( -6.773376348128482327, -7.215568602681039501, -6.661184042391679050 ) ) ;
#110879 = DIRECTION ( 'NONE',  ( 0.7592566023653005702, -0.6507913734559639396, 0.000000000000000000 ) ) ;
#110880 = CARTESIAN_POINT ( 'NONE',  ( 1.551716534671506498, 1.565040117424065347, 1.355267069636761912 ) ) ;
#110881 = DIRECTION ( 'NONE',  ( 0.000000000000000000, -1.000000000000000000, 0.000000000000000000 ) ) ;
#110882 = ORIENTED_EDGE ( 'NONE', *, *, #117706, .F. ) ;
#110883 = CARTESIAN_POINT ( 'NONE',  ( 5.777939495331589015, 1.783485896618082878, -0.3162516061415173718 ) ) ;
#110884 = CARTESIAN_POINT ( 'NONE',  ( 4.960304097753311936, 6.880383762169266504, 1.599625672291268286 ) ) ;
#110885 = CARTESIAN_POINT ( 'NONE',  ( -4.151088913318013773, 2.978104609995165131, -0.7749999999999935829 ) ) ;
#110886 = CARTESIAN_POINT ( 'NONE',  ( 0.4745106373920011666, -1.311730567922615665, 1.249698552857400946 ) ) ;
#110887 = CARTESIAN_POINT ( 'NONE',  ( 4.814553946184248368, 7.670711132973337065, -1.082531754730548412 ) ) ;
#110888 = CARTESIAN_POINT ( 'NONE',  ( 0.1216811705908975721, 2.536982183874236352, -1.996294991408742003 ) ) ;
#110889 = CARTESIAN_POINT ( 'NONE',  ( 2.888834398507355239, 1.879202789969806497, -1.127179367409691935 ) ) ;
#110890 = ORIENTED_EDGE ( 'NONE', *, *, #207656, .F. ) ;
#110892 = CARTESIAN_POINT ( 'NONE',  ( 9.426996880203592610, 9.892584536526015881, -0.7998128361456281477 ) ) ;
#110891 = CARTESIAN_POINT ( 'NONE',  ( 0.7132427667453158371, -1.655377960257615966, -1.052639099659122390 ) ) ;
#110893 = CARTESIAN_POINT ( 'NONE',  ( 4.569893716599374933, -0.8992288252529623271, 1.691407037985042772 ) ) ;
#110894 = CYLINDRICAL_SURFACE ( 'NONE', #3882, 1.250000000000000000 ) ;
#110895 = CARTESIAN_POINT ( 'NONE',  ( -5.941092982759174745, 7.138105816550336158, 1.109076209742832164 ) ) ;
#110896 = DIRECTION ( 'NONE',  ( 5.578564026256491869E-16, 1.000000000000000000, 9.066213480720160632E-32 ) ) ;
#110897 = CARTESIAN_POINT ( 'NONE',  ( -1.402160292154681736E-14, -0.4281249996585808071, 1.575800808251672791 ) ) ;
#110899 = ORIENTED_EDGE ( 'NONE', *, *, #72048, .F. ) ;
#110898 = CARTESIAN_POINT ( 'NONE',  ( 5.016153647376205171, 6.875265226737464985, 1.443375672974062551 ) ) ;
#110900 = CARTESIAN_POINT ( 'NONE',  ( -7.836249599018719536, 12.08611559892311504, 0.7216878364870478180 ) ) ;
#110901 = CARTESIAN_POINT ( 'NONE',  ( 1.991316529349271836, 1.880942973025516940, -1.065213018539921563 ) ) ;
#110902 = CARTESIAN_POINT ( 'NONE',  ( -5.469788628470539926, 5.346117919495872783, -0.7998128361456362523 ) ) ;
#110903 = CARTESIAN_POINT ( 'NONE',  ( 3.902768115887398803, 5.646591783325653147, -1.599625672291269396 ) ) ;
#110904 = CARTESIAN_POINT ( 'NONE',  ( 1.553431815599433108, 0.5335803070953272220, -1.745854899344486233 ) ) ;
#110905 = CARTESIAN_POINT ( 'NONE',  ( 0.01804983835817890528, -0.5593552815991027494, 2.045460531183339814 ) ) ;
#110906 = CARTESIAN_POINT ( 'NONE',  ( 4.805575371506604299, -0.4859443722219913830, 1.759630929660048526 ) ) ;
#110907 = CARTESIAN_POINT ( 'NONE',  ( 12.32702100841206239, 6.004295755469880369, 1.110179225836540162 ) ) ;
#110908 = CARTESIAN_POINT ( 'NONE',  ( 3.463059065379545221, -1.560675823418774533, 1.104941681961457256 ) ) ;
#110909 = ORIENTED_EDGE ( 'NONE', *, *, #24241, .T. ) ;
#110910 = CARTESIAN_POINT ( 'NONE',  ( 3.719166427026363131, -1.735901824557140927, -0.9304994270666072653 ) ) ;
#110911 = VERTEX_POINT ( 'NONE', #72651 ) ;
#110912 = CARTESIAN_POINT ( 'NONE',  ( 6.356980358691139088, 0.3275572002108660952, -1.914087848568704731 ) ) ;
#110913 = EDGE_LOOP ( 'NONE', ( #107405, #118444, #161415 ) ) ;
#110914 = CARTESIAN_POINT ( 'NONE',  ( -6.611536185319534908, 7.742488966741438716, 1.199719254218452047 ) ) ;
#110916 = CARTESIAN_POINT ( 'NONE',  ( 5.941668366282724101, -1.996146358238064522, 0.7160658055916299114 ) ) ;
#110915 = CARTESIAN_POINT ( 'NONE',  ( -5.418418667316934112, 6.350518529071726981, -1.199719254218453823 ) ) ;
#110917 = CARTESIAN_POINT ( 'NONE',  ( 5.492461626867537916, 9.421972641405202964, -0.7216878364870458196 ) ) ;
#110918 = CARTESIAN_POINT ( 'NONE',  ( 3.773993364719562926, 1.897484654492180400, -0.2369724479281897500 ) ) ;
#110919 = B_SPLINE_CURVE_WITH_KNOTS ( 'NONE', 3,
 ( #206949, #109539, #205883, #27132, #93239, #159271, #213329 ),
 .UNSPECIFIED., .F., .F.,
 ( 4, 3, 4 ),
 ( 3.314949680324100580E-05, 0.0009000000012044581665, 0.001958074173707502127 ),
 .UNSPECIFIED. ) ;
#110920 = CARTESIAN_POINT ( 'NONE',  ( 5.763841807162588537, 6.241519824923047466, -1.009562751112670576 ) ) ;
#110921 = DIRECTION ( 'NONE',  ( 0.000000000000000000, 0.000000000000000000, 1.000000000000000000 ) ) ;
#110922 = CARTESIAN_POINT ( 'NONE',  ( 4.523580528814945545, 5.306540700819438960, 1.199719254218452047 ) ) ;
#110923 = AXIS2_PLACEMENT_3D ( 'NONE', #115452, #131686, #143673 ) ;
#110924 = CARTESIAN_POINT ( 'NONE',  ( 5.268231569329090647, 2.010679013512342017, -0.1011730594673541789 ) ) ;
#110925 = CARTESIAN_POINT ( 'NONE',  ( 0.1505076982582145839, 7.030243935902785957, 1.995512553310466952 ) ) ;
#110926 = CARTESIAN_POINT ( 'NONE',  ( 6.076747101522134820, -1.735163100867884500, -0.5679748894881069265 ) ) ;
#110927 = CARTESIAN_POINT ( 'NONE',  ( 0.6782873735513492708, -1.106163567672680204, -1.749894625276714688 ) ) ;
#110928 = CARTESIAN_POINT ( 'NONE',  ( -8.351459436338048548, 8.845716885256940998, -0.7216878364870278340 ) ) ;
#110929 = CARTESIAN_POINT ( 'NONE',  ( -5.448385796200811981, 7.521903143423984694, -1.249286997217812223 ) ) ;
#110930 = DIRECTION ( 'NONE',  ( 3.330669073875478989E-16, -3.540251991789410786E-16, -1.000000000000000000 ) ) ;
#110931 = CARTESIAN_POINT ( 'NONE',  ( 6.438356904408193415, 1.850619875698428674, 0.2722718653145329015 ) ) ;
#110932 = CARTESIAN_POINT ( 'NONE',  ( 5.774883364416965037, 8.824782127540085952, -1.199719254218440723 ) ) ;
#110933 =( NAMED_UNIT ( * ) SI_UNIT ( $, .STERADIAN. ) SOLID_ANGLE_UNIT ( ) );
#110934 = AXIS2_PLACEMENT_3D ( 'NONE', #159621, #193179, #13360 ) ;
#110935 = DIRECTION ( 'NONE',  ( -0.6483454320283799088, 0.000000000000000000, 0.7613463080411786432 ) ) ;
#110936 = CARTESIAN_POINT ( 'NONE',  ( 0.6823417656249934904, 11.75520833367473017, 1.181850606188764807 ) ) ;
#110937 = CARTESIAN_POINT ( 'NONE',  ( -3.100010679019018500, 6.768429558830820980, 1.040834085586084257E-14 ) ) ;
#110939 = CARTESIAN_POINT ( 'NONE',  ( -6.770317605177755382, 8.992066187497757213, 1.599625672291269396 ) ) ;
#110938 = CARTESIAN_POINT ( 'NONE',  ( -11.86145016429273014, 10.90000000000000036, -1.100000000000000533 ) ) ;
#110940 = CARTESIAN_POINT ( 'NONE',  ( 3.568775204899740316, -0.8506723435033979319, 1.511049830170706931 ) ) ;
#110941 = CARTESIAN_POINT ( 'NONE',  ( -5.525111292768871252, 6.404716915440499037, -1.199719254218446718 ) ) ;
#110942 = CARTESIAN_POINT ( 'NONE',  ( 0.7607008448355723207, -0.6940761377024067258, -1.950597895851911456 ) ) ;
#110943 = CARTESIAN_POINT ( 'NONE',  ( 3.814152603263697650, 1.130891212129871093, -1.789721717560237790 ) ) ;
#110944 = CARTESIAN_POINT ( 'NONE',  ( 5.379888026524302980, 5.170957540566797128, -0.7998128361456211532 ) ) ;
#110945 = CARTESIAN_POINT ( 'NONE',  ( 6.414979237560321401, 10.63589287712906462, 1.040834085586084257E-14 ) ) ;
#110946 = CARTESIAN_POINT ( 'NONE',  ( 0.3548561630248124876, 6.502427107676207463, 3.303236143568316407 ) ) ;
#110947 = CARTESIAN_POINT ( 'NONE',  ( 0.5847281401991512029, 1.882922653073782815, 0.5772291209212175866 ) ) ;
#110948 = CARTESIAN_POINT ( 'NONE',  ( 4.149381719138396818, 7.633502232665817289, 0.8094099469760536181 ) ) ;
#110949 = CARTESIAN_POINT ( 'NONE',  ( 3.877268743828266029, 6.506935386899531437, 1.082531754730558626 ) ) ;
#110951 = CARTESIAN_POINT ( 'NONE',  ( 0.000000000000000000, -2.500000000000002220, 0.000000000000000000 ) ) ;
#110950 = CARTESIAN_POINT ( 'NONE',  ( 3.475000000000000533, -1.225000000000000311, 0.000000000000000000 ) ) ;
#110952 = CARTESIAN_POINT ( 'NONE',  ( 3.381108394495379699, 2.072348265612040219, -0.9799971971852624586 ) ) ;
#110953 = CARTESIAN_POINT ( 'NONE',  ( 1.172165686010542496, -1.159919637379997814, 1.409874495853599141 ) ) ;
#110954 = CARTESIAN_POINT ( 'NONE',  ( 3.357576282340120066, -1.451192137084562628, -1.245647637661301044 ) ) ;
#110955 = CARTESIAN_POINT ( 'NONE',  ( 5.529746549527311039, 7.544733289238903851, -1.599625672291281386 ) ) ;
#110956 = CARTESIAN_POINT ( 'NONE',  ( 6.195713011320782115, 8.251417818006149929, -1.443375672974057666 ) ) ;
#110957 = CARTESIAN_POINT ( 'NONE',  ( -7.862839020921525091, 11.26073039346208660, -1.199719254218446718 ) ) ;
#110958 = CARTESIAN_POINT ( 'NONE',  ( 1.599859548348059324, 1.391279381849828800, 1.455310581225319311 ) ) ;
#110959 = CARTESIAN_POINT ( 'NONE',  ( 1.973419848571813073, -0.2453196125269933581, 1.946320556625024345 ) ) ;
#110960 = CARTESIAN_POINT ( 'NONE',  ( -9.820183334999905256, 10.35130206712171130, 1.040834085586084257E-14 ) ) ;
#110961 = CARTESIAN_POINT ( 'NONE',  ( -7.365103760721662951, 9.615707025640515937, 1.599625672291295375 ) ) ;
#110963 = CARTESIAN_POINT ( 'NONE',  ( 3.977242411272710942, 1.666424048269627534, -0.5965368118019414023 ) ) ;
#110962 = CARTESIAN_POINT ( 'NONE',  ( 4.716787809154822320, -0.1028738300157816532, 2.088225860312553195 ) ) ;
#110964 = CARTESIAN_POINT ( 'NONE',  ( -1.724555757181258864, 13.99999999999692513, 11.68000002332616205 ) ) ;
#110966 = CARTESIAN_POINT ( 'NONE',  ( -0.02900071798685524560, -0.004641455105012376459, -2.173770343569726649 ) ) ;
#110965 = CYLINDRICAL_SURFACE ( 'NONE', #90174, 0.07999999999999998779 ) ;
#110967 = CARTESIAN_POINT ( 'NONE',  ( 3.925522983587381276, 0.9287783018587884021, -1.471562914255954757 ) ) ;
#110968 = EDGE_CURVE ( 'NONE', #71109, #73672, #97846, .T. ) ;
#110969 = CARTESIAN_POINT ( 'NONE',  ( 9.426996880203592610, 9.892584536526015881, -0.7998128361456281477 ) ) ;
#110970 = CARTESIAN_POINT ( 'NONE',  ( -4.067937748088393590, 7.725456827083305278, 0.6547958487484796253 ) ) ;
#110971 = CARTESIAN_POINT ( 'NONE',  ( 4.182719533963025427, -0.8905394866418876454, -1.487461311242815443 ) ) ;
#110972 =( GEOMETRIC_REPRESENTATION_CONTEXT ( 3 ) GLOBAL_UNCERTAINTY_ASSIGNED_CONTEXT ( ( #134864 ) ) GLOBAL_UNIT_ASSIGNED_CONTEXT ( ( #79255, #92343, #160506 ) ) REPRESENTATION_CONTEXT ( 'NONE', 'WORKASPACE' ) );
#110973 = CARTESIAN_POINT ( 'NONE',  ( 4.563029256048502624, 1.681186374793992355, -1.373936881898863982 ) ) ;
#110974 = CARTESIAN_POINT ( 'NONE',  ( 5.196852952739813070, 4.957416621151553571, -0.7998128361456221525 ) ) ;
#110975 = CARTESIAN_POINT ( 'NONE',  ( 6.333220217719927270, -1.622483202430196725, -1.197309987464048486 ) ) ;
#110976 = CARTESIAN_POINT ( 'NONE',  ( 5.125000000000002665, -2.052068128417943171, 3.046444613966958600E-13 ) ) ;
#110977 = DIRECTION ( 'NONE',  ( -0.9999980456341538426, 0.000000000000000000, -0.001977050295941262543 ) ) ;
#110978 = CARTESIAN_POINT ( 'NONE',  ( 3.223571483072392940, -1.856993652095505487, 0.5122080487700955143 ) ) ;
#110979 = CARTESIAN_POINT ( 'NONE',  ( -1.500000000000008216, 10.53125000068279249, 3.469446951953614189E-15 ) ) ;
#110980 = CARTESIAN_POINT ( 'NONE',  ( 0.3291711827644402399, 1.527175228150777331, -1.613279532339807476 ) ) ;
#110981 = ORIENTED_EDGE ( 'NONE', *, *, #212871, .T. ) ;
#110982 = CARTESIAN_POINT ( 'NONE',  ( -0.1411974294641968053, 0.7397609206469482057, -1.984549174418163808 ) ) ;
#110983 = CARTESIAN_POINT ( 'NONE',  ( -0.7500000000000215383, 3.441666666666689967, 1.299038105676671107 ) ) ;
#110984 = CARTESIAN_POINT ( 'NONE',  ( 5.823390672269506574, 6.752709524857930745, -1.199719254218446718 ) ) ;
#110985 = EDGE_CURVE ( 'NONE', #120459, #60268, #23208, .T. ) ;
#110986 = CARTESIAN_POINT ( 'NONE',  ( 2.930584098205230248, -1.096850167032170420, -1.931549987457868989 ) ) ;
#110987 = CARTESIAN_POINT ( 'NONE',  ( 4.370186222871176085, 4.005496238621469196, 0.1648321253336959835 ) ) ;
#110988 = CARTESIAN_POINT ( 'NONE',  ( 6.751597309925441159, 9.860318714012938912, -1.082531754730537088 ) ) ;
#110989 = ADVANCED_FACE ( 'NONE', ( #42319 ), #49439, .T. ) ;
#110990 = CARTESIAN_POINT ( 'NONE',  ( 0.4571195463272426651, 7.927888240403390796, 1.992899296338177306 ) ) ;
#110991 = CARTESIAN_POINT ( 'NONE',  ( 5.090160327287878594, 4.903218234782778850, -0.7998128361456481317 ) ) ;
#110992 = CARTESIAN_POINT ( 'NONE',  ( 0.9674229098759130618, -1.967888300253183953, -0.4390273639364171698 ) ) ;
#110994 = CARTESIAN_POINT ( 'NONE',  ( 5.178211798877670802, -1.100624681205965461, -1.744318484351764509 ) ) ;
#110993 = CARTESIAN_POINT ( 'NONE',  ( 8.860417081730671995, 10.29590700256267155, 1.199719254218453823 ) ) ;
#110995 = CARTESIAN_POINT ( 'NONE',  ( -0.7499999999999972244, 5.358333333333353821, -1.299038105676652011 ) ) ;
#110996 = CARTESIAN_POINT ( 'NONE',  ( -2.754277761870538299, 6.365074488824250309, 1.040834085586084257E-14 ) ) ;
#110997 = FACE_OUTER_BOUND ( 'NONE', #105703, .T. ) ;
#110998 = CARTESIAN_POINT ( 'NONE',  ( 1.364683531249986537, 0.4052083336747511200, -0.7879004041258309554 ) ) ;
#110999 = CARTESIAN_POINT ( 'NONE',  ( 0.2976568962721929390, -1.769157359987379996, -0.05240849467303894393 ) ) ;
#111000 = CARTESIAN_POINT ( 'NONE',  ( 5.572856105055380205, -0.7716597722284452843, 1.553080519226685885 ) ) ;
#111001 = CARTESIAN_POINT ( 'NONE',  ( 5.425286103790146974, -1.110369212591550747, -1.340227399214832360 ) ) ;
#111002 = B_SPLINE_CURVE_WITH_KNOTS ( 'NONE', 3,
 ( #158048, #159093, #207828, #12817 ),
 .UNSPECIFIED., .F., .F.,
 ( 4, 4 ),
 ( 0.000000000000000000, 0.0006799945003891866378 ),
 .UNSPECIFIED. ) ;
#111003 = CARTESIAN_POINT ( 'NONE',  ( 2.964700083287651999, -2.118976988643240578, -0.8750470330559836363 ) ) ;
#111004 = CARTESIAN_POINT ( 'NONE',  ( 0.6823417656249882723, -0.6572916663252492686, 1.181850606188755259 ) ) ;
#111005 = CARTESIAN_POINT ( 'NONE',  ( 2.466542765887615563, 0.09048117372523720170, -1.839033023284454060 ) ) ;
#111006 = CARTESIAN_POINT ( 'NONE',  ( 10.07100917685271035, 10.64393221595000938, 0.7998128361456462443 ) ) ;
#111007 = CARTESIAN_POINT ( 'NONE',  ( -10.71870444596734195, 5.124999999999999112, -5.395310463726811001 ) ) ;
#111008 = CARTESIAN_POINT ( 'NONE',  ( 2.309345278970798887, -0.4025885200794159235, 1.780468244869021222 ) ) ;
#111009 = CARTESIAN_POINT ( 'NONE',  ( 2.233046271152541618, 2.016033844848092560, 0.04667593304989729741 ) ) ;
#111010 = CARTESIAN_POINT ( 'NONE',  ( -4.731432421044888592, 4.622352034081546712, -0.7216878364870207285 ) ) ;
#111011 = CARTESIAN_POINT ( 'NONE',  ( 8.132223770642788452, 15.75611528059600097, -8.453506921246367156 ) ) ;
#111012 = CARTESIAN_POINT ( 'NONE',  ( 4.243269300766455920, -1.833519874744583111, 1.035826785333898270 ) ) ;
#111013 = CARTESIAN_POINT ( 'NONE',  ( -5.201524489137236529, 9.220195670635433771, 0.7998128361456481317 ) ) ;
#111014 = CARTESIAN_POINT ( 'NONE',  ( 8.332566079752199428, 13.17553009179483148, 8.539185921479196750 ) ) ;
#111015 = CARTESIAN_POINT ( 'NONE',  ( 2.488806849732328796, 2.007603858877416769, 0.5053560088097220904 ) ) ;
#111016 = CARTESIAN_POINT ( 'NONE',  ( 3.734381245560244089, 6.444196322207211836, 1.199719254218462483 ) ) ;
#111017 = CARTESIAN_POINT ( 'NONE',  ( 0.6801582343749900117, -0.6614583329919085930, -1.178068619123883165 ) ) ;
#111018 = CARTESIAN_POINT ( 'NONE',  ( 5.092489908381383934, -1.177591669451777179, 1.763244422785560150 ) ) ;
#111019 = CARTESIAN_POINT ( 'NONE',  ( 6.410779360540267646, 1.349177972556347971, -1.230185023894624141 ) ) ;
#111020 = EDGE_LOOP ( 'NONE', ( #115635, #212303, #185197, #36293 ) ) ;
#111021 = CARTESIAN_POINT ( 'NONE',  ( -5.387385936583832802, 7.378645907471495846, -1.599625672291271394 ) ) ;
#111022 = CARTESIAN_POINT ( 'NONE',  ( 9.154780037725547714, 11.70366268214508487, 1.599625672291279388 ) ) ;
#111023 = CARTESIAN_POINT ( 'NONE',  ( 4.651856102820254968, 7.480896982382013505, -1.082531754730548412 ) ) ;
#111024 = CARTESIAN_POINT ( 'NONE',  ( 3.475000000000000533, -1.560416665710748996, 2.006292185433948827 ) ) ;
#111025 = CARTESIAN_POINT ( 'NONE',  ( -6.417086777969760902, 6.381022750586497594, 0.7998128361456341429 ) ) ;
#111026 = CARTESIAN_POINT ( 'NONE',  ( 5.976833544478475702, -1.498421880457675215, 1.500811427713820478 ) ) ;
#111027 = CARTESIAN_POINT ( 'NONE',  ( 0.9738169395155724661, 2.029595412481857153, -0.5617393031529455127 ) ) ;
#111028 = CARTESIAN_POINT ( 'NONE',  ( -5.276058054373441664, 6.184431147304315424, -1.199719254218453823 ) ) ;
#111029 = CARTESIAN_POINT ( 'NONE',  ( 9.738834413317897898, 10.25639499182604730, 0.000000000000000000 ) ) ;
#111030 = CARTESIAN_POINT ( 'NONE',  ( 6.614093472281312280, 1.855988364702824800, -0.1360997465041282051 ) ) ;
#111031 = CARTESIAN_POINT ( 'NONE',  ( 8.911787042884274257, 9.291506392986812912, 0.7998128361456462443 ) ) ;
#111032 = CARTESIAN_POINT ( 'NONE',  ( -6.966220764712169000, 6.002124920821316323, -2.420000000000000373 ) ) ;
#111033 = CARTESIAN_POINT ( 'NONE',  ( -4.604929450496978660, 5.401447776115099408, -1.199719254218453823 ) ) ;
#111034 = CARTESIAN_POINT ( 'NONE',  ( -8.920901888112002354, 11.43080484092926241, 1.443375672974064550 ) ) ;
#111035 = CARTESIAN_POINT ( 'NONE',  ( -9.928151704202875294, 5.423124072284297270, 6.082134274749043001 ) ) ;
#111036 = CARTESIAN_POINT ( 'NONE',  ( 6.938893903907228378E-15, 10.64264068711930733, 1.214306433183764966E-14 ) ) ;
#111038 = CARTESIAN_POINT ( 'NONE',  ( 2.471086628630547288, 1.751123931924388089, 0.8847596551376719631 ) ) ;
#111037 = CARTESIAN_POINT ( 'NONE',  ( -7.640183256500752584, 8.872300873127729304, -1.199719254218446718 ) ) ;
#111039 = CARTESIAN_POINT ( 'NONE',  ( 1.024558638192473170, 1.287004556549703693, -1.736669753874709343 ) ) ;
#111041 = CARTESIAN_POINT ( 'NONE',  ( -6.098685391867989303, 6.020399689055939696, 0.3646554611961040360 ) ) ;
#111040 = CARTESIAN_POINT ( 'NONE',  ( -4.437261413422502798, 8.398831758960053406, 0.000000000000000000 ) ) ;
#111042 = CARTESIAN_POINT ( 'NONE',  ( -0.6823417656250212460, 1.801041667008083991, 1.181850606188755259 ) ) ;
#111043 = CARTESIAN_POINT ( 'NONE',  ( 2.688496201417677867, -0.9952141288376895600, -1.419535560660119655 ) ) ;
#111044 = CARTESIAN_POINT ( 'NONE',  ( 2.466429552724667129, 0.08583113499382444278, -1.738331801394930043 ) ) ;
#111045 = CARTESIAN_POINT ( 'NONE',  ( 8.283668668269706714, 8.766627655843892697, 1.040834085586084257E-14 ) ) ;
#111046 = CARTESIAN_POINT ( 'NONE',  ( -10.48267169704037727, 5.268073273308885973, 5.153989745587932880 ) ) ;
#111047 = CARTESIAN_POINT ( 'NONE',  ( 2.354842093047845530, -0.8645933883619570937, 1.821462535208747457 ) ) ;
#111048 = CARTESIAN_POINT ( 'NONE',  ( 6.925078400183552141, 7.052169149086129352, 2.642497803771151954 ) ) ;
#111049 = CARTESIAN_POINT ( 'NONE',  ( -4.472210567661380587, 6.310941310395290493, 1.599625672291270506 ) ) ;
#111050 = AXIS2_PLACEMENT_3D ( 'NONE', #33951, #198564, #182322 ) ;
#111051 = CARTESIAN_POINT ( 'NONE',  ( 0.7605432175010603535, -1.429589592961340028, 1.357792370201470256 ) ) ;
#111053 = CARTESIAN_POINT ( 'NONE',  ( -5.966997003790232235, 7.094489604910957148, -1.082531754730549967 ) ) ;
#111052 = CARTESIAN_POINT ( 'NONE',  ( 5.484596585704371918, -1.208295678440996390, 1.482354609825987435 ) ) ;
#111054 = CARTESIAN_POINT ( 'NONE',  ( -5.926322542504872892, 8.007405281046052536, -1.443375672974066548 ) ) ;
#111055 = CARTESIAN_POINT ( 'NONE',  ( 5.742760583840166966, 8.857581893525663830, 1.199719254218452047 ) ) ;
#111056 = CARTESIAN_POINT ( 'NONE',  ( -5.108390017298964914, 9.181815130149269422, 0.000000000000000000 ) ) ;
#111057 = CARTESIAN_POINT ( 'NONE',  ( 1.383469627199322538, 0.1461868815116218467, -2.014428406654201531 ) ) ;
#111058 = LINE ( 'NONE', #13481, #69805 ) ;
#111059 = CARTESIAN_POINT ( 'NONE',  ( 4.700386263483860461, -2.306923794945021200, -0.06181454844297362694 ) ) ;
#111061 = EDGE_CURVE ( 'NONE', #109578, #93416, #45900, .T. ) ;
#111060 = CARTESIAN_POINT ( 'NONE',  ( 6.144970055084349347, -0.2864424343173576082, -1.940704187532462210 ) ) ;
#111062 = CARTESIAN_POINT ( 'NONE',  ( 3.203904402660478379, 0.7104733393662396868, -1.828749470067204896 ) ) ;
#111063 = CARTESIAN_POINT ( 'NONE',  ( 9.745613490124728884, 10.26430391476735338, 0.7998128361456462443 ) ) ;
#111064 = CARTESIAN_POINT ( 'NONE',  ( -9.498276863272749893, 14.58059102403192320, 7.333831086845977509 ) ) ;
#111065 = EDGE_LOOP ( 'NONE', ( #145193, #34101, #28938, #40514 ) ) ;
#111066 = CARTESIAN_POINT ( 'NONE',  ( 1.165409582065090266, 1.953992404094638591, -0.8159742408818432269 ) ) ;
#111068 = CARTESIAN_POINT ( 'NONE',  ( -8.290974629956718189, 9.631557475493025322, -1.199719254218446718 ) ) ;
#111067 = CARTESIAN_POINT ( 'NONE',  ( -3.785751206713858785, 5.439795712631356750, 1.599625672291267398 ) ) ;
#111069 = CARTESIAN_POINT ( 'NONE',  ( 1.464538624043790316, 0.1369371521719800755, -1.836096087760468398 ) ) ;
#111070 = ORIENTED_EDGE ( 'NONE', *, *, #153873, .T. ) ;
#111071 = CARTESIAN_POINT ( 'NONE',  ( 11.95134404050519272, 7.565927718848042716, -0.2102339791074976649 ) ) ;
#111072 = CARTESIAN_POINT ( 'NONE',  ( 2.443736651115399283, -1.977012053918187906, 0.7674769708189137507 ) ) ;
#111073 = CARTESIAN_POINT ( 'NONE',  ( -0.7499999999999972244, 4.889583334016150751, -1.299038105676652899 ) ) ;
#111074 = CARTESIAN_POINT ( 'NONE',  ( 6.089583550832340819, 10.25626457594641749, 1.040834085586084257E-14 ) ) ;
#111075 = CARTESIAN_POINT ( 'NONE',  ( -0.6125000000000279110, 2.520833334016120197, -1.060881119635969094 ) ) ;
#111076 = ORIENTED_EDGE ( 'NONE', *, *, #212414, .F. ) ;
#111077 = CARTESIAN_POINT ( 'NONE',  ( 3.567699708620798216, 2.011335548252995764, -0.4479969848151729162 ) ) ;
#111078 = AXIS2_PLACEMENT_3D ( 'NONE', #157978, #23674, #89784 ) ;
#111080 = FACE_OUTER_BOUND ( 'NONE', #118880, .T. ) ;
#111079 = CARTESIAN_POINT ( 'NONE',  ( -7.934546212495630968, 10.28005655271014795, -1.599625672291263179 ) ) ;
#111081 = CARTESIAN_POINT ( 'NONE',  ( -0.6823417656249969321, 3.467708333674754506, -1.181850606188749264 ) ) ;
#111082 = CARTESIAN_POINT ( 'NONE',  ( -3.475000000000000533, -2.829166666666666163, -2.006292185433948827 ) ) ;
#111083 = DIRECTION ( 'NONE',  ( 0.000000000000000000, 0.000000000000000000, 1.000000000000000000 ) ) ;
#111084 = CARTESIAN_POINT ( 'NONE',  ( 2.706632988724329891, -0.8634771713065221288, -2.091333714195188431 ) ) ;
#111085 = CARTESIAN_POINT ( 'NONE',  ( -8.839552966430007430, 11.33589776563360019, -1.443375672974059665 ) ) ;
#111086 = CARTESIAN_POINT ( 'NONE',  ( 2.320317256442219644, -0.6965147209693119956, -1.672536871252501500 ) ) ;
#111087 = CARTESIAN_POINT ( 'NONE',  ( 3.362411380332845035, -1.847649188899632255, -0.5059680389012406465 ) ) ;
#111088 = CARTESIAN_POINT ( 'NONE',  ( 4.668459276380106715, -0.8822503692092443783, -1.873099891353036561 ) ) ;
#111089 = CARTESIAN_POINT ( 'NONE',  ( 0.6823417656249882723, 2.488541667008084435, -1.181850606188749264 ) ) ;
#111090 = STYLED_ITEM ( 'NONE', ( #18640 ), #164931 ) ;
#111091 = CARTESIAN_POINT ( 'NONE',  ( 1.727351915365995083, -1.857048012799527248, 0.6622322079550806428 ) ) ;
#111092 = CARTESIAN_POINT ( 'NONE',  ( 6.375613808387889492, 1.842787572768100457, -0.5617375553943514399 ) ) ;
#111093 = CARTESIAN_POINT ( 'NONE',  ( 2.887410755087606695, 1.321643875934110479, 1.324118206929347563 ) ) ;
#111095 = CARTESIAN_POINT ( 'NONE',  ( 4.632842592818133376, 8.443130954262043630, -0.3954830847591808696 ) ) ;
#111094 = CARTESIAN_POINT ( 'NONE',  ( 2.315413608375629817, 2.062204878978285194, 1.035883635760030508 ) ) ;
#111096 = CARTESIAN_POINT ( 'NONE',  ( 2.840123846975282973, -0.9592540151425684725, 1.594648687322928859 ) ) ;
#111097 = CARTESIAN_POINT ( 'NONE',  ( -0.6823417656250212460, 3.301041667008085323, 1.181850606188767472 ) ) ;
#111098 = CARTESIAN_POINT ( 'NONE',  ( 6.285603487943992818, -1.943538462464271088, 0.6912672899390749359 ) ) ;
#111099 = CARTESIAN_POINT ( 'NONE',  ( -5.610376637956639101, 5.439860920571172542, 0.000000000000000000 ) ) ;
#111100 = CARTESIAN_POINT ( 'NONE',  ( 7.287671262545424966, 8.461036880179857889, -1.199719254218451159 ) ) ;
#111101 = CARTESIAN_POINT ( 'NONE',  ( -1.478132491927081960, 3.421797542362725153, -0.2687277897297897788 ) ) ;
#111102 = CARTESIAN_POINT ( 'NONE',  ( 6.616252143301227129, -0.9890948110137095517, -1.859226117534703571 ) ) ;
#111103 = CARTESIAN_POINT ( 'NONE',  ( -1.364683531249997417, 4.321875000341417028, 1.214306433183764966E-14 ) ) ;
#111104 = CARTESIAN_POINT ( 'NONE',  ( 6.362596528949501895, -1.533591692085239266, 1.523617273982772247 ) ) ;
#111106 = EDGE_CURVE ( 'NONE', #100761, #161998, #106284, .T. ) ;
#111105 = CARTESIAN_POINT ( 'NONE',  ( 6.305333282589566934, 1.756257216537491450, -0.9971998561906397773 ) ) ;
#111107 = CARTESIAN_POINT ( 'NONE',  ( 0.6823417656249882723, -0.07395833299191079124, -1.181850606188749264 ) ) ;
#111108 = CARTESIAN_POINT ( 'NONE',  ( -4.690757960648240577, 6.495636925554817864, 1.443375672974064550 ) ) ;
#111109 = ADVANCED_FACE ( 'NONE', ( #105187 ), #204765, .T. ) ;
#111112 = CARTESIAN_POINT ( 'NONE',  ( 4.907688418466886304, 5.788353245375237321, -1.082531754730548412 ) ) ;
#111111 = CARTESIAN_POINT ( 'NONE',  ( 0.000000000000000000, -0.5468749995220422155, -3.793834371823813001 ) ) ;
#111110 = CARTESIAN_POINT ( 'NONE',  ( 7.062871678076271920, 7.204714810702593120, -0.7998128361456341429 ) ) ;
#111113 = CARTESIAN_POINT ( 'NONE',  ( -2.979759899953417612, 6.698413326579433225, 0.7998128361456352531 ) ) ;
#111115 = CARTESIAN_POINT ( 'NONE',  ( 2.975796278104340331, -0.8128168404246680634, 1.845627246706407210 ) ) ;
#111114 = CARTESIAN_POINT ( 'NONE',  ( 5.225796113160614986, 0.8128206588041908542, -1.845625551132886288 ) ) ;
#111116 = CARTESIAN_POINT ( 'NONE',  ( -7.660520486921249983, 8.896027641951645748, -1.199719254218446718 ) ) ;
#111118 = CARTESIAN_POINT ( 'NONE',  ( -6.821160681006823268, 9.051383109298335228, 1.443375672974064550 ) ) ;
#111117 = CARTESIAN_POINT ( 'NONE',  ( -9.219181267612684749, 10.81842823604534765, 1.082531754730558626 ) ) ;
#111119 = CARTESIAN_POINT ( 'NONE',  ( 1.499999999999990896, 5.025000000000022560, 1.214306433183764966E-14 ) ) ;
#111121 = CARTESIAN_POINT ( 'NONE',  ( 1.364683531249997417, 9.984375000341398021, 2.602085213965210642E-15 ) ) ;
#111120 = CARTESIAN_POINT ( 'NONE',  ( 6.245025451202089073, -1.828886558906620774, 1.152162773130911644 ) ) ;
#111122 = DIRECTION ( 'NONE',  ( 0.000000000000000000, 0.000000000000000000, 1.000000000000000000 ) ) ;
#111123 = CARTESIAN_POINT ( 'NONE',  ( -11.31504510220803894, 6.390522733111290599, -4.000539294108416577 ) ) ;
#111125 = CARTESIAN_POINT ( 'NONE',  ( 0.1400564425528905699, 0.7337865575636399740, 1.769695213874568962 ) ) ;
#111124 = CARTESIAN_POINT ( 'NONE',  ( -5.694061327615147050, 9.586895948952255608, 0.000000000000000000 ) ) ;
#111126 = CARTESIAN_POINT ( 'NONE',  ( -1.402160292154681736E-14, -0.8656249996585829720, 1.575800808251672791 ) ) ;
#111127 = LINE ( 'NONE', #177130, #48238 ) ;
#111128 = CARTESIAN_POINT ( 'NONE',  ( 1.787319861506628804, 1.187891131197996497, 1.250883549239764081 ) ) ;
#111129 = CARTESIAN_POINT ( 'NONE',  ( 6.318982112420993502, 9.529840343536603697, -1.199719254218452047 ) ) ;
#111130 = CARTESIAN_POINT ( 'NONE',  ( 6.530187263637528439, 7.647581891445782709, -1.199719254218452047 ) ) ;
#111131 = CARTESIAN_POINT ( 'NONE',  ( 0.1216811705908975721, 2.536982183874236352, -1.996294991408742003 ) ) ;
#111132 = CARTESIAN_POINT ( 'NONE',  ( 0.4734442463095941411, 1.011852719971978232, 1.451749726636430093 ) ) ;
#111133 = CARTESIAN_POINT ( 'NONE',  ( -3.633221978782283923, 7.182583375313884133, -0.7216878364870267237 ) ) ;
#111134 = CARTESIAN_POINT ( 'NONE',  ( 2.104154084628720334, -0.8588668247239000797, 1.820802598171267439 ) ) ;
#111135 = CARTESIAN_POINT ( 'NONE',  ( -0.3914079065636231203, 3.043201908700346792, -0.4248930002255434379 ) ) ;
#111136 = CARTESIAN_POINT ( 'NONE',  ( 3.926972183325681875, 2.094573593246536802, 0.6948772193901550098 ) ) ;
#111137 = VECTOR ( 'NONE', #24669, 1000.000000000000000 ) ;
#111138 = B_SPLINE_CURVE_WITH_KNOTS ( 'NONE', 3,
 ( #210834, #81904, #16881, #131772 ),
 .UNSPECIFIED., .F., .F.,
 ( 4, 4 ),
 ( 8.516827915679375891E-05, 0.0002597075693986928267 ),
 .UNSPECIFIED. ) ;
#111139 = CARTESIAN_POINT ( 'NONE',  ( 5.805598453987085072, -1.706804643700374102, -1.341652511797826186 ) ) ;
#111140 = VERTEX_POINT ( 'NONE', #187472 ) ;
#111141 = CARTESIAN_POINT ( 'NONE',  ( 2.925527285498711549, 6.635141943048991742, 0.7998128361456281477 ) ) ;
#111143 = CARTESIAN_POINT ( 'NONE',  ( 7.985389288324691748, 10.33937347451072775, -1.443375672974058777 ) ) ;
#111142 = CIRCLE ( 'NONE', #159469, 3.971937515251341644 ) ;
#111145 = CARTESIAN_POINT ( 'NONE',  ( 2.724232643812212196, 2.001515029240468646, 0.2440086781289458329 ) ) ;
#111144 = CARTESIAN_POINT ( 'NONE',  ( 3.422626747576805961, -0.8610355553571764631, -1.937992358232228041 ) ) ;
#111147 = ORIENTED_EDGE ( 'NONE', *, *, #129564, .T. ) ;
#111146 = CARTESIAN_POINT ( 'NONE',  ( 3.269578866965703767, 0.4354455071775619190, -1.758352452871074334 ) ) ;
#111148 = CARTESIAN_POINT ( 'NONE',  ( 5.580062740476173566, 8.667767742934335828, 1.199719254218451159 ) ) ;
#111149 = VERTEX_POINT ( 'NONE', #40170 ) ;
#111150 = CARTESIAN_POINT ( 'NONE',  ( 0.3209005354254980680, -0.09642172165634513292, 1.868300368337752815 ) ) ;
#111151 = CARTESIAN_POINT ( 'NONE',  ( 5.126954644262057492, 9.133197518281081173, 0.7998128361456462443 ) ) ;
#111152 = EDGE_CURVE ( 'NONE', #41918, #20303, #48362, .T. ) ;
#111154 = CARTESIAN_POINT ( 'NONE',  ( 1.938566325679047297, -1.478098309594473525, 1.218629399928832013 ) ) ;
#111153 = CARTESIAN_POINT ( 'NONE',  ( -4.928552533767591726, 5.708731696605642725, 1.199719254218462483 ) ) ;
#111155 = CARTESIAN_POINT ( 'NONE',  ( 0.000000000000000000, 5.999999999999998224, -11.00000000000000000 ) ) ;
#111156 = CARTESIAN_POINT ( 'NONE',  ( -11.96217875511318063, 12.27145633421023341, -0.9561995067075080845 ) ) ;
#111157 = CARTESIAN_POINT ( 'NONE',  ( -0.6823417656250212460, 1.863541667008083991, 1.181850606188755259 ) ) ;
#111158 = DIRECTION ( 'NONE',  ( 0.000000000000000000, 0.000000000000000000, 1.000000000000000000 ) ) ;
#111159 = CARTESIAN_POINT ( 'NONE',  ( -8.025536864285518490, 11.45054454405341282, -1.199719254218446718 ) ) ;
#111160 = CARTESIAN_POINT ( 'NONE',  ( 5.366167234668930419, 1.061923416652654550, 1.882811416686725359 ) ) ;
#111161 = CARTESIAN_POINT ( 'NONE',  ( -6.129694847154231852, 6.323934541200937787, -0.7216878364870338292 ) ) ;
#111162 = CARTESIAN_POINT ( 'NONE',  ( -7.910256278930404505, 8.193330178365746619, -0.7998128361456362523 ) ) ;
#111163 = CARTESIAN_POINT ( 'NONE',  ( 2.689816194747224110, 2.012238202079220439, -0.6693303307304664385 ) ) ;
#111165 = CARTESIAN_POINT ( 'NONE',  ( -12.76914910123260682, 7.416938840849524262, -2.145643146812736823 ) ) ;
#111164 = CARTESIAN_POINT ( 'NONE',  ( -0.1296875068448125057, 7.629137130509072939, -2.426516348560475933 ) ) ;
#111166 = CARTESIAN_POINT ( 'NONE',  ( 4.552002736099131752, 1.970983365533407694, -0.04540313215006633318 ) ) ;
#111167 = CARTESIAN_POINT ( 'NONE',  ( 0.01783784634934187929, -0.5327901187049766119, 1.941387642157591742 ) ) ;
#111168 = ORIENTED_EDGE ( 'NONE', *, *, #24646, .T. ) ;
#111169 = CARTESIAN_POINT ( 'NONE',  ( 6.087133394233009476, 1.761630753581880704, 1.174362570269470218 ) ) ;
#111170 = CARTESIAN_POINT ( 'NONE',  ( 1.777638883463123598, -0.9165151389911446733, 1.199999999999999734 ) ) ;
#111171 = CARTESIAN_POINT ( 'NONE',  ( 0.5200892513525963157, 2.048054262204841880, -0.3022008342252607838 ) ) ;
#111172 = CARTESIAN_POINT ( 'NONE',  ( 2.976435162280165247, -0.1435924003432750840, -1.936700533151126891 ) ) ;
#111173 = ORIENTED_EDGE ( 'NONE', *, *, #158482, .T. ) ;
#111174 = CARTESIAN_POINT ( 'NONE',  ( -4.253564693897453175, 7.314528304839084782, -0.9025151233474463242 ) ) ;
#111175 = CARTESIAN_POINT ( 'NONE',  ( 7.035755370848908896, 7.173079118937375931, 0.7998128361456352531 ) ) ;
#111177 = CARTESIAN_POINT ( 'NONE',  ( 5.296431564432884542, 9.330920591813708143, 1.040834085586084257E-14 ) ) ;
#111176 = CARTESIAN_POINT ( 'NONE',  ( 3.714856679239968873, -0.1534820204720024339, 2.085054752100850894 ) ) ;
#111178 = CARTESIAN_POINT ( 'NONE',  ( 3.051993976407674225, 6.574760382535328240, -0.7216878364870338292 ) ) ;
#111180 = ORIENTED_EDGE ( 'NONE', *, *, #178838, .T. ) ;
#111179 = CARTESIAN_POINT ( 'NONE',  ( 0.01197859805690624189, -1.811022649853447630, -0.04676520365421397291 ) ) ;
#111181 = CARTESIAN_POINT ( 'NONE',  ( 5.865903189996043210, 2.174886565178067777, -0.3735607071253947975 ) ) ;
#111182 = LINE ( 'NONE', #41872, #68115 ) ;
#111183 = CARTESIAN_POINT ( 'NONE',  ( 3.118423654462946892, -1.086285162511631652, -1.920806481261853493 ) ) ;
#111184 = CARTESIAN_POINT ( 'NONE',  ( -10.95308175811721085, 12.29999999999998295, 1.799999999999999600 ) ) ;
#111185 = CARTESIAN_POINT ( 'NONE',  ( 1.682132150489405564, 0.9841149911452107268, 1.639481845682550398 ) ) ;
#111186 = CARTESIAN_POINT ( 'NONE',  ( 10.23370702021670020, 10.83374636654133383, 0.7998128361456462443 ) ) ;
#111187 = CARTESIAN_POINT ( 'NONE',  ( 5.072747062355987602, 1.430223858385268665, -1.497173470029027120 ) ) ;
#111189 = CARTESIAN_POINT ( 'NONE',  ( 2.711983997553393699, -2.138339778157403615, 0.3160903847422363300 ) ) ;
#111188 = CARTESIAN_POINT ( 'NONE',  ( 0.008173644115962452189, -6.287979527546275094, 10.90726532705803820 ) ) ;
#111190 = CARTESIAN_POINT ( 'NONE',  ( 4.775033345069852331, 2.044829088842615494, -0.7888500489584143738 ) ) ;
#111191 = ORIENTED_EDGE ( 'NONE', *, *, #148232, .F. ) ;
#111192 = CARTESIAN_POINT ( 'NONE',  ( 8.563946585326370098, 13.14302144952281814, 0.7998128361456462443 ) ) ;
#111193 = CARTESIAN_POINT ( 'NONE',  ( 1.220146605508150803E-14, 9.468750000682799595, -1.499999999999998446 ) ) ;
#111194 = CARTESIAN_POINT ( 'NONE',  ( -0.05606965051303709063, 7.151966587341615167, 1.999903488156155262 ) ) ;
#111195 = CARTESIAN_POINT ( 'NONE',  ( 5.737035277238070385, 6.722237907313067140, -1.199719254218452047 ) ) ;
#111196 = CARTESIAN_POINT ( 'NONE',  ( -1.642778471874998480, -2.238541666188708312, 2.845375778867863303 ) ) ;
#111197 = CARTESIAN_POINT ( 'NONE',  ( -5.164730172163054966, 4.990216387137135889, -0.7998128361456362523 ) ) ;
#111198 = CARTESIAN_POINT ( 'NONE',  ( 0.2642963535325442703, 1.880433764241522088, -0.7283817610406128074 ) ) ;
#111199 = AXIS2_PLACEMENT_3D ( 'NONE', #181580, #671, #146994 ) ;
#111200 = CARTESIAN_POINT ( 'NONE',  ( -9.327646496521989405, 10.94497100310623594, -1.082531754730539753 ) ) ;
#111201 = CARTESIAN_POINT ( 'NONE',  ( 5.520104819419390907, 6.469152373191302985, 1.199719254218452935 ) ) ;
#111202 = CARTESIAN_POINT ( 'NONE',  ( 4.539934223682924319, 1.348354173984022575, 1.571082123823979826 ) ) ;
#111203 = CARTESIAN_POINT ( 'NONE',  ( 2.912629423498619197, 1.395154039405178903, -1.328744637545350882 ) ) ;
#111204 = CARTESIAN_POINT ( 'NONE',  ( 0.1578276607246929530, 1.163290555716024244, 1.646825313395771762 ) ) ;
#111205 = CARTESIAN_POINT ( 'NONE',  ( -4.900252779738026199, 4.865835280224682258, -0.2959858980189531419 ) ) ;
#111206 = CARTESIAN_POINT ( 'NONE',  ( 4.313465427442102929, 8.184126765324453601, 0.7998128361456462443 ) ) ;
#111207 = DIRECTION ( 'NONE',  ( 0.000000000000000000, 1.000000000000000000, 0.000000000000000000 ) ) ;
#111208 = CARTESIAN_POINT ( 'NONE',  ( 4.205875300247041260, 0.6677108253347485700, -1.852911535531636789 ) ) ;
#111209 = CARTESIAN_POINT ( 'NONE',  ( 0.3225714733509216781, 2.098294765757203528, 0.6321472216322538973 ) ) ;
#111210 = CARTESIAN_POINT ( 'NONE',  ( 3.650846181029033133, -1.491723252493650786, 1.052289205326198074 ) ) ;
#111211 = PRODUCT_DEFINITION_SHAPE ( 'NONE', 'NONE',  #214415 ) ;
#111212 = CARTESIAN_POINT ( 'NONE',  ( 7.404161286838808920, 8.771181268467660885, -1.082531754730548412 ) ) ;
#111213 = CARTESIAN_POINT ( 'NONE',  ( 2.806174607904299734, 5.257325561654889512, -1.082531754730543083 ) ) ;
#111214 = CARTESIAN_POINT ( 'NONE',  ( -6.688968683495758683, 8.897159112202094988, -1.599625672291271394 ) ) ;
#111215 = CARTESIAN_POINT ( 'NONE',  ( 4.553559489343365740, 6.405848385690952718, -1.599625672291269396 ) ) ;
#111216 = ORIENTED_EDGE ( 'NONE', *, *, #86952, .T. ) ;
#111218 = CARTESIAN_POINT ( 'NONE',  ( 5.607686816480834224, 1.527379804643314687, 1.311666717936723403 ) ) ;
#111217 = CARTESIAN_POINT ( 'NONE',  ( 1.487592393518050837, -1.832424703912252317, -0.1798031890194173865 ) ) ;
#111219 = CARTESIAN_POINT ( 'NONE',  ( 0.4921457485732755321, 2.200376924867069484, 0.6639341530902067579 ) ) ;
#111220 = CARTESIAN_POINT ( 'NONE',  ( 5.014483083204026137, 0.7471541359172824137, 1.814103259000845458 ) ) ;
#111221 = CARTESIAN_POINT ( 'NONE',  ( -6.531277313481209212, 8.642909503859968368, 1.599625672291283607 ) ) ;
#111222 = CYLINDRICAL_SURFACE ( 'NONE', #22555, 1.500000000000000222 ) ;
#111223 = CARTESIAN_POINT ( 'NONE',  ( -3.164938793786285842, 5.779846795137578930, -1.199719254218452935 ) ) ;
#111224 = SURFACE_STYLE_FILL_AREA ( #99172 ) ;
#111225 = CARTESIAN_POINT ( 'NONE',  ( -5.635349125135588721, 6.603604063193491136, 1.199719254218452935 ) ) ;
#111227 = CARTESIAN_POINT ( 'NONE',  ( 6.420749384593221087, 1.653102913324438816, 0.6326092773807339142 ) ) ;
#111226 = CARTESIAN_POINT ( 'NONE',  ( 1.980132433977495499, -2.051005990652774447, -0.4047881525126810209 ) ) ;
#111228 = DIRECTION ( 'NONE',  ( 1.000000000000000000, 0.000000000000000000, 0.000000000000000000 ) ) ;
#111229 = CARTESIAN_POINT ( 'NONE',  ( -0.1104750535120251204, 2.866086309876151539, -2.591737134608104842 ) ) ;
#111230 = CARTESIAN_POINT ( 'NONE',  ( 1.504977638028012432, -1.727349551440153119, 0.2125612633746311042 ) ) ;
#111231 = AXIS2_PLACEMENT_3D ( 'NONE', #57178, #105977, #140602 ) ;
#111232 = CARTESIAN_POINT ( 'NONE',  ( 3.988069740714122791, 7.804498464141805592, 0.7998128361456321445 ) ) ;
#111233 = DIRECTION ( 'NONE',  ( 1.000000000000000000, 0.000000000000000000, 0.000000000000000000 ) ) ;
#111234 = CARTESIAN_POINT ( 'NONE',  ( 1.347838067242516313, 1.722766431120416941, 0.08778956860019770936 ) ) ;
#111235 = CARTESIAN_POINT ( 'NONE',  ( 1.523247060345904291, -2.062048068855956373, 0.7425582295156886170 ) ) ;
#111236 = CARTESIAN_POINT ( 'NONE',  ( 3.721466898765386500, -0.1629207441977159332, 2.200919931280575170 ) ) ;
#111237 = CARTESIAN_POINT ( 'NONE',  ( -9.917242840447775265, 4.174869238508773783, -6.172972641688763140 ) ) ;
#111238 = CARTESIAN_POINT ( 'NONE',  ( 2.149520630032801805, 1.890536112741852959, -1.067247343769129442 ) ) ;
#111239 = CARTESIAN_POINT ( 'NONE',  ( 0.7678472254676466102, 0.8974085622692473674, 1.589837017038860045 ) ) ;
#111240 = CARTESIAN_POINT ( 'NONE',  ( 3.942653875399897423, -1.566338124119817987, 1.424821879184964946 ) ) ;
#111241 = CARTESIAN_POINT ( 'NONE',  ( 6.539320575229250920, 3.702490941164796379, 2.411252750440337156 ) ) ;
#111242 = EDGE_LOOP ( 'NONE', ( #111920, #42560, #180341, #173071 ) ) ;
#111244 = CARTESIAN_POINT ( 'NONE',  ( -1.402160292154681736E-14, -0.1156249996585793222, 1.575800808251672791 ) ) ;
#111243 = CARTESIAN_POINT ( 'NONE',  ( 3.966586032518903959, -2.139059804502403850, -0.8247178969851276520 ) ) ;
#111245 = CARTESIAN_POINT ( 'NONE',  ( 0.07755575628181145265, 0.6932613274447991802, -2.271134039238668301 ) ) ;
#111246 = CARTESIAN_POINT ( 'NONE',  ( 3.246287715468270108, 5.874753870433235825, 1.199719254218450271 ) ) ;
#111248 = EDGE_CURVE ( 'NONE', #107614, #152613, #138904, .T. ) ;
#111247 = AXIS2_PLACEMENT_3D ( 'NONE', #98587, #212311, #32512 ) ;
#111249 = CARTESIAN_POINT ( 'NONE',  ( 6.199871938995108245, 1.529590366309235172, 1.610960538716522006 ) ) ;
#111250 = CARTESIAN_POINT ( 'NONE',  ( -5.395781948558855845, 9.238903340053241209, 0.7216878364870458196 ) ) ;
#111251 = CARTESIAN_POINT ( 'NONE',  ( 5.016153647376205171, 6.875265226737464985, 1.443375672974062551 ) ) ;
#111252 = CARTESIAN_POINT ( 'NONE',  ( -8.324343128666356506, 8.814081192973304724, 1.040834085586084257E-14 ) ) ;
#111253 = CARTESIAN_POINT ( 'NONE',  ( 4.421367491832268293, 7.211993602896056288, 1.082531754730549078 ) ) ;
#111254 = ORIENTED_EDGE ( 'NONE', *, *, #157474, .T. ) ;
#111255 = CARTESIAN_POINT ( 'NONE',  ( 4.430314669760617718, -1.560499787156752971, -1.277043788614096176 ) ) ;
#111257 = CARTESIAN_POINT ( 'NONE',  ( 2.430602512062591369, -1.272252061732727091, 1.623331442124707591 ) ) ;
#111256 = CARTESIAN_POINT ( 'NONE',  ( 6.636879889089462026, 7.701780277814560982, -1.199719254218446718 ) ) ;
#111258 = FACE_OUTER_BOUND ( 'NONE', #28687, .T. ) ;
#111259 = CARTESIAN_POINT ( 'NONE',  ( 3.892599500454932304, 7.555466827257172113, 0.7216878364870257245 ) ) ;
#111260 = CARTESIAN_POINT ( 'NONE',  ( -3.285556943750000514, -2.588541666188707513, -1.896917185911906500 ) ) ;
#111261 = CARTESIAN_POINT ( 'NONE',  ( 0.6823417656249899377, 4.426041667008086655, -1.181850606188754593 ) ) ;
#111262 = CARTESIAN_POINT ( 'NONE',  ( 5.525378525699438548, -1.388074942811763357, -1.695776126864618316 ) ) ;
#111263 = CARTESIAN_POINT ( 'NONE',  ( 2.250625165576759290, 1.976955744075848065, -0.3961026872240576702 ) ) ;
#111264 = CARTESIAN_POINT ( 'NONE',  ( 2.577489280727011778, -0.9446877197298314544, 1.580272903027237774 ) ) ;
#111265 = CARTESIAN_POINT ( 'NONE',  ( 5.849453209292126310, 8.911780279894442103, 1.199719254218462483 ) ) ;
#111267 = ADVANCED_FACE ( 'NONE', ( #56417 ), #45398, .T. ) ;
#111266 =( LENGTH_UNIT ( ) NAMED_UNIT ( * ) SI_UNIT ( .MILLI., .METRE. ) );
#111268 = CARTESIAN_POINT ( 'NONE',  ( 5.649374308873757577, -1.440485763676568443, -1.121356984487072328 ) ) ;
#111269 = CARTESIAN_POINT ( 'NONE',  ( 6.029922689959810178, -1.701949372586025744, 1.081063231324945528 ) ) ;
#111270 = CARTESIAN_POINT ( 'NONE',  ( -6.340409392685171674, 10.54889472477470846, 0.7998128361456481317 ) ) ;
#111272 = CARTESIAN_POINT ( 'NONE',  ( -5.679940009482361774, 5.591294530676332641, 0.7998128361456281477 ) ) ;
#111271 = CARTESIAN_POINT ( 'NONE',  ( 5.208033936170274103, -2.252144374781993363, 0.2163938657309023850 ) ) ;
#111273 = CARTESIAN_POINT ( 'NONE',  ( 1.014449334229026611, -0.9484566428747326361, -1.880489036503508959 ) ) ;
#111274 = CARTESIAN_POINT ( 'NONE',  ( -6.882699257592852504, 8.058845884393651460, -1.199719254218452047 ) ) ;
#111275 = CARTESIAN_POINT ( 'NONE',  ( 8.372323551638698902, 9.726464550788689323, 1.199719254218462483 ) ) ;
#111276 = CARTESIAN_POINT ( 'NONE',  ( 5.831415467209187575, 9.817418788470464008, 0.000000000000000000 ) ) ;
#111277 = CARTESIAN_POINT ( 'NONE',  ( -8.715193815486133033, 9.062147627688959872, 0.7998128361456462443 ) ) ;
#111278 = CARTESIAN_POINT ( 'NONE',  ( 1.913131547260902510, -0.6205095947705829840, 0.2971265334020881110 ) ) ;
#111279 = CARTESIAN_POINT ( 'NONE',  ( 6.846504384776753049, 9.010674420371453053, -1.443375672974058777 ) ) ;
#111280 = CARTESIAN_POINT ( 'NONE',  ( 4.085089063302896228, 7.714230733137671159, -0.6301764584765887633 ) ) ;
#111281 = CARTESIAN_POINT ( 'NONE',  ( -8.839552966430007430, 11.33589776563360019, -1.443375672974059665 ) ) ;
#111283 = CARTESIAN_POINT ( 'NONE',  ( 2.953626239309721679, -1.957189270898977762, 1.050815160798105552 ) ) ;
#111282 = CARTESIAN_POINT ( 'NONE',  ( 1.951583061186522583, -1.892041120407188304, 0.9578705467366486204 ) ) ;
#111284 = CARTESIAN_POINT ( 'NONE',  ( -1.992711204631002198E-15, 2.999999999999989342, 1.224999999999989875 ) ) ;
#111285 = CARTESIAN_POINT ( 'NONE',  ( -5.424143973919053785, 8.485862515284315677, 1.199719254218454489 ) ) ;
#111286 = CARTESIAN_POINT ( 'NONE',  ( 5.449487677688982679, 8.445153826357429949, -1.199719254218446718 ) ) ;
#111287 = CARTESIAN_POINT ( 'NONE',  ( 3.912515228517557286, 0.7039278570535618673, 1.831416474553926310 ) ) ;
#111288 = CARTESIAN_POINT ( 'NONE',  ( 9.215791728987056786, 11.77484298861683598, -1.599625672291262513 ) ) ;
#111290 =( BOUNDED_SURFACE ( )  B_SPLINE_SURFACE ( 1, 2, ( 
 ( #47664, #61757, #177652, #46587, #126842, #207990, #31396, #97470, #191736, #192800, #43392, #94284, #193878, #109513, #209044, #44459, #175521, #159249, #10849, #160324, #127926, #29261, #95353, #161403, #12987, #211185, #82253, #84396, #81202, #32452, #180826, #85460, #184017, #151546, #148344, #49765, #214345, #83313, #165649, #98521, #68113, #164583, #17238, #101711, #198134, #35634, #65975, #115891, #33512, #132123, #16168, #114827, #51908, #134250, #181876, #147280, #213312, #34572, #200256, #118031, #102787, #99585, #149399, #135305, #50831, #167784, #982, #19380, #199184, #67047, #64937, #3113, #52958, #69184, #116958, #166720, #100644, #133184, #182957, #201318, #18311, #150483, #168845, #131087, #119096, #197077, #2043, #185076, #36702, #48714, #156884, #140658, #123399, #107114, #39928, #21495, #6324, #106037, #121253, #172059, #37784, #20448, #88682, #104936, #87605, #24719, #153675, #72398, #5243, #103858, #74557, #173137, #71319, #205601, #55104, #138498, #154741, #189363, #190418, #124459, #137432, #41004, #204520, #187224, #56167, #203450, #90821, #122331, #8471, #206672, #86530, #42076, #58304, #108189, #186150, #188288, #70253, #152596, #23653, #22576, #89761, #4182, #155810, #136366, #7394, #38852, #202386, #170977, #73473, #139574, #57239, #54036, #120173, #169908, #44201, #143866, #95092, #92961, #195769, #210931, #211993, #79872, #10600, #63634, #60427, #11671, #161140, #109263, #175271, #47408, #129788, #159007, #194692, #209859, #208797, #77745, #76677, #128721, #61497, #178462, #112449, #174215, #25788, #46334, #30071, #125521, #27935, #9547, #91899, #127664, #176328, #94029, #62557, #193626, #157955, #12728, #142791, #75623, #26856, #126587, #78801, #110322, #29005, #177391, #96161, #160067, #45268, #144925, #192548, #141732, #162213, #207740, #145982, #111389, #59365, #13798, #191482, #43150, #48469, #114584, #201064, #31148, #97222, #166461, #100391, #101457, #164331, #98273, #2861, #116697, #180575, #182696, #113520, #64690, #213060, #117781, #1798, #183773, #32197, #82004, #150227 ),
 ( #115631, #18053, #148092, #84139, #16983, #200009, #163275, #214097, #130835, #50575, #181626, #83062, #132924, #15921, #14856, #65724, #147038, #33255, #35383, #80946, #34315, #179529, #68931, #196827, #131872, #67855, #197881, #49511, #167529, #134003, #51659, #149138, #99339, #165388, #720, #66784, #198929, #19127, #85206, #151290, #135051, #102527, #138247, #204261, #186967, #88424, #36452, #106852, #104677, #189113, #168589, #122070, #52706, #156631, #118836, #71063, #188033, #20189, #184822, #123156, #89502, #39663, #170725, #140401, #86277, #54850, #154490, #203203, #6069, #23391, #121000, #152347, #3925, #55912, #105771, #38599, #72139, #69995, #172882, #22311, #24456, #103600, #155557, #136107, #7137, #202123, #21243, #137179, #171797, #90570, #73209, #8220, #139316, #205345, #53782, #119915, #74305, #185891, #56982, #40747, #87350, #37525, #169658, #153416, #4987, #207488, #177134, #160886, #109000, #59107, #157698, #192290, #208538, #60174, #12481, #128474, #206420, #127403, #95909, #175017, #125267, #42891, #26604, #92705, #190172, #158751, #9295, #76420, #78555, #110066, #10346, #142531, #144673, #126331, #210686, #191228, #43950, #176078, #27676, #75368, #25537, #28751, #45020, #93771, #58044, #124209, #159811, #193375, #94835, #13553, #11415, #77490, #143609, #209602, #61246, #91645, #178210, #46084, #111130, #62315, #194442, #112203, #29826, #161963, #79625, #41826, #107939, #141480, #173964, #213860, #49274, #165142, #130593, #195519, #196582, #179277, #65480, #116447, #64448, #147842, #18868, #211745, #34068, #167283, #146795, #182441, #467, #83880, #67602, #51401, #100139, #17792, #16733, #212811, #131630, #82818, #31955, #148894, #163025, #145744, #197629, #15673, #48224, #149971, #114337, #115395, #180332, #14608, #199756, #1540, #98039, #166202, #164092, #181388, #33011, #133748, #101195, #35123, #81760, #117521, #99090, #66537, #132678, #198684, #183514, #50329, #63383, #129538, #47156, #113272, #30900, #96977, #80705, #153158, #134802, #125813, #54592, #87088, #4733, #190709, #120739 ) ),
 .UNSPECIFIED., .F., .F., .F. ) 
 B_SPLINE_SURFACE_WITH_KNOTS ( ( 2, 2 ),
 ( 3, 2, 2, 2, 2, 2, 2, 2, 2, 2, 2, 2, 2, 2, 2, 2, 2, 2, 2, 2, 2, 2, 2, 2, 2, 2, 2, 2, 2, 2, 2, 2, 2, 2, 2, 2, 2, 2, 2, 2, 2, 2, 2, 2, 2, 2, 2, 2, 2, 2, 2, 2, 2, 2, 2, 2, 2, 2, 2, 2, 2, 2, 2, 2, 2, 2, 2, 2, 2, 2, 2, 2, 2, 2, 2, 2, 2, 2, 2, 2, 2, 2, 2, 2, 2, 2, 2, 2, 2, 2, 2, 2, 2, 2, 2, 2, 2, 2, 2, 2, 2, 2, 2, 2, 2, 2, 2, 2, 2, 2, 2, 2, 2, 2, 2, 2, 2, 2, 2, 2, 3 ),
 ( 0.000000000000000000, 1.000000000000000000 ),
 ( 0.000000000000000000, 0.008333333333333333218, 0.01666666666666666644, 0.02500000000000000139, 0.03333333333333333287, 0.04166666666666666435, 0.05000000000000000278, 0.05833333333333333426, 0.06666666666666666574, 0.07499999999999999722, 0.08333333333333332871, 0.09166666666666666019, 0.1000000000000000056, 0.1083333333333333370, 0.1166666666666666685, 0.1250000000000000000, 0.1333333333333333315, 0.1416666666666666630, 0.1499999999999999944, 0.1583333333333333259, 0.1666666666666666574, 0.1749999999999999889, 0.1833333333333333204, 0.1916666666666666796, 0.2000000000000000111, 0.2083333333333333426, 0.2166666666666666741, 0.2250000000000000056, 0.2333333333333333370, 0.2416666666666666685, 0.2500000000000000000, 0.2583333333333333592, 0.2666666666666666630, 0.2750000000000000222, 0.2833333333333333259, 0.2916666666666666852, 0.2999999999999999889, 0.3083333333333333481, 0.3166666666666666519, 0.3250000000000000111, 0.3333333333333333148, 0.3416666666666666741, 0.3499999999999999778, 0.3583333333333333370, 0.3666666666666666408, 0.3750000000000000000, 0.3833333333333333592, 0.3916666666666666630, 0.4000000000000000222, 0.4083333333333333259, 0.4166666666666666852, 0.4249999999999999889, 0.4333333333333333481, 0.4416666666666666519, 0.4500000000000000111, 0.4583333333333333148, 0.4666666666666666741, 0.4749999999999999778, 0.4833333333333333370, 0.4916666666666666408, 0.5000000000000000000, 0.5083333333333333037, 0.5166666666666667185, 0.5250000000000000222, 0.5333333333333333259, 0.5416666666666666297, 0.5500000000000000444, 0.5583333333333333481, 0.5666666666666666519, 0.5749999999999999556, 0.5833333333333333703, 0.5916666666666666741, 0.5999999999999999778, 0.6083333333333332815, 0.6166666666666666963, 0.6250000000000000000, 0.6333333333333333037, 0.6416666666666667185, 0.6500000000000000222, 0.6583333333333333259, 0.6666666666666666297, 0.6750000000000000444, 0.6833333333333333481, 0.6916666666666666519, 0.6999999999999999556, 0.7083333333333333703, 0.7166666666666666741, 0.7249999999999999778, 0.7333333333333332815, 0.7416666666666666963, 0.7500000000000000000, 0.7583333333333333037, 0.7666666666666667185, 0.7750000000000000222, 0.7833333333333333259, 0.7916666666666666297, 0.8000000000000000444, 0.8083333333333333481, 0.8166666666666666519, 0.8249999999999999556, 0.8333333333333333703, 0.8416666666666666741, 0.8499999999999999778, 0.8583333333333332815, 0.8666666666666666963, 0.8750000000000000000, 0.8833333333333333037, 0.8916666666666667185, 0.9000000000000000222, 0.9083333333333333259, 0.9166666666666666297, 0.9250000000000000444, 0.9333333333333333481, 0.9416666666666666519, 0.9499999999999999556, 0.9583333333333333703, 0.9666666666666666741, 0.9749999999999999778, 0.9833333333333332815, 0.9916666666666666963, 1.000000000000000000 ),
 .UNSPECIFIED. ) 
 GEOMETRIC_REPRESENTATION_ITEM ( )  RATIONAL_B_SPLINE_SURFACE ( (
 ( 1.000000000000000000, 0.8660254037844387076, 1.000000000000000000, 0.8660254037844387076, 1.000000000000000000, 0.8660254037844387076, 1.000000000000000000, 0.8660254037844387076, 1.000000000000000000, 0.8660254037844387076, 1.000000000000000000, 0.8660254037844387076, 1.000000000000000000, 0.8660254037844387076, 1.000000000000000000, 0.8660254037844387076, 1.000000000000000000, 0.8660254037844387076, 1.000000000000000000, 0.8660254037844387076, 1.000000000000000000, 0.8660254037844387076, 1.000000000000000000, 0.8660254037844387076, 1.000000000000000000, 0.8660254037844387076, 1.000000000000000000, 0.8660254037844387076, 1.000000000000000000, 0.8660254037844387076, 1.000000000000000000, 0.8660254037844387076, 1.000000000000000000, 0.8660254037844387076, 1.000000000000000000, 0.8660254037844387076, 1.000000000000000000, 0.8660254037844387076, 1.000000000000000000, 0.8660254037844387076, 1.000000000000000000, 0.8660254037844387076, 1.000000000000000000, 0.8660254037844387076, 1.000000000000000000, 0.8660254037844387076, 1.000000000000000000, 0.8660254037844387076, 1.000000000000000000, 0.8660254037844387076, 1.000000000000000000, 0.8660254037844387076, 1.000000000000000000, 0.8660254037844387076, 1.000000000000000000, 0.8660254037844387076, 1.000000000000000000, 0.8660254037844387076, 1.000000000000000000, 0.8660254037844387076, 1.000000000000000000, 0.8660254037844387076, 1.000000000000000000, 0.8660254037844387076, 1.000000000000000000, 0.8660254037844387076, 1.000000000000000000, 0.8660254037844387076, 1.000000000000000000, 0.8660254037844387076, 1.000000000000000000, 0.8660254037844387076, 1.000000000000000000, 0.8660254037844387076, 1.000000000000000000, 0.8660254037844387076, 1.000000000000000000, 0.8660254037844387076, 1.000000000000000000, 0.8660254037844387076, 1.000000000000000000, 0.8660254037844387076, 1.000000000000000000, 0.8660254037844387076, 1.000000000000000000, 0.8660254037844387076, 1.000000000000000000, 0.8660254037844387076, 1.000000000000000000, 0.8660254037844387076, 1.000000000000000000, 0.8660254037844387076, 1.000000000000000000, 0.8660254037844387076, 1.000000000000000000, 0.8660254037844387076, 1.000000000000000000, 0.8660254037844387076, 1.000000000000000000, 0.8660254037844387076, 1.000000000000000000, 0.8660254037844387076, 1.000000000000000000, 0.8660254037844387076, 1.000000000000000000, 0.8660254037844387076, 1.000000000000000000, 0.8660254037844387076, 1.000000000000000000, 0.8660254037844387076, 1.000000000000000000, 0.8660254037844387076, 1.000000000000000000, 0.8660254037844387076, 1.000000000000000000, 0.8660254037844387076, 1.000000000000000000, 0.8660254037844387076, 1.000000000000000000, 0.8660254037844387076, 1.000000000000000000, 0.8660254037844387076, 1.000000000000000000, 0.8660254037844387076, 1.000000000000000000, 0.8660254037844387076, 1.000000000000000000, 0.8660254037844387076, 1.000000000000000000, 0.8660254037844387076, 1.000000000000000000, 0.8660254037844387076, 1.000000000000000000, 0.8660254037844387076, 1.000000000000000000, 0.8660254037844387076, 1.000000000000000000, 0.8660254037844387076, 1.000000000000000000, 0.8660254037844387076, 1.000000000000000000, 0.8660254037844387076, 1.000000000000000000, 0.8660254037844387076, 1.000000000000000000, 0.8660254037844387076, 1.000000000000000000, 0.8660254037844387076, 1.000000000000000000, 0.8660254037844387076, 1.000000000000000000, 0.8660254037844387076, 1.000000000000000000, 0.8660254037844387076, 1.000000000000000000, 0.8660254037844387076, 1.000000000000000000, 0.8660254037844387076, 1.000000000000000000, 0.8660254037844387076, 1.000000000000000000, 0.8660254037844387076, 1.000000000000000000, 0.8660254037844387076, 1.000000000000000000, 0.8660254037844387076, 1.000000000000000000, 0.8660254037844387076, 1.000000000000000000, 0.8660254037844387076, 1.000000000000000000, 0.8660254037844387076, 1.000000000000000000, 0.8660254037844387076, 1.000000000000000000, 0.8660254037844387076, 1.000000000000000000, 0.8660254037844387076, 1.000000000000000000, 0.8660254037844387076, 1.000000000000000000, 0.8660254037844387076, 1.000000000000000000, 0.8660254037844387076, 1.000000000000000000, 0.8660254037844387076, 1.000000000000000000, 0.8660254037844387076, 1.000000000000000000, 0.8660254037844387076, 1.000000000000000000, 0.8660254037844387076, 1.000000000000000000, 0.8660254037844387076, 1.000000000000000000, 0.8660254037844387076, 1.000000000000000000, 0.8660254037844387076, 1.000000000000000000, 0.8660254037844387076, 1.000000000000000000, 0.8660254037844387076, 1.000000000000000000, 0.8660254037844387076, 1.000000000000000000, 0.8660254037844387076, 1.000000000000000000, 0.8660254037844387076, 1.000000000000000000, 0.8660254037844387076, 1.000000000000000000, 0.8660254037844387076, 1.000000000000000000, 0.8660254037844387076, 1.000000000000000000, 0.8660254037844387076, 1.000000000000000000, 0.8660254037844387076, 1.000000000000000000, 0.8660254037844387076, 1.000000000000000000, 0.8660254037844387076, 1.000000000000000000, 0.8660254037844387076, 1.000000000000000000, 0.8660254037844387076, 1.000000000000000000, 0.8660254037844387076, 1.000000000000000000, 0.8660254037844387076, 1.000000000000000000, 0.8660254037844387076, 1.000000000000000000, 0.8660254037844387076, 1.000000000000000000, 0.8660254037844387076, 1.000000000000000000, 0.8660254037844387076, 1.000000000000000000, 0.8660254037844387076, 1.000000000000000000),
 ( 1.000000000000000000, 0.8660254037844387076, 1.000000000000000000, 0.8660254037844387076, 1.000000000000000000, 0.8660254037844387076, 1.000000000000000000, 0.8660254037844387076, 1.000000000000000000, 0.8660254037844387076, 1.000000000000000000, 0.8660254037844387076, 1.000000000000000000, 0.8660254037844387076, 1.000000000000000000, 0.8660254037844387076, 1.000000000000000000, 0.8660254037844387076, 1.000000000000000000, 0.8660254037844387076, 1.000000000000000000, 0.8660254037844387076, 1.000000000000000000, 0.8660254037844387076, 1.000000000000000000, 0.8660254037844387076, 1.000000000000000000, 0.8660254037844387076, 1.000000000000000000, 0.8660254037844387076, 1.000000000000000000, 0.8660254037844387076, 1.000000000000000000, 0.8660254037844387076, 1.000000000000000000, 0.8660254037844387076, 1.000000000000000000, 0.8660254037844387076, 1.000000000000000000, 0.8660254037844387076, 1.000000000000000000, 0.8660254037844387076, 1.000000000000000000, 0.8660254037844387076, 1.000000000000000000, 0.8660254037844387076, 1.000000000000000000, 0.8660254037844387076, 1.000000000000000000, 0.8660254037844387076, 1.000000000000000000, 0.8660254037844387076, 1.000000000000000000, 0.8660254037844387076, 1.000000000000000000, 0.8660254037844387076, 1.000000000000000000, 0.8660254037844387076, 1.000000000000000000, 0.8660254037844387076, 1.000000000000000000, 0.8660254037844387076, 1.000000000000000000, 0.8660254037844387076, 1.000000000000000000, 0.8660254037844387076, 1.000000000000000000, 0.8660254037844387076, 1.000000000000000000, 0.8660254037844387076, 1.000000000000000000, 0.8660254037844387076, 1.000000000000000000, 0.8660254037844387076, 1.000000000000000000, 0.8660254037844387076, 1.000000000000000000, 0.8660254037844387076, 1.000000000000000000, 0.8660254037844387076, 1.000000000000000000, 0.8660254037844387076, 1.000000000000000000, 0.8660254037844387076, 1.000000000000000000, 0.8660254037844387076, 1.000000000000000000, 0.8660254037844387076, 1.000000000000000000, 0.8660254037844387076, 1.000000000000000000, 0.8660254037844387076, 1.000000000000000000, 0.8660254037844387076, 1.000000000000000000, 0.8660254037844387076, 1.000000000000000000, 0.8660254037844387076, 1.000000000000000000, 0.8660254037844387076, 1.000000000000000000, 0.8660254037844387076, 1.000000000000000000, 0.8660254037844387076, 1.000000000000000000, 0.8660254037844387076, 1.000000000000000000, 0.8660254037844387076, 1.000000000000000000, 0.8660254037844387076, 1.000000000000000000, 0.8660254037844387076, 1.000000000000000000, 0.8660254037844387076, 1.000000000000000000, 0.8660254037844387076, 1.000000000000000000, 0.8660254037844387076, 1.000000000000000000, 0.8660254037844387076, 1.000000000000000000, 0.8660254037844387076, 1.000000000000000000, 0.8660254037844387076, 1.000000000000000000, 0.8660254037844387076, 1.000000000000000000, 0.8660254037844387076, 1.000000000000000000, 0.8660254037844387076, 1.000000000000000000, 0.8660254037844387076, 1.000000000000000000, 0.8660254037844387076, 1.000000000000000000, 0.8660254037844387076, 1.000000000000000000, 0.8660254037844387076, 1.000000000000000000, 0.8660254037844387076, 1.000000000000000000, 0.8660254037844387076, 1.000000000000000000, 0.8660254037844387076, 1.000000000000000000, 0.8660254037844387076, 1.000000000000000000, 0.8660254037844387076, 1.000000000000000000, 0.8660254037844387076, 1.000000000000000000, 0.8660254037844387076, 1.000000000000000000, 0.8660254037844387076, 1.000000000000000000, 0.8660254037844387076, 1.000000000000000000, 0.8660254037844387076, 1.000000000000000000, 0.8660254037844387076, 1.000000000000000000, 0.8660254037844387076, 1.000000000000000000, 0.8660254037844387076, 1.000000000000000000, 0.8660254037844387076, 1.000000000000000000, 0.8660254037844387076, 1.000000000000000000, 0.8660254037844387076, 1.000000000000000000, 0.8660254037844387076, 1.000000000000000000, 0.8660254037844387076, 1.000000000000000000, 0.8660254037844387076, 1.000000000000000000, 0.8660254037844387076, 1.000000000000000000, 0.8660254037844387076, 1.000000000000000000, 0.8660254037844387076, 1.000000000000000000, 0.8660254037844387076, 1.000000000000000000, 0.8660254037844387076, 1.000000000000000000, 0.8660254037844387076, 1.000000000000000000, 0.8660254037844387076, 1.000000000000000000, 0.8660254037844387076, 1.000000000000000000, 0.8660254037844387076, 1.000000000000000000, 0.8660254037844387076, 1.000000000000000000, 0.8660254037844387076, 1.000000000000000000, 0.8660254037844387076, 1.000000000000000000, 0.8660254037844387076, 1.000000000000000000, 0.8660254037844387076, 1.000000000000000000, 0.8660254037844387076, 1.000000000000000000, 0.8660254037844387076, 1.000000000000000000, 0.8660254037844387076, 1.000000000000000000, 0.8660254037844387076, 1.000000000000000000, 0.8660254037844387076, 1.000000000000000000, 0.8660254037844387076, 1.000000000000000000, 0.8660254037844387076, 1.000000000000000000, 0.8660254037844387076, 1.000000000000000000, 0.8660254037844387076, 1.000000000000000000, 0.8660254037844387076, 1.000000000000000000, 0.8660254037844387076, 1.000000000000000000, 0.8660254037844387076, 1.000000000000000000, 0.8660254037844387076, 1.000000000000000000, 0.8660254037844387076, 1.000000000000000000, 0.8660254037844387076, 1.000000000000000000, 0.8660254037844387076, 1.000000000000000000, 0.8660254037844387076, 1.000000000000000000, 0.8660254037844387076, 1.000000000000000000) ) ) 
 REPRESENTATION_ITEM ( '' )  SURFACE ( )  );
#111289 = CARTESIAN_POINT ( 'NONE',  ( -5.565401824202027115, 6.214873266482019432, 0.9197014482419992865 ) ) ;
#111291 = CARTESIAN_POINT ( 'NONE',  ( 2.822068529938852155, 6.444163718237301275, -0.7998128361456291469 ) ) ;
#111292 = CARTESIAN_POINT ( 'NONE',  ( -5.506019780925599960, 5.596313630600862510, 0.7216878364870257245 ) ) ;
#111294 = ORIENTED_EDGE ( 'NONE', *, *, #200849, .T. ) ;
#111293 = CARTESIAN_POINT ( 'NONE',  ( -6.399085315970137522, 9.449054721065074602, -1.082531754730538864 ) ) ;
#111295 = TOROIDAL_SURFACE ( 'NONE', #17797, 10.75000000000000000, 0.5000000000000007772 ) ;
#111296 = CARTESIAN_POINT ( 'NONE',  ( 3.639029512587122372, 2.014767915268770082, 0.6618469929612482705 ) ) ;
#111297 = CARTESIAN_POINT ( 'NONE',  ( -5.123001941117347080, 7.070197912760590064, 1.599625672291263179 ) ) ;
#111298 = CARTESIAN_POINT ( 'NONE',  ( 4.768538688506021472, -1.414568798902924307, 1.634688457493836289 ) ) ;
#111299 = CARTESIAN_POINT ( 'NONE',  ( 3.825598141381767903, 0.9817388958630569595, -1.557492293685861284 ) ) ;
#111300 = CIRCLE ( 'NONE', #100857, 11.92000000000000171 ) ;
#111301 = CARTESIAN_POINT ( 'NONE',  ( -4.566676325625886435, 6.985790553628898003, 1.179912429979562249 ) ) ;
#111302 = CARTESIAN_POINT ( 'NONE',  ( -1.402160292154681736E-14, -0.4906249996585810846, -1.575800808251665908 ) ) ;
#111303 = CARTESIAN_POINT ( 'NONE',  ( 5.806559702419027857, 1.537982464610265332, 0.8144831216923865691 ) ) ;
#111304 = CARTESIAN_POINT ( 'NONE',  ( 1.278248824818062671E-15, 1.062499999999996003, 1.224999999999968781 ) ) ;
#111305 = CARTESIAN_POINT ( 'NONE',  ( 3.389175213736285386, 6.897862149426897460, 0.7216878364870317197 ) ) ;
#111306 = CARTESIAN_POINT ( 'NONE',  ( -0.4359507092143430351, -8.863025497813993070, 9.827344407697081508 ) ) ;
#111307 = CARTESIAN_POINT ( 'NONE',  ( 3.432649856329002880, 2.108609624295390006, 0.4754391814798044069 ) ) ;
#111308 = CARTESIAN_POINT ( 'NONE',  ( 5.483749906247235906, 1.861732415968733401, 0.7741956105717237024 ) ) ;
#111309 = CARTESIAN_POINT ( 'NONE',  ( -9.449669878600625239, 10.12696240122997082, -0.7216878364870267237 ) ) ;
#111310 = CARTESIAN_POINT ( 'NONE',  ( 2.518638242371186386, 1.412657066830936392, -1.636333507658905173 ) ) ;
#111311 = CARTESIAN_POINT ( 'NONE',  ( 3.233620971007169942, -1.321289716990686980, -1.463211747571713461 ) ) ;
#111312 = CARTESIAN_POINT ( 'NONE',  ( 0.2225716830646235489, 2.098996182288978218, 0.6302611576235671587 ) ) ;
#111313 = CARTESIAN_POINT ( 'NONE',  ( 4.792492878049551486, 1.612589784423448025, -1.081918670939057137 ) ) ;
#111316 = ORIENTED_EDGE ( 'NONE', *, *, #104333, .T. ) ;
#111315 = DIRECTION ( 'NONE',  ( -0.01538971728768316095, 0.9998815712882226370, 0.000000000000000000 ) ) ;
#111314 = CARTESIAN_POINT ( 'NONE',  ( -9.341204649691320583, 10.96078884847042545, 1.082531754730558626 ) ) ;
#111317 = CARTESIAN_POINT ( 'NONE',  ( -7.117104292530948229, 7.267986194233038155, -0.7998128361456362523 ) ) ;
#111318 = CARTESIAN_POINT ( 'NONE',  ( 11.86239285000045740, 9.719999999999982876, 1.812080536912751283 ) ) ;
#111320 = ORIENTED_EDGE ( 'NONE', *, *, #137088, .F. ) ;
#111319 = CARTESIAN_POINT ( 'NONE',  ( -5.652823702255029836, 5.559658838911111900, -0.7998128361456362523 ) ) ;
#111321 = CARTESIAN_POINT ( 'NONE',  ( -7.321039761255057066, 11.48503745486550365, 0.000000000000000000 ) ) ;
#111322 = CARTESIAN_POINT ( 'NONE',  ( 2.221956617217385244, -2.140583525707707935, 0.5359638216213060691 ) ) ;
#111324 = ADVANCED_FACE ( 'NONE', ( #151662 ), #44309, .T. ) ;
#111323 = CARTESIAN_POINT ( 'NONE',  ( 3.285556943750000514, -1.713541666188707735, 1.896917185911906500 ) ) ;
#111325 = CARTESIAN_POINT ( 'NONE',  ( 6.385602409055195494, -1.848352663145738095, 0.6577735930803210174 ) ) ;
#111326 = CARTESIAN_POINT ( 'NONE',  ( -1.201851678989727383E-14, 5.509375000341415252, -1.575800808251660134 ) ) ;
#111327 = CARTESIAN_POINT ( 'NONE',  ( -1.201851678989727383E-14, 3.993750000682817713, 1.732050807568877637 ) ) ;
#111328 = CARTESIAN_POINT ( 'NONE',  ( 6.062205217752669739, 6.048677139763619870, -0.4177986087803304271 ) ) ;
#111329 = CARTESIAN_POINT ( 'NONE',  ( 0.07479286986305369589, 0.2526433113205875935, -1.890777245541554574 ) ) ;
#111330 = CARTESIAN_POINT ( 'NONE',  ( 4.857273802806507668, 1.820629801081237620, -0.2732171615176108848 ) ) ;
#111331 = ORIENTED_EDGE ( 'NONE', *, *, #99953, .T. ) ;
#111332 = CARTESIAN_POINT ( 'NONE',  ( 0.6124999999999793943, 2.479166667349472331, -1.060881119635965764 ) ) ;
#111333 = CARTESIAN_POINT ( 'NONE',  ( -8.505042434474312074, 8.816971016508505343, -0.7998128361456291469 ) ) ;
#111334 = CARTESIAN_POINT ( 'NONE',  ( 0.000000000000000000, 3.481540744127370690, 0.000000000000000000 ) ) ;
#111335 = CARTESIAN_POINT ( 'NONE',  ( 5.801066647469003357, -0.3129311994157328303, -2.097281602037828208 ) ) ;
#111336 = CARTESIAN_POINT ( 'NONE',  ( 9.287126810668082655, 11.47221324207556137, -7.528596418336154450 ) ) ;
#111337 = CARTESIAN_POINT ( 'NONE',  ( 5.009901455449552010, 5.803638771901306725, -1.199719254218452047 ) ) ;
#111338 = CARTESIAN_POINT ( 'NONE',  ( 6.081337768261708909, 1.905808788339557802, -0.7845383490599889820 ) ) ;
#111341 = CARTESIAN_POINT ( 'NONE',  ( 3.227900028218867234, 1.797025815167479390, 0.4004103908350764573 ) ) ;
#111340 = CARTESIAN_POINT ( 'NONE',  ( 1.820531350174507512, -1.319122485308525716, 1.313071031887176998 ) ) ;
#111339 = CARTESIAN_POINT ( 'NONE',  ( -10.25773349932952527, -6.796015482748905434, -2.597247770456278818E-17 ) ) ;
#111342 = CARTESIAN_POINT ( 'NONE',  ( 8.718056468787178659, 10.12981962079525289, 1.199719254218462483 ) ) ;
#111343 = CARTESIAN_POINT ( 'NONE',  ( -4.911970600500787043, 4.733485073844196478, 0.4366108110982139801 ) ) ;
#111344 = CARTESIAN_POINT ( 'NONE',  ( -5.094831863685302942, 9.165997284266655498, 0.7998128361456291469 ) ) ;
#111346 = VERTEX_POINT ( 'NONE', #11778 ) ;
#111345 = FACE_OUTER_BOUND ( 'NONE', #159573, .T. ) ;
#111347 = CARTESIAN_POINT ( 'NONE',  ( 3.879664727460280904, 2.078262106501146622, -0.7427522710690689367 ) ) ;
#111348 = CARTESIAN_POINT ( 'NONE',  ( 5.554102117330329769, 2.260170762534471578, -0.1031424389980051676 ) ) ;
#111349 = CARTESIAN_POINT ( 'NONE',  ( -6.344852701515500293, 9.385783337534627790, 1.082531754730548412 ) ) ;
#111350 = CARTESIAN_POINT ( 'NONE',  ( 5.590068458682615038, 1.086043493620889144, 1.449778898616445488 ) ) ;
#111351 = CARTESIAN_POINT ( 'NONE',  ( 6.280494692369203769, -0.5183099952858164494, -1.844178102243919870 ) ) ;
#111352 = CARTESIAN_POINT ( 'NONE',  ( 4.365362273920243119, 6.116008624372161862, 1.443375672974062551 ) ) ;
#111353 = CARTESIAN_POINT ( 'NONE',  ( 5.647288160985431738, -1.475499438119257878, -1.149758287351684949 ) ) ;
#111354 = CARTESIAN_POINT ( 'NONE',  ( 6.059226159983991167, -1.612925389857391645, 1.026989893868179404 ) ) ;
#111355 = CARTESIAN_POINT ( 'NONE',  ( -5.786256696412555911, 6.075953140482280190, 0.5845640519336701146 ) ) ;
#111356 = MECHANICAL_DESIGN_GEOMETRIC_PRESENTATION_REPRESENTATION (  '', ( #31820 ), #194305 ) ;
#111357 = CARTESIAN_POINT ( 'NONE',  ( 0.5318453760667535279, 0.9654296485097979552, -1.602142582367314549 ) ) ;
#111358 = CARTESIAN_POINT ( 'NONE',  ( 1.217982839071569012, 0.9896824804975331569, -1.756856037137774162 ) ) ;
#111360 = CARTESIAN_POINT ( 'NONE',  ( 3.791714260247856849, 1.525338472785308097, 1.452445685796518227 ) ) ;
#111359 = CARTESIAN_POINT ( 'NONE',  ( -9.154780037725563702, 11.70366268214508487, 1.599625672291281386 ) ) ;
#111361 = CARTESIAN_POINT ( 'NONE',  ( 8.934986926605834157, 10.38290515491702770, -1.199719254218446718 ) ) ;
#111363 = CARTESIAN_POINT ( 'NONE',  ( -10.01677656239806247, 10.58066083241955901, 0.7998128361456462443 ) ) ;
#111362 = CARTESIAN_POINT ( 'NONE',  ( 1.499999999999985123, 0.04583333333335545129, -0.8660254037844323793 ) ) ;
#111364 = CARTESIAN_POINT ( 'NONE',  ( 11.55950211276791251, 9.799999999999982947, 3.221476510067111665 ) ) ;
#111366 = EDGE_CURVE ( 'NONE', #17507, #54631, #58702, .T. ) ;
#111365 = CARTESIAN_POINT ( 'NONE',  ( 3.076430314242516229, 0.9118049750012310328, 1.802366903320629765 ) ) ;
#111367 = CARTESIAN_POINT ( 'NONE',  ( 1.364683531249988535, 3.363541667008084879, 0.7879004041258500513 ) ) ;
#111368 = CARTESIAN_POINT ( 'NONE',  ( 3.871016551901614200, 4.474939717762034697, -1.199719254218446718 ) ) ;
#111369 = CARTESIAN_POINT ( 'NONE',  ( 3.233815116076131257, -1.449111151313630996, -1.604113057997895053 ) ) ;
#111370 = CARTESIAN_POINT ( 'NONE',  ( 5.840530312436913007, 10.03597880781023299, 0.000000000000000000 ) ) ;
#111371 = CARTESIAN_POINT ( 'NONE',  ( 0.7499999999999902300, 4.566666666666691299, -1.299038105676658228 ) ) ;
#111373 = DIRECTION ( 'NONE',  ( 1.000000000000000000, -0.000000000000000000, -0.000000000000000000 ) ) ;
#111372 = CARTESIAN_POINT ( 'NONE',  ( 5.332099551924443404, 9.442809587212341427, 0.000000000000000000 ) ) ;
#111374 = CARTESIAN_POINT ( 'NONE',  ( 7.415946836550703303, 11.59576237604377091, 0.7216878364870438212 ) ) ;
#111376 = CARTESIAN_POINT ( 'NONE',  ( 8.349821703134351125, 15.09698064520563676, -8.558241530613692305 ) ) ;
#111375 = CARTESIAN_POINT ( 'NONE',  ( 1.205810543264747681, -1.711434635494583967, -1.335908126413299923 ) ) ;
#111377 = CARTESIAN_POINT ( 'NONE',  ( -5.233084105194862445, 9.049089189461916760, 0.7216878364870458196 ) ) ;
#111378 = EDGE_CURVE ( 'NONE', #127447, #6715, #28046, .T. ) ;
#111379 = CARTESIAN_POINT ( 'NONE',  ( 0.6823417656249899377, 1.092708333674752286, 1.181850606188755259 ) ) ;
#111380 = CARTESIAN_POINT ( 'NONE',  ( 1.822082775007987543, 1.258534617508931586, -1.793986466278547853 ) ) ;
#111381 = CARTESIAN_POINT ( 'NONE',  ( 6.883263157960391787, 1.253787318140922480, 2.167784446185747171 ) ) ;
#111382 = CARTESIAN_POINT ( 'NONE',  ( 2.044175283654376951, 0.8654258166664110519, -2.090645895884978955 ) ) ;
#111383 = CARTESIAN_POINT ( 'NONE',  ( -6.018930129462987999, 9.109503353427070849, 1.199719254218452047 ) ) ;
#111384 = CARTESIAN_POINT ( 'NONE',  ( -2.887523529586332405, 5.352232636950553513, 1.082531754730560403 ) ) ;
#111385 = CARTESIAN_POINT ( 'NONE',  ( -1.364683531250010295, 4.842708333674756283, 0.7879004041258379498 ) ) ;
#111386 = CARTESIAN_POINT ( 'NONE',  ( 5.220047253295719614, 7.706380104734268599, 1.202949228536150938 ) ) ;
#111387 = AXIS2_PLACEMENT_3D ( 'NONE', #164308, #99315, #84112 ) ;
#111388 = CARTESIAN_POINT ( 'NONE',  ( -1.500000000000001110, 11.77083333333333570, 0.8660254037844419273 ) ) ;
#111389 = CARTESIAN_POINT ( 'NONE',  ( 6.699137298928145690, 8.909022496873262753, 1.443375672974065660 ) ) ;
#111390 = CARTESIAN_POINT ( 'NONE',  ( 4.358513420383302694, -1.312205524322278549, 1.187683162289454142 ) ) ;
#111391 = CARTESIAN_POINT ( 'NONE',  ( 9.420217803396747414, 9.884675613584706255, 0.7998128361456462443 ) ) ;
#111392 = CARTESIAN_POINT ( 'NONE',  ( 0.7453164640696362531, -1.806240154289909139, 1.082582905463305378 ) ) ;
#111393 = CARTESIAN_POINT ( 'NONE',  ( -1.364683531250010295, 8.630208333674731946, 0.7879004041258445001 ) ) ;
#111394 = CARTESIAN_POINT ( 'NONE',  ( -5.635349125135588721, 6.603604063193491136, 1.199719254218452935 ) ) ;
#111395 = CARTESIAN_POINT ( 'NONE',  ( 6.116814581292481456, 0.2004514801264325186, 2.006445662566976651 ) ) ;
#111396 = VERTEX_POINT ( 'NONE', #42185 ) ;
#111397 = CARTESIAN_POINT ( 'NONE',  ( 10.58621901417202515, 11.24501035948919991, -0.7998128361456281477 ) ) ;
#111398 = CARTESIAN_POINT ( 'NONE',  ( 3.291731440620565330, -0.7593194595177065187, 1.709801165022284408 ) ) ;
#111399 = CARTESIAN_POINT ( 'NONE',  ( 3.696198088285786998, 0.9351842759567146057, -1.847102243037239910 ) ) ;
#111400 = EDGE_CURVE ( 'NONE', #117810, #11760, #170482, .T. ) ;
#111401 = CARTESIAN_POINT ( 'NONE',  ( -4.773879485343255347, 8.583626809626847987, 0.000000000000000000 ) ) ;
#111402 =( NAMED_UNIT ( * ) SI_UNIT ( $, .STERADIAN. ) SOLID_ANGLE_UNIT ( ) );
#111403 = CARTESIAN_POINT ( 'NONE',  ( 9.237182729612253951, 9.671134694169463586, 0.7998128361456462443 ) ) ;
#111404 = CARTESIAN_POINT ( 'NONE',  ( -8.143643823302737061, 12.65266822716189843, 0.000000000000000000 ) ) ;
#111405 = CARTESIAN_POINT ( 'NONE',  ( 6.192270064542984898, -2.150811787302907785, -0.2168040374768212541 ) ) ;
#111406 = CARTESIAN_POINT ( 'NONE',  ( -1.364683531249997417, 5.071875000341417916, 1.214306433183764966E-14 ) ) ;
#111407 = CARTESIAN_POINT ( 'NONE',  ( 3.473055881322492322, 1.772541284497713976, 0.8411618914155660764 ) ) ;
#111408 = CARTESIAN_POINT ( 'NONE',  ( 0.4739822347885510601, 1.752760637641921360, 0.9961516927870716076 ) ) ;
#111409 = CARTESIAN_POINT ( 'NONE',  ( -3.983199035293045309, 7.838694717720641414, 0.2268021594909743477 ) ) ;
#111411 = CARTESIAN_POINT ( 'NONE',  ( -2.279984679289828176, 5.601133616484927025, -0.06592222766762731445 ) ) ;
#111410 = CARTESIAN_POINT ( 'NONE',  ( 6.611572464958476836, 10.86525164242692298, 0.7998128361456462443 ) ) ;
#111412 = CARTESIAN_POINT ( 'NONE',  ( 0.7724589312842686795, -1.759198622581410021, -0.6360808729843556719 ) ) ;
#111413 = CARTESIAN_POINT ( 'NONE',  ( 0.6823417656249917140, 3.342708333674754506, 1.181850606188765695 ) ) ;
#111414 = CARTESIAN_POINT ( 'NONE',  ( 3.058842833410029272, 0.4931317667464900634, 1.951740033431844434 ) ) ;
#111416 = CARTESIAN_POINT ( 'NONE',  ( 1.827892122045454260, 0.8069190765337170834, -1.957623834376254646 ) ) ;
#111415 = CARTESIAN_POINT ( 'NONE',  ( -6.399085315970142851, 8.488685506763726352, -1.443375672974059665 ) ) ;
#111417 = CARTESIAN_POINT ( 'NONE',  ( 10.36376191611410746, 9.171481364675830861, -6.003992305501989257 ) ) ;
#111418 = CARTESIAN_POINT ( 'NONE',  ( 3.930184216435282707, 1.147649575447948100, 1.722966636330313550 ) ) ;
#111419 = CARTESIAN_POINT ( 'NONE',  ( 6.912678218121202534, 9.158153569265168770, 1.599625672291268286 ) ) ;
#111421 = CARTESIAN_POINT ( 'NONE',  ( 2.381428537494710618, 5.930083727052461562, 0.7998128361456462443 ) ) ;
#111420 = CARTESIAN_POINT ( 'NONE',  ( 0.5036076356924833464, -2.080315145378656805, 0.2087293992604210557 ) ) ;
#111423 = ORIENTED_EDGE ( 'NONE', *, *, #132407, .T. ) ;
#111422 = CARTESIAN_POINT ( 'NONE',  ( 5.877927443470423619, 1.089437568142386015, 1.464738158297604453 ) ) ;
#111424 = CARTESIAN_POINT ( 'NONE',  ( 7.391166297744269365, 11.77477778067701664, 1.040834085586084257E-14 ) ) ;
#111425 = CARTESIAN_POINT ( 'NONE',  ( 7.720982897393571243, -6.134628647623485698, -7.834948825496923952 ) ) ;
#111426 = CARTESIAN_POINT ( 'NONE',  ( 11.86512089291903749, 8.353562777165519648, -1.599672920186862912 ) ) ;
#111427 = CARTESIAN_POINT ( 'NONE',  ( 5.948300505803369553, 2.203960110721484789, 0.1139900122707343255 ) ) ;
#111428 = CARTESIAN_POINT ( 'NONE',  ( -0.6823417656250039265, 12.63020833367473017, -1.181850606188755259 ) ) ;
#111429 = CARTESIAN_POINT ( 'NONE',  ( 4.793567869993575314, 1.782951692925707654, -0.6917526515820491273 ) ) ;
#111430 = CARTESIAN_POINT ( 'NONE',  ( -8.622095623286845978, 12.14652976288826913, 1.199719254218462483 ) ) ;
#111431 = PRESENTATION_LAYER_ASSIGNMENT (  '', '', ( #146024 ) ) ;
#111432 = CARTESIAN_POINT ( 'NONE',  ( 7.644099680006512187, 7.812537802962739697, 1.040834085586084257E-14 ) ) ;
#111433 = CIRCLE ( 'NONE', #42127, 11.99999999999999112 ) ;
#111434 = CARTESIAN_POINT ( 'NONE',  ( -11.91826848676326200, 11.00833707238759374, -1.400000051401919077 ) ) ;
#111435 = CARTESIAN_POINT ( 'NONE',  ( 4.975479186090860928, 4.907073259968533385, 0.7216878364870317197 ) ) ;
#111436 = DIRECTION ( 'NONE',  ( 1.000000000000000000, -0.000000000000000000, -0.000000000000000000 ) ) ;
#111437 = CARTESIAN_POINT ( 'NONE',  ( 5.657830175604453338, 5.495223381160312393, 0.7998128361456341429 ) ) ;
#111438 = ORIENTED_EDGE ( 'NONE', *, *, #173816, .F. ) ;
#111439 = CARTESIAN_POINT ( 'NONE',  ( -7.910256278930404505, 8.193330178365746619, -0.7998128361456362523 ) ) ;
#111440 = CARTESIAN_POINT ( 'NONE',  ( 4.358574879328508622, -1.387578095181252413, 1.254630796652965730 ) ) ;
#111441 = CARTESIAN_POINT ( 'NONE',  ( -3.752568318859959007, 7.355240624044412812, 0.6449737300090957470 ) ) ;
#111442 = CARTESIAN_POINT ( 'NONE',  ( 5.397027666691686321, 8.454226823519094935, 1.199719254218451159 ) ) ;
#111443 = CARTESIAN_POINT ( 'NONE',  ( 1.772826578343088544, 3.950000000000001954, -0.4500000000000284883 ) ) ;
#111444 = CARTESIAN_POINT ( 'NONE',  ( -5.258916259484140099, 7.686978671390940043, 1.214082833407425621 ) ) ;
#111445 = CARTESIAN_POINT ( 'NONE',  ( -5.246642258808529746, 9.064907035344523578, 0.000000000000000000 ) ) ;
#111446 = CARTESIAN_POINT ( 'NONE',  ( 3.765413976293345844, 5.416068943807445635, 1.599625672291267398 ) ) ;
#111447 = CARTESIAN_POINT ( 'NONE',  ( 2.324999910687207461, -1.798643183423669134, -0.8027048682860711271 ) ) ;
#111448 = CARTESIAN_POINT ( 'NONE',  ( 3.374625213368151133, -0.3961236654455925765, -1.976952669325626299 ) ) ;
#111449 = CARTESIAN_POINT ( 'NONE',  ( -6.398558430645608475, 9.552403038140164782, -1.199719254218440723 ) ) ;
#111450 = CARTESIAN_POINT ( 'NONE',  ( 4.179656494762836516, 8.098292687190454586, -0.7998128361456362523 ) ) ;
#111451 = CARTESIAN_POINT ( 'NONE',  ( 6.827182134110194589, 2.412578537245218424, 2.569476350730160785 ) ) ;
#111452 = B_SPLINE_CURVE_WITH_KNOTS ( 'NONE', 3,
 ( #184523, #17743, #18820, #101145, #52414, #183468 ),
 .UNSPECIFIED., .F., .F.,
 ( 4, 2, 4 ),
 ( 0.0006378314054480060599, 0.0009584618939205532184, 0.001279092382393100377 ),
 .UNSPECIFIED. ) ;
#111453 = CARTESIAN_POINT ( 'NONE',  ( 3.697391623616069101, -0.6365095100077067247, 2.096977347260075231 ) ) ;
#111454 = CARTESIAN_POINT ( 'NONE',  ( 1.734723475976807094E-15, 2.499999999999998668, 0.000000000000000000 ) ) ;
#111455 = CARTESIAN_POINT ( 'NONE',  ( 2.010648722831087198, 1.429088002864507212, -1.291968487218410511 ) ) ;
#111456 = CARTESIAN_POINT ( 'NONE',  ( -10.30827686509187835, 10.92074451889568643, 1.040834085586084257E-14 ) ) ;
#111457 = CARTESIAN_POINT ( 'NONE',  ( 0.2333540202161506205, 0.2466631755442013352, -2.080888922837381916 ) ) ;
#111458 = CARTESIAN_POINT ( 'NONE',  ( 3.933273961740298752, 5.682181936820735579, 1.443375672974058777 ) ) ;
#111459 = CARTESIAN_POINT ( 'NONE',  ( 8.281332899848809603, 8.555976559445431562, 0.7998128361456481317 ) ) ;
#111460 =( BOUNDED_SURFACE ( )  B_SPLINE_SURFACE ( 3, 2, ( 
 ( #4774, #70852, #136966 ),
 ( #24245, #122938, #90346 ),
 ( #39450, #139102, #140186 ),
 ( #188895, #206207, #91430 ),
 ( #57835, #10143, #126123 ),
 ( #173753, #174819, #23175 ),
 ( #205129, #207280, #142327 ),
 ( #27466, #89289, #171580 ) ),
 .UNSPECIFIED., .F., .F., .T. ) 
 B_SPLINE_SURFACE_WITH_KNOTS ( ( 4, 2, 2, 4 ),
 ( 3, 3 ),
 ( 0.000000000000000000, 0.0004924884914732709533, 0.0007387327372099063757, 0.0009849769829465419065 ),
 ( 0.000000000000000000, 1.000000000000000000 ),
 .UNSPECIFIED. ) 
 GEOMETRIC_REPRESENTATION_ITEM ( )  RATIONAL_B_SPLINE_SURFACE ( (
 ( 1.000000000000000000, 0.7045118851637552915, 1.000000000000000000),
 ( 1.000000000000000000, 0.7593505504065475309, 1.000000000000000000),
 ( 1.000000000000000000, 0.8104906253031783914, 1.000000000000000000),
 ( 1.000000000000000000, 0.8722646935501797705, 1.000000000000000000),
 ( 1.000000000000000000, 0.8905178607894786991, 1.000000000000000000),
 ( 1.000000000000000000, 0.9170530604353607229, 1.000000000000000000),
 ( 1.000000000000000000, 0.9248184710077410609, 1.000000000000000000),
 ( 1.000000000000000000, 0.9238795325112870716, 1.000000000000000000) ) ) 
 REPRESENTATION_ITEM ( '' )  SURFACE ( )  );
#111461 = CARTESIAN_POINT ( 'NONE',  ( 2.758194185376297902, 5.305311418659259814, 1.199719254218452047 ) ) ;
#111462 = CARTESIAN_POINT ( 'NONE',  ( 5.072158865288233898, 7.971250205261355859, 1.082531754730549078 ) ) ;
#111463 = ORIENTED_EDGE ( 'NONE', *, *, #25018, .F. ) ;
#111465 = CARTESIAN_POINT ( 'NONE',  ( 1.506495127224609876, -2.003582159550582276, -0.1952931609562995052 ) ) ;
#111464 = CARTESIAN_POINT ( 'NONE',  ( 4.704558828624370470, 1.604442792107749760, 0.9031527321438773681 ) ) ;
#111466 = CARTESIAN_POINT ( 'NONE',  ( 3.849189735728062001, -1.136876111170448178, 1.997481460179703960 ) ) ;
#111468 = CARTESIAN_POINT ( 'NONE',  ( 2.377597188713850507, -1.806433865756534640, 0.4466691629738496760 ) ) ;
#111467 = CARTESIAN_POINT ( 'NONE',  ( -0.1290005225502398323, 0.2247172878383028038, -2.207197350255707402 ) ) ;
#111469 = CARTESIAN_POINT ( 'NONE',  ( -3.285556943749998737, -1.480208332855375453, 1.896917185911908499 ) ) ;
#111470 = DIRECTION ( 'NONE',  ( 0.000000000000000000, 0.000000000000000000, -1.000000000000000000 ) ) ;
#111471 = CARTESIAN_POINT ( 'NONE',  ( 5.554919272666569263, 0.3793472168572444292, 1.874222000232607765 ) ) ;
#111472 = CARTESIAN_POINT ( 'NONE',  ( -7.751511138711140170, 10.06651563329490529, -1.599625672291263179 ) ) ;
#111473 = CARTESIAN_POINT ( 'NONE',  ( -5.478903473698260029, 6.525047153136981137, -1.082531754730549967 ) ) ;
#111475 = CARTESIAN_POINT ( 'NONE',  ( 3.063207453921251489, 0.2760179531714930246, -1.850060308400132358 ) ) ;
#111474 = CARTESIAN_POINT ( 'NONE',  ( 4.774988821994140764, 1.950233014344885385, -0.7539837885136254636 ) ) ;
#111476 = CARTESIAN_POINT ( 'NONE',  ( 7.144783764721768904, 7.437928601704619780, 1.040834085586084257E-14 ) ) ;
#111477 = CARTESIAN_POINT ( 'NONE',  ( -4.690757960648240577, 6.495636925554817864, 1.443375672974064550 ) ) ;
#111478 = CARTESIAN_POINT ( 'NONE',  ( 5.602095939246814815, -1.725068444894608310, 0.006287883723511687381 ) ) ;
#111479 = CARTESIAN_POINT ( 'NONE',  ( -6.087774667736030487, 7.061157519568837415, 1.199719254218450271 ) ) ;
#111480 = CARTESIAN_POINT ( 'NONE',  ( 1.037308000539336694, -1.367553460919969543, 1.066146521862390673 ) ) ;
#111481 =( LENGTH_UNIT ( ) NAMED_UNIT ( * ) SI_UNIT ( .MILLI., .METRE. ) );
#111482 = CARTESIAN_POINT ( 'NONE',  ( -1.499999999999997558, 7.809273069926255140, -3.635729725621148489 ) ) ;
#111483 = DIRECTION ( 'NONE',  ( -1.000000000000000000, 0.000000000000000000, 0.000000000000000000 ) ) ;
#111484 = CARTESIAN_POINT ( 'NONE',  ( 5.752828983992735346, -0.5200050086436918129, -2.107789999013423454 ) ) ;
#111485 = CARTESIAN_POINT ( 'NONE',  ( 4.301258635363705451, 1.467727663998198429, 1.085573330547324744 ) ) ;
#111486 = CARTESIAN_POINT ( 'NONE',  ( 2.219515905360454067, 0.3404028402014187549, -1.931851785523025944 ) ) ;
#111487 = CARTESIAN_POINT ( 'NONE',  ( 0.01740989766754827417, -1.933669582450600499, 0.8627405663345076858 ) ) ;
#111488 = CARTESIAN_POINT ( 'NONE',  ( 9.406473150210953094, 3.553052365627046072, 7.380698111333699352 ) ) ;
#111489 = CARTESIAN_POINT ( 'NONE',  ( 3.348500752450959350, 6.850408611260626834, 0.7216878364870540352 ) ) ;
#111490 = CARTESIAN_POINT ( 'NONE',  ( 8.263858322729371153, 9.599921783727809910, -1.199719254218446718 ) ) ;
#111491 = EDGE_CURVE ( 'NONE', #82008, #55892, #141842, .T. ) ;
#111492 = CARTESIAN_POINT ( 'NONE',  ( 2.666775373343560407, 0.7166976873529752323, 1.995817185486338019 ) ) ;
#111493 = CARTESIAN_POINT ( 'NONE',  ( -4.121315508874276112, 4.870918184183829602, -1.082531754730549967 ) ) ;
#111494 = CARTESIAN_POINT ( 'NONE',  ( -1.115562610750309283E-14, 9.843750000682801371, 1.500000000000001554 ) ) ;
#111495 = CIRCLE ( 'NONE', #90741, 0.5000000000000007772 ) ;
#111496 = CARTESIAN_POINT ( 'NONE',  ( -5.297426666345223190, 6.395294968284933823, -1.134026229594787383 ) ) ;
#111497 = CARTESIAN_POINT ( 'NONE',  ( 1.006788857090525013, 0.5974033793386055446, 1.982218910981221827 ) ) ;
#111499 = CARTESIAN_POINT ( 'NONE',  ( -1.500000000000015099, 13.26041666734946567, -0.8660254037844309360 ) ) ;
#111498 = CARTESIAN_POINT ( 'NONE',  ( -10.91033920341480723, 4.885615726745547782, 4.996448585388906238 ) ) ;
#111501 = ORIENTED_EDGE ( 'NONE', *, *, #27143, .T. ) ;
#111500 = CARTESIAN_POINT ( 'NONE',  ( 3.405137934272496558, -0.4347481476216079055, -2.178183672434565565 ) ) ;
#111502 = CARTESIAN_POINT ( 'NONE',  ( 0.3526649539562948243, 0.2173941373411722999, -2.288394520000771148 ) ) ;
#111504 = CARTESIAN_POINT ( 'NONE',  ( 6.121949867982135807, 2.033011618171334245, -0.3470327977990442792 ) ) ;
#111503 = CARTESIAN_POINT ( 'NONE',  ( 4.708759422647839976, 4.387974169377582001, -0.7998128361456211532 ) ) ;
#111506 = CARTESIAN_POINT ( 'NONE',  ( -1.737500000000000266, -2.158333333333331439, -3.009438278150923907 ) ) ;
#111505 = CARTESIAN_POINT ( 'NONE',  ( 6.229045230835819069, 6.231917288922055320, -0.7998128361456481317 ) ) ;
#111507 = CARTESIAN_POINT ( 'NONE',  ( 0.2329586101569892376, 6.948071080078905837, -2.440796105365902857 ) ) ;
#111508 = CARTESIAN_POINT ( 'NONE',  ( 5.108874002337426390, -0.2646564886703614006, 1.822002613180016883 ) ) ;
#111509 = CARTESIAN_POINT ( 'NONE',  ( 2.679707916995359263, 6.278076336469897711, -0.7998128361456291469 ) ) ;
#111510 = SURFACE_SIDE_STYLE ('',( #114709 ) ) ;
#111511 = CARTESIAN_POINT ( 'NONE',  ( 3.170621359714973941, -1.593115903276512757, -0.6614109595024783017 ) ) ;
#111512 = CARTESIAN_POINT ( 'NONE',  ( 0.7961116948485976730, -0.9110139862544311962, -1.799120828532501326 ) ) ;
#111513 = CARTESIAN_POINT ( 'NONE',  ( 3.094664012895144367, -0.4461126415513679833, 2.254854857015383462 ) ) ;
#111514 = CARTESIAN_POINT ( 'NONE',  ( -0.6823417656250212460, 3.363541667008085323, 1.181850606188767472 ) ) ;
#111515 = CARTESIAN_POINT ( 'NONE',  ( 2.935161367736533133, 0.2740405928264351143, 2.245665650516134093 ) ) ;
#111516 = CARTESIAN_POINT ( 'NONE',  ( 5.549480973255512595, -1.659368771798474196, -1.296820645603852018 ) ) ;
#111517 = CARTESIAN_POINT ( 'NONE',  ( -3.984117037569407938, 5.741498858621315371, 1.599625672291270506 ) ) ;
#111518 = CARTESIAN_POINT ( 'NONE',  ( 4.129968326689526847, 0.9481555284369269643, -1.494110371635357648 ) ) ;
#111519 = CARTESIAN_POINT ( 'NONE',  ( 5.555090253297246150, 7.504024600312024340, 1.599625672291267398 ) ) ;
#111521 = CARTESIAN_POINT ( 'NONE',  ( 6.251568577072929678, 2.286574220100371591, -0.1642174239346057829 ) ) ;
#111520 = CARTESIAN_POINT ( 'NONE',  ( 3.892599500454941630, 6.595097612955829192, 1.082531754730549078 ) ) ;
#111522 = CARTESIAN_POINT ( 'NONE',  ( 4.242028835625204053, 0.4931972713904734795, 1.773778790588397491 ) ) ;
#111523 = CARTESIAN_POINT ( 'NONE',  ( -5.759516327706961647, 5.613857225279885732, -0.7998128361456221525 ) ) ;
#111524 = CARTESIAN_POINT ( 'NONE',  ( 4.650083499362864359, 7.408552601689905259, 1.082531754730558626 ) ) ;
#111525 = CARTESIAN_POINT ( 'NONE',  ( -1.500000000000013101, 4.129166666666687746, -0.8660254037844313801 ) ) ;
#111526 =( GEOMETRIC_REPRESENTATION_CONTEXT ( 3 ) GLOBAL_UNCERTAINTY_ASSIGNED_CONTEXT ( ( #115579 ) ) GLOBAL_UNIT_ASSIGNED_CONTEXT ( ( #162627, #196188, #47830 ) ) REPRESENTATION_CONTEXT ( 'NONE', 'WORKASPACE' ) );
#111527 = CARTESIAN_POINT ( 'NONE',  ( 5.050807487124363782, -1.850163549229045579, -1.174163402404400092 ) ) ;
#111528 = CARTESIAN_POINT ( 'NONE',  ( -3.438964519360665051, 7.163875705896082913, -0.7998128361456281477 ) ) ;
#111529 = FACE_OUTER_BOUND ( 'NONE', #211869, .T. ) ;
#111530 = CARTESIAN_POINT ( 'NONE',  ( 0.4648879685169841069, -7.768188185258929401, 9.920930332858635126 ) ) ;
#111531 = CARTESIAN_POINT ( 'NONE',  ( -1.364683531249997417, 4.009375000341424133, 1.214306433183764966E-14 ) ) ;
#111532 = CARTESIAN_POINT ( 'NONE',  ( 3.193887106011963350, -0.7802878698427909709, 1.761581285093082982 ) ) ;
#111533 = CARTESIAN_POINT ( 'NONE',  ( 1.364683531249996529, 9.213541667008062319, 0.7879004041258405033 ) ) ;
#111534 = CARTESIAN_POINT ( 'NONE',  ( -4.338245966692955591, 5.124003718305597310, 1.082531754730560403 ) ) ;
#111535 = CARTESIAN_POINT ( 'NONE',  ( 0.2994921435493704820, -0.2801620449621230469, -2.203647339609093869 ) ) ;
#111536 = ORIENTED_EDGE ( 'NONE', *, *, #60217, .T. ) ;
#111538 =( LENGTH_UNIT ( ) NAMED_UNIT ( * ) SI_UNIT ( .MILLI., .METRE. ) );
#111537 = CARTESIAN_POINT ( 'NONE',  ( -3.662110889467009578, 7.286563447771212232, 0.7216878364870338292 ) ) ;
#111539 = CARTESIAN_POINT ( 'NONE',  ( 4.005544317833563461, 6.760553239859419250, -1.199719254218452047 ) ) ;
#111540 = CARTESIAN_POINT ( 'NONE',  ( -15.75000000000000000, 13.79999999999998295, 3.199999999999997957 ) ) ;
#111541 = CARTESIAN_POINT ( 'NONE',  ( 0.000000000000000000, 13.49999999999999822, 0.000000000000000000 ) ) ;
#111542 = CARTESIAN_POINT ( 'NONE',  ( 0.5146009213643799596, 6.747837823239234645, -3.492810981166099005 ) ) ;
#111543 = CARTESIAN_POINT ( 'NONE',  ( 2.507021497916587460, -1.721230695331811722, 0.2570161617474544524 ) ) ;
#111544 = CARTESIAN_POINT ( 'NONE',  ( -4.715984300600573498, 7.775727532590477331, -0.9995835380776016965 ) ) ;
#111545 = CARTESIAN_POINT ( 'NONE',  ( 0.5374593765826127800, 1.831924746014142791, -0.7026076897959919743 ) ) ;
#111546 = CARTESIAN_POINT ( 'NONE',  ( -0.6823417656250212460, 1.863541667008083991, 1.181850606188755259 ) ) ;
#111547 = CARTESIAN_POINT ( 'NONE',  ( 5.946190753372003535, 2.158995856162956084, 0.1107517376499680406 ) ) ;
#111548 = CARTESIAN_POINT ( 'NONE',  ( -9.592557376868645846, 11.15007068022363157, -1.199719254218441611 ) ) ;
#111549 = CARTESIAN_POINT ( 'NONE',  ( -6.358410854684789726, 8.441231968597481483, -1.443375672974058777 ) ) ;
#111550 = CARTESIAN_POINT ( 'NONE',  ( 5.225516498768126183, -2.053876642077703707, 0.6744380372525200507 ) ) ;
#111552 = EDGE_LOOP ( 'NONE', ( #127980, #184223, #53964, #8228 ) ) ;
#111551 = CARTESIAN_POINT ( 'NONE',  ( -0.2104748580754166321, -0.006608320950486632102, -2.103482951484026309 ) ) ;
#111553 = CARTESIAN_POINT ( 'NONE',  ( -1.364683531250012516, 3.988541667008088876, -0.7879004041258300672 ) ) ;
#111554 = CARTESIAN_POINT ( 'NONE',  ( 0.7900579835180140398, -1.855660487967484951, -0.2351621623290362506 ) ) ;
#111555 = CARTESIAN_POINT ( 'NONE',  ( 5.747320757027973848, -1.692087196126054849, -0.3772414270737846631 ) ) ;
#111557 = CARTESIAN_POINT ( 'NONE',  ( 2.876726420669137863, -0.1638259704515396820, -2.185508879517850112 ) ) ;
#111556 = CARTESIAN_POINT ( 'NONE',  ( 1.360316468749968033, 1.015625000341371820, -4.163336342344337027E-14 ) ) ;
#111558 = CARTESIAN_POINT ( 'NONE',  ( 2.995503060082918889, 1.979820613015465858, -1.185208598768563881 ) ) ;
#111559 = B_SPLINE_CURVE_WITH_KNOTS ( 'NONE', 3,
 ( #15403, #64184, #81493, #30624, #213591, #181119, #51125, #32738, #80426, #112997 ),
 .UNSPECIFIED., .F., .F.,
 ( 4, 2, 2, 2, 4 ),
 ( 0.0002564548269640155843, 0.0006929466575915253432, 0.001129438488219035265, 0.001565930318846545186, 0.002002422149474054891 ),
 .UNSPECIFIED. ) ;
#111560 = CARTESIAN_POINT ( 'NONE',  ( 5.905559377550752664, -0.5051061836833131702, 1.997775138168448761 ) ) ;
#111561 = CARTESIAN_POINT ( 'NONE',  ( 1.148265734048327769, -1.531264750074516234, 1.194210492925862344 ) ) ;
#111562 = CARTESIAN_POINT ( 'NONE',  ( -6.846504384776765484, 8.050305206070113684, -1.082531754730543083 ) ) ;
#111563 = FACE_OUTER_BOUND ( 'NONE', #205884, .T. ) ;
#111564 = CARTESIAN_POINT ( 'NONE',  ( 5.575758015699216585, 5.849789923344298259, -0.7899890411014517388 ) ) ;
#111565 = CARTESIAN_POINT ( 'NONE',  ( 4.113620189327307664, 1.705085180707970771, 1.260635662952174663 ) ) ;
#111566 = CARTESIAN_POINT ( 'NONE',  ( -1.338312056661794536E-15, 3.975933801733731787, 11.54759062144379023 ) ) ;
#111567 = CARTESIAN_POINT ( 'NONE',  ( 2.268204128460939550, 1.842446992372799963, -0.8197738674571022344 ) ) ;
#111568 = CARTESIAN_POINT ( 'NONE',  ( -5.056828107772852299, 7.883087978168217269, -1.082531754730548412 ) ) ;
#111569 = CARTESIAN_POINT ( 'NONE',  ( 5.983472182158235952, 2.041168445429199618, -0.8392293214988936212 ) ) ;
#111570 = DIRECTION ( 'NONE',  ( 0.000000000000000000, 1.000000000000000000, 0.000000000000000000 ) ) ;
#111571 = CARTESIAN_POINT ( 'NONE',  ( -3.440154425158069795, -3.082311296064041528, 0.07384894924763349411 ) ) ;
#111572 = DIRECTION ( 'NONE',  ( -1.000000000000000000, 0.000000000000000000, 0.000000000000000000 ) ) ;
#111573 = CARTESIAN_POINT ( 'NONE',  ( -6.831329296439251131, 9.063246493969506545, -1.599625672291271394 ) ) ;
#111575 = CARTESIAN_POINT ( 'NONE',  ( 6.825078400183577365, 2.023440267519378999, 2.448151054272352578 ) ) ;
#111574 = CARTESIAN_POINT ( 'NONE',  ( -4.936046011350697427, 8.098431898006973384, 1.075429046246343612 ) ) ;
#111576 = DIRECTION ( 'NONE',  ( 0.000000000000000000, -1.000000000000000000, 0.000000000000000000 ) ) ;
#111577 = ORIENTED_EDGE ( 'NONE', *, *, #61190, .T. ) ;
#111578 = CARTESIAN_POINT ( 'NONE',  ( 4.786040499707863383, -0.9732044846940243188, 1.816634495032407814 ) ) ;
#111579 = CARTESIAN_POINT ( 'NONE',  ( 4.067759563269675915, 7.712442911444558291, -0.5649101002591673248 ) ) ;
#111580 = CARTESIAN_POINT ( 'NONE',  ( 0.000000000000000000, 8.499999999999996447, 0.000000000000000000 ) ) ;
#111581 = CARTESIAN_POINT ( 'NONE',  ( -5.603597561149804562, 5.431951997629870910, 0.7998128361456341429 ) ) ;
#111582 = CARTESIAN_POINT ( 'NONE',  ( -5.340986169140711226, 5.195848383611072485, 0.000000000000000000 ) ) ;
#111583 = CARTESIAN_POINT ( 'NONE',  ( 4.072919328976184694, -1.495020084728536203, 1.358112258667160344 ) ) ;
#111584 = CARTESIAN_POINT ( 'NONE',  ( -1.500000000000015099, 0.3791666666666850261, -0.8660254037844383745 ) ) ;
#111586 = CARTESIAN_POINT ( 'NONE',  ( 9.137832345930652522, 10.72352116074969075, -1.082531754730543083 ) ) ;
#111585 = CARTESIAN_POINT ( 'NONE',  ( -5.842637852846353397, 5.781108681267656202, 0.7998128361456281477 ) ) ;
#111587 = CARTESIAN_POINT ( 'NONE',  ( 7.308008492965924141, 8.484763649003774333, -1.199719254218451159 ) ) ;
#111588 = CARTESIAN_POINT ( 'NONE',  ( 2.711851390082948399, -2.038666671984638690, 0.3009093235433103475 ) ) ;
#111589 = CARTESIAN_POINT ( 'NONE',  ( 3.111954093273407551, 0.05229746705895028935, 2.015912966248374349 ) ) ;
#111590 = ORIENTED_EDGE ( 'NONE', *, *, #83669, .T. ) ;
#111591 = CARTESIAN_POINT ( 'NONE',  ( 1.882262909678001916, 3.299172163371817401, -0.4004916885353014266 ) ) ;
#111592 = CARTESIAN_POINT ( 'NONE',  ( 4.680589345215795838, 6.483773540883647435, -1.599625672291256295 ) ) ;
#111593 = VECTOR ( 'NONE', #145550, 1000.000000000000000 ) ;
#111595 = ORIENTED_EDGE ( 'NONE', *, *, #144753, .F. ) ;
#111594 = CARTESIAN_POINT ( 'NONE',  ( -3.031872956992967882, 6.300826765685804354, -0.7659957782561641615 ) ) ;
#111596 = CARTESIAN_POINT ( 'NONE',  ( 3.409529676982744562, 0.4871283372531940992, 1.956261718130556382 ) ) ;
#111597 = CARTESIAN_POINT ( 'NONE',  ( 2.906014618889842360, 1.333239036598636407, -1.269987479889053139 ) ) ;
#111598 = AXIS2_PLACEMENT_3D ( 'NONE', #34827, #100901, #18581 ) ;
#111599 = CARTESIAN_POINT ( 'NONE',  ( 6.516270054225981490, -1.036149114087565382, -1.948532232987249424 ) ) ;
#111600 = CARTESIAN_POINT ( 'NONE',  ( 4.603875680292229156, 7.528882839386387360, 1.199719254218452047 ) ) ;
#111601 = CARTESIAN_POINT ( 'NONE',  ( 2.372553944209778720, -1.331880425775422205, 1.702409713178254069 ) ) ;
#111602 = CARTESIAN_POINT ( 'NONE',  ( -6.898401231254901234, 6.942556279419168419, -0.7998128361456291469 ) ) ;
#111603 = CARTESIAN_POINT ( 'NONE',  ( 2.706789001878449508, -1.702045039646230107, -1.544681222897727357 ) ) ;
#111604 = ORIENTED_EDGE ( 'NONE', *, *, #50310, .F. ) ;
#111605 = FACE_OUTER_BOUND ( 'NONE', #21763, .T. ) ;
#111606 = CARTESIAN_POINT ( 'NONE',  ( 1.322894217037654085, -0.04941562205608432401, 1.870173573632450958 ) ) ;
#111607 = VERTEX_POINT ( 'NONE', #122444 ) ;
#111608 = CARTESIAN_POINT ( 'NONE',  ( 5.735224789204648843, -1.782488891340678894, 0.8425237689327728097 ) ) ;
#111610 = CARTESIAN_POINT ( 'NONE',  ( 9.070041577417981671, 9.684062716516882219, -0.7216878364870197293 ) ) ;
#111609 = CARTESIAN_POINT ( 'NONE',  ( 1.364683531249988535, 2.905208333674754506, -0.7879004041258239610 ) ) ;
#111612 = CARTESIAN_POINT ( 'NONE',  ( 0.6455096168876961471, -1.890800792967793686, 1.137844069391671820 ) ) ;
#111611 = CARTESIAN_POINT ( 'NONE',  ( -5.689618019229208734, 9.789638122409414223, 0.7998128361456481317 ) ) ;
#111613 = CARTESIAN_POINT ( 'NONE',  ( 6.109843426155951107, 0.6047356833836557977, -1.980059631771100781 ) ) ;
#111614 = CARTESIAN_POINT ( 'NONE',  ( 6.277588818327314080, 7.282607361925381717, 1.199719254218462483 ) ) ;
#111615 = CARTESIAN_POINT ( 'NONE',  ( -4.903245109636583443, 8.872203061218007392, -0.7998128361456281477 ) ) ;
#111616 = CARTESIAN_POINT ( 'NONE',  ( 6.539320575229255361, 7.051987793746187450, 2.801414728815339039 ) ) ;
#111617 = CARTESIAN_POINT ( 'NONE',  ( 5.313337694394675736, -0.2901137614541632881, 1.949896409304814116 ) ) ;
#111618 = CARTESIAN_POINT ( 'NONE',  ( 6.345964425358009642, -1.322526734765665513, -1.526637064097993157 ) ) ;
#111619 = CARTESIAN_POINT ( 'NONE',  ( -1.500000000000015099, 0.6604166673494823447, -0.8660254037844313801 ) ) ;
#111620 = CARTESIAN_POINT ( 'NONE',  ( 4.741030679083562127, 0.3911436318500530751, 2.274166950501448348 ) ) ;
#111621 = CARTESIAN_POINT ( 'NONE',  ( 1.832955167792608364, -1.957230265441430417, -0.6508311760726466222 ) ) ;
#111622 = CARTESIAN_POINT ( 'NONE',  ( 6.968527767744098433, 9.153035033833367251, 1.443375672974076540 ) ) ;
#111623 = CARTESIAN_POINT ( 'NONE',  ( 6.690022453700429139, 6.769724048930809701, 0.7998128361456331437 ) ) ;
#111624 = CARTESIAN_POINT ( 'NONE',  ( 3.953084306836263995, 6.769626237021087789, 1.199719254218452047 ) ) ;
#111625 = CARTESIAN_POINT ( 'NONE',  ( 0.6823417656249899377, 2.405208333674753618, 1.181850606188767472 ) ) ;
#111626 = CARTESIAN_POINT ( 'NONE',  ( 3.878514461961128479, 6.682628084666728085, -1.199719254218448494 ) ) ;
#111627 = CARTESIAN_POINT ( 'NONE',  ( 6.168596704093459060, 7.259412911939593371, -1.082531754730543083 ) ) ;
#111628 = CARTESIAN_POINT ( 'NONE',  ( 3.807220332926362083, -1.777014928589750076, 1.247251757893479640 ) ) ;
#111630 = CARTESIAN_POINT ( 'NONE',  ( 4.388128076750056117, -0.4078595375654435751, -1.795341762384855544 ) ) ;
#111629 = CARTESIAN_POINT ( 'NONE',  ( -3.118012141462980669, 6.581505231774690046, 0.7216878364870317197 ) ) ;
#111631 = EDGE_CURVE ( 'NONE', #157630, #50845, #57348, .T. ) ;
#111633 = CARTESIAN_POINT ( 'NONE',  ( 6.720655732516647163, 2.082321177337285167, 2.135279995619132620 ) ) ;
#111632 = FACE_OUTER_BOUND ( 'NONE', #5023, .T. ) ;
#111634 = CARTESIAN_POINT ( 'NONE',  ( 5.425378541715013547, -1.389685604419872655, -1.694579525865948844 ) ) ;
#111635 = LINE ( 'NONE', #177646, #129316 ) ;
#111636 = CARTESIAN_POINT ( 'NONE',  ( 5.717715967963762580, -2.208827357630326560, 0.4893477075747532101 ) ) ;
#111637 = ORIENTED_EDGE ( 'NONE', *, *, #198065, .F. ) ;
#111638 = CARTESIAN_POINT ( 'NONE',  ( -4.028535363944735437, 7.777154369360758324, -0.5044922354892691363 ) ) ;
#111639 = CARTESIAN_POINT ( 'NONE',  ( 4.636584873806110174, 8.438537862545894441, 0.4145994950837776916 ) ) ;
#111640 = CARTESIAN_POINT ( 'NONE',  ( -6.902509602688830626, 7.225551755991315162, -0.7216878364870338292 ) ) ;
#111641 = CARTESIAN_POINT ( 'NONE',  ( -6.643335646896348479, -7.986884274785886362, -6.845108005540228469 ) ) ;
#111642 = CARTESIAN_POINT ( 'NONE',  ( 0.9008075156715513732, 1.443549170786810443, 1.023676300919857507 ) ) ;
#111643 = CARTESIAN_POINT ( 'NONE',  ( 4.793612393603923216, 1.877549684267119101, -0.7266104139797191497 ) ) ;
#111644 = CARTESIAN_POINT ( 'NONE',  ( 5.147291874682557555, 9.156924287104992288, 0.7998128361456462443 ) ) ;
#111645 = CARTESIAN_POINT ( 'NONE',  ( 4.190527447551747109, -2.082725220463335081, -0.3111483248238402499 ) ) ;
#111646 = CARTESIAN_POINT ( 'NONE',  ( 1.985809494836645817, -1.915157380443854418, 0.04907906824581054206 ) ) ;
#111647 = CARTESIAN_POINT ( 'NONE',  ( 2.849184837166184536, 6.475799410002530898, 0.7998128361456362523 ) ) ;
#111648 = CARTESIAN_POINT ( 'NONE',  ( 3.244544899158372520, -1.939951241085198896, -0.3392403660903812734 ) ) ;
#111649 = CARTESIAN_POINT ( 'NONE',  ( 5.080334495226257907, 0.9990293545295618749, 1.755361416599170443 ) ) ;
#111650 = CARTESIAN_POINT ( 'NONE',  ( 2.026040307571222332, 1.079255042350239391, -1.527726335390042767 ) ) ;
#111653 = EDGE_LOOP ( 'NONE', ( #78448, #47092, #148101, #184320 ) ) ;
#111652 = CARTESIAN_POINT ( 'NONE',  ( 1.845825534506392085, -1.251752223804462272, -1.445855903880132631 ) ) ;
#111651 = CARTESIAN_POINT ( 'NONE',  ( 5.426277463695272196, 1.022757762066462961, -1.388784613272223689 ) ) ;
#111655 = CARTESIAN_POINT ( 'NONE',  ( 3.687454593236936251, 7.245854758844324728, -0.7216878364870267237 ) ) ;
#111654 = CARTESIAN_POINT ( 'NONE',  ( 1.577102763248950046, -2.096353118739826993, -0.6898709473643764856 ) ) ;
#111656 = CARTESIAN_POINT ( 'NONE',  ( 1.364683531249988757, 2.446875000341415696, 1.214306433183764966E-14 ) ) ;
#111657 = CARTESIAN_POINT ( 'NONE',  ( 8.402302512167096893, 10.82577223566020841, -1.599625672291268286 ) ) ;
#111658 = CARTESIAN_POINT ( 'NONE',  ( 11.92619526248521034, 11.02744613914163807, 1.328859120100916558 ) ) ;
#111659 = DIRECTION ( 'NONE',  ( -0.8002608041566210417, 0.5996521035822340862, 0.000000000000000000 ) ) ;
#111660 = CARTESIAN_POINT ( 'NONE',  ( 0.1054570145121072472, 2.614151819895196738, -2.076146791065091701 ) ) ;
#111661 = COLOUR_RGB ( '', 0.72549020, 0.75294118, 0.79215686) ;
#111662 = DIRECTION ( 'NONE',  ( -4.440892098500624683E-16, 6.661338147750949103E-16, -1.000000000000000000 ) ) ;
#111663 = CIRCLE ( 'NONE', #32123, 11.09999999999999964 ) ;
#111664 = ADVANCED_FACE ( 'NONE', ( #25896 ), #175378, .F. ) ;
#111665 = CARTESIAN_POINT ( 'NONE',  ( 0.5552397518338060278, 1.722184604005328357, -1.148819969904082861 ) ) ;
#111666 = CARTESIAN_POINT ( 'NONE',  ( -1.499999999999997780, 2.150000000000019895, 1.214306433183764966E-14 ) ) ;
#111667 = CARTESIAN_POINT ( 'NONE',  ( 6.634017235788401301, 6.634108284708264414, 0.7998128361456341429 ) ) ;
#111668 = CARTESIAN_POINT ( 'NONE',  ( -7.283754839039664475, 9.520799950344851936, -1.599625672291263179 ) ) ;
#111669 = CARTESIAN_POINT ( 'NONE',  ( 6.201928923608456046, 6.200281597156833691, 0.7998128361456352531 ) ) ;
#111670 = CARTESIAN_POINT ( 'NONE',  ( 6.428397668822618094, -0.9990526908794925554, -1.870407359624715937 ) ) ;
#111671 =( LENGTH_UNIT ( ) NAMED_UNIT ( * ) SI_UNIT ( .MILLI., .METRE. ) );
#111672 = CARTESIAN_POINT ( 'NONE',  ( -0.6823417656250003738, 2.217708333674753174, -1.181850606188749264 ) ) ;
#111674 = CARTESIAN_POINT ( 'NONE',  ( 4.356247428692526569, 3.976710176429713250, 0.7998128361456341429 ) ) ;
#111673 = CARTESIAN_POINT ( 'NONE',  ( 0.07479286986305544449, 6.948552162806721277, -2.450557996216149892 ) ) ;
#111675 = CARTESIAN_POINT ( 'NONE',  ( 4.253279712585047001, -1.993766238088546361, -0.2985801555873274227 ) ) ;
#111676 = CARTESIAN_POINT ( 'NONE',  ( 4.329236433732988942, -1.484621416154695117, -1.210779873830228670 ) ) ;
#111677 = FACE_OUTER_BOUND ( 'NONE', #116739, .T. ) ;
#111678 = CARTESIAN_POINT ( 'NONE',  ( 2.384552795368581890, -0.3778730364575392797, -2.158588602542845347 ) ) ;
#111679 = FACE_OUTER_BOUND ( 'NONE', #29319, .T. ) ;
#111680 = CARTESIAN_POINT ( 'NONE',  ( -1.500000000000001332, 0.9312500006828163812, 0.000000000000000000 ) ) ;
#111681 = CARTESIAN_POINT ( 'NONE',  ( 5.010025764882303001, -0.7205479882510434919, 1.880027049715059073 ) ) ;
#111682 = CARTESIAN_POINT ( 'NONE',  ( -6.693975156845199059, 8.832723654451292816, 1.599625672291283607 ) ) ;
#111684 = CARTESIAN_POINT ( 'NONE',  ( 5.730101960677154160, 2.114805460001396575, 0.1033778851832044821 ) ) ;
#111683 = CARTESIAN_POINT ( 'NONE',  ( -2.643476764984671767, 6.027880625883323518, 1.040834085586084257E-14 ) ) ;
#111685 = CARTESIAN_POINT ( 'NONE',  ( 1.364683531250000303, 9.067708333674733723, -0.7879004041258355073 ) ) ;
#111687 = CARTESIAN_POINT ( 'NONE',  ( -5.745623237141265882, 9.925253886631958622, 0.7998128361456291469 ) ) ;
#111686 = CARTESIAN_POINT ( 'NONE',  ( 3.878531184313998015, -0.2068018975109634505, -2.080507369234054771 ) ) ;
#111689 = VERTEX_POINT ( 'NONE', #191591 ) ;
#111688 = CARTESIAN_POINT ( 'NONE',  ( 1.447837905203141373, 1.722567860661971206, 0.08979103728979326293 ) ) ;
#111690 = CARTESIAN_POINT ( 'NONE',  ( 4.781546299372162245, 0.2051969522943071500, -2.110614603223801122 ) ) ;
#111691 = CARTESIAN_POINT ( 'NONE',  ( 4.961394147597008697, 7.875711374583454827, -1.199719254218452047 ) ) ;
#111692 = TOROIDAL_SURFACE ( 'NONE', #56268, 11.92000000000000171, 0.08000000000000000167 ) ;
#111693 = CARTESIAN_POINT ( 'NONE',  ( 7.834948825496932834, -6.134628647623485698, 7.720982897393583677 ) ) ;
#111694 = CARTESIAN_POINT ( 'NONE',  ( -7.013428937081412684, 5.939655416065874327, 2.436399677959149468 ) ) ;
#111695 = CARTESIAN_POINT ( 'NONE',  ( 6.226218857173709154, 8.287007971501239467, 1.599625672291281386 ) ) ;
#111696 = ORIENTED_EDGE ( 'NONE', *, *, #35037, .T. ) ;
#111697 = CARTESIAN_POINT ( 'NONE',  ( 0.000000000000000000, -5.223431457505076203, 0.000000000000000000 ) ) ;
#111698 = ORIENTED_EDGE ( 'NONE', *, *, #210974, .F. ) ;
#111700 = CARTESIAN_POINT ( 'NONE',  ( 1.787489318380721448, 1.733277665728020001, -0.5263807565755849183 ) ) ;
#111699 = CARTESIAN_POINT ( 'NONE',  ( 5.559725510055676168, 8.644040974110419384, 1.199719254218451159 ) ) ;
#111701 = CARTESIAN_POINT ( 'NONE',  ( -7.054319997812058318, 7.124461507069184130, 1.040834085586084257E-14 ) ) ;
#111702 = ORIENTED_EDGE ( 'NONE', *, *, #8106, .F. ) ;
#111703 = CARTESIAN_POINT ( 'NONE',  ( 3.029357257649615054, 5.621668336311468117, -1.199719254218446718 ) ) ;
#111704 = CARTESIAN_POINT ( 'NONE',  ( 4.227110032410640095, 8.153655147779589996, 0.7998128361456271485 ) ) ;
#111705 = CARTESIAN_POINT ( 'NONE',  ( 3.123486050149349769, -0.3508677868355335461, 1.776971544703136452 ) ) ;
#111706 = CARTESIAN_POINT ( 'NONE',  ( 6.639320575229236354, 1.260096212659385984, 2.110683211146132443 ) ) ;
#111707 =( LENGTH_UNIT ( ) NAMED_UNIT ( * ) SI_UNIT ( .MILLI., .METRE. ) );
#111708 = CARTESIAN_POINT ( 'NONE',  ( 4.254136489245101238, 7.273159757992218921, 0.9281648423343953347 ) ) ;
#111709 = VERTEX_POINT ( 'NONE', #126695 ) ;
#111710 = CARTESIAN_POINT ( 'NONE',  ( 4.369486748645814878, -0.3193033414996570007, 1.833288415851072273 ) ) ;
#111711 = CARTESIAN_POINT ( 'NONE',  ( 1.159628707424670280, 1.142309718407741093, 1.537566464135895261 ) ) ;
#111712 = CARTESIAN_POINT ( 'NONE',  ( 6.704134009050578769, -1.925936059460537697, 0.04828832120675958378 ) ) ;
#111713 = CARTESIAN_POINT ( 'NONE',  ( -1.115562610750309283E-14, 11.56249999999999822, 1.500000000000001554 ) ) ;
#111714 = DIRECTION ( 'NONE',  ( -1.276756478318932585E-15, 1.000000000000000000, -1.665334536937738262E-16 ) ) ;
#111715 = CARTESIAN_POINT ( 'NONE',  ( 1.224999999999992983, 1.458333334016139071, -0.7072540797572817173 ) ) ;
#111716 = SURFACE_STYLE_FILL_AREA ( #210195 ) ;
#111717 = CARTESIAN_POINT ( 'NONE',  ( -4.622967192579922724, 4.495809267539077503, 1.214306433183764966E-14 ) ) ;
#111718 = CARTESIAN_POINT ( 'NONE',  ( 7.293923454472077239, 10.49303254931736262, 1.082531754730558626 ) ) ;
#111719 = CARTESIAN_POINT ( 'NONE',  ( 6.315293006042116630, -1.687366247620238457, -1.015419155273014740 ) ) ;
#111720 = CARTESIAN_POINT ( 'NONE',  ( -3.906720819032141190, 7.709591388846142479, -0.7998128361456281477 ) ) ;
#111721 = CARTESIAN_POINT ( 'NONE',  ( -11.95360554405587017, 9.995550034974055365, -1.059413164304675359 ) ) ;
#111722 = CARTESIAN_POINT ( 'NONE',  ( 0.3575176574102476579, 2.067590324638542310, -0.3087094068163088179 ) ) ;
#111723 = CARTESIAN_POINT ( 'NONE',  ( 4.840804290916858932, 0.3290424097142484738, 1.897927756555679801 ) ) ;
#111724 = CARTESIAN_POINT ( 'NONE',  ( -5.371001409308059138, 9.417918744168066070, -0.7998128361456231517 ) ) ;
#111725 = CARTESIAN_POINT ( 'NONE',  ( 1.201864610381056853, -1.825762228264395048, -0.004348209057210283834 ) ) ;
#111726 = CARTESIAN_POINT ( 'NONE',  ( 1.981372325807278623, -0.1102420082176903682, -2.204251428397439483 ) ) ;
#111727 = SURFACE_STYLE_FILL_AREA ( #45612 ) ;
#111728 = CARTESIAN_POINT ( 'NONE',  ( 0.2637284958507991606, 0.5978344860198721022, -1.816641584731902626 ) ) ;
#111729 = ORIENTED_EDGE ( 'NONE', *, *, #117853, .F. ) ;
#111730 = CARTESIAN_POINT ( 'NONE',  ( 0.3441184698094986727, -0.9315698024882634876, 1.735327799219071210 ) ) ;
#111732 = B_SPLINE_CURVE_WITH_KNOTS ( 'NONE', 3,
 ( #201834, #119617, #189880, #20950, #39368, #37232, #53479, #106554 ),
 .UNSPECIFIED., .F., .F.,
 ( 4, 2, 2, 4 ),
 ( 6.586514544919025777E-16, 0.0002305131806121977036, 0.0004610263612237367544, 0.0009220527224468139885 ),
 .UNSPECIFIED. ) ;
#111731 = CARTESIAN_POINT ( 'NONE',  ( 2.718228044968384882, 1.829540209339441503, 0.6518440813585175686 ) ) ;
#111733 = ORIENTED_EDGE ( 'NONE', *, *, #191590, .T. ) ;
#111734 = CARTESIAN_POINT ( 'NONE',  ( 1.352888501574830205, -0.9090079681693465918, 1.799646022210943386 ) ) ;
#111736 = CARTESIAN_POINT ( 'NONE',  ( 5.278104476702146108, -0.9935453584285673934, -1.573305019461817444 ) ) ;
#111735 = CARTESIAN_POINT ( 'NONE',  ( -5.119085517611572378, 8.129960982925583224, 1.199719254218452935 ) ) ;
#111737 = CARTESIAN_POINT ( 'NONE',  ( 5.224688093219824303, 7.188831756880171397, -1.599625672291283607 ) ) ;
#111738 = PRESENTATION_STYLE_ASSIGNMENT (( #48809 ) ) ;
#111739 = DIRECTION ( 'NONE',  ( -1.224646799147353207E-16, 1.000000000000000000, 0.000000000000000000 ) ) ;
#111740 = CARTESIAN_POINT ( 'NONE',  ( -3.405069135326500351, 7.124331091189553433, 1.040834085586084257E-14 ) ) ;
#111741 = CARTESIAN_POINT ( 'NONE',  ( -5.803772275101700906, 8.928762199997411386, -1.199719254218452047 ) ) ;
#111742 = CARTESIAN_POINT ( 'NONE',  ( 1.663894474538109236, 1.130263417742288112, 1.877492182091732076 ) ) ;
#111743 = CARTESIAN_POINT ( 'NONE',  ( 4.717874267875568961, 4.606534188717351874, -0.7216878364870188411 ) ) ;
#111744 = CARTESIAN_POINT ( 'NONE',  ( 5.840530312436913007, 10.03597880781023299, 0.000000000000000000 ) ) ;
#111745 = PLANE ( 'NONE',  #64990 ) ;
#111746 = CARTESIAN_POINT ( 'NONE',  ( 3.264084022359412529, 0.8216391472936382945, 1.630427331384458833 ) ) ;
#111747 = CARTESIAN_POINT ( 'NONE',  ( -3.918470089549458635, 4.530302178351167441, -1.199719254218452047 ) ) ;
#111748 = CARTESIAN_POINT ( 'NONE',  ( -2.916975605234527702, 6.554888639415577423, 1.040834085586084257E-14 ) ) ;
#111749 = CARTESIAN_POINT ( 'NONE',  ( -0.4134159855572216435, 2.995616482383578028, -2.020255554130489184 ) ) ;
#111750 = DIRECTION ( 'NONE',  ( 0.000000000000000000, 8.546850786086437571E-32, 1.000000000000000000 ) ) ;
#111751 = CARTESIAN_POINT ( 'NONE',  ( 8.594979316059474073, 12.11489407112305372, 1.199719254218450271 ) ) ;
#111752 = AXIS2_PLACEMENT_3D ( 'NONE', #86820, #90037, #152885 ) ;
#111753 = CARTESIAN_POINT ( 'NONE',  ( 0.8559318490590170914, 1.924348548886562815, -0.09362981192203097269 ) ) ;
#111754 = CARTESIAN_POINT ( 'NONE',  ( 5.752778578519474273, -0.4731148833870613690, -1.903749215227706015 ) ) ;
#111755 = CARTESIAN_POINT ( 'NONE',  ( -6.690058733339450114, 9.892486724616283311, 1.199719254218452047 ) ) ;
#111756 = CARTESIAN_POINT ( 'NONE',  ( 5.335297142177534369, 6.183267073083954735, -1.199719254218452047 ) ) ;
#111757 = EDGE_CURVE ( 'NONE', #197667, #148685, #7822, .T. ) ;
#111758 = CARTESIAN_POINT ( 'NONE',  ( 5.179302069984247581, 1.471482994053765925, 1.624232740060495228 ) ) ;
#111759 = CARTESIAN_POINT ( 'NONE',  ( 3.486418057008484617, 7.219238166485217434, 1.040834085586084257E-14 ) ) ;
#111760 = CARTESIAN_POINT ( 'NONE',  ( 4.082924941702062327, 1.964217522864346810, 0.6541895251909736198 ) ) ;
#111762 = CARTESIAN_POINT ( 'NONE',  ( -1.364683531250014514, 1.051041667008090208, -0.7879004041258289570 ) ) ;
#111761 = CARTESIAN_POINT ( 'NONE',  ( 7.690609288285140899, 14.45647329385417912, 9.157199668769314016 ) ) ;
#111763 = ORIENTED_EDGE ( 'NONE', *, *, #156034, .T. ) ;
#111764 = CARTESIAN_POINT ( 'NONE',  ( 4.535913861531776448, -1.846855032230051208, 1.368429651993019025 ) ) ;
#111766 = ORIENTED_EDGE ( 'NONE', *, *, #150154, .F. ) ;
#111765 = CARTESIAN_POINT ( 'NONE',  ( 6.466876084038451822, 10.48851316477946582, 1.040834085586084257E-14 ) ) ;
#111768 = CARTESIAN_POINT ( 'NONE',  ( 1.642778471875000035, -0.2260416661887081069, -2.845375778867859751 ) ) ;
#111767 = CARTESIAN_POINT ( 'NONE',  ( 5.058600711674583472, 8.915801573680086634, 0.000000000000000000 ) ) ;
#111769 = CARTESIAN_POINT ( 'NONE',  ( -7.446209719563363194, -5.223431457505083308, -8.064677165291197269 ) ) ;
#111770 = DIRECTION ( 'NONE',  ( -1.000000000000000000, 7.771561172376097755E-16, 4.440892098500627148E-16 ) ) ;
#111771 = CARTESIAN_POINT ( 'NONE',  ( 3.609261671491706736, -1.913043583297647565, 0.3329670706836064809 ) ) ;
#111772 = EDGE_LOOP ( 'NONE', ( #91656, #83332, #65239, #71627 ) ) ;
#111774 = EDGE_CURVE ( 'NONE', #29321, #128826, #141217, .T. ) ;
#111773 = CARTESIAN_POINT ( 'NONE',  ( 9.693716643646590470, 12.33242205571964512, 1.443375672974076540 ) ) ;
#111775 = ORIENTED_EDGE ( 'NONE', *, *, #22536, .F. ) ;
#111776 = CARTESIAN_POINT ( 'NONE',  ( 4.904515063324526025, -1.898637117948184017, -0.2282459111111398431 ) ) ;
#111777 = DIRECTION ( 'NONE',  ( -3.330669073875477510E-16, 2.265265487380573707E-16, 1.000000000000000000 ) ) ;
#111778 = CARTESIAN_POINT ( 'NONE',  ( 5.807552366672524613, -0.4147409827905921831, 1.674012740457442305 ) ) ;
#111779 = CARTESIAN_POINT ( 'NONE',  ( 4.294157853547872605, -0.8666056138363427142, -1.820986994602633802 ) ) ;
#111780 = CARTESIAN_POINT ( 'NONE',  ( -1.608462485350627524, 8.735270501766752460, 2.463594439587639240 ) ) ;
#111781 = CARTESIAN_POINT ( 'NONE',  ( 2.280145854635793334, 1.358931147977986420, 1.738775483816151768 ) ) ;
#111783 = CARTESIAN_POINT ( 'NONE',  ( -4.828112100242303306, 4.805421336470338645, -0.7216878364870338292 ) ) ;
#111782 = CARTESIAN_POINT ( 'NONE',  ( -10.66756793585402363, 11.33991743478486391, 0.7998128361456462443 ) ) ;
#111785 = CARTESIAN_POINT ( 'NONE',  ( 6.731742716130249882, -1.158518921844574834, -1.337957499386055682 ) ) ;
#111784 = CARTESIAN_POINT ( 'NONE',  ( 1.834041477103361739, 2.068079971995392619, 0.3053845110000241170 ) ) ;
#111786 = CARTESIAN_POINT ( 'NONE',  ( 5.414685466650038137, -1.281359335986744341, -1.556910257834144051 ) ) ;
#111788 = CARTESIAN_POINT ( 'NONE',  ( 2.924086828919622238, 1.272802903806929953, -1.906236438263966271 ) ) ;
#111787 = CARTESIAN_POINT ( 'NONE',  ( 5.598591087800349086, 5.496387455380669529, -0.7998128361456481317 ) ) ;
#111789 = CARTESIAN_POINT ( 'NONE',  ( 1.622608716997505418, -1.639457832600412113, 0.5842430463761526527 ) ) ;
#111790 = VECTOR ( 'NONE', #212628, 1000.000000000000000 ) ;
#111791 = CARTESIAN_POINT ( 'NONE',  ( 11.92619526913699701, 10.90000000000000036, -1.328859060402686199 ) ) ;
#111792 = CARTESIAN_POINT ( 'NONE',  ( 0.8601780606121096628, -0.6315397308106798224, 1.614934579331471998 ) ) ;
#111793 = CARTESIAN_POINT ( 'NONE',  ( -1.360316468750042862, 0.1510416670080827195, -0.7853790794159282163 ) ) ;
#111794 = CARTESIAN_POINT ( 'NONE',  ( -11.41381675112453387, 12.69999999999998153, 3.704697986577180302 ) ) ;
#111795 = CARTESIAN_POINT ( 'NONE',  ( 1.082764339582122481, 1.293380948865870073, -1.743738868014677035 ) ) ;
#111796 = CARTESIAN_POINT ( 'NONE',  ( 1.921111612355221654, -1.799121770747251547, 0.9110121207814986244 ) ) ;
#111797 = CARTESIAN_POINT ( 'NONE',  ( 3.781250000000002665, 0.7852924748301846058, 1.895863743164001081 ) ) ;
#111798 = CARTESIAN_POINT ( 'NONE',  ( -1.402160292154681736E-14, 1.118750000682820378, -1.732050807568863648 ) ) ;
#111799 = CARTESIAN_POINT ( 'NONE',  ( 0.1824732010112985747, -1.867734037610004449, -0.4713708115406111676 ) ) ;
#111800 = CARTESIAN_POINT ( 'NONE',  ( -1.364683531250000748, 13.60937500034139980, 0.000000000000000000 ) ) ;
#111801 = CARTESIAN_POINT ( 'NONE',  ( 3.885193193976806292, -2.073655658835142024, -0.7971110592776513570 ) ) ;
#111802 = ORIENTED_EDGE ( 'NONE', *, *, #11046, .T. ) ;
#111803 = CARTESIAN_POINT ( 'NONE',  ( 6.391719147208887897, 6.567463349398139805, 2.438448605600926467 ) ) ;
#111804 = CARTESIAN_POINT ( 'NONE',  ( 0.7499999999999867883, -0.9333333333333138082, -1.299038105676652011 ) ) ;
#111806 = ADVANCED_FACE ( 'NONE', ( #206782 ), #173252, .F. ) ;
#111805 = CARTESIAN_POINT ( 'NONE',  ( 8.589254009457354400, 9.979550084910457031, -1.199719254218446718 ) ) ;
#111807 = CARTESIAN_POINT ( 'NONE',  ( -10.59781858645781405, 9.799999999999984723, 3.302687032930891498 ) ) ;
#111808 = CARTESIAN_POINT ( 'NONE',  ( 5.776847720190436242, 1.604795045139913556, -0.6741588622883755155 ) ) ;
#111809 = CARTESIAN_POINT ( 'NONE',  ( 3.771884902471400292, -1.933230903833718539, 0.3329965046865584477 ) ) ;
#111811 = CARTESIAN_POINT ( 'NONE',  ( -4.609409038966229666, 8.321468278861834378, -0.7216878364870267237 ) ) ;
#111810 = CARTESIAN_POINT ( 'NONE',  ( 4.681643115420508039, 4.356338477612361260, 0.7998128361456341429 ) ) ;
#111812 = CARTESIAN_POINT ( 'NONE',  ( -1.476450096886795516, 4.272190093455678905, -0.2781497094537733195 ) ) ;
#111813 = CARTESIAN_POINT ( 'NONE',  ( 4.868612525405347391, -1.482742447731852709, 1.708856814797095725 ) ) ;
#111814 = CIRCLE ( 'NONE', #104951, 0.08000000000000020983 ) ;
#111815 = B_SPLINE_CURVE_WITH_KNOTS ( 'NONE', 3,
 ( #10232, #7007, #42774, #77372, #140278, #142414 ),
 .UNSPECIFIED., .F., .F.,
 ( 4, 2, 4 ),
 ( 0.000000000000000000, 0.0003845013059668469482, 0.0007690026119336938965 ),
 .UNSPECIFIED. ) ;
#111816 = AXIS2_PLACEMENT_3D ( 'NONE', #63200, #148722, #127228 ) ;
#111817 = CARTESIAN_POINT ( 'NONE',  ( 1.803259461591859347, -1.743671650923955374, 1.101644963814436329 ) ) ;
#111818 = CARTESIAN_POINT ( 'NONE',  ( -7.043624497499477499, 8.176315654292865887, 1.199719254218450271 ) ) ;
#111819 = ORIENTED_EDGE ( 'NONE', *, *, #13980, .F. ) ;
#111821 = ADVANCED_FACE ( 'NONE', ( #164441 ), #165503, .T. ) ;
#111820 = CARTESIAN_POINT ( 'NONE',  ( -1.402160292154681736E-14, 1.368750000682821710, -1.732050807568863648 ) ) ;
#111822 = CARTESIAN_POINT ( 'NONE',  ( 3.954256261376987602, 0.6707706173689140794, 1.746330409709492937 ) ) ;
#111823 = CARTESIAN_POINT ( 'NONE',  ( 2.426026400502009128, -1.286032909179233297, -1.163566193670103832 ) ) ;
#111824 = CARTESIAN_POINT ( 'NONE',  ( 6.110890996357365879, -0.2699588104537915534, 2.174781792473476472 ) ) ;
#111825 = CARTESIAN_POINT ( 'NONE',  ( 0.4291286860223576527, 2.112415399404877547, 0.6383354507134838540 ) ) ;
#111826 = CARTESIAN_POINT ( 'NONE',  ( 4.487301133948972343, 1.932317252032596633, -0.9692046190768679459 ) ) ;
#111827 = CARTESIAN_POINT ( 'NONE',  ( 4.962805208576138938, 0.1888075513713943498, -1.932747541012701964 ) ) ;
#111828 = CARTESIAN_POINT ( 'NONE',  ( -3.267151830768952880, 5.795132321663641228, -1.082531754730549078 ) ) ;
#111829 = EDGE_CURVE ( 'NONE', #99756, #144460, #21866, .T. ) ;
#111830 = CARTESIAN_POINT ( 'NONE',  ( 6.450466390465378730, 0.5869013949594548141, 1.776180802621520005 ) ) ;
#111831 = CARTESIAN_POINT ( 'NONE',  ( 4.117415066209698438, 7.437700365148243620, 0.6807796091479866307 ) ) ;
#111832 = PLANE ( 'NONE',  #207600 ) ;
#111833 = CARTESIAN_POINT ( 'NONE',  ( 0.08834397731360790762, 1.226219587655341448, 1.729930300845914815 ) ) ;
#111834 = CARTESIAN_POINT ( 'NONE',  ( -0.6801582343750004478, 2.348958333674739052, -1.178068619123869398 ) ) ;
#111836 = CARTESIAN_POINT ( 'NONE',  ( 5.608046130584797950, -0.04667949407829303371, 2.016033753796213635 ) ) ;
#111835 = CIRCLE ( 'NONE', #132516, 0.08000000000000020983 ) ;
#111837 = CARTESIAN_POINT ( 'NONE',  ( -4.270455198180246548, 4.084545274072787890, 0.7216878364870317197 ) ) ;
#111838 = CARTESIAN_POINT ( 'NONE',  ( 6.421758314367153275, 10.64380180007036891, -0.7998128361456291469 ) ) ;
#111839 = CARTESIAN_POINT ( 'NONE',  ( 2.609770642201842072, -0.3830433331901555993, -0.1872689674646474400 ) ) ;
#111840 = CARTESIAN_POINT ( 'NONE',  ( 3.000428103051573814, -0.5303778429210231904, -1.746945217264872507 ) ) ;
#111841 = CARTESIAN_POINT ( 'NONE',  ( 2.538337413235943973, 1.040872164564849767, -1.945885072647230318 ) ) ;
#111842 = ORIENTED_EDGE ( 'NONE', *, *, #103265, .T. ) ;
#111843 = CARTESIAN_POINT ( 'NONE',  ( -3.960390268523300339, 7.634556056670224855, 1.214306433183764966E-14 ) ) ;
#111844 = CARTESIAN_POINT ( 'NONE',  ( 0.4000000000000045186, 3.950000000000022826, -1.561251128379126385E-14 ) ) ;
#111845 = CARTESIAN_POINT ( 'NONE',  ( -8.345207244411405156, 9.694828859023472134, 1.199719254218462483 ) ) ;
#111846 = CARTESIAN_POINT ( 'NONE',  ( 1.494405286683021306, -1.076835855708496936, 1.708581493997686662 ) ) ;
#111847 = CARTESIAN_POINT ( 'NONE',  ( 1.348456458401224412, 1.042098076042829780, -1.846665823592225975 ) ) ;
#111848 = AXIS2_PLACEMENT_3D ( 'NONE', #61095, #60025, #93620 ) ;
#111849 = CARTESIAN_POINT ( 'NONE',  ( -5.855142236255304944, 7.924361590421551860, -1.599625672291271394 ) ) ;
#111850 = CARTESIAN_POINT ( 'NONE',  ( 2.043593076603223757, 1.278923709890807503, 1.352104710524345554 ) ) ;
#111851 = CARTESIAN_POINT ( 'NONE',  ( 3.181359600701000989, 6.863336634126477875, 0.000000000000000000 ) ) ;
#111852 = CARTESIAN_POINT ( 'NONE',  ( 5.893449486436047380, 1.558864155394885875, 1.348126965055055804 ) ) ;
#111853 = CARTESIAN_POINT ( 'NONE',  ( 6.065077313367789102, -1.076319894221990259, 1.704936797084610101 ) ) ;
#111854 = ORIENTED_EDGE ( 'NONE', *, *, #91211, .F. ) ;
#111855 = ORIENTED_EDGE ( 'NONE', *, *, #187677, .F. ) ;
#111856 = CARTESIAN_POINT ( 'NONE',  ( 0.01493835450741834783, 6.487495393664098664, -3.100011470320001905 ) ) ;
#111857 = CARTESIAN_POINT ( 'NONE',  ( 4.494645072041675071, -0.4025399330690944133, -1.780595394402582077 ) ) ;
#111859 = CARTESIAN_POINT ( 'NONE',  ( -5.338497050760650176, 6.533440992188984886, -1.368045069562271010 ) ) ;
#111858 = CARTESIAN_POINT ( 'NONE',  ( -5.652823702255029836, 5.559658838911111900, -0.7998128361456362523 ) ) ;
#111860 = CARTESIAN_POINT ( 'NONE',  ( 5.770588788983777917, 7.358121641400980018, 1.301467365913897112 ) ) ;
#111861 = CARTESIAN_POINT ( 'NONE',  ( 6.538435458278026857, 1.930121188254026787, -0.5825698962980339068 ) ) ;
#111862 = CARTESIAN_POINT ( 'NONE',  ( 5.314338895140062746, 1.702579029208791450, 0.7012131971957940024 ) ) ;
#111863 = CARTESIAN_POINT ( 'NONE',  ( 0.07680821025394035662, 2.052785608010514018, -2.228496998325917744 ) ) ;
#111864 = CARTESIAN_POINT ( 'NONE',  ( 4.600386337014011673, -2.307077041318765342, -0.05981084109947519545 ) ) ;
#111865 = CARTESIAN_POINT ( 'NONE',  ( 4.206772801990143584, 8.129928378955675328, 0.7998128361456271485 ) ) ;
#111866 = CARTESIAN_POINT ( 'NONE',  ( 5.817692603468245238, -2.110333850551704415, 0.4673072906974176655 ) ) ;
#111867 = CARTESIAN_POINT ( 'NONE',  ( 7.657657833620182153, 7.828355648845348291, -0.7998128361456281477 ) ) ;
#111868 = CARTESIAN_POINT ( 'NONE',  ( 1.452572125225624955, -1.666495805118956897, -0.9969474394922008820 ) ) ;
#111869 = ORIENTED_EDGE ( 'NONE', *, *, #212623, .F. ) ;
#111870 = CARTESIAN_POINT ( 'NONE',  ( 4.657739267062822819, -0.4975208956916782332, -2.243777209869437517 ) ) ;
#111871 = CARTESIAN_POINT ( 'NONE',  ( -6.385527162356468445, 10.39360608948380538, 1.040834085586084257E-14 ) ) ;
#111872 = CARTESIAN_POINT ( 'NONE',  ( -5.178288325776719603, 5.006034233019745372, 0.000000000000000000 ) ) ;
#111873 = CARTESIAN_POINT ( 'NONE',  ( 4.961713530105988923, 1.850188064717460223, -0.2750520410098392654 ) ) ;
#111874 =( BOUNDED_CURVE ( )  B_SPLINE_CURVE ( 2, ( #111119, #56972, #73199, #40736, #28739, #209590, #94824 ),
 .UNSPECIFIED., .F., .T. ) 
 B_SPLINE_CURVE_WITH_KNOTS ( ( 3, 2, 2, 3 ),
 ( 0.1249999999999998612, 0.1309523809523809035, 0.1369047619047619735, 0.1428571428571429880 ),
 .UNSPECIFIED. ) 
 CURVE ( )  GEOMETRIC_REPRESENTATION_ITEM ( )  RATIONAL_B_SPLINE_CURVE ( ( 1.000000000000003109, 0.8660254037844355990, 1.000000000000000000, 0.8660254037844387076, 1.000000000000000000, 0.8660254037844355990, 1.000000000000003109 ) ) 
 REPRESENTATION_ITEM ( '' )  );
#111877 = CARTESIAN_POINT ( 'NONE',  ( -6.445975688654487001, 6.485002823043819475, -0.7998128361456362523 ) ) ;
#111876 = CARTESIAN_POINT ( 'NONE',  ( -1.500000000000013101, 0.4520833340161533598, 0.8660254037844403729 ) ) ;
#111875 = CARTESIAN_POINT ( 'NONE',  ( 1.951281838316549777, -1.706683157587106425, 0.8630329916254894096 ) ) ;
#111878 = CARTESIAN_POINT ( 'NONE',  ( 3.985166894971280183, -0.2153072539897090687, -2.196357064762343825 ) ) ;
#111879 = CARTESIAN_POINT ( 'NONE',  ( 6.883263157960333167, 4.698395927207251077, 2.408847447403542841 ) ) ;
#111880 = CARTESIAN_POINT ( 'NONE',  ( 2.381428537494710618, 5.930083727052461562, 0.7998128361456462443 ) ) ;
#111881 = CARTESIAN_POINT ( 'NONE',  ( 5.682275777458841048, 8.683053269460405232, 1.082531754730547524 ) ) ;
#111882 = CARTESIAN_POINT ( 'NONE',  ( -10.30827686509187835, 10.92074451889568643, 1.040834085586084257E-14 ) ) ;
#111883 = CARTESIAN_POINT ( 'NONE',  ( -5.261973015435229328, 9.153069261400824885, 0.000000000000000000 ) ) ;
#111884 = CARTESIAN_POINT ( 'NONE',  ( 1.423050710548888542, -0.05258038247234024520, 1.970828066091591557 ) ) ;
#111885 = CARTESIAN_POINT ( 'NONE',  ( 1.202667248822903989, -2.307758714249080079, 0.002725711325006137473 ) ) ;
#111886 = CARTESIAN_POINT ( 'NONE',  ( 2.822649888979886335, -1.354935067541668259, 1.419045635080482093 ) ) ;
#111887 = CARTESIAN_POINT ( 'NONE',  ( 0.000000000000000000, 0.6185895741317448682, 0.000000000000000000 ) ) ;
#111888 = CARTESIAN_POINT ( 'NONE',  ( 4.891499300893256574, -1.887858789894794054, 0.8311416006015391877 ) ) ;
#111889 = CARTESIAN_POINT ( 'NONE',  ( 4.026408433578586354, 7.641300905909586660, 1.040834085586084257E-14 ) ) ;
#111890 = CARTESIAN_POINT ( 'NONE',  ( 4.746236293235721604, 7.694970221153795364, 1.199719254218451159 ) ) ;
#111891 = ORIENTED_EDGE ( 'NONE', *, *, #155462, .F. ) ;
#111892 =( BOUNDED_CURVE ( )  B_SPLINE_CURVE ( 2, ( #90133, #138885, #204903, #56557, #122717, #205985, #213433, #60812, #96545 ),
 .UNSPECIFIED., .F., .T. ) 
 B_SPLINE_CURVE_WITH_KNOTS ( ( 3, 2, 2, 2, 3 ),
 ( 0.3906250000000001665, 0.3958333333333333148, 0.4062500000000000000, 0.4166666666666666852, 0.4218749999999998335 ),
 .UNSPECIFIED. ) 
 CURVE ( )  GEOMETRIC_REPRESENTATION_ITEM ( )  RATIONAL_B_SPLINE_CURVE ( ( 0.9330127018922194093, 0.9330127018922215187, 1.000000000000000000, 0.8660254037844387076, 1.000000000000000000, 0.8660254037844387076, 1.000000000000000000, 0.9330127018922215187, 0.9330127018922194093 ) ) 
 REPRESENTATION_ITEM ( '' )  );
#111893 = DIRECTION ( 'NONE',  ( -0.000000000000000000, -8.546850786086437571E-32, -1.000000000000000000 ) ) ;
#111894 = CARTESIAN_POINT ( 'NONE',  ( 10.72180055030867329, 11.40318881831530540, 0.7998128361456341429 ) ) ;
#111895 = CARTESIAN_POINT ( 'NONE',  ( 1.112457285868488910, 2.168641027238225938, -0.1045176843600063021 ) ) ;
#111896 = CARTESIAN_POINT ( 'NONE',  ( 5.367048706163316751, 7.354919138647580290, -1.599625672291281386 ) ) ;
#111897 = EDGE_CURVE ( 'NONE', #209619, #84144, #194679, .T. ) ;
#111898 = CARTESIAN_POINT ( 'NONE',  ( 6.773376349081638104, -7.645986912801321367, 6.661184041422480107 ) ) ;
#111899 = CARTESIAN_POINT ( 'NONE',  ( -4.042674711113225960, 3.868317915292367015, -2.500000000000000444 ) ) ;
#111900 = CARTESIAN_POINT ( 'NONE',  ( 2.336979506217982117, -1.672866993182718698, 0.8370366242000035761 ) ) ;
#111901 = CARTESIAN_POINT ( 'NONE',  ( 6.679002375395027613, -0.09866081283815136826, -2.159460157733564145 ) ) ;
#111903 = SURFACE_STYLE_USAGE ( .BOTH. , #62020 ) ;
#111902 = CARTESIAN_POINT ( 'NONE',  ( 0.07755575628183573877, 1.996246338214379801, -2.602582295553407032 ) ) ;
#111904 = CARTESIAN_POINT ( 'NONE',  ( 1.364683531249988757, -0.6156249996585803075, 0.000000000000000000 ) ) ;
#111905 =( BOUNDED_SURFACE ( )  B_SPLINE_SURFACE ( 3, 2, ( 
 ( #179719, #213251, #132067 ),
 ( #17182, #31336, #163468 ),
 ( #65920, #97413, #15048 ),
 ( #115834, #81141, #198078 ) ),
 .UNSPECIFIED., .F., .F., .F. ) 
 B_SPLINE_SURFACE_WITH_KNOTS ( ( 4, 4 ),
 ( 3, 3 ),
 ( 0.06089817005132014405, 0.06334004685008763624 ),
 ( 0.000000000000000000, 1.000000000000000000 ),
 .UNSPECIFIED. ) 
 GEOMETRIC_REPRESENTATION_ITEM ( )  RATIONAL_B_SPLINE_SURFACE ( (
 ( 1.000000000000000000, 0.7169883299104516938, 1.000000000000000000),
 ( 1.000000000000000000, 0.7174882367719587206, 1.000000000000000000),
 ( 1.000000000000000000, 0.7180609655865445307, 1.000000000000000000),
 ( 1.000000000000000000, 0.7187540731123146509, 1.000000000000000000) ) ) 
 REPRESENTATION_ITEM ( '' )  SURFACE ( )  );
#111906 = CARTESIAN_POINT ( 'NONE',  ( 2.402860538037488780, -0.3286879766849961082, -1.883663324302800257 ) ) ;
#111907 = PRESENTATION_LAYER_ASSIGNMENT (  '', '', ( #15000 ) ) ;
#111908 = CARTESIAN_POINT ( 'NONE',  ( 3.889309559433737906, 1.281865973830035754, 1.220554204183731173 ) ) ;
#111909 = CARTESIAN_POINT ( 'NONE',  ( 2.314975094136799694, 1.534822137071165660, -1.140449143091977646 ) ) ;
#111910 = CIRCLE ( 'NONE', #101462, 0.07999999999999998779 ) ;
#111911 = CARTESIAN_POINT ( 'NONE',  ( -4.717347382551060342, 7.590990148696470818, 1.199719254218464037 ) ) ;
#111913 = CARTESIAN_POINT ( 'NONE',  ( 5.642171489992906075, 0.7808347329528000369, 1.749441798972359408 ) ) ;
#111912 = FACE_OUTER_BOUND ( 'NONE', #171477, .T. ) ;
#111914 = CARTESIAN_POINT ( 'NONE',  ( -1.500000000000015099, -0.8291666666666407393, 0.8660254037844403729 ) ) ;
#111915 = CARTESIAN_POINT ( 'NONE',  ( 6.391062254520311292, 0.1913994329204322109, 1.960204640275018395 ) ) ;
#111916 = CARTESIAN_POINT ( 'NONE',  ( 1.499999999999987121, 4.795833333333353821, -0.8660254037844323793 ) ) ;
#111917 = CARTESIAN_POINT ( 'NONE',  ( -1.420000000000001039, 6.120000000000041851, -2.499999999999995115 ) ) ;
#111918 = CARTESIAN_POINT ( 'NONE',  ( 4.979306205331720747, 1.745251617482036943, -0.6738592683939447214 ) ) ;
#111920 = ORIENTED_EDGE ( 'NONE', *, *, #80961, .T. ) ;
#111919 = CARTESIAN_POINT ( 'NONE',  ( 1.681982107312831154, -0.9779208310041755947, 1.541497997293653555 ) ) ;
#111922 = CARTESIAN_POINT ( 'NONE',  ( 4.601545839464173504, 8.365386937211251706, 0.1680730238927778675 ) ) ;
#111921 = CARTESIAN_POINT ( 'NONE',  ( 4.688207069967821106, -1.042061291317699423, 1.945354640606362873 ) ) ;
#111923 = CARTESIAN_POINT ( 'NONE',  ( 0.6823417656249864960, -0.8239583329919114574, -1.181850606188749264 ) ) ;
#111924 = CARTESIAN_POINT ( 'NONE',  ( 1.891156856157749866, 0.2001100897341882012, 2.052929594394680812 ) ) ;
#111925 = CARTESIAN_POINT ( 'NONE',  ( 4.625302960556422427, 8.547937220624488575, 1.040834085586084257E-14 ) ) ;
#111926 = CARTESIAN_POINT ( 'NONE',  ( -7.666245793523398078, 11.03137162816423356, 1.199719254218453823 ) ) ;
#111927 = CARTESIAN_POINT ( 'NONE',  ( 1.318127287744129683, 3.538098647990162604, 0.3960634941688977451 ) ) ;
#111928 = CARTESIAN_POINT ( 'NONE',  ( 7.777967379493318845, -5.907420853759296264, 7.664830294503448549 ) ) ;
#111929 = CARTESIAN_POINT ( 'NONE',  ( 5.668190738965027897, 8.770583741171307679, -1.199719254218452047 ) ) ;
#111930 = EDGE_LOOP ( 'NONE', ( #23712, #205121, #103905, #134462 ) ) ;
#111931 = CARTESIAN_POINT ( 'NONE',  ( 5.512195382060368409, 2.068158883198469855, -0.09793725168850964113 ) ) ;
#111932 = CARTESIAN_POINT ( 'NONE',  ( -1.364683531250014514, -0.9072916663252470482, 0.7879004041258379498 ) ) ;
#111933 = CARTESIAN_POINT ( 'NONE',  ( 2.565889408427945995, 2.120439650033152379, -0.4189318973958494619 ) ) ;
#111934 = CARTESIAN_POINT ( 'NONE',  ( -4.699286343732877569, 8.265425651823845143, 0.5948934201362279239 ) ) ;
#111935 = CARTESIAN_POINT ( 'NONE',  ( 3.369790118769320664, 0.4886731666619185677, -1.959541563195909220 ) ) ;
#111936 = CARTESIAN_POINT ( 'NONE',  ( 6.620655732516651071, 1.241313378043694238, 2.288056600130850882 ) ) ;
#111937 = VERTEX_POINT ( 'NONE', #111494 ) ;
#111938 = EDGE_CURVE ( 'NONE', #113870, #123257, #76707, .T. ) ;
#111940 = CARTESIAN_POINT ( 'NONE',  ( 7.809133291791403586, 8.213003049952529722, -0.7216878364870257245 ) ) ;
#111939 = CARTESIAN_POINT ( 'NONE',  ( 0.000000000000000000, -1.487500000000001599, -4.012584370867899430 ) ) ;
#111941 = CARTESIAN_POINT ( 'NONE',  ( -5.126391479298592735, 5.153413945369351268, 0.000000000000000000 ) ) ;
#111942 = CARTESIAN_POINT ( 'NONE',  ( 1.428923106112218067, -1.700960256238340573, 1.082842518468102089 ) ) ;
#111943 = CARTESIAN_POINT ( 'NONE',  ( 6.497619750234602698, -2.191128968173004843, 0.05151875470104508997 ) ) ;
#111944 = CARTESIAN_POINT ( 'NONE',  ( 0.7499999999999920064, 5.014583334016150751, 1.299038105676669330 ) ) ;
#111945 = CARTESIAN_POINT ( 'NONE',  ( 4.482611839828003930, -1.244964735940889522, 1.451779576051547282 ) ) ;
#111946 = CARTESIAN_POINT ( 'NONE',  ( -3.253066792275140173, 5.882662793374543675, 1.199719254218462483 ) ) ;
#111947 = CARTESIAN_POINT ( 'NONE',  ( 7.443063143778065438, 7.785921210603627962, -0.7216878364870257245 ) ) ;
#111949 = CARTESIAN_POINT ( 'NONE',  ( 2.249625261780491936, 1.976952429928409805, -0.3961248688731587309 ) ) ;
#111948 = CARTESIAN_POINT ( 'NONE',  ( -8.961576348508641487, 11.47825837805867799, -1.443375672974058777 ) ) ;
#111950 = CARTESIAN_POINT ( 'NONE',  ( -1.364683531250010295, 13.69270833367473195, 0.7879004041258445001 ) ) ;
#111951 = CARTESIAN_POINT ( 'NONE',  ( -4.950662367645459305, 5.804802846121667415, -1.199719254218453823 ) ) ;
#111952 = CARTESIAN_POINT ( 'NONE',  ( 4.981344092214620822, 1.608381032133517019, -0.6233497484429885160 ) ) ;
#111953 = CARTESIAN_POINT ( 'NONE',  ( 6.933015448541703485, 9.181880338089085214, 1.599625672291268286 ) ) ;
#111954 = CARTESIAN_POINT ( 'NONE',  ( 9.083599731475976213, 12.58098820582193689, 1.082531754730546636 ) ) ;
#111955 = CARTESIAN_POINT ( 'NONE',  ( -2.550000000000000266, 2.499999999999998668, -1.849324200890692271 ) ) ;
#111956 = FACE_OUTER_BOUND ( 'NONE', #61888, .T. ) ;
#111958 =( BOUNDED_SURFACE ( )  B_SPLINE_SURFACE ( 3, 2, ( 
 ( #201359, #168883, #104976 ),
 ( #171017, #154781, #20487 ),
 ( #204559, #3155, #56207 ),
 ( #136408, #69226, #35678 ) ),
 .UNSPECIFIED., .F., .F., .T. ) 
 B_SPLINE_SURFACE_WITH_KNOTS ( ( 4, 4 ),
 ( 3, 3 ),
 ( 0.000000000000000000, 3.124390133962058787E-05 ),
 ( 0.000000000000000000, 1.000000000000000000 ),
 .UNSPECIFIED. ) 
 GEOMETRIC_REPRESENTATION_ITEM ( )  RATIONAL_B_SPLINE_SURFACE ( (
 ( 1.000000000000000000, 0.7100530722023771224, 1.000000000000000000),
 ( 1.000000000000000000, 0.7100778649077736926, 1.000000000000000000),
 ( 1.000000000000000000, 0.7091082185075937572, 1.000000000000000000),
 ( 1.000000000000000000, 0.7071067811862440378, 1.000000000000000000) ) ) 
 REPRESENTATION_ITEM ( '' )  SURFACE ( )  );
#111957 = CARTESIAN_POINT ( 'NONE',  ( 1.481394567461959300, -0.05474761849930119550, 2.069712792878583230 ) ) ;
#111959 = CARTESIAN_POINT ( 'NONE',  ( 6.760220206081136496, -2.069995208266177666, 0.04663682477341199450 ) ) ;
#111960 = ORIENTED_EDGE ( 'NONE', *, *, #12966, .T. ) ;
#111961 = CARTESIAN_POINT ( 'NONE',  ( 4.705596528438695358, 1.345619282010660500, 1.212945642518966416 ) ) ;
#111962 = CARTESIAN_POINT ( 'NONE',  ( 5.554000203453580475, 6.508696987897830688, -1.199719254218452047 ) ) ;
#111963 = FACE_OUTER_BOUND ( 'NONE', #81415, .T. ) ;
#111964 = CARTESIAN_POINT ( 'NONE',  ( 6.305303276254960565, 1.572402219250234268, -0.8993151100721032964 ) ) ;
#111965 = CARTESIAN_POINT ( 'NONE',  ( 6.007671464186837618, 6.181573927739029806, 0.7216878364870328300 ) ) ;
#111966 = CARTESIAN_POINT ( 'NONE',  ( -15.75000000000000000, 11.29999999999998117, 1.799999999999999600 ) ) ;
#111967 = CARTESIAN_POINT ( 'NONE',  ( 3.152458698460915532, -1.659165413833121550, 1.431739491984926671 ) ) ;
#111968 = VERTEX_POINT ( 'NONE', #33366 ) ;
#111969 = EDGE_CURVE ( 'NONE', #155662, #97860, #211035, .T. ) ;
#111971 = CARTESIAN_POINT ( 'NONE',  ( 8.483651433849084711, 10.92067931095586886, 1.599625672291281386 ) ) ;
#111970 = CARTESIAN_POINT ( 'NONE',  ( 0.9066075625437097774, 0.5660373911110065936, 1.878450800843839419 ) ) ;
#111972 = VECTOR ( 'NONE', #151798, 1000.000000000000000 ) ;
#111973 = CARTESIAN_POINT ( 'NONE',  ( 4.464398116780900594, -1.859039872360370937, -0.4615888831297955686 ) ) ;
#111974 = AXIS2_PLACEMENT_3D ( 'NONE', #27235, #155126, #6708 ) ;
#111975 = CARTESIAN_POINT ( 'NONE',  ( -1.500000000000021982, 7.438721522839123246, 4.195160983902633589 ) ) ;
#111976 = FILL_AREA_STYLE_COLOUR ( '', #53439 ) ;
#111977 = CARTESIAN_POINT ( 'NONE',  ( -0.6823417656250003738, -0.7822916663252423852, -1.181850606188749264 ) ) ;
#111978 = CIRCLE ( 'NONE', #125899, 0.1999999999999996503 ) ;
#111979 = CARTESIAN_POINT ( 'NONE',  ( 5.260200412422194383, 7.159986452624450770, -1.443375672974051449 ) ) ;
#111980 = CARTESIAN_POINT ( 'NONE',  ( -8.920901888112002354, 11.43080484092926241, 1.443375672974064550 ) ) ;
#111981 = CARTESIAN_POINT ( 'NONE',  ( 2.395597313961893349, 1.670541196947441742, 1.371929806955954234 ) ) ;
#111982 = CARTESIAN_POINT ( 'NONE',  ( -5.646044625448194410, 5.551749915969804938, 0.000000000000000000 ) ) ;
#111983 = CARTESIAN_POINT ( 'NONE',  ( 5.727393547130178675, 5.646656991265468939, 0.000000000000000000 ) ) ;
#111984 = CARTESIAN_POINT ( 'NONE',  ( 1.817148636465517164, -0.2269042555285011864, 1.811363274943120771 ) ) ;
#111985 = CARTESIAN_POINT ( 'NONE',  ( 0.0004480315400831600455, -0.9938866557669153723, 1.873244595478529728 ) ) ;
#111986 = CARTESIAN_POINT ( 'NONE',  ( 4.137589658204786858, -1.258905094989382967, -1.322318538811013466 ) ) ;
#111987 = AXIS2_PLACEMENT_3D ( 'NONE', #205270, #156557, #203135 ) ;
#111988 = CARTESIAN_POINT ( 'NONE',  ( 9.272303875213562918, 13.02406837586111443, -8.983758935644893029 ) ) ;
#111989 = ORIENTED_EDGE ( 'NONE', *, *, #50440, .F. ) ;
#111990 = CARTESIAN_POINT ( 'NONE',  ( 3.350016042381760872, -0.8005406348832925234, 1.799716665148870964 ) ) ;
#111991 = VERTEX_POINT ( 'NONE', #112557 ) ;
#111992 = CARTESIAN_POINT ( 'NONE',  ( 6.550339418841141459, -1.498220820903242601, 1.235316290203094081 ) ) ;
#111993 = ORIENTED_EDGE ( 'NONE', *, *, #160843, .T. ) ;
#111994 = CARTESIAN_POINT ( 'NONE',  ( -7.422162748838431412, 7.623887726591770608, -0.7998128361456362523 ) ) ;
#111996 = CARTESIAN_POINT ( 'NONE',  ( 5.308877466510794285, -0.5174029350529658622, -2.056363676157816123 ) ) ;
#111995 = CARTESIAN_POINT ( 'NONE',  ( 5.318541398310776103, 9.426991741329731056, -0.7998128361456481317 ) ) ;
#111997 = CARTESIAN_POINT ( 'NONE',  ( 6.658462837642789012, 9.821938173008357253, 1.082531754730549078 ) ) ;
#111999 = VERTEX_POINT ( 'NONE', #178569 ) ;
#111998 = CARTESIAN_POINT ( 'NONE',  ( 3.106014470790594562, -0.7728303494197851231, 1.749331318715248385 ) ) ;
#112000 = CARTESIAN_POINT ( 'NONE',  ( 4.581598608702507569, 7.168929433314090716, -1.325851593340146461 ) ) ;
#112001 = DIRECTION ( 'NONE',  ( 0.000000000000000000, 0.000000000000000000, -1.000000000000000000 ) ) ;
#112002 = FACE_OUTER_BOUND ( 'NONE', #51325, .T. ) ;
#112003 = CARTESIAN_POINT ( 'NONE',  ( 4.758451920691616266, 2.007841679651333422, 0.1459793341078066131 ) ) ;
#112004 = CARTESIAN_POINT ( 'NONE',  ( -4.946829630374642406, 6.829763058803005826, -1.486263735186076129 ) ) ;
#112005 = CARTESIAN_POINT ( 'NONE',  ( 6.358013415952256331, 1.820405254634300363, -0.1396899356524081148 ) ) ;
#112006 = CARTESIAN_POINT ( 'NONE',  ( 1.012269475826784060, 2.068064858651061932, -0.09981174449213289779 ) ) ;
#112007 = CARTESIAN_POINT ( 'NONE',  ( -6.710922849084449915, 10.77323439066645783, 0.000000000000000000 ) ) ;
#112008 = CARTESIAN_POINT ( 'NONE',  ( -5.962047440371475382, 7.122956488241998230, -1.095284208787988822 ) ) ;
#112009 = CARTESIAN_POINT ( 'NONE',  ( -0.6125000000000175859, 2.104166667349471886, 1.060881119635908476 ) ) ;
#112010 = CARTESIAN_POINT ( 'NONE',  ( 6.385618529757402406, 1.291587659170100766, 1.353439767483602285 ) ) ;
#112011 = CARTESIAN_POINT ( 'NONE',  ( 5.425234023762710578, 9.481190127698507553, -0.7998128361456291469 ) ) ;
#112012 = CARTESIAN_POINT ( 'NONE',  ( -4.731959306369413198, 5.479372931307791461, -1.199719254218446718 ) ) ;
#112013 = CARTESIAN_POINT ( 'NONE',  ( -8.012344526598182026E-15, 11.10937500034139802, -1.575800808251669460 ) ) ;
#112014 = CARTESIAN_POINT ( 'NONE',  ( -4.786191920824102830, 5.542644314838231168, 1.199719254218462483 ) ) ;
#112016 = CARTESIAN_POINT ( 'NONE',  ( -6.420668264523499147, 9.648474187656182366, 1.199719254218452935 ) ) ;
#112015 = PRESENTATION_STYLE_ASSIGNMENT (( #27482 ) ) ;
#112017 = CARTESIAN_POINT ( 'NONE',  ( 4.219182763733449804, 1.701723821253621427, 0.3326838626578206282 ) ) ;
#112018 = CARTESIAN_POINT ( 'NONE',  ( -3.255929445576174697, 6.950334786480840243, -0.7998128361456281477 ) ) ;
#112019 = CARTESIAN_POINT ( 'NONE',  ( 1.534126288888465917, 1.230018689141991306, 1.665114864061276734 ) ) ;
#112020 = CARTESIAN_POINT ( 'NONE',  ( 2.847379581703746609, 0.3079039886237054935, -2.094596350150164987 ) ) ;
#112021 = CARTESIAN_POINT ( 'NONE',  ( 5.301401758143367893, 6.143722458377430584, 1.199719254218462483 ) ) ;
#112022 = CARTESIAN_POINT ( 'NONE',  ( 8.697719238366680372, 10.10609285197134533, 1.199719254218462483 ) ) ;
#112023 = CARTESIAN_POINT ( 'NONE',  ( 0.000000000000000000, 3.466143782776612170, 0.000000000000000000 ) ) ;
#112024 = CARTESIAN_POINT ( 'NONE',  ( 0.9363041846261275225, -1.098647377812447923, 1.634312829373037568 ) ) ;
#112025 = CARTESIAN_POINT ( 'NONE',  ( 4.197832665289490173, 7.575126408543901846, 0.9117821302269245587 ) ) ;
#112026 = CARTESIAN_POINT ( 'NONE',  ( 3.538314903486612817, 7.071858454135611538, 1.040834085586084257E-14 ) ) ;
#112028 = CARTESIAN_POINT ( 'NONE',  ( 0.000000000000000000, 0.08000000000000020983, 0.000000000000000000 ) ) ;
#112027 = CARTESIAN_POINT ( 'NONE',  ( 1.737500000000001155, -1.983333333333333393, 3.009438278150922130 ) ) ;
#112029 = CARTESIAN_POINT ( 'NONE',  ( 3.135043019019596144, -2.021410203770683367, 1.080917199049796107 ) ) ;
#112030 = CARTESIAN_POINT ( 'NONE',  ( 0.8908993799596062191, 1.611356928563783208, -0.8583080905386344384 ) ) ;
#112031 = CARTESIAN_POINT ( 'NONE',  ( 3.498220628606643956, -0.9384276995785534314, 1.666209768436441419 ) ) ;
#112032 = CARTESIAN_POINT ( 'NONE',  ( 4.667750024854814050, 8.667735138964429709, -0.7998128361456381397 ) ) ;
#112034 = EDGE_CURVE ( 'NONE', #138713, #105777, #8037, .T. ) ;
#112033 = CARTESIAN_POINT ( 'NONE',  ( 6.602457619730749627, 10.64669162308715222, 0.7216878364870438212 ) ) ;
#112035 = CARTESIAN_POINT ( 'NONE',  ( -9.508345801885592863, 9.987491611821676329, 0.7998128361456462443 ) ) ;
#112036 = CARTESIAN_POINT ( 'NONE',  ( 2.285404485177256362, 0.09469097253389560653, -2.011075120970148511 ) ) ;
#112037 = CARTESIAN_POINT ( 'NONE',  ( 2.641395077882053410, 1.795597516233004232, -0.7905247784146393064 ) ) ;
#112038 = CARTESIAN_POINT ( 'NONE',  ( -7.797910906154257304, 12.24931315715533486, 0.000000000000000000 ) ) ;
#112039 = ADVANCED_BREP_SHAPE_REPRESENTATION ( '', ( #156054, #200407 ), #83064 ) ;
#112040 = CARTESIAN_POINT ( 'NONE',  ( -6.581593504430098385, 9.765943957555402122, -1.199719254218440723 ) ) ;
#112041 = CARTESIAN_POINT ( 'NONE',  ( -10.84254087577847869, 4.919568073182958301, 5.035408296252059657 ) ) ;
#112043 = CARTESIAN_POINT ( 'NONE',  ( 3.414700241993049001, 1.599697164860384380, 0.7574896018788888075 ) ) ;
#112042 = CARTESIAN_POINT ( 'NONE',  ( 4.822261998019022222, 2.000437409348213347, 0.6074620046824655839 ) ) ;
#112044 = CARTESIAN_POINT ( 'NONE',  ( -8.065673738752591859, 14.99999998464884854, 8.613976760015685130 ) ) ;
#112046 = CARTESIAN_POINT ( 'NONE',  ( 6.632792736454030447, -2.050728487082712270, 1.024446431767987331 ) ) ;
#112045 = CARTESIAN_POINT ( 'NONE',  ( 1.458253848507185202, 8.740113170334296910, -2.549233421402206101 ) ) ;
#112047 = CARTESIAN_POINT ( 'NONE',  ( 4.945099085969404840, 0.5415675326034079529, -1.653987846916603610 ) ) ;
#112048 = CARTESIAN_POINT ( 'NONE',  ( 7.567422294721922960, 11.98040977715095323, 0.7998128361456462443 ) ) ;
#112049 = CARTESIAN_POINT ( 'NONE',  ( 4.147546876296400065, -0.1688817038796013026, -1.725555368340276008 ) ) ;
#112050 = VECTOR ( 'NONE', #37035, 1000.000000000000000 ) ;
#112051 = CARTESIAN_POINT ( 'NONE',  ( 4.756392321286846858, -2.170573799849393470, -0.05792142139850359195 ) ) ;
#112052 = CARTESIAN_POINT ( 'NONE',  ( 4.356247428692526569, 3.976710176429713250, 0.7998128361456341429 ) ) ;
#112053 = CARTESIAN_POINT ( 'NONE',  ( 5.630092293170263495, 2.014432788975322630, 0.09412139267171715229 ) ) ;
#112054 = CARTESIAN_POINT ( 'NONE',  ( 5.375000000000002665, 2.052068128417941395, -3.059081846666863488E-13 ) ) ;
#112055 = CARTESIAN_POINT ( 'NONE',  ( 0.7499999999999920064, 5.264583334016151639, 1.299038105676669330 ) ) ;
#112056 = CARTESIAN_POINT ( 'NONE',  ( 3.258729403965909821, -1.459781800624770032, 1.257100956980856443 ) ) ;
#112057 = CARTESIAN_POINT ( 'NONE',  ( -1.500000000000001110, 9.552083334016128191, 0.8660254037844419273 ) ) ;
#112058 = CARTESIAN_POINT ( 'NONE',  ( 6.521772982575972044, -0.4919494239215887466, 2.174507958589830370 ) ) ;
#112059 = EDGE_LOOP ( 'NONE', ( #194903, #205919, #16256, #82854 ) ) ;
#112060 = CARTESIAN_POINT ( 'NONE',  ( 6.883263157960369583, 7.629137130509070275, 2.546189081643289942 ) ) ;
#112061 = CARTESIAN_POINT ( 'NONE',  ( 1.499999999999989120, 2.504166666666687302, 0.8660254037844524744 ) ) ;
#112062 = CARTESIAN_POINT ( 'NONE',  ( 6.311484202361478779, 7.322151976631905868, -1.199719254218446718 ) ) ;
#112063 = CARTESIAN_POINT ( 'NONE',  ( 3.088771134150660735, -1.321542420002120855, 1.785288483701172657 ) ) ;
#112064 = CARTESIAN_POINT ( 'NONE',  ( 4.350813900535696277, 4.000456626940672500, 0.2320863031703649382 ) ) ;
#112065 = CARTESIAN_POINT ( 'NONE',  ( 8.446366511633696561, 8.956441806435218922, 1.040834085586084257E-14 ) ) ;
#112066 = CARTESIAN_POINT ( 'NONE',  ( -10.61567108937589765, 11.48729714713446803, 0.7216878364870438212 ) ) ;
#112067 = CARTESIAN_POINT ( 'NONE',  ( 3.040771591214902259, 6.769593633051179005, -0.7998128361456362523 ) ) ;
#112068 = CARTESIAN_POINT ( 'NONE',  ( 0.5103889644224939293, -1.913802852362625151, 0.6352017490645140985 ) ) ;
#112070 = CARTESIAN_POINT ( 'NONE',  ( 5.617653825673187384, 0.4058615334493093085, -2.022196393678155957 ) ) ;
#112069 = CARTESIAN_POINT ( 'NONE',  ( 8.402302512167096893, 10.82577223566020841, -1.599625672291268286 ) ) ;
#112071 = DIRECTION ( 'NONE',  ( -0.2684563758389304500, -5.222015543130708508E-15, 0.9632918427306581544 ) ) ;
#112072 = CARTESIAN_POINT ( 'NONE',  ( -4.277761160311629673, 4.949475094240346706, 1.199719254218462483 ) ) ;
#112074 = EDGE_CURVE ( 'NONE', #47959, #26714, #30324, .T. ) ;
#112073 = CARTESIAN_POINT ( 'NONE',  ( 1.499999999999991118, 5.535416667349481123, 0.8660254037844524744 ) ) ;
#112075 = CARTESIAN_POINT ( 'NONE',  ( -1.364683531250000748, 1.509375000341421691, 0.000000000000000000 ) ) ;
#112076 = CARTESIAN_POINT ( 'NONE',  ( 6.731728662460410462, -1.222180481402233898, -1.416172877279207931 ) ) ;
#112077 = CARTESIAN_POINT ( 'NONE',  ( 5.660742353926829118, 1.040242247344788762, 1.387327330804826619 ) ) ;
#112078 = CARTESIAN_POINT ( 'NONE',  ( 5.108843383178156117, -0.2480618215125965365, 1.722539690991312877 ) ) ;
#112079 = CARTESIAN_POINT ( 'NONE',  ( 3.298623631688667235, 1.806097335442503393, -1.411605728516792002 ) ) ;
#112080 = CARTESIAN_POINT ( 'NONE',  ( -1.364683531250014514, -0.9697916663252473812, 0.7879004041258379498 ) ) ;
#112081 = CARTESIAN_POINT ( 'NONE',  ( 0.9723034553027898319, -0.04304006056080753040, -1.840805954149108858 ) ) ;
#112082 = EDGE_CURVE ( 'NONE', #135468, #99737, #125740, .T. ) ;
#112083 = CARTESIAN_POINT ( 'NONE',  ( -9.336326716892651589, -1.000000000000000888, 2.500000000000000444 ) ) ;
#112084 = FILL_AREA_STYLE ('',( #146672 ) ) ;
#112085 = CARTESIAN_POINT ( 'NONE',  ( 1.571042225754931465, 0.1381101175703668971, -1.820421783975199048 ) ) ;
#112086 = CARTESIAN_POINT ( 'NONE',  ( 3.059220373557011818, -1.198860207862334049, 1.621182619130703051 ) ) ;
#112087 = CARTESIAN_POINT ( 'NONE',  ( 0.9201892814816802213, 1.302667801055312990, -1.762099327409505811 ) ) ;
#112088 = CARTESIAN_POINT ( 'NONE',  ( 9.885616400973860962, 14.58603459789345891, -7.683487713304058886 ) ) ;
#112089 = CARTESIAN_POINT ( 'NONE',  ( 4.647555896809190124, -1.626162052001564717, -1.338137134695188468 ) ) ;
#112090 = CARTESIAN_POINT ( 'NONE',  ( -6.632963465583701534, 8.761543347979550589, -1.599625672291263179 ) ) ;
#112091 = CARTESIAN_POINT ( 'NONE',  ( 8.248303390504895916, 13.81254849593766565, 9.579712001821075518 ) ) ;
#112092 = CARTESIAN_POINT ( 'NONE',  ( 1.785682506433339478, -1.950172559450613852, 0.6955597780969878796 ) ) ;
#112093 = CARTESIAN_POINT ( 'NONE',  ( 5.952193131599331721, 6.902979060742733708, 1.199719254218462483 ) ) ;
#112094 = CARTESIAN_POINT ( 'NONE',  ( -0.6801582343750074422, -0.1197916663252529546, -1.178068619123865846 ) ) ;
#112095 = CARTESIAN_POINT ( 'NONE',  ( 4.811248821985151913, 1.762591750878339081, -1.178568461981117643 ) ) ;
#112096 = CARTESIAN_POINT ( 'NONE',  ( 0.1176308287326099516, -1.889623933557175617, 0.3742946393059803367 ) ) ;
#112097 = ORIENTED_EDGE ( 'NONE', *, *, #169486, .F. ) ;
#112098 = CARTESIAN_POINT ( 'NONE',  ( -6.168033539574333979, 6.160736982450306876, 0.7998128361456281477 ) ) ;
#112099 = CARTESIAN_POINT ( 'NONE',  ( -11.41157692552970815, 11.25910337086999924, -3.404533818002362100 ) ) ;
#112100 = CARTESIAN_POINT ( 'NONE',  ( 5.167065940139554669, 9.042344340222555843, -0.7216878364870458196 ) ) ;
#112101 = CARTESIAN_POINT ( 'NONE',  ( -1.737500000000000266, -2.114583332377416802, -3.009438278150923907 ) ) ;
#112102 = CARTESIAN_POINT ( 'NONE',  ( -3.730464822054482710, 7.503959392372201442, 1.040834085586084257E-14 ) ) ;
#112103 = CARTESIAN_POINT ( 'NONE',  ( -0.05205951232617207075, -2.027416208471942038, 0.9083432681902519068 ) ) ;
#112104 = CARTESIAN_POINT ( 'NONE',  ( 1.008971530259877403, 1.594680585555088292, -1.375637761830387440 ) ) ;
#112105 = CARTESIAN_POINT ( 'NONE',  ( -6.317173229324657413, 6.334733287159020954, 0.000000000000000000 ) ) ;
#112106 = CARTESIAN_POINT ( 'NONE',  ( 9.053093885623066939, 11.58502883802551153, -1.599625672291262513 ) ) ;
#112107 = CARTESIAN_POINT ( 'NONE',  ( 5.401151054173385369, -1.597185415876556158, 0.9547389691558528790 ) ) ;
#112108 = CARTESIAN_POINT ( 'NONE',  ( 8.914649696185335870, 10.35917838609310593, -1.199719254218446718 ) ) ;
#112109 = CARTESIAN_POINT ( 'NONE',  ( -0.4339943706424748138, 3.986694575294704723, 0.4851827343914845714 ) ) ;
#112110 = EDGE_CURVE ( 'NONE', #8134, #20648, #11539, .T. ) ;
#112111 = CARTESIAN_POINT ( 'NONE',  ( -3.122120512896910505, 6.864500708346841229, 0.7998128361456352531 ) ) ;
#112112 = CARTESIAN_POINT ( 'NONE',  ( -8.351459436338023679, 12.68719374246231624, -0.7216878364870267237 ) ) ;
#112114 = CARTESIAN_POINT ( 'NONE',  ( 2.014041202081144011, 1.956828179156915315, -0.1411808619533050091 ) ) ;
#112113 = CARTESIAN_POINT ( 'NONE',  ( -7.881367368245678406, 8.089350105908421185, 0.7998128361456602331 ) ) ;
#112115 = CARTESIAN_POINT ( 'NONE',  ( 1.094844843509492183, -0.5259716649698794599, -2.096624219460433647 ) ) ;
#112117 = CARTESIAN_POINT ( 'NONE',  ( -5.998154408198820953, 6.083692137903044639, 0.6724663025347333845 ) ) ;
#112116 = CARTESIAN_POINT ( 'NONE',  ( -6.459533842268148973, 6.500820668926428958, 0.000000000000000000 ) ) ;
#112118 = CARTESIAN_POINT ( 'NONE',  ( -1.364683531250000748, -0.2406249996585799189, 0.000000000000000000 ) ) ;
#112119 = CARTESIAN_POINT ( 'NONE',  ( 2.547823072707461112, 1.587006686370129316, -0.6987220570618419835 ) ) ;
#112120 = CARTESIAN_POINT ( 'NONE',  ( 2.659766076405935653, -1.200293992427956757, 1.260412480424155435 ) ) ;
#112121 = CARTESIAN_POINT ( 'NONE',  ( 5.978782553946477840, 9.919070713005490703, 1.040834085586084257E-14 ) ) ;
#112122 = CARTESIAN_POINT ( 'NONE',  ( -10.96033999287893224, 4.843182460328104177, 4.379153535238802242 ) ) ;
#112123 = CARTESIAN_POINT ( 'NONE',  ( 0.7376574009502723239, -1.897405874265755354, -0.6818954202830117550 ) ) ;
#112124 = CARTESIAN_POINT ( 'NONE',  ( 6.825078400183550720, 0.5766433668599518780, 2.097246334241170906 ) ) ;
#112126 = MECHANICAL_DESIGN_GEOMETRIC_PRESENTATION_REPRESENTATION (  '', ( #119060 ), #164014 ) ;
#112125 = CARTESIAN_POINT ( 'NONE',  ( -4.176793841461789114, 7.030620694084159794, -1.199719254218455378 ) ) ;
#112127 = CARTESIAN_POINT ( 'NONE',  ( 1.358210660854881402, 0.7971155783631430625, 1.803302576489584697 ) ) ;
#112128 =( GEOMETRIC_REPRESENTATION_CONTEXT ( 3 ) GLOBAL_UNCERTAINTY_ASSIGNED_CONTEXT ( ( #83008 ) ) GLOBAL_UNIT_ASSIGNED_CONTEXT ( ( #206182, #175848, #93537 ) ) REPRESENTATION_CONTEXT ( 'NONE', 'WORKASPACE' ) );
#112130 = CARTESIAN_POINT ( 'NONE',  ( -5.424670859243583720, 8.382514198209223721, 1.082531754730550855 ) ) ;
#112129 = CARTESIAN_POINT ( 'NONE',  ( 6.011958326525193463, -0.6379227081053112647, 1.803018720113582773 ) ) ;
#112131 = CARTESIAN_POINT ( 'NONE',  ( -5.763624699140868834, 9.738329559057408602, -0.7216878364870338292 ) ) ;
#112132 = CARTESIAN_POINT ( 'NONE',  ( 5.905458427204159477, 9.047396044116986502, 1.199719254218452047 ) ) ;
#112133 = CARTESIAN_POINT ( 'NONE',  ( -7.065734331377342414, 8.272386803808890576, -1.199719254218452047 ) ) ;
#112134 = CARTESIAN_POINT ( 'NONE',  ( 0.8561247329088355063, 0.8163843618401511737, -1.847503835822896789 ) ) ;
#112135 = CARTESIAN_POINT ( 'NONE',  ( -11.92619526913700057, 19.00000000000000000, 1.328859060402684644 ) ) ;
#112136 = CARTESIAN_POINT ( 'NONE',  ( 4.524672722398297431, 1.423327999681742062, -1.816260527432728811 ) ) ;
#112137 = CARTESIAN_POINT ( 'NONE',  ( 5.775826483351648832, -1.914393393812302113, 0.4282712878391075062 ) ) ;
#112138 = CARTESIAN_POINT ( 'NONE',  ( 2.166782468979636000, 1.457124453068344039, -1.313723524322525815 ) ) ;
#112139 = CARTESIAN_POINT ( 'NONE',  ( 10.26082332744404368, 10.86538205830655279, -0.7998128361456281477 ) ) ;
#112140 = CARTESIAN_POINT ( 'NONE',  ( -9.608223705632537914, 14.88228430527884605, 7.189021993539767230 ) ) ;
#112141 = ORIENTED_EDGE ( 'NONE', *, *, #196828, .T. ) ;
#112142 = CARTESIAN_POINT ( 'NONE',  ( 1.411481693167576434, -1.991701369327549154, 0.7188087792022596068 ) ) ;
#112143 =( BOUNDED_SURFACE ( )  B_SPLINE_SURFACE ( 3, 2, ( 
 ( #164178, #85038, #200892 ),
 ( #34154, #551, #18954 ),
 ( #66616, #86110, #50416 ),
 ( #132763, #116535, #197718 ),
 ( #82904, #100224, #20021 ),
 ( #81848, #166292, #3751 ),
 ( #115479, #17881, #83966 ),
 ( #98127, #152181, #147931 ) ),
 .UNSPECIFIED., .F., .F., .T. ) 
 B_SPLINE_SURFACE_WITH_KNOTS ( ( 4, 2, 2, 4 ),
 ( 3, 3 ),
 ( 0.000000000000000000, 0.0002475938981900030044, 0.0004951877963800060088, 0.0009903755927600120176 ),
 ( 0.000000000000000000, 1.000000000000000000 ),
 .UNSPECIFIED. ) 
 GEOMETRIC_REPRESENTATION_ITEM ( )  RATIONAL_B_SPLINE_SURFACE ( (
 ( 1.000000000000000000, 0.9238795325112901802, 1.000000000000000000),
 ( 1.000000000000000000, 0.9248499699755211578, 1.000000000000000000),
 ( 1.000000000000000000, 0.9171047238581211403, 1.000000000000000000),
 ( 1.000000000000000000, 0.8907236462371712626, 1.000000000000000000),
 ( 1.000000000000000000, 0.8725411758595091882, 1.000000000000000000),
 ( 1.000000000000000000, 0.8105159241142133597, 1.000000000000000000),
 ( 1.000000000000000000, 0.7599483315140991291, 1.000000000000000000),
 ( 1.000000000000000000, 0.7045118851637763857, 1.000000000000000000) ) ) 
 REPRESENTATION_ITEM ( '' )  SURFACE ( )  );
#112145 = CARTESIAN_POINT ( 'NONE',  ( -8.345207244411405156, 9.694828859023472134, 1.199719254218462483 ) ) ;
#112144 = CARTESIAN_POINT ( 'NONE',  ( -3.761497552787613330, 6.475832013972435242, 1.199719254218464037 ) ) ;
#112146 = CARTESIAN_POINT ( 'NONE',  ( 0.9547317490294878750, 0.3612830171869831353, -1.805165878648997912 ) ) ;
#112147 = EDGE_LOOP ( 'NONE', ( #98154, #128490, #167473, #200836 ) ) ;
#112148 = B_SPLINE_CURVE_WITH_KNOTS ( 'NONE', 3,
 ( #185335, #34817, #33762, #52154, #169093, #166979, #67299, #17489 ),
 .UNSPECIFIED., .F., .F.,
 ( 4, 2, 2, 4 ),
 ( 0.000000000000000000, 0.0006775471553183762393, 0.001016320732977563437, 0.001355094310636750744 ),
 .UNSPECIFIED. ) ;
#112149 = CARTESIAN_POINT ( 'NONE',  ( 11.08707159853939217, 9.067765128333563851, 4.459508006857516804 ) ) ;
#112150 = CARTESIAN_POINT ( 'NONE',  ( 2.777707764728345907, 0.3069055913166895966, -2.098134212408508059 ) ) ;
#112151 = CARTESIAN_POINT ( 'NONE',  ( -1.201851678989727383E-14, 3.743750000682817269, 1.732050807568877637 ) ) ;
#112152 = CARTESIAN_POINT ( 'NONE',  ( 7.889955328148847258, 11.29236608522730911, -1.199719254218446718 ) ) ;
#112153 = DIRECTION ( 'NONE',  ( 0.000000000000000000, 0.000000000000000000, 1.000000000000000000 ) ) ;
#112154 = CARTESIAN_POINT ( 'NONE',  ( 3.198563317047153465, -0.5950029230564283234, -1.973035911149529698 ) ) ;
#112156 = PLANE ( 'NONE',  #86226 ) ;
#112155 = CARTESIAN_POINT ( 'NONE',  ( -6.744291347794091784, 9.955758108146730123, -1.199719254218440723 ) ) ;
#112157 = CARTESIAN_POINT ( 'NONE',  ( 0.6823417656249917140, 3.592708333674754506, 1.181850606188765695 ) ) ;
#112158 = CARTESIAN_POINT ( 'NONE',  ( 0.07775346131142897577, 0.6705917366217004627, -2.369298483346020667 ) ) ;
#112159 = CARTESIAN_POINT ( 'NONE',  ( 1.286956418854628525, 3.652345658002387196, 0.4592741676705694998 ) ) ;
#112160 = CARTESIAN_POINT ( 'NONE',  ( 0.1005910224048736229, -2.206496634663042133, -0.04943112074598519229 ) ) ;
#112161 = CARTESIAN_POINT ( 'NONE',  ( 2.513255990918183524, 2.019876067157271748, 1.019300669498679479 ) ) ;
#112162 = CARTESIAN_POINT ( 'NONE',  ( -8.175203439360366531, 12.48156174598837787, 1.040834085586084257E-14 ) ) ;
#112163 = CARTESIAN_POINT ( 'NONE',  ( 2.337905319157699502, -1.045887089798164915, -1.478944033197209462 ) ) ;
#112164 = CARTESIAN_POINT ( 'NONE',  ( 2.061615604755413500, 1.182011660234401962, 1.507458768284040129 ) ) ;
#112165 = CARTESIAN_POINT ( 'NONE',  ( 3.051297593704501043, 1.777051743073382761, -1.062048545217339823 ) ) ;
#112166 = CARTESIAN_POINT ( 'NONE',  ( 0.6823417656249899377, 3.488541667008085323, -1.181850606188754593 ) ) ;
#112167 = CARTESIAN_POINT ( 'NONE',  ( 1.920718329235811872, 1.838843090712917405, 0.7113003943867537426 ) ) ;
#112168 = CARTESIAN_POINT ( 'NONE',  ( 6.604134034941783860, -1.926004669841055339, 0.05029594667986003048 ) ) ;
#112169 = CARTESIAN_POINT ( 'NONE',  ( 2.430351462470367707, 1.813921419787648315, 0.4566771774890953095 ) ) ;
#112171 = CARTESIAN_POINT ( 'NONE',  ( 4.893454165248502186, 8.027304163657891678, -0.9628252682179049282 ) ) ;
#112170 = CARTESIAN_POINT ( 'NONE',  ( 1.629934303081633340, -2.171740791250169611, 0.7807429155501348639 ) ) ;
#112172 = CARTESIAN_POINT ( 'NONE',  ( 2.435812105726247623, 1.142245297582837882, 1.469210208790121763 ) ) ;
#112173 = CARTESIAN_POINT ( 'NONE',  ( 0.6823417656249917140, 3.342708333674754506, 1.181850606188765695 ) ) ;
#112174 = CARTESIAN_POINT ( 'NONE',  ( 5.881316448893678661, -0.05433346072863074611, 2.062130925675903725 ) ) ;
#112175 = CARTESIAN_POINT ( 'NONE',  ( -4.225337428953291230, 8.081310767087481750, 0.7998128361456341429 ) ) ;
#112176 = CARTESIAN_POINT ( 'NONE',  ( 5.926885707468349196, 10.06645042535509660, 1.040834085586084257E-14 ) ) ;
#112177 = CARTESIAN_POINT ( 'NONE',  ( -1.435188857121534545, 3.628165074272017065, 0.4528096192972221878 ) ) ;
#112179 = CARTESIAN_POINT ( 'NONE',  ( 6.159223736743516753, -1.804415119744419149, -1.085654967431331164 ) ) ;
#112178 = TOROIDAL_SURFACE ( 'NONE', #202037, 2.649999999999999911, 0.1000000000000000056 ) ;
#112180 = CARTESIAN_POINT ( 'NONE',  ( -1.364683531250012516, 4.301041667008089320, -0.7879004041258300672 ) ) ;
#112181 = CARTESIAN_POINT ( 'NONE',  ( 6.221977808853903724, -1.195094089922192016, -1.800988070004491792 ) ) ;
#112182 = CARTESIAN_POINT ( 'NONE',  ( 5.988927272769587695, -1.918439801222410201, -0.6316595152702029203 ) ) ;
#112183 = CARTESIAN_POINT ( 'NONE',  ( -0.6823417656250246877, -0.1989583329919109023, 1.181850606188755259 ) ) ;
#112184 = CARTESIAN_POINT ( 'NONE',  ( -4.107757355260591936, 7.736207981205250661, 1.040834085586084257E-14 ) ) ;
#112187 = CARTESIAN_POINT ( 'NONE',  ( 5.829642864196171281, 5.903597551091405826, 0.7216878364870317197 ) ) ;
#112186 = CARTESIAN_POINT ( 'NONE',  ( 6.825078400183548055, 3.702925343214446663, 2.370119418288775925 ) ) ;
#112185 = CARTESIAN_POINT ( 'NONE',  ( 4.864343252252968597, 8.897093904262280972, 0.000000000000000000 ) ) ;
#112188 = CARTESIAN_POINT ( 'NONE',  ( -6.140917232347002042, 6.129101290685087911, -0.7998128361456362523 ) ) ;
#112189 = CARTESIAN_POINT ( 'NONE',  ( 5.120327457147888950, 1.987497208294352280, 0.3399611521368098854 ) ) ;
#112190 = CARTESIAN_POINT ( 'NONE',  ( -7.365103760721662951, 9.615707025640515937, 1.599625672291295375 ) ) ;
#112192 = CARTESIAN_POINT ( 'NONE',  ( -7.743115126736118015, 8.206258200713163475, 0.7216878364870317197 ) ) ;
#112191 = CARTESIAN_POINT ( 'NONE',  ( -8.920901888112002354, 11.43080484092926241, 1.443375672974064550 ) ) ;
#112193 = DIRECTION ( 'NONE',  ( 1.000000000000000000, -0.000000000000000000, -0.000000000000000000 ) ) ;
#112195 = CARTESIAN_POINT ( 'NONE',  ( -1.402160292154681736E-14, 9.921875000341399797, 1.575800808251682339 ) ) ;
#112194 = CARTESIAN_POINT ( 'NONE',  ( 5.700121470611750674, -2.161883445634639411, -0.004416275431240455560 ) ) ;
#112196 = CARTESIAN_POINT ( 'NONE',  ( -11.96362345633627200, 7.996868700864697921, 1.065082418458907609 ) ) ;
#112198 = CARTESIAN_POINT ( 'NONE',  ( 0.2982578006338062471, 1.320465477219048722, -1.388022668363431356 ) ) ;
#112197 = CARTESIAN_POINT ( 'NONE',  ( -5.653386866774179786, 8.579073197003079798, 1.082531754730548412 ) ) ;
#112199 = CARTESIAN_POINT ( 'NONE',  ( 1.364683531249986537, -0.03229166632525094088, -0.7879004041258309554 ) ) ;
#112200 = CARTESIAN_POINT ( 'NONE',  ( 6.539320575229251808, 7.629137130509035636, 2.803262396134009737 ) ) ;
#112201 = CARTESIAN_POINT ( 'NONE',  ( 1.980655567072008072, -0.08268669962357808045, -1.723028944404185303 ) ) ;
#112202 = CARTESIAN_POINT ( 'NONE',  ( 7.506374323821472849, 8.786466794993730289, -1.199719254218452047 ) ) ;
#112203 = CARTESIAN_POINT ( 'NONE',  ( 4.993145711582793744, 9.047363440147082159, -0.7998128361456481317 ) ) ;
#112204 = CARTESIAN_POINT ( 'NONE',  ( -11.89629718460002294, 8.889724561396670666, 1.217720464611954156 ) ) ;
#112205 = CARTESIAN_POINT ( 'NONE',  ( 6.749288224047839790, -1.502610544577225982, -1.113804566994440970 ) ) ;
#112206 = CARTESIAN_POINT ( 'NONE',  ( 0.3814940398445298420, 0.1953205766255173559, -2.003579427208526553 ) ) ;
#112207 = CARTESIAN_POINT ( 'NONE',  ( -4.832429956831352236, 4.840456299650983674, 0.2774298518010898662 ) ) ;
#112208 = CARTESIAN_POINT ( 'NONE',  ( 3.592985822966657583, -0.4282699184722462693, -2.164648485658649868 ) ) ;
#112209 = CARTESIAN_POINT ( 'NONE',  ( 5.454042025912737124, -0.7881617977381920603, 2.023119649181570168 ) ) ;
#112210 = ORIENTED_EDGE ( 'NONE', *, *, #2302, .T. ) ;
#112211 = CARTESIAN_POINT ( 'NONE',  ( 8.229436053370658755, 12.54483312900040026, 0.7216878364870438212 ) ) ;
#112213 = CARTESIAN_POINT ( 'NONE',  ( 2.478138860811992306, -2.011206848916185397, -0.1455134472309257965 ) ) ;
#112212 = CARTESIAN_POINT ( 'NONE',  ( 3.756581929197760683, 2.110411401290826383, 0.2062832702387565331 ) ) ;
#112215 = ORIENTED_EDGE ( 'NONE', *, *, #76035, .T. ) ;
#112214 = CARTESIAN_POINT ( 'NONE',  ( 1.933590839544163664, -1.756428034162808904, 0.4429697619106263695 ) ) ;
#112216 = CARTESIAN_POINT ( 'NONE',  ( 5.203297092594585393, 9.292540051327542017, 0.7998128361456341429 ) ) ;
#112217 = EDGE_CURVE ( 'NONE', #108029, #121330, #198294, .T. ) ;
#112218 = VERTEX_POINT ( 'NONE', #121120 ) ;
#112219 = CARTESIAN_POINT ( 'NONE',  ( 0.6724591444495706671, -1.759989063064151038, -0.6342292696241008665 ) ) ;
#112220 = ADVANCED_FACE ( 'NONE', ( #100504 ), #832, .F. ) ;
#112221 = CARTESIAN_POINT ( 'NONE',  ( 5.178324605415663306, 8.128796908705222535, 1.199719254218462483 ) ) ;
#112223 = CARTESIAN_POINT ( 'NONE',  ( 1.797909001537282503, -0.9065369449853509787, -1.687681949719927577 ) ) ;
#112222 = CARTESIAN_POINT ( 'NONE',  ( -3.903858165731105778, 6.641919395739846799, 1.199719254218464037 ) ) ;
#112224 =( NAMED_UNIT ( * ) SI_UNIT ( $, .STERADIAN. ) SOLID_ANGLE_UNIT ( ) );
#112225 = CARTESIAN_POINT ( 'NONE',  ( -4.868066621355794155, 4.979192643662380569, -0.7254044385785942683 ) ) ;
#112226 = CARTESIAN_POINT ( 'NONE',  ( 0.6823417656249882723, 0.4885416670080827695, -1.181850606188749264 ) ) ;
#112227 = CARTESIAN_POINT ( 'NONE',  ( 5.858512798400357546, 6.179092012920288646, 0.8810539604525641222 ) ) ;
#112228 = CARTESIAN_POINT ( 'NONE',  ( -8.188234707649510113, 11.64035869464474082, -1.199719254218446718 ) ) ;
#112229 = CARTESIAN_POINT ( 'NONE',  ( 5.717692609583751029, -2.109997883074541392, 0.4692839721026839661 ) ) ;
#112230 = CARTESIAN_POINT ( 'NONE',  ( -5.858531774880906262, 6.967946837850073294, 1.082531754730549078 ) ) ;
#112231 = CARTESIAN_POINT ( 'NONE',  ( -5.562588163356775972, 9.711712967216715953, 0.7998128361456291469 ) ) ;
#112232 = CARTESIAN_POINT ( 'NONE',  ( 2.953504815971871533, -1.868289524550557523, 1.003269902519102086 ) ) ;
#112234 = CARTESIAN_POINT ( 'NONE',  ( -11.91002632418505058, 5.203875245307159503, 4.700031268430899800 ) ) ;
#112233 = CARTESIAN_POINT ( 'NONE',  ( 1.500000000000023981, 5.754166666666687746, 0.8660254037844334896 ) ) ;
#112235 = CARTESIAN_POINT ( 'NONE',  ( 3.989495051124877456, 1.425666444934305499, 1.361731899605103768 ) ) ;
#112236 = CARTESIAN_POINT ( 'NONE',  ( 5.361546783204238942, -1.511448857895525855, -1.171587532507123441 ) ) ;
#112237 = ORIENTED_EDGE ( 'NONE', *, *, #49372, .T. ) ;
#112238 = CARTESIAN_POINT ( 'NONE',  ( -2.057629584373543707, 2.441452740530747789, 11.54123292161952641 ) ) ;
#112239 = CARTESIAN_POINT ( 'NONE',  ( 0.7485892145711986467, -2.054541080789675789, -0.2550698046258002005 ) ) ;
#112240 = CARTESIAN_POINT ( 'NONE',  ( 2.765492612253204641, 1.039303555060458351, 1.640259502831205918 ) ) ;
#112241 = EDGE_LOOP ( 'NONE', ( #103612, #190570, #2540, #181906, #123890, #8673, #76440 ) ) ;
#112242 = CARTESIAN_POINT ( 'NONE',  ( -7.065207446497166366, 9.336104335703744539, 0.000000000000000000 ) ) ;
#112243 = CARTESIAN_POINT ( 'NONE',  ( 7.686546744304875389, 7.932335721302671949, 0.7998128361456291469 ) ) ;
#112245 = CARTESIAN_POINT ( 'NONE',  ( 4.984594031318565932, 8.967110136513669616, 0.7998128361456462443 ) ) ;
#112244 = CARTESIAN_POINT ( 'NONE',  ( 2.748082359423655419, 0.7051493092682534769, 1.968258087557398284 ) ) ;
#112246 = CARTESIAN_POINT ( 'NONE',  ( 4.380693030546916944, 6.204170850428461392, 1.443375672974058777 ) ) ;
#112248 = ORIENTED_EDGE ( 'NONE', *, *, #82581, .T. ) ;
#112247 = CARTESIAN_POINT ( 'NONE',  ( 0.9085206565882588681, -0.4392767353821840914, -1.757246876086359988 ) ) ;
#112249 = CARTESIAN_POINT ( 'NONE',  ( 4.037865812933420173, -1.521084700717803884, -1.599171214764223636 ) ) ;
#112250 = CARTESIAN_POINT ( 'NONE',  ( 3.469938103458301448, 2.153457811087633011, -0.4814610123115290463 ) ) ;
#112251 = CARTESIAN_POINT ( 'NONE',  ( 7.422199028477372451, 10.74665040227725044, -1.199719254218441611 ) ) ;
#112252 = FILL_AREA_STYLE_COLOUR ( '', #172384 ) ;
#112253 = CARTESIAN_POINT ( 'NONE',  ( 2.244649938279310142, 1.855272219182309668, 0.4629769397326845004 ) ) ;
#112254 = CARTESIAN_POINT ( 'NONE',  ( 11.44800751629994906, 13.79999999999999893, -3.302956944461097777 ) ) ;
#112255 = CARTESIAN_POINT ( 'NONE',  ( 4.018080225218490398, 2.055083638104511223, -0.2504045000601487492 ) ) ;
#112257 = CARTESIAN_POINT ( 'NONE',  ( 2.641676655999642076, -1.601130012699041982, -1.452526871000489495 ) ) ;
#112256 = CARTESIAN_POINT ( 'NONE',  ( 0.4635785636673654952, -6.836568542495036205, 10.85353573482952250 ) ) ;
#112258 = CARTESIAN_POINT ( 'NONE',  ( 5.161759341795384870, 1.079763445194487970, 1.907048802792680631 ) ) ;
#112259 = CARTESIAN_POINT ( 'NONE',  ( -6.143440778383317813, 6.339971461045375456, 7.509178883279419847E-06 ) ) ;
#112260 = CARTESIAN_POINT ( 'NONE',  ( 1.458777222063855739, 0.9000000000000014655, -1.713029193092652225 ) ) ;
#112261 = CARTESIAN_POINT ( 'NONE',  ( -9.053319117722196552, 15.44694771161291236, 7.821787350058786004 ) ) ;
#112262 = CARTESIAN_POINT ( 'NONE',  ( 5.037736595929563244, 8.035053907629919223, -1.199719254218452047 ) ) ;
#112263 = CARTESIAN_POINT ( 'NONE',  ( 1.642778471875001811, -3.230208332855373676, 2.845375778867859751 ) ) ;
#112264 = CARTESIAN_POINT ( 'NONE',  ( -3.806807270387036368, 7.663301925418665839, 0.000000000000000000 ) ) ;
#112266 = CARTESIAN_POINT ( 'NONE',  ( 0.7916389524552720491, 1.525042296397002284, -1.319230309296010928 ) ) ;
#112265 = CIRCLE ( 'NONE', #195236, 0.07999999999999951594 ) ;
#112267 = CARTESIAN_POINT ( 'NONE',  ( -9.341204650135658483, 10.00041963468749984, 1.040834085586084257E-14 ) ) ;
#112268 = CARTESIAN_POINT ( 'NONE',  ( 4.434477146351770926, -1.196200190851111733, 1.689492296227593116 ) ) ;
#112269 = CARTESIAN_POINT ( 'NONE',  ( 3.387250987759330645, 1.741285041988534621, -0.8245012487104221854 ) ) ;
#112270 = CARTESIAN_POINT ( 'NONE',  ( 6.204719021523306566, 1.975628225290576356, 0.7617523325972180848 ) ) ;
#112271 = CARTESIAN_POINT ( 'NONE',  ( 6.484877546038077867, 6.460111979999551224, 1.040834085586084257E-14 ) ) ;
#112272 = CARTESIAN_POINT ( 'NONE',  ( 9.367496997597639208, 4.469082183885418225, 7.499999999999949374 ) ) ;
#112273 = CARTESIAN_POINT ( 'NONE',  ( 3.450015926008513478, -0.8023341227383492535, 1.798807795796441678 ) ) ;
#112274 = CARTESIAN_POINT ( 'NONE',  ( 5.789115795541526666, 1.732349586671273922, 1.501262892615047750 ) ) ;
#112275 = CARTESIAN_POINT ( 'NONE',  ( 4.564971734551386717, -1.632036996880025903, -0.8184370388232551363 ) ) ;
#112276 = CARTESIAN_POINT ( 'NONE',  ( 6.753369913382843315, 8.011924666102361314, -1.082531754730548412 ) ) ;
#112278 = ADVANCED_FACE ( 'NONE', ( #70112 ), #86396, .T. ) ;
#112277 = CARTESIAN_POINT ( 'NONE',  ( 3.673896439178911066, 7.230036912443299713, 0.7216878364870317197 ) ) ;
#112279 = CARTESIAN_POINT ( 'NONE',  ( -5.094831863685302942, 9.165997284266655498, 0.7998128361456291469 ) ) ;
#112280 = CARTESIAN_POINT ( 'NONE',  ( 6.391743074199808916, 6.421731439513382433, -0.7998128361456481317 ) ) ;
#112281 = ORIENTED_EDGE ( 'NONE', *, *, #179232, .T. ) ;
#112283 = CARTESIAN_POINT ( 'NONE',  ( 5.097907127711155617, 1.355137859109056819, 1.488956579698009763 ) ) ;
#112282 = CARTESIAN_POINT ( 'NONE',  ( 1.065666191918061445, -1.167978014494171823, 1.423405568861766168 ) ) ;
#112284 = CARTESIAN_POINT ( 'NONE',  ( 1.423680875022467873, 0.9325134783980688624, 2.100857314651356500 ) ) ;
#112285 = CARTESIAN_POINT ( 'NONE',  ( 5.137533780887935997, 1.831872034461759835, -0.7024582609849658876 ) ) ;
#112286 = CARTESIAN_POINT ( 'NONE',  ( -5.371001409308059138, 9.417918744168066070, -0.7998128361456231517 ) ) ;
#112287 = CARTESIAN_POINT ( 'NONE',  ( -5.271422797614987665, 5.044414773505913274, -0.7998128361456221525 ) ) ;
#112288 = CARTESIAN_POINT ( 'NONE',  ( 0.000000000000000000, 1.551257596039481879, 0.000000000000000000 ) ) ;
#112289 = CARTESIAN_POINT ( 'NONE',  ( -4.014095998097799267, 6.840806543492835345, -1.199719254218450271 ) ) ;
#112291 = CARTESIAN_POINT ( 'NONE',  ( 6.772329494929559601, -1.084452473627237845, 1.399072979944876449 ) ) ;
#112290 = CARTESIAN_POINT ( 'NONE',  ( 1.470382607095675143, -1.986325758040393685, -0.6527442681472686026 ) ) ;
#112292 = CARTESIAN_POINT ( 'NONE',  ( -0.4000000000000114575, 2.999999999999999112, 2.023857702507764422 ) ) ;
#112293 = CARTESIAN_POINT ( 'NONE',  ( -0.1102773484823937195, 1.312263477441493187, -2.452793124480449283 ) ) ;
#112294 = CARTESIAN_POINT ( 'NONE',  ( 1.311604768886602157, 1.169564267535606605, -1.289085965974474668 ) ) ;
#112295 = CARTESIAN_POINT ( 'NONE',  ( 5.666418135507635512, 8.698239360479199433, 1.199719254218462483 ) ) ;
#112297 = DIRECTION ( 'NONE',  ( 0.000000000000000000, 0.000000000000000000, -1.000000000000000000 ) ) ;
#112296 = DIRECTION ( 'NONE',  ( 0.000000000000000000, 1.000000000000000000, 0.000000000000000000 ) ) ;
#112298 = CARTESIAN_POINT ( 'NONE',  ( 1.945521746005531627, 0.6619316864419527713, -1.593019548489343240 ) ) ;
#112300 = EDGE_CURVE ( 'NONE', #135057, #93531, #212047, .T. ) ;
#112299 = CARTESIAN_POINT ( 'NONE',  ( 1.699035084177059174, 1.824418957995146195, 1.213967346723361596 ) ) ;
#112301 = CARTESIAN_POINT ( 'NONE',  ( -0.05262932013434371004, -1.547529252455181581, -0.7825623337873451879 ) ) ;
#112302 = CARTESIAN_POINT ( 'NONE',  ( 4.020313978404310262, -1.133593497508533110, -1.893353337301090233 ) ) ;
#112303 = CARTESIAN_POINT ( 'NONE',  ( -1.286813488861823895, 3.652992958535467238, -0.4595522011843558574 ) ) ;
#112304 = CARTESIAN_POINT ( 'NONE',  ( 0.8136159317379263456, -1.833160233796997218, -1.162963494187698510 ) ) ;
#112305 = CARTESIAN_POINT ( 'NONE',  ( 0.1877650043593872553, -0.8638833939697135866, 1.608357707688967242 ) ) ;
#112306 = CARTESIAN_POINT ( 'NONE',  ( 3.098929814713128561, 1.916056983672033587, 0.9012583305440853287 ) ) ;
#112307 = STYLED_ITEM ( 'NONE', ( #75641 ), #91304 ) ;
#112308 = CARTESIAN_POINT ( 'NONE',  ( 6.639320575229258559, 7.629137130509072051, 2.496737603865983424 ) ) ;
#112309 = ORIENTED_EDGE ( 'NONE', *, *, #82886, .T. ) ;
#112311 = CARTESIAN_POINT ( 'NONE',  ( 1.364683531249988757, -0.5531249996585801965, 0.000000000000000000 ) ) ;
#112310 = CARTESIAN_POINT ( 'NONE',  ( 3.298623631688667235, 1.806097335442503393, -1.411605728516792002 ) ) ;
#112312 = CARTESIAN_POINT ( 'NONE',  ( 3.277320446201373638, 4.846626492033466072, 1.599625672291267398 ) ) ;
#112313 = CARTESIAN_POINT ( 'NONE',  ( 5.515469562660962666, 5.329135999392899947, 0.7998128361456341429 ) ) ;
#112314 = CARTESIAN_POINT ( 'NONE',  ( 5.707756388377941192, 1.680692789272177468, 1.452518960167401341 ) ) ;
#112315 = CARTESIAN_POINT ( 'NONE',  ( -6.317736394288148816, 8.393778431468064127, 1.443375672974078761 ) ) ;
#112316 = CARTESIAN_POINT ( 'NONE',  ( 3.850152436600926542, 7.435668909435648288, -0.7216878364870197293 ) ) ;
#112317 = CARTESIAN_POINT ( 'NONE',  ( -6.304178240230145391, 9.338329799368375816, 1.082531754730548412 ) ) ;
#112318 = CARTESIAN_POINT ( 'NONE',  ( 4.502716413514295191, 6.346531463890372926, -1.443375672974068769 ) ) ;
#112319 = ORIENTED_EDGE ( 'NONE', *, *, #196992, .T. ) ;
#112320 = CARTESIAN_POINT ( 'NONE',  ( 4.500625067706437221, -1.976956227568788638, 0.3961002554062897918 ) ) ;
#112322 = CARTESIAN_POINT ( 'NONE',  ( 2.536046341495324707, 1.265347977242038402, 1.628790341535201636 ) ) ;
#112321 = CARTESIAN_POINT ( 'NONE',  ( 7.311924916471702396, 7.425000578838787391, -0.7998128361456281477 ) ) ;
#112323 = DIRECTION ( 'NONE',  ( 0.000000000000000000, 1.000000000000000000, 0.000000000000000000 ) ) ;
#112324 = CARTESIAN_POINT ( 'NONE',  ( 4.041739190205284160, 7.729463131965888856, 0.000000000000000000 ) ) ;
#112326 = ADVANCED_FACE ( 'NONE', ( #186008 ), #137300, .T. ) ;
#112325 = CARTESIAN_POINT ( 'NONE',  ( -7.137427454244817504, -7.616807780282264240, -7.137427454241226599 ) ) ;
#112327 = CARTESIAN_POINT ( 'NONE',  ( 1.364683531249990311, 5.113541667008084879, 0.7879004041258500513 ) ) ;
#112328 = CARTESIAN_POINT ( 'NONE',  ( 5.068408068084750973, -2.062719301109996461, -0.7404068969242217912 ) ) ;
#112329 = CARTESIAN_POINT ( 'NONE',  ( 2.567029916978436077, -1.034165006014248211, 1.730866473406714068 ) ) ;
#112330 = CARTESIAN_POINT ( 'NONE',  ( 1.856743374925871715, 0.3135980649527739250, -1.814175028193690808 ) ) ;
#112331 = VECTOR ( 'NONE', #147866, 1000.000000000000114 ) ;
#112332 = EDGE_CURVE ( 'NONE', #137516, #95128, #68758, .T. ) ;
#112333 = CARTESIAN_POINT ( 'NONE',  ( 6.096362627639171805, 10.26417349888772179, -0.7998128361456291469 ) ) ;
#112334 = SURFACE_STYLE_USAGE ( .BOTH. , #179409 ) ;
#112335 = CARTESIAN_POINT ( 'NONE',  ( 5.280226139177822908, -1.012770463184736736, 1.518683248463777113 ) ) ;
#112336 = CARTESIAN_POINT ( 'NONE',  ( 6.012342310302175363, -1.897698807000438359, 0.6819931642896917001 ) ) ;
#112337 = CARTESIAN_POINT ( 'NONE',  ( -6.744291347794091784, 9.955758108146730123, -1.199719254218440723 ) ) ;
#112339 = CARTESIAN_POINT ( 'NONE',  ( -6.967964602780620353, 7.093989889524320525, 0.000000000000000000 ) ) ;
#112338 = CARTESIAN_POINT ( 'NONE',  ( 5.664971525351325532, -2.042639428312309935, -0.9732368426803981176 ) ) ;
#112340 = CARTESIAN_POINT ( 'NONE',  ( 1.278104297367024467, 1.255928009607910623, 1.690453460462447044 ) ) ;
#112341 = CARTESIAN_POINT ( 'NONE',  ( -7.598418745816086783, 7.829519723065708092, 0.000000000000000000 ) ) ;
#112342 = CARTESIAN_POINT ( 'NONE',  ( 8.191097360950562845, 12.70803068775103739, -0.7998128361456352531 ) ) ;
#112343 = CARTESIAN_POINT ( 'NONE',  ( 3.998552357014331982, 7.829812261164016185, 1.248643980066187585E-14 ) ) ;
#112344 = CARTESIAN_POINT ( 'NONE',  ( 8.378074386687003994, 13.00815134976859078, 15.76159487570644124 ) ) ;
#112345 = CARTESIAN_POINT ( 'NONE',  ( -8.376239975144482486, 8.666701480623698828, 1.040834085586084257E-14 ) ) ;
#112346 = UNCERTAINTY_MEASURE_WITH_UNIT (LENGTH_MEASURE( 1.000000000000000082E-05 ), #145452, 'distance_accuracy_value', 'NONE');
#112347 = CARTESIAN_POINT ( 'NONE',  ( 6.933015448541703485, 9.181880338089085214, 1.599625672291268286 ) ) ;
#112348 = CARTESIAN_POINT ( 'NONE',  ( 5.645731234294472323, 6.129814942853209381, -0.7970442531908157324 ) ) ;
#112349 = CARTESIAN_POINT ( 'NONE',  ( -7.998947442382709383, 12.27592974951444660, 0.7216878364870478180 ) ) ;
#112350 = CARTESIAN_POINT ( 'NONE',  ( 3.023905552101690208, -0.4295200811062405699, 2.179336035515607950 ) ) ;
#112351 = CARTESIAN_POINT ( 'NONE',  ( 3.215772567386471437, 6.427315425527130088, -0.8732430475888955934 ) ) ;
#112352 = CARTESIAN_POINT ( 'NONE',  ( -6.473091995881817162, 6.516638514809040217, 0.7998128361456281477 ) ) ;
#112353 = CARTESIAN_POINT ( 'NONE',  ( 6.368579470117202490, 8.453095353268645695, 1.599625672291281386 ) ) ;
#112354 = CARTESIAN_POINT ( 'NONE',  ( 3.666413850373055006, -0.7928392042928497085, -1.794698522912529182 ) ) ;
#112355 = CARTESIAN_POINT ( 'NONE',  ( 5.660692828905515839, 6.562895374266609849, -1.199719254218445830 ) ) ;
#112356 = CARTESIAN_POINT ( 'NONE',  ( -4.034767475943390025, 7.597003608976943489, -0.2951547658557127640 ) ) ;
#112357 = CARTESIAN_POINT ( 'NONE',  ( 4.518945272056516416, 4.166524327021037699, 0.7998128361456341429 ) ) ;
#112358 = CARTESIAN_POINT ( 'NONE',  ( -5.370438244788932280, 6.398504386076097283, 1.082531754730549078 ) ) ;
#112359 = CARTESIAN_POINT ( 'NONE',  ( -7.266807147244793263, 8.540658428949452485, 1.082531754730549967 ) ) ;
#112360 = CARTESIAN_POINT ( 'NONE',  ( 2.338272602237463360, -1.224740070204191289, -1.730971256048131401 ) ) ;
#112361 = CARTESIAN_POINT ( 'NONE',  ( -6.473091995881817162, 6.516638514809040217, 0.7998128361456281477 ) ) ;
#112362 = CARTESIAN_POINT ( 'NONE',  ( 4.276362541559985075, -1.246951984143488623, 1.765614359104182629 ) ) ;
#112363 = CARTESIAN_POINT ( 'NONE',  ( 2.313779677144182312, 1.201330555204615180, -1.395457044143719072 ) ) ;
#112364 = CARTESIAN_POINT ( 'NONE',  ( -4.525130642185515306, 7.025754810433701536, 1.158151338111103046 ) ) ;
#112365 = CARTESIAN_POINT ( 'NONE',  ( -0.6823417656250246877, 0.3635416670080895973, 1.181850606188755259 ) ) ;
#112366 = B_SPLINE_CURVE_WITH_KNOTS ( 'NONE', 3,
 ( #50634, #34376, #198988, #32256, #82060, #97276, #148152, #13852, #62609, #64747, #81004, #212044, #777 ),
 .UNSPECIFIED., .F., .F.,
 ( 4, 3, 3, 3, 4 ),
 ( 0.000000000000000000, 3.127676560591855702E-05, 7.184563044157459683E-05, 0.0001122497773744156145, 0.0001140446530104083958 ),
 .UNSPECIFIED. ) ;
#112367 = CARTESIAN_POINT ( 'NONE',  ( 5.929613673486688441, 0.8517357041802063877, -1.517590187452934281 ) ) ;
#112368 = CARTESIAN_POINT ( 'NONE',  ( 6.727182134110222478, 0.005875948494733079785, 1.810970247402940547 ) ) ;
#112369 = CARTESIAN_POINT ( 'NONE',  ( 4.744990575102895569, 5.598539094783909320, -1.082531754730548412 ) ) ;
#112370 =( NAMED_UNIT ( * ) PLANE_ANGLE_UNIT ( ) SI_UNIT ( $, .RADIAN. ) );
#112371 = CARTESIAN_POINT ( 'NONE',  ( 3.573254463033649131, 0.05508235185803719847, -2.161170636208443963 ) ) ;
#112372 = CARTESIAN_POINT ( 'NONE',  ( 4.569685373303983944, 1.560260980002409870, -1.276848140101802365 ) ) ;
#112373 = CARTESIAN_POINT ( 'NONE',  ( -9.964879715919934711, 10.72804054476916313, 0.7216878364870438212 ) ) ;
#112374 = CARTESIAN_POINT ( 'NONE',  ( 2.184651956524386041, -2.119909832212972578, -0.4221607449544013679 ) ) ;
#112375 = CARTESIAN_POINT ( 'NONE',  ( 2.635955087654485940, 0.9327151613215716175, -1.736774642614127284 ) ) ;
#112376 = CARTESIAN_POINT ( 'NONE',  ( 1.394453263437886604E-15, -2.668749999044085275, 3.474999999999999645 ) ) ;
#112377 = CARTESIAN_POINT ( 'NONE',  ( 4.616706917144582256, -0.09184519841067168011, 1.939997386343417896 ) ) ;
#112380 = EDGE_LOOP ( 'NONE', ( #190927, #25642, #68968, #194488, #77783, #59814, #84175 ) ) ;
#112379 = FACE_OUTER_BOUND ( 'NONE', #198219, .T. ) ;
#112378 = CARTESIAN_POINT ( 'NONE',  ( -7.632877294369372123, 11.84884791016554573, 0.7216878364870458196 ) ) ;
#112381 = CARTESIAN_POINT ( 'NONE',  ( -4.055297343818976330, 5.824542549245813383, 1.443375672974065660 ) ) ;
#112382 = LINE ( 'NONE', #27862, #164808 ) ;
#112384 = VERTEX_POINT ( 'NONE', #53898 ) ;
#112383 = CARTESIAN_POINT ( 'NONE',  ( -4.980641328173854632, 6.904110530993182948, 1.599625672291263179 ) ) ;
#112385 = CARTESIAN_POINT ( 'NONE',  ( -8.066738210006693777, 10.43428054980638997, 1.443375672974090751 ) ) ;
#112386 = CARTESIAN_POINT ( 'NONE',  ( 1.518904762042364354, 1.481482853740143657, -1.635709697223409531 ) ) ;
#112387 = CARTESIAN_POINT ( 'NONE',  ( -3.285556943749998737, -1.480208332855375453, 1.896917185911908499 ) ) ;
#112388 = CARTESIAN_POINT ( 'NONE',  ( 5.840667439708360220, -1.913134005453724251, -0.4332900713753874977 ) ) ;
#112389 = CARTESIAN_POINT ( 'NONE',  ( 0.6823417656249917140, 5.155208333674749177, 1.181850606188765695 ) ) ;
#112390 = CARTESIAN_POINT ( 'NONE',  ( 0.7499999999999902300, 3.597916667349487785, -1.299038105676658228 ) ) ;
#112391 = CARTESIAN_POINT ( 'NONE',  ( 5.337709665475443011, 6.539638787446115487, -1.341754179669167213 ) ) ;
#112392 = CARTESIAN_POINT ( 'NONE',  ( 0.1749903794560566384, 0.2522965209616668814, -1.990827758811020809 ) ) ;
#112393 = CARTESIAN_POINT ( 'NONE',  ( 3.872867692073681756, 1.733033312621637068, -0.6219614626309655225 ) ) ;
#112394 = ORIENTED_EDGE ( 'NONE', *, *, #167891, .F. ) ;
#112395 = CARTESIAN_POINT ( 'NONE',  ( 1.360316468750001784, -0.7552083329919376808, 0.7853790794158941324 ) ) ;
#112396 = ADVANCED_FACE ( 'NONE', ( #168706 ), #21362, .T. ) ;
#112397 = CARTESIAN_POINT ( 'NONE',  ( -7.182068686937172153, 9.402166106225269715, 1.599625672291283607 ) ) ;
#112398 = FACE_OUTER_BOUND ( 'NONE', #115046, .T. ) ;
#112400 = CIRCLE ( 'NONE', #115775, 0.07999999999999998779 ) ;
#112399 = CARTESIAN_POINT ( 'NONE',  ( 6.222909436229170588, 1.570324008046734221, -1.425282903188800798 ) ) ;
#112401 = PRESENTATION_STYLE_ASSIGNMENT (( #162162 ) ) ;
#112402 = CARTESIAN_POINT ( 'NONE',  ( 5.961834861707224320, 7.978559976790334574, -1.599625672291262513 ) ) ;
#112403 = CARTESIAN_POINT ( 'NONE',  ( 6.837187436585446143, -1.842956594435873896, 0.9222261209423606720 ) ) ;
#112406 = CARTESIAN_POINT ( 'NONE',  ( 3.860763913883006992, 0.2215400755124704024, -1.827792592973469743 ) ) ;
#112405 = CARTESIAN_POINT ( 'NONE',  ( 1.609564491371988426, 0.5446964562696824386, -1.779540750359181800 ) ) ;
#112404 = CARTESIAN_POINT ( 'NONE',  ( -9.604686356149278126, 4.518459255872631530, 7.193747284969081335 ) ) ;
#112407 = CARTESIAN_POINT ( 'NONE',  ( 6.448874621594486989, 10.67543749183559143, 0.7998128361456462443 ) ) ;
#112408 = FILL_AREA_STYLE_COLOUR ( '', #30948 ) ;
#112409 = CARTESIAN_POINT ( 'NONE',  ( -6.363572996767778100, 8.517530811019446091, -1.599625672291271394 ) ) ;
#112410 = CARTESIAN_POINT ( 'NONE',  ( 1.499999999999990896, 4.556250000682819490, 1.214306433183764966E-14 ) ) ;
#112411 = CARTESIAN_POINT ( 'NONE',  ( 3.282038605231399231, 1.400092287458438722, 1.705885466304429166 ) ) ;
#112412 = CARTESIAN_POINT ( 'NONE',  ( 6.432949606591497727, 0.2122621168692347127, 2.252429721023613496 ) ) ;
#112413 = CARTESIAN_POINT ( 'NONE',  ( -5.233084105194862445, 9.049089189461916760, 0.7216878364870458196 ) ) ;
#112414 = CARTESIAN_POINT ( 'NONE',  ( 5.836161222118039227, -1.013825144121174526, -1.501122385605196952 ) ) ;
#112415 = CARTESIAN_POINT ( 'NONE',  ( 6.503150280507321135, -0.1381757461387123076, 1.884094533524976578 ) ) ;
#112416 = CARTESIAN_POINT ( 'NONE',  ( -4.521192831603464413, 5.406218046348621797, 1.258376203098745316 ) ) ;
#112417 = CARTESIAN_POINT ( 'NONE',  ( 6.139502064137229986, -1.356240498024411600, -1.288626068300227523 ) ) ;
#112418 = CARTESIAN_POINT ( 'NONE',  ( 6.162542460989155479, -0.6707643300355231597, -1.736165932305182125 ) ) ;
#112419 = FACE_OUTER_BOUND ( 'NONE', #195272, .T. ) ;
#112420 = AXIS2_PLACEMENT_3D ( 'NONE', #192646, #26952, #44299 ) ;
#112421 = CARTESIAN_POINT ( 'NONE',  ( 6.702016551492756768, -1.769339222028827319, 0.04870252428828580893 ) ) ;
#112422 = CARTESIAN_POINT ( 'NONE',  ( 1.200408080392855181, 1.350732740426639822, -1.497504596960941958 ) ) ;
#112424 = CARTESIAN_POINT ( 'NONE',  ( 3.088603512095712045, -2.074978072712420296, -0.3595722787458465186 ) ) ;
#112423 = CARTESIAN_POINT ( 'NONE',  ( -9.829825065107822724, 11.42688298316931572, 1.199719254218462483 ) ) ;
#112425 = CARTESIAN_POINT ( 'NONE',  ( 9.745613490124728884, 10.26430391476735338, 0.7998128361456462443 ) ) ;
#112427 = CARTESIAN_POINT ( 'NONE',  ( -9.840520565420403543, 10.37502883594562597, 1.040834085586084257E-14 ) ) ;
#112426 = CARTESIAN_POINT ( 'NONE',  ( 1.499999999999985123, -0.7041666666666481778, -0.8660254037844323793 ) ) ;
#112428 = SURFACE_SIDE_STYLE ('',( #132902 ) ) ;
#112429 = CARTESIAN_POINT ( 'NONE',  ( 2.584245202030683419, 1.084020786718616680, 1.704056320703779992 ) ) ;
#112430 = CARTESIAN_POINT ( 'NONE',  ( 1.364683531249990311, 3.384375000341416140, 1.214306433183764966E-14 ) ) ;
#112431 = CARTESIAN_POINT ( 'NONE',  ( 9.408995418203963013, 12.00024729270324286, 1.443375672974076540 ) ) ;
#112432 = CARTESIAN_POINT ( 'NONE',  ( 3.128364550451453230, 1.203671540783244565, -1.795256801906938815 ) ) ;
#112433 = LINE ( 'NONE', #195754, #199201 ) ;
#112435 = CARTESIAN_POINT ( 'NONE',  ( 4.518610335104485287, 8.493738834255713854, 0.000000000000000000 ) ) ;
#112434 = CARTESIAN_POINT ( 'NONE',  ( 6.318982112420993502, 9.529840343536603697, -1.199719254218452047 ) ) ;
#112436 = CARTESIAN_POINT ( 'NONE',  ( 9.286972035236624734, 11.85788667924133399, -1.443375672974058777 ) ) ;
#112437 = CARTESIAN_POINT ( 'NONE',  ( 0.9421113726552653445, 1.458074577165750396, 1.608915699534870569 ) ) ;
#112438 = VECTOR ( 'NONE', #143957, 1000.000000000000000 ) ;
#112439 = CARTESIAN_POINT ( 'NONE',  ( -6.073689629242158716, 9.069426419882418600, -1.082531754730538864 ) ) ;
#112440 = CARTESIAN_POINT ( 'NONE',  ( -1.364683531250014514, 0.4885416670080875434, -0.7879004041258289570 ) ) ;
#112441 = CARTESIAN_POINT ( 'NONE',  ( 2.630644284709309666, 0.2711686948545319886, 2.174668582101045633 ) ) ;
#112442 = CARTESIAN_POINT ( 'NONE',  ( 0.4636475088198339645, 7.942422027498646564, 1.946104516853490285 ) ) ;
#112443 = CARTESIAN_POINT ( 'NONE',  ( 2.712116605023757288, -2.238012884330255581, 0.3312714459411686962 ) ) ;
#112444 = CARTESIAN_POINT ( 'NONE',  ( -9.006694118179950692, 9.402231314165087284, 1.040834085586084257E-14 ) ) ;
#112445 = CARTESIAN_POINT ( 'NONE',  ( -2.779058300676980675, 5.225689869889666106, -1.082531754730543083 ) ) ;
#112446 = CARTESIAN_POINT ( 'NONE',  ( 0.6823417656249899377, 3.738541667008085767, -1.181850606188754593 ) ) ;
#112447 = CARTESIAN_POINT ( 'NONE',  ( 4.816695983655697511, 8.110494931179941247, 0.8576603160085185529 ) ) ;
#112448 = CARTESIAN_POINT ( 'NONE',  ( -1.500000000000015099, 10.97916666666666785, -0.8660254037844309360 ) ) ;
#112449 = CARTESIAN_POINT ( 'NONE',  ( 7.200788982633824276, 7.573544365927161515, 0.000000000000000000 ) ) ;
#112450 = CARTESIAN_POINT ( 'NONE',  ( 3.163107763524728444, 0.2631224511941733790, -1.749944513356870734 ) ) ;
#112451 = CARTESIAN_POINT ( 'NONE',  ( 8.992082194361556091, 11.51384853155376220, 1.599625672291279388 ) ) ;
#112453 = AXIS2_PLACEMENT_3D ( 'NONE', #155572, #7155, #208556 ) ;
#112452 = CARTESIAN_POINT ( 'NONE',  ( 6.387735258934439386, 1.517164627179751646, 1.602757196154185770 ) ) ;
#112454 = CARTESIAN_POINT ( 'NONE',  ( 1.364683531249996529, 9.713541667008064096, 0.7879004041258405033 ) ) ;
#112455 = CARTESIAN_POINT ( 'NONE',  ( -4.553559489343377287, 6.405848385690952718, -1.599625672291271394 ) ) ;
#112456 = CARTESIAN_POINT ( 'NONE',  ( 6.046499952770106212, -1.423952032562772807, 1.427948417171531759 ) ) ;
#112457 = ORIENTED_EDGE ( 'NONE', *, *, #59313, .T. ) ;
#112458 = ADVANCED_FACE ( 'NONE', ( #34431 ), #127091, .T. ) ;
#112459 = CARTESIAN_POINT ( 'NONE',  ( 3.713615009860570471, -1.843089489661838831, 0.3189824552965599413 ) ) ;
#112460 = ADVANCED_FACE ( 'NONE', ( #84852 ), #16258, .T. ) ;
#112461 = CARTESIAN_POINT ( 'NONE',  ( 2.834898843300116766, -1.979765732921334731, -0.6052725283285932401 ) ) ;
#112462 = CARTESIAN_POINT ( 'NONE',  ( -6.468648687051513413, 7.679749902049126220, 1.082531754730549078 ) ) ;
#112463 = CARTESIAN_POINT ( 'NONE',  ( -10.95308175811721085, 11.29999999999998117, 1.799999999999999600 ) ) ;
#112464 = CARTESIAN_POINT ( 'NONE',  ( 2.482948226198860464, 5.072301959192136778, 2.500000000000000444 ) ) ;
#112465 = CARTESIAN_POINT ( 'NONE',  ( -5.800535780310947409, 5.989883198674579745, 0.3271122460986007896 ) ) ;
#112466 = CARTESIAN_POINT ( 'NONE',  ( 3.469446951953614189E-15, 5.900000000000023448, 1.214306433183764966E-14 ) ) ;
#112467 = CARTESIAN_POINT ( 'NONE',  ( 1.364683531249988535, 5.717708333674752730, -0.7879004041258300672 ) ) ;
#112468 = AXIS2_PLACEMENT_3D ( 'NONE', #141819, #190503, #123489 ) ;
#112469 = CARTESIAN_POINT ( 'NONE',  ( 3.350005920730843911, -0.7974703105717847462, 1.792663495558038056 ) ) ;
#112470 = CARTESIAN_POINT ( 'NONE',  ( 0.7024996975148189993, -1.423740904080775138, -1.427721366232127753 ) ) ;
#112471 = EDGE_CURVE ( 'NONE', #147411, #162878, #125923, .T. ) ;
#112472 = CARTESIAN_POINT ( 'NONE',  ( -4.309512724297390740, 6.121127159803966933, 1.599625672291270506 ) ) ;
#112474 =( LENGTH_UNIT ( ) NAMED_UNIT ( * ) SI_UNIT ( .MILLI., .METRE. ) );
#112473 = CARTESIAN_POINT ( 'NONE',  ( 8.341290820905593151, 10.75459192918846618, 1.599625672291281386 ) ) ;
#112475 = CARTESIAN_POINT ( 'NONE',  ( 1.106479506788549116, 1.420293003395491693, -1.217391549091076275 ) ) ;
#112476 = CARTESIAN_POINT ( 'NONE',  ( -0.6823417656249969321, 3.217708333674754062, -1.181850606188749264 ) ) ;
#112477 = CARTESIAN_POINT ( 'NONE',  ( 3.357684704777043283, -1.527344908821237635, -1.311707263431096671 ) ) ;
#112479 = CARTESIAN_POINT ( 'NONE',  ( 2.056417290815291121, -1.299724242359597826, 1.671285701813587821 ) ) ;
#112478 = CARTESIAN_POINT ( 'NONE',  ( -7.266807147244793263, 8.540658428949452485, 1.082531754730549967 ) ) ;
#112480 = CARTESIAN_POINT ( 'NONE',  ( 1.451998047843341633, 7.315968950353821221, 4.301760722578430673 ) ) ;
#112481 = CARTESIAN_POINT ( 'NONE',  ( 3.719242722441223226, -1.824546119899137731, -0.9785211796824041519 ) ) ;
#112482 = CARTESIAN_POINT ( 'NONE',  ( 5.643937085038755797, 9.806620042512378177, -0.7998128361456481317 ) ) ;
#112484 = LINE ( 'NONE', #27970, #42593 ) ;
#112483 = CARTESIAN_POINT ( 'NONE',  ( 5.542948256250054051, -1.647469546829454234, -1.286982348046373570 ) ) ;
#112486 = EDGE_LOOP ( 'NONE', ( #178247, #40594, #214035, #95032 ) ) ;
#112485 = CARTESIAN_POINT ( 'NONE',  ( 4.717693524642503355, -1.790169364231732674, 0.3569235582787863570 ) ) ;
#112487 = CARTESIAN_POINT ( 'NONE',  ( 8.378048858240820351, 11.86180853700128601, -1.199719254218446718 ) ) ;
#112488 = CARTESIAN_POINT ( 'NONE',  ( 11.57754556164262993, 8.947311289249686439, -4.715264992745044736 ) ) ;
#112489 = CARTESIAN_POINT ( 'NONE',  ( 6.809632187368197087, -0.4906261968062891055, 2.159508175712351541 ) ) ;
#112490 = CARTESIAN_POINT ( 'NONE',  ( 1.364683531249996529, 10.77604166700806942, 0.7879004041258403923 ) ) ;
#112491 = CARTESIAN_POINT ( 'NONE',  ( 5.320932177894995618, 1.445329238430465013, -1.252218921613167169 ) ) ;
#112492 = CARTESIAN_POINT ( 'NONE',  ( -7.947050595904583403, 12.42330946186405249, 0.7998128361456481317 ) ) ;
#112493 = CARTESIAN_POINT ( 'NONE',  ( 5.632522751473472589, 8.658694745772667289, -1.199719254218440723 ) ) ;
#112494 = CARTESIAN_POINT ( 'NONE',  ( -1.360316468750044638, 1.151041667008095404, -0.7853790794159261068 ) ) ;
#112495 = CARTESIAN_POINT ( 'NONE',  ( 4.324687812634892659, 5.108185871904570519, 1.082531754730560403 ) ) ;
#112496 = CARTESIAN_POINT ( 'NONE',  ( 9.554207839743581232, -7.792803924024971352, -0.03436587256738153628 ) ) ;
#112497 = CARTESIAN_POINT ( 'NONE',  ( 0.7316835000789992938, 1.813914744281470925, 0.3150931809976220133 ) ) ;
#112498 = ORIENTED_EDGE ( 'NONE', *, *, #61376, .T. ) ;
#112499 = FILL_AREA_STYLE_COLOUR ( '', #16457 ) ;
#112500 = CARTESIAN_POINT ( 'NONE',  ( 5.026551685794929725, 1.789549103570491351, 0.5443708928771497924 ) ) ;
#112501 = CARTESIAN_POINT ( 'NONE',  ( -0.02319159430949970999, 4.096340798889516854, -2.366022381217198767 ) ) ;
#112502 = CARTESIAN_POINT ( 'NONE',  ( 6.855582950365507244, 8.027210192628430718, -1.199719254218452047 ) ) ;
#112503 = CARTESIAN_POINT ( 'NONE',  ( 0.000000000000000000, 0.08000000000000020983, 0.000000000000000000 ) ) ;
#112504 = CARTESIAN_POINT ( 'NONE',  ( -5.615968211774352348, 7.384814024763004525, 1.238619054342107839 ) ) ;
#112505 = CARTESIAN_POINT ( 'NONE',  ( -4.772106882330223954, 8.511282429453158827, -0.7216878364870267237 ) ) ;
#112506 = CARTESIAN_POINT ( 'NONE',  ( 2.496672843210871129, 6.064535417054653266, -0.7998128361456291469 ) ) ;
#112507 = CARTESIAN_POINT ( 'NONE',  ( 1.551539110526085619, 1.487754399324931365, 1.290523904849065095 ) ) ;
#112508 = CARTESIAN_POINT ( 'NONE',  ( 3.814077502958601595, 1.076299547611740293, -1.704950967544152984 ) ) ;
#112509 = CARTESIAN_POINT ( 'NONE',  ( -6.184490626128011925, 10.36698949712469364, -0.7998128361456291469 ) ) ;
#112510 = CARTESIAN_POINT ( 'NONE',  ( 3.718679271898170491, 7.560485927181699317, 0.7998128361456271485 ) ) ;
#112511 = CARTESIAN_POINT ( 'NONE',  ( 3.662233025353780480, -1.472007171213615351, 1.623636439255560227 ) ) ;
#112512 = CARTESIAN_POINT ( 'NONE',  ( 9.333041836208478159, 3.553060279300227275, -7.472413793088525935 ) ) ;
#112513 = CARTESIAN_POINT ( 'NONE',  ( -10.63367255181986160, 11.30037282007833532, 1.040834085586084257E-14 ) ) ;
#112514 = DIRECTION ( 'NONE',  ( 0.000000000000000000, -1.000000000000000000, 0.000000000000000000 ) ) ;
#112515 = DIRECTION ( 'NONE',  ( -3.330669073875485398E-16, 1.665334536937734071E-16, 1.000000000000000000 ) ) ;
#112516 = CARTESIAN_POINT ( 'NONE',  ( 3.445180431648323882, 6.073108699348104267, 1.082531754730549078 ) ) ;
#112518 = EDGE_CURVE ( 'NONE', #50089, #139477, #132647, .T. ) ;
#112517 = CARTESIAN_POINT ( 'NONE',  ( 7.202405917357655341, 9.425892875049191488, 1.599625672291281386 ) ) ;
#112519 = CARTESIAN_POINT ( 'NONE',  ( 3.891353782322113375, 4.498666486585943147, -1.199719254218446718 ) ) ;
#112520 = CARTESIAN_POINT ( 'NONE',  ( 6.753369913382843315, 8.011924666102361314, -1.082531754730548412 ) ) ;
#112521 = VERTEX_POINT ( 'NONE', #148490 ) ;
#112523 = CARTESIAN_POINT ( 'NONE',  ( 2.068995670861985658, -1.554830924100785161, 1.278664071131753843 ) ) ;
#112522 = CARTESIAN_POINT ( 'NONE',  ( 4.897927690869709139, -0.6253142351902387652, -1.731941863025769246 ) ) ;
#112524 = CARTESIAN_POINT ( 'NONE',  ( 4.657739267062822819, -0.4975208956916782332, -2.243777209869437517 ) ) ;
#112526 = CARTESIAN_POINT ( 'NONE',  ( 2.623689330893996363, 1.826062842344724269, -0.3576783775682371158 ) ) ;
#112525 = CARTESIAN_POINT ( 'NONE',  ( -0.02919842301646497981, 2.009414862388910983, -2.487882213790572283 ) ) ;
#112527 = CARTESIAN_POINT ( 'NONE',  ( 3.285556943750000514, -2.413541666188708579, 1.896917185911906500 ) ) ;
#112528 = DIRECTION ( 'NONE',  ( 0.000000000000000000, 0.000000000000000000, -1.000000000000000000 ) ) ;
#112529 = CARTESIAN_POINT ( 'NONE',  ( 5.256085721135645095, 0.7693902824621422498, -1.750971482026221437 ) ) ;
#112530 = CARTESIAN_POINT ( 'NONE',  ( -7.808606406466886973, 11.19745900993164511, 1.199719254218453823 ) ) ;
#112531 = CIRCLE ( 'NONE', #105541, 12.00000000000000178 ) ;
#112532 = CARTESIAN_POINT ( 'NONE',  ( -5.641601317062248988, 6.714861303728305586, -1.082531754730549967 ) ) ;
#112534 = CARTESIAN_POINT ( 'NONE',  ( 3.572993900519233712, 0.04689164532409998559, -1.870237235490713079 ) ) ;
#112533 = CARTESIAN_POINT ( 'NONE',  ( 5.284749326355624888, 1.843379893440146633, -0.9865243283948360586 ) ) ;
#112535 = CARTESIAN_POINT ( 'NONE',  ( 5.490689023854504747, 9.349628261231513804, 1.040834085586084257E-14 ) ) ;
#112536 = CARTESIAN_POINT ( 'NONE',  ( 5.407694413872749628, -0.8332299576223768378, -1.642021276980778932 ) ) ;
#112537 = CARTESIAN_POINT ( 'NONE',  ( 3.816783937446950770, 4.411668334231586996, 1.199719254218464037 ) ) ;
#112538 = CARTESIAN_POINT ( 'NONE',  ( 3.469446951953614189E-15, 6.120000000000021423, 1.214306433183764966E-14 ) ) ;
#112539 = CARTESIAN_POINT ( 'NONE',  ( 5.303229652072571021, 1.413297086782526302, 0.9885393367406664078 ) ) ;
#112540 = CARTESIAN_POINT ( 'NONE',  ( -5.215082642750900277, 9.236013516518044142, 0.000000000000000000 ) ) ;
#112541 =( BOUNDED_SURFACE ( )  B_SPLINE_SURFACE ( 3, 2, ( 
 ( #26810, #175225, #62511 ),
 ( #162166, #109214, #211949 ),
 ( #92912, #210886, #60376 ),
 ( #160023, #194645, #195724 ),
 ( #10553, #46287, #209814 ),
 ( #77696, #76627, #112404 ) ),
 .UNSPECIFIED., .F., .F., .T. ) 
 B_SPLINE_SURFACE_WITH_KNOTS ( ( 4, 2, 4 ),
 ( 3, 3 ),
 ( 1.843143693225357538E-18, 0.0009693014523152131655, 0.001938602904630424596 ),
 ( 0.000000000000000000, 1.000000000000000000 ),
 .UNSPECIFIED. ) 
 GEOMETRIC_REPRESENTATION_ITEM ( )  RATIONAL_B_SPLINE_SURFACE ( (
 ( 1.000000000000000000, 0.8462384754710218226, 1.000000000000000000),
 ( 1.000000000000000000, 0.8473855914980132908, 1.000000000000000000),
 ( 1.000000000000000000, 0.8490776175548976346, 1.000000000000000000),
 ( 1.000000000000000000, 0.8506485811854621604, 1.000000000000000000),
 ( 1.000000000000000000, 0.8507605089031664569, 1.000000000000000000),
 ( 1.000000000000000000, 0.8509629433967630385, 1.000000000000000000) ) ) 
 REPRESENTATION_ITEM ( '' )  SURFACE ( )  );
#112542 = CARTESIAN_POINT ( 'NONE',  ( 0.6329805529394582075, 0.5017471949167272571, 1.659931108299773639 ) ) ;
#112543 = CARTESIAN_POINT ( 'NONE',  ( 10.91970695577495754, -9.999999999999994671, 0.08000000000000194456 ) ) ;
#112544 = CARTESIAN_POINT ( 'NONE',  ( 1.913843478179610536, 3.256154753185164452, 0.4414708703499702902 ) ) ;
#112545 = CARTESIAN_POINT ( 'NONE',  ( -1.499999999999997780, 7.388542872122518368, -4.154462424328208670 ) ) ;
#112546 = CARTESIAN_POINT ( 'NONE',  ( 4.821225769315531373, -1.936335391968559527, -0.9821231961690338741 ) ) ;
#112547 = CARTESIAN_POINT ( 'NONE',  ( 3.826616632296374831, 1.734130841282412128, 0.5711148077138239465 ) ) ;
#112548 = CARTESIAN_POINT ( 'NONE',  ( 1.164813196467245904, 1.489159823276710926, -1.277213275948145599 ) ) ;
#112549 = CARTESIAN_POINT ( 'NONE',  ( 6.227753904044541322, 0.8083430201051154951, -1.957153335705215103 ) ) ;
#112551 = CARTESIAN_POINT ( 'NONE',  ( 0.6823417656249917140, 3.655208333674754506, 1.181850606188765695 ) ) ;
#112550 = CARTESIAN_POINT ( 'NONE',  ( 0.3930492761001015967, 1.902410075555853064, -1.278529456123769892 ) ) ;
#112552 = CARTESIAN_POINT ( 'NONE',  ( 1.579999999999999183, 8.674529973577541853, 2.499999999999998668 ) ) ;
#112553 = CARTESIAN_POINT ( 'NONE',  ( 8.697719238366680372, 10.10609285197134533, 1.199719254218462483 ) ) ;
#112554 = CARTESIAN_POINT ( 'NONE',  ( 2.948016456289838771, -1.425740979638410399, -1.569777838261996017 ) ) ;
#112555 = CARTESIAN_POINT ( 'NONE',  ( -3.131570295076647525, 6.597323077657299528, 1.040834085586084257E-14 ) ) ;
#112556 = AXIS2_PLACEMENT_3D ( 'NONE', #128060, #74947, #58695 ) ;
#112557 = CARTESIAN_POINT ( 'NONE',  ( 7.204675194429079505E-15, -1.443749999044083854, -3.475000000000000089 ) ) ;
#112558 = CARTESIAN_POINT ( 'NONE',  ( -4.161989969270909917, 5.878740935614591656, 1.443375672974064550 ) ) ;
#112559 = CARTESIAN_POINT ( 'NONE',  ( 0.5321919801732944988, 1.189095644551215525, 1.694524325727378322 ) ) ;
#112561 = CARTESIAN_POINT ( 'NONE',  ( 1.499999999999997113, 13.67708333401613352, -0.8660254037844378194 ) ) ;
#112560 = CARTESIAN_POINT ( 'NONE',  ( 6.983263157960361234, 4.694303448529787204, 2.516403841208918912 ) ) ;
#112562 = ORIENTED_EDGE ( 'NONE', *, *, #113661, .F. ) ;
#112565 = VERTEX_POINT ( 'NONE', #53103 ) ;
#112564 = CARTESIAN_POINT ( 'NONE',  ( 2.420824200137431603, -0.8528996238171372424, -2.051222908810364842 ) ) ;
#112563 = COLOUR_RGB ( '', 0.66274510, 0.83137255, 0.94901961) ;
#112566 = CARTESIAN_POINT ( 'NONE',  ( 0.2472849680876147149, 2.272430822888141133, -0.3459996173978163725 ) ) ;
#112568 = CARTESIAN_POINT ( 'NONE',  ( 5.840703832811390050, -2.011083492259890360, -0.4572853040550031167 ) ) ;
#112567 = CARTESIAN_POINT ( 'NONE',  ( 3.846762897975340767, 5.510976019103107859, -1.599625672291256295 ) ) ;
#112570 = CARTESIAN_POINT ( 'NONE',  ( -3.475000000000000533, -2.800000000000000266, 0.000000000000000000 ) ) ;
#112569 = CARTESIAN_POINT ( 'NONE',  ( 6.042093733545556233, 7.078139439671806699, -1.199719254218452047 ) ) ;
#112571 = CARTESIAN_POINT ( 'NONE',  ( 6.062430963966053632, 7.101866208495718702, -1.199719254218452047 ) ) ;
#112572 = ADVANCED_FACE ( 'NONE', ( #166865 ), #195075, .T. ) ;
#112573 = CARTESIAN_POINT ( 'NONE',  ( 0.2331563151865729544, 6.948071805571808035, -2.540803835148666145 ) ) ;
#112574 = CARTESIAN_POINT ( 'NONE',  ( 5.653808312887880660, 0.7519890275384639722, 1.680886247995525773 ) ) ;
#112575 = CARTESIAN_POINT ( 'NONE',  ( 4.878236342818665250, 4.585697242910212523, 1.040834085586084257E-14 ) ) ;
#112576 = CARTESIAN_POINT ( 'NONE',  ( 2.379564082050821483, 1.058669913282745956, 1.361546577445968964 ) ) ;
#112577 = CARTESIAN_POINT ( 'NONE',  ( 1.059780186608853203, 1.205045252304644210, 1.616690996016925563 ) ) ;
#112578 = CARTESIAN_POINT ( 'NONE',  ( 2.110373620506571957, 0.004507209458638748376, 2.298851035670963050 ) ) ;
#112579 = CARTESIAN_POINT ( 'NONE',  ( -1.364683531250012516, 4.301041667008089320, -0.7879004041258300672 ) ) ;
#112580 = CARTESIAN_POINT ( 'NONE',  ( 2.126610404160976575, 1.303795175273964269, -1.848758590024823123 ) ) ;
#112581 = CARTESIAN_POINT ( 'NONE',  ( 3.598352328373265685, -2.103663943315597251, -0.1031874809700270568 ) ) ;
#112582 = CARTESIAN_POINT ( 'NONE',  ( -4.228163802615396705, 6.026220084508304708, -1.599625672291271394 ) ) ;
#112583 = CARTESIAN_POINT ( 'NONE',  ( 2.301682877085888368, -1.769492147959438322, 0.03813942612425345879 ) ) ;
#112585 = EDGE_CURVE ( 'NONE', #4447, #191630, #7974, .T. ) ;
#112584 = CARTESIAN_POINT ( 'NONE',  ( 4.638861114170084399, 8.563755066507100722, 0.7998128361456462443 ) ) ;
#112587 = CARTESIAN_POINT ( 'NONE',  ( 5.794527259016318155, 1.876155144389481721, -1.316939630280162365 ) ) ;
#112586 = CARTESIAN_POINT ( 'NONE',  ( 4.367134876933267407, 8.109091433148536865, 0.000000000000000000 ) ) ;
#112588 = CARTESIAN_POINT ( 'NONE',  ( 4.048646477676579813, -1.531818510360350327, -1.021117339664041834 ) ) ;
#112589 = CARTESIAN_POINT ( 'NONE',  ( -3.574546055497324737, 7.322054164722185732, 0.7998128361456341429 ) ) ;
#112590 = CARTESIAN_POINT ( 'NONE',  ( 6.778713616708431644, 7.010846762355714468, 1.040834085586084257E-14 ) ) ;
#112591 = CARTESIAN_POINT ( 'NONE',  ( -1.500000000000011324, 3.420833333333355597, 0.8660254037844403729 ) ) ;
#112592 = CARTESIAN_POINT ( 'NONE',  ( 4.576244502665470115, -2.125281509430646754, -0.5339713055512520512 ) ) ;
#112593 = CARTESIAN_POINT ( 'NONE',  ( -4.141125853970233806, 6.918731698685530063, -1.199719254218452047 ) ) ;
#112594 = CARTESIAN_POINT ( 'NONE',  ( 0.2734184563537064849, 7.240553437303591799, -1.983365796752657007 ) ) ;
#112595 = LINE ( 'NONE', #212135, #7301 ) ;
#112596 = CARTESIAN_POINT ( 'NONE',  ( 0.6823417656249899377, 4.676041667008086655, -1.181850606188754593 ) ) ;
#112597 = CARTESIAN_POINT ( 'NONE',  ( 2.666528119303875233, -1.328299865307873695, 1.395581591625531193 ) ) ;
#112598 = CARTESIAN_POINT ( 'NONE',  ( 1.364683531249997417, 8.984375000341396245, 2.602085213965210642E-15 ) ) ;
#112600 = CARTESIAN_POINT ( 'NONE',  ( -3.307826292054304673, 6.802955074131234348, -0.7216878364870267237 ) ) ;
#112599 = AXIS2_PLACEMENT_3D ( 'NONE', #132177, #168893, #87654 ) ;
#112601 = CARTESIAN_POINT ( 'NONE',  ( 5.273731010124149243, 0.4114677744767555878, -2.080124947408354963 ) ) ;
#112602 = CARTESIAN_POINT ( 'NONE',  ( -6.970300371201519241, 7.304640985922785212, 0.7216878364870317197 ) ) ;
#112603 = ORIENTED_EDGE ( 'NONE', *, *, #90038, .F. ) ;
#112604 = CARTESIAN_POINT ( 'NONE',  ( -4.990809943606281607, 6.915973915664348937, -1.443375672974066548 ) ) ;
#112605 = CARTESIAN_POINT ( 'NONE',  ( 4.517891501851804215, 6.293959390292322986, -1.599625672291255185 ) ) ;
#112606 = CARTESIAN_POINT ( 'NONE',  ( 5.987831981441137152, -1.833028718050220940, -0.1737628300680846560 ) ) ;
#112607 = CARTESIAN_POINT ( 'NONE',  ( 1.220146605508150803E-14, 11.21875000068279249, -1.499999999999998446 ) ) ;
#112608 = FACE_OUTER_BOUND ( 'NONE', #107849, .T. ) ;
#112609 = CARTESIAN_POINT ( 'NONE',  ( -1.201851678989727383E-14, 3.509375000341421469, -1.575800808251660134 ) ) ;
#112610 = CARTESIAN_POINT ( 'NONE',  ( 1.874151978141885833, -0.08570891532005876778, -1.738468184182701881 ) ) ;
#112611 = CARTESIAN_POINT ( 'NONE',  ( 0.3089402658475807195, -1.578002999302514642, 1.165503548361209063 ) ) ;
#112612 = CARTESIAN_POINT ( 'NONE',  ( 1.364683531249986537, 0.1760416670080860446, 0.7879004041258500513 ) ) ;
#112613 = CARTESIAN_POINT ( 'NONE',  ( -1.500000000000038636, 7.000000000000000000, -10.64483442802187874 ) ) ;
#112614 = CARTESIAN_POINT ( 'NONE',  ( 6.051685545382852638, 0.6321331830463626789, -2.067208725892249799 ) ) ;
#112615 = CARTESIAN_POINT ( 'NONE',  ( -10.14557902172788495, 10.73093036830436553, 1.040834085586084257E-14 ) ) ;
#112616 = EDGE_CURVE ( 'NONE', #184155, #198714, #153329, .T. ) ;
#112617 = CARTESIAN_POINT ( 'NONE',  ( -5.355107487273497391, 9.191449801886996340, 0.7216878364870458196 ) ) ;
#112618 = AXIS2_PLACEMENT_3D ( 'NONE', #74883, #108513, #140990 ) ;
#112619 = CARTESIAN_POINT ( 'NONE',  ( 5.981359018292748075, 1.999130597612966742, -0.8229454869796914984 ) ) ;
#112621 = ORIENTED_EDGE ( 'NONE', *, *, #24605, .F. ) ;
#112620 = CARTESIAN_POINT ( 'NONE',  ( 0.000000000000000000, 1.000000000000000888, 0.000000000000000000 ) ) ;
#112622 = CARTESIAN_POINT ( 'NONE',  ( -1.201851678989727383E-14, 4.696875000341419693, -1.575800808251660134 ) ) ;
#112623 = CARTESIAN_POINT ( 'NONE',  ( 6.819606788702130551, -1.912791534441590668, 0.4766558377571166183 ) ) ;
#112624 = CARTESIAN_POINT ( 'NONE',  ( 6.362590153729421161, -0.5805357501837383749, 1.633877867761362124 ) ) ;
#112626 = CARTESIAN_POINT ( 'NONE',  ( 3.527062600443749307, -2.024233912922444478, 0.8403589366152917073 ) ) ;
#112625 = CARTESIAN_POINT ( 'NONE',  ( -2.754243431018125239E-14, 0.2031250003414269978, 1.570758158831750295 ) ) ;
#112627 = CARTESIAN_POINT ( 'NONE',  ( 3.259088711995949517, -1.748676463734340603, 1.505793948229345869 ) ) ;
#112628 = CARTESIAN_POINT ( 'NONE',  ( 6.204382384804184802, -0.7375479284208189545, -1.924474620761642996 ) ) ;
#112629 = CARTESIAN_POINT ( 'NONE',  ( 1.605311038211139740, -1.927294583035423114, 0.2376585312828301821 ) ) ;
#112630 = CARTESIAN_POINT ( 'NONE',  ( -5.219525951136845698, 8.072902128759544382, -1.082531754730543971 ) ) ;
#112631 = AXIS2_PLACEMENT_3D ( 'NONE', #199843, #102353, #135933 ) ;
#112632 = CARTESIAN_POINT ( 'NONE',  ( -0.3199376857465079937, -8.148349307653480977, -9.520891725236014125 ) ) ;
#112633 = CARTESIAN_POINT ( 'NONE',  ( -6.773846765317340868, -7.246166700180801001, -6.773846765317301788 ) ) ;
#112634 = CARTESIAN_POINT ( 'NONE',  ( 3.779626292077961747, 0.2561244552635975058, -2.104982076983111572 ) ) ;
#112635 = DIRECTION ( 'NONE',  ( 0.000000000000000000, 0.000000000000000000, -1.000000000000000000 ) ) ;
#112636 = CARTESIAN_POINT ( 'NONE',  ( 2.654922836763852878, 1.081066371885472277, 1.701947380796410059 ) ) ;
#112637 = CARTESIAN_POINT ( 'NONE',  ( -4.541618270453545492, 8.242379048930368768, 0.7216878364870458196 ) ) ;
#112638 = CARTESIAN_POINT ( 'NONE',  ( 4.489439581592091777, 1.972811803287272348, -0.9889974963176446643 ) ) ;
#112639 = CARTESIAN_POINT ( 'NONE',  ( 0.000000000000000000, -0.2843749995220433702, -3.793834371823813001 ) ) ;
#112640 = CARTESIAN_POINT ( 'NONE',  ( -2.004536931766795593, -3.116556058128074902, -2.754590913354557635 ) ) ;
#112641 = CARTESIAN_POINT ( 'NONE',  ( 0.01192831195480706721, -0.7772932952810689411, -1.650495136788888040 ) ) ;
#112642 = CARTESIAN_POINT ( 'NONE',  ( 2.535011536075336913, 5.133042487381361596, -7.499999999999997335 ) ) ;
#112644 = CARTESIAN_POINT ( 'NONE',  ( 6.825078400183555161, 2.003297025668087983, 2.546134486959560572 ) ) ;
#112643 = CARTESIAN_POINT ( 'NONE',  ( -5.435611771797328906, 7.629049766310559200, 1.344574814272103236 ) ) ;
#112645 = CARTESIAN_POINT ( 'NONE',  ( 0.000000000000000000, 0.000000000000000000, 0.000000000000000000 ) ) ;
#112646 = ORIENTED_EDGE ( 'NONE', *, *, #130897, .F. ) ;
#112647 = CARTESIAN_POINT ( 'NONE',  ( 4.610263661134276880, -0.8792652907330700263, -1.864042625929088759 ) ) ;
#112648 = CARTESIAN_POINT ( 'NONE',  ( -1.360316468750034868, 2.619791667008062319, -0.7853790794159261068 ) ) ;
#112649 = DIRECTION ( 'NONE',  ( -0.000000000000000000, 1.000000000000000000, -0.000000000000000000 ) ) ;
#112650 = CARTESIAN_POINT ( 'NONE',  ( -4.066556009095094737, 6.831733546331167695, 1.199719254218464037 ) ) ;
#112651 = CARTESIAN_POINT ( 'NONE',  ( -4.655245641445871385, 6.524482229810530498, 1.599625672291263179 ) ) ;
#112652 = CARTESIAN_POINT ( 'NONE',  ( 2.877608074518396286, 0.2940240112025078179, -1.998017427383149913 ) ) ;
#112653 = CARTESIAN_POINT ( 'NONE',  ( -0.7500000000000006661, 0.6083333333333564852, -1.299038105676652011 ) ) ;
#112655 = CARTESIAN_POINT ( 'NONE',  ( 7.443063144222396232, 11.62739806832741785, 1.040834085586084257E-14 ) ) ;
#112654 = CARTESIAN_POINT ( 'NONE',  ( -4.305596300791617814, 7.180890229968955651, 1.199719254218452935 ) ) ;
#112656 = CARTESIAN_POINT ( 'NONE',  ( 5.621827251160867789, 9.710548892996357040, 1.040834085586084257E-14 ) ) ;
#112657 = CARTESIAN_POINT ( 'NONE',  ( 3.555589940775650604, 0.5024415226424256975, -1.998565159594118068 ) ) ;
#112658 = CARTESIAN_POINT ( 'NONE',  ( 2.813125141109920069, 1.117832431973438734, -1.678005364621336426 ) ) ;
#112659 = CARTESIAN_POINT ( 'NONE',  ( 1.874158809982179319, 3.299964346911585356, -0.3999999999999993006 ) ) ;
#112660 = CARTESIAN_POINT ( 'NONE',  ( 4.333802657862601215, 8.207853534148366492, 0.7998128361456462443 ) ) ;
#112662 = ORIENTED_EDGE ( 'NONE', *, *, #150919, .F. ) ;
#112661 = CARTESIAN_POINT ( 'NONE',  ( -0.2555917649598457575, 7.163498069672973756, -2.096924645512515895 ) ) ;
#112663 = CARTESIAN_POINT ( 'NONE',  ( 0.8668490835730925381, 1.774987751554598869, -0.4888055736953432207 ) ) ;
#112664 = CARTESIAN_POINT ( 'NONE',  ( 0.01296380302724577452, -0.9916191462571806170, -2.081274906121612034 ) ) ;
#112665 = CARTESIAN_POINT ( 'NONE',  ( 5.357406976055401948, 6.279338222599979424, 1.199719254218452935 ) ) ;
#112666 = CARTESIAN_POINT ( 'NONE',  ( 2.688937055384226671, -0.3666181952855402382, -2.130111032054008646 ) ) ;
#112667 = CARTESIAN_POINT ( 'NONE',  ( -2.928197990871687306, 5.399686175116803710, 1.082531754730560403 ) ) ;
#112668 = CARTESIAN_POINT ( 'NONE',  ( 4.487589638097394307, -0.5612149057237262317, 2.041579019078069379 ) ) ;
#112669 = CARTESIAN_POINT ( 'NONE',  ( 2.847332689139534523, -1.183592279326161290, 1.970102427710369808 ) ) ;
#112670 = CARTESIAN_POINT ( 'NONE',  ( -11.89942855770814134, 11.29999999999999893, -0.7000000000000009548 ) ) ;
#112671 = CARTESIAN_POINT ( 'NONE',  ( 1.182252951876180180, -1.824241171369020531, -0.4133900166373091767 ) ) ;
#112672 = CARTESIAN_POINT ( 'NONE',  ( 4.469576204829595945, 1.912561584401346604, -0.4778803491252373026 ) ) ;
#112673 = CARTESIAN_POINT ( 'NONE',  ( 4.135954056172497673, 2.015980767636461835, -0.05432360925018697717 ) ) ;
#112675 = CARTESIAN_POINT ( 'NONE',  ( 8.541273586484978253, 12.90864358430044589, 0.000000000000000000 ) ) ;
#112674 = CARTESIAN_POINT ( 'NONE',  ( -1.364683531250012516, 2.780208333674754506, 0.7879004041258379498 ) ) ;
#112677 = CARTESIAN_POINT ( 'NONE',  ( 6.428360055892773595, 1.214212339677790409, -1.720619796903441578 ) ) ;
#112676 = CARTESIAN_POINT ( 'NONE',  ( -6.470265622219711688, 8.571729197388226140, -1.599625672291263179 ) ) ;
#112678 = CARTESIAN_POINT ( 'NONE',  ( 6.250451049865752395, -2.060019788584551481, -0.2068627631737207651 ) ) ;
#112679 = CARTESIAN_POINT ( 'NONE',  ( 6.979750152936881058, 7.037463354714830643, 0.7998128361456341429 ) ) ;
#112680 = CARTESIAN_POINT ( 'NONE',  ( -6.901263884555985051, 8.010228272525461435, 1.199719254218450271 ) ) ;
#112681 = CARTESIAN_POINT ( 'NONE',  ( 6.539320575229274901, 4.692178491785949923, 2.665866134390063813 ) ) ;
#112682 = CARTESIAN_POINT ( 'NONE',  ( 4.733256667524862848, -1.802829663221987788, 0.7981805449851049339 ) ) ;
#112683 = CARTESIAN_POINT ( 'NONE',  ( 6.011974661143067777, -0.6766988549865710079, 1.903214300750865506 ) ) ;
#112684 = CARTESIAN_POINT ( 'NONE',  ( -1.500000000000015099, 0.4104166673494891726, -0.8660254037844383745 ) ) ;
#112685 = CARTESIAN_POINT ( 'NONE',  ( 4.987122935671228774, -0.2785958505117277495, -2.290767236937583995 ) ) ;
#112686 = CARTESIAN_POINT ( 'NONE',  ( 1.622013285028017338, 2.032735996446675131, -0.3486163383695956575 ) ) ;
#112687 = CARTESIAN_POINT ( 'NONE',  ( 7.836249599018724865, 9.205007956019091608, -1.082531754730537976 ) ) ;
#112688 = CARTESIAN_POINT ( 'NONE',  ( 5.987861119090863049, 7.014868056141362551, 1.199719254218452047 ) ) ;
#112689 = CARTESIAN_POINT ( 'NONE',  ( 4.278479993564246797, 7.149254538203735798, 1.199719254218452047 ) ) ;
#112690 = CARTESIAN_POINT ( 'NONE',  ( 0.6823417656249882723, 1.988541667008083991, -1.181850606188749264 ) ) ;
#112691 = CARTESIAN_POINT ( 'NONE',  ( 3.607351389687783794, 6.366271167014519783, 1.199719254218451159 ) ) ;
#112692 = CARTESIAN_POINT ( 'NONE',  ( 5.870317324592803310, 7.871789516823500144, -1.443375672974057666 ) ) ;
#112693 = CARTESIAN_POINT ( 'NONE',  ( 4.563029256048502624, 1.681186374793992355, -1.373936881898863982 ) ) ;
#112694 = CARTESIAN_POINT ( 'NONE',  ( -3.241630445535677918, -0.8887487162373168825, -0.5775286854858272534 ) ) ;
#112696 = CARTESIAN_POINT ( 'NONE',  ( 3.561895345837225779, -1.234009368583251387, 1.366721199326895952 ) ) ;
#112695 = CARTESIAN_POINT ( 'NONE',  ( -4.297571505851936813, 4.116180966356429494, 1.214306433183764966E-14 ) ) ;
#112698 = FACE_OUTER_BOUND ( 'NONE', #108502, .T. ) ;
#112697 = CARTESIAN_POINT ( 'NONE',  ( 1.364683531249988535, 4.655208333674755394, -0.7879004041258300672 ) ) ;
#112699 = CARTESIAN_POINT ( 'NONE',  ( 5.935146830689759234, -1.586316731616247200, -1.512381816529739353 ) ) ;
#112700 = CARTESIAN_POINT ( 'NONE',  ( 1.499999999999963141, 7.750000000000000000, -9.886859966642596476 ) ) ;
#112701 = CARTESIAN_POINT ( 'NONE',  ( 5.594667793837476033, -0.5436135106791986082, -2.196135934016548052 ) ) ;
#112702 = VERTEX_POINT ( 'NONE', #131801 ) ;
#112703 = CARTESIAN_POINT ( 'NONE',  ( -5.030466903028923298, 6.770262730772157234, -1.447917484242104758 ) ) ;
#112704 = CARTESIAN_POINT ( 'NONE',  ( 4.817101577040221905, 8.228953320636518853, 0.8951067572735508238 ) ) ;
#112705 = CARTESIAN_POINT ( 'NONE',  ( -6.604230223188181093, 6.877559146573883453, 0.7216878364870317197 ) ) ;
#112706 = CARTESIAN_POINT ( 'NONE',  ( -3.172739462086278550, 6.087116567132428990, 0.9300064228868381022 ) ) ;
#112707 = CARTESIAN_POINT ( 'NONE',  ( 0.4964904254905980197, 1.474999729349553590, -0.9777959528048956184 ) ) ;
#112708 = CARTESIAN_POINT ( 'NONE',  ( 5.777995030156034773, 1.982912992605226465, -0.3464542934713372158 ) ) ;
#112709 = CARTESIAN_POINT ( 'NONE',  ( 3.821394775679032740, -0.1568257194812898159, 2.100186923160925812 ) ) ;
#112710 = CARTESIAN_POINT ( 'NONE',  ( 2.354979200267411255, 0.09147625538302081583, -1.913532508166473800 ) ) ;
#112711 = CARTESIAN_POINT ( 'NONE',  ( 2.496672843210871129, 6.064535417054653266, -0.7998128361456291469 ) ) ;
#112712 = CARTESIAN_POINT ( 'NONE',  ( 3.139063269091638908, -0.1420806666206550495, -1.964468959564101613 ) ) ;
#112713 = CARTESIAN_POINT ( 'NONE',  ( 5.959241620951676310, -1.704104911329520800, 1.083944116985413819 ) ) ;
#112714 = CARTESIAN_POINT ( 'NONE',  ( 1.902992089709685031, 1.553661375375714471, 1.041555772207984676 ) ) ;
#112715 = CARTESIAN_POINT ( 'NONE',  ( 2.312880826517309085, -1.518475810973318074, 1.242258525517292433 ) ) ;
#112718 = ORIENTED_EDGE ( 'NONE', *, *, #14697, .T. ) ;
#112717 = CARTESIAN_POINT ( 'NONE',  ( 0.8614045922798494459, -1.509235727096858826, -1.174430983434850972 ) ) ;
#112716 = CARTESIAN_POINT ( 'NONE',  ( 3.896855043588220546, 1.455827857355775246, -0.9247512240674607975 ) ) ;
#112720 = CARTESIAN_POINT ( 'NONE',  ( 4.853455804012212660, 7.645820290447483458, 1.082531754730558626 ) ) ;
#112719 = CARTESIAN_POINT ( 'NONE',  ( 1.700138637298425737, -0.7412910010123253679, 2.078789392164873906 ) ) ;
#112721 = ADVANCED_FACE ( 'NONE', ( #85128 ), #151214, .F. ) ;
#112722 = CARTESIAN_POINT ( 'NONE',  ( -1.364683531250012516, 2.092708333674750953, 0.7879004041258379498 ) ) ;
#112723 = PRODUCT_RELATED_PRODUCT_CATEGORY ( 'part', '', ( #92073 ) ) ;
#112724 = CARTESIAN_POINT ( 'NONE',  ( 7.727257484784855635, 11.10255193463598111, -1.199719254218446718 ) ) ;
#112726 = CARTESIAN_POINT ( 'NONE',  ( 11.84103413958623818, 11.11004478473146229, 1.443924719788817423 ) ) ;
#112725 = COLOUR_RGB ( '', 0.08235294, 0.09019608, 0.10196078) ;
#112727 = CARTESIAN_POINT ( 'NONE',  ( 0.3999999999999941380, 3.949999999999995293, 0.4999999999999501510 ) ) ;
#112728 = CARTESIAN_POINT ( 'NONE',  ( -0.1950010711912115446, 2.645508648321929002, -2.067621631602482690 ) ) ;
#112729 = DIRECTION ( 'NONE',  ( -3.347138415753902517E-16, -0.6000000000000019762, -0.7999999999999986011 ) ) ;
#112730 = CARTESIAN_POINT ( 'NONE',  ( 0.3442982867475213871, -0.9772804826688463731, 1.825211318103404867 ) ) ;
#112732 = CARTESIAN_POINT ( 'NONE',  ( 1.499999999999989120, 1.525000000000019451, 0.000000000000000000 ) ) ;
#112731 = CIRCLE ( 'NONE', #43570, 0.08000000000000020983 ) ;
#112733 = CARTESIAN_POINT ( 'NONE',  ( 5.587931867126699537, 9.671004278289832001, -0.7998128361456291469 ) ) ;
#112734 = CARTESIAN_POINT ( 'NONE',  ( -7.395082721250053837, 10.71501471051202614, -1.199719254218446718 ) ) ;
#112735 = CARTESIAN_POINT ( 'NONE',  ( 4.044074958626150185, 7.940114228364351767, 0.7998128361456271485 ) ) ;
#112736 = CARTESIAN_POINT ( 'NONE',  ( 5.760427271636393343, 2.118038551301495875, 0.1041057254967461404 ) ) ;
#112737 = CARTESIAN_POINT ( 'NONE',  ( 4.248501033035879004, 6.049946853332221153, -1.599625672291273171 ) ) ;
#112738 = CARTESIAN_POINT ( 'NONE',  ( -1.201851678989727383E-14, 2.696875000341417916, -1.575800808251660134 ) ) ;
#112739 = CARTESIAN_POINT ( 'NONE',  ( -1.500000000000011324, 4.379166666666688634, -0.8660254037844313801 ) ) ;
#112741 = CARTESIAN_POINT ( 'NONE',  ( 2.496672843210871129, 6.064535417054653266, -0.7998128361456291469 ) ) ;
#112740 = CARTESIAN_POINT ( 'NONE',  ( 5.898874287966751950, 0.3812104124719677412, 1.924297140916144233 ) ) ;
#112742 = CARTESIAN_POINT ( 'NONE',  ( 3.831407535526813124, -1.356092489331266027, 1.492026659919619025 ) ) ;
#112743 = CARTESIAN_POINT ( 'NONE',  ( 3.608511690770484837, 1.820787697044351505, 0.5958877267112758780 ) ) ;
#112744 = CARTESIAN_POINT ( 'NONE',  ( 1.681448347407452193, 1.514353137444489406, 1.584415833815432162 ) ) ;
#112745 =( BOUNDED_CURVE ( )  B_SPLINE_CURVE ( 2, ( #198712, #180361, #82847, #68707, #164121, #66564, #3696, #48252, #16763 ),
 .UNSPECIFIED., .F., .T. ) 
 B_SPLINE_CURVE_WITH_KNOTS ( ( 3, 2, 2, 2, 3 ),
 ( 0.1093749999999997641, 0.1145833333333333287, 0.1250000000000000000, 0.1354166666666666574, 0.1406250000000002776 ),
 .UNSPECIFIED. ) 
 CURVE ( )  GEOMETRIC_REPRESENTATION_ITEM ( )  RATIONAL_B_SPLINE_CURVE ( ( 0.9330127018922194093, 0.9330127018922163007, 1.000000000000000000, 0.8660254037844387076, 1.000000000000000000, 0.8660254037844387076, 1.000000000000000000, 0.9330127018922158566, 0.9330127018922194093 ) ) 
 REPRESENTATION_ITEM ( '' )  );
#112746 = CARTESIAN_POINT ( 'NONE',  ( 0.1394461523056788055, 0.009327122704651916868, -1.719853553173174010 ) ) ;
#112747 = CARTESIAN_POINT ( 'NONE',  ( -1.402160292154681736E-14, 1.368750000682821710, -1.732050807568863648 ) ) ;
#112748 = CARTESIAN_POINT ( 'NONE',  ( 5.027594669734884114, -0.2912581947275821315, 1.991892893239319617 ) ) ;
#112749 = CARTESIAN_POINT ( 'NONE',  ( -5.194745412330402878, 9.212286747694129474, 0.000000000000000000 ) ) ;
#112751 = CARTESIAN_POINT ( 'NONE',  ( 5.747700551816460113, 2.085811977426319519, -0.3625847027708250514 ) ) ;
#112750 = CARTESIAN_POINT ( 'NONE',  ( -3.090895834235680262, 5.589500325708124606, 1.082531754730560403 ) ) ;
#112752 = CARTESIAN_POINT ( 'NONE',  ( -1.046564900588939029, 13.26134948416639148, -1.059077843570422672 ) ) ;
#112754 = CARTESIAN_POINT ( 'NONE',  ( -8.120407659942227241, 8.438506789546210030, 0.7998128361456341429 ) ) ;
#112753 = CARTESIAN_POINT ( 'NONE',  ( 2.911755628046075906, -1.032623549580795608, -1.817877418097467501 ) ) ;
#112756 = ORIENTED_EDGE ( 'NONE', *, *, #96950, .T. ) ;
#112755 = CARTESIAN_POINT ( 'NONE',  ( 1.359898630301906053, 0.6939498547450100308, 1.579201994853156821 ) ) ;
#112757 = CARTESIAN_POINT ( 'NONE',  ( 5.853796514643677007, -1.537196951383312804, -1.461068456062891041 ) ) ;
#112758 = CARTESIAN_POINT ( 'NONE',  ( 7.122110765880372618, 7.203550736482235095, 0.7998128361456341429 ) ) ;
#112759 =( NAMED_UNIT ( * ) PLANE_ANGLE_UNIT ( ) SI_UNIT ( $, .RADIAN. ) );
#112760 = CARTESIAN_POINT ( 'NONE',  ( 6.661184041420942670, -7.473374494058216300, -6.773376349083130243 ) ) ;
#112762 = CARTESIAN_POINT ( 'NONE',  ( 7.551528372687370094, 11.75394083486988528, -0.7216878364870267237 ) ) ;
#112761 = CARTESIAN_POINT ( 'NONE',  ( 5.459129407796876166, 9.520734742405036144, 1.040834085586084257E-14 ) ) ;
#112763 = VERTEX_POINT ( 'NONE', #24371 ) ;
#112764 = DIRECTION ( 'NONE',  ( 1.207943261119674327E-30, 2.168404344971008079E-15, -1.000000000000000000 ) ) ;
#112766 = CARTESIAN_POINT ( 'NONE',  ( 2.068756839025966521, -1.399621434743709703, 1.149952615172030512 ) ) ;
#112765 = CARTESIAN_POINT ( 'NONE',  ( 6.879836604291781121, 6.991173891287354003, -0.7998128361456341429 ) ) ;
#112768 = CARTESIAN_POINT ( 'NONE',  ( -5.669280788808708671, 9.765911353585494226, 0.7998128361456481317 ) ) ;
#112767 = CIRCLE ( 'NONE', #102320, 2.250000000000000444 ) ;
#112769 = ORIENTED_EDGE ( 'NONE', *, *, #114112, .T. ) ;
#112770 = CARTESIAN_POINT ( 'NONE',  ( 2.703961570921634028, 5.242040035128820108, -1.199719254218446718 ) ) ;
#112771 = ORIENTED_EDGE ( 'NONE', *, *, #57003, .T. ) ;
#112772 = CARTESIAN_POINT ( 'NONE',  ( 6.561219994370630637, 6.619454513046008515, 0.000000000000000000 ) ) ;
#112773 = CARTESIAN_POINT ( 'NONE',  ( 2.174188805400371294, 0.7754062184415695391, 1.637274071133995035 ) ) ;
#112774 = CARTESIAN_POINT ( 'NONE',  ( 6.539320575229291777, 2.092415259949731432, 2.107292781797183601 ) ) ;
#112775 = PRESENTATION_STYLE_ASSIGNMENT (( #82316 ) ) ;
#112776 = CARTESIAN_POINT ( 'NONE',  ( 4.490901714065265615, 7.023505696618186356, 1.148426366857359771 ) ) ;
#112777 = CARTESIAN_POINT ( 'NONE',  ( 4.510102262511601623, 1.860682779278443277, -0.04454786357706643635 ) ) ;
#112778 = CARTESIAN_POINT ( 'NONE',  ( 0.7728743906838764222, 1.688931763573727540, -0.9039392725495792869 ) ) ;
#112779 = CARTESIAN_POINT ( 'NONE',  ( 0.3756504392133250825, 1.046533627790873000, 1.495644344755318045 ) ) ;
#112780 = LINE ( 'NONE', #211259, #204734 ) ;
#112781 = DIRECTION ( 'NONE',  ( -2.126226658603517140E-31, 1.665334536937738015E-16, 1.000000000000000000 ) ) ;
#112782 = AXIS2_PLACEMENT_3D ( 'NONE', #83417, #19474, #201412 ) ;
#112783 = CARTESIAN_POINT ( 'NONE',  ( 4.716601407767927689, 8.224641112169805979, 0.6639617910879731522 ) ) ;
#112784 = CARTESIAN_POINT ( 'NONE',  ( -3.145128448690317935, 5.652771709238564313, -1.082531754730549967 ) ) ;
#112785 = CARTESIAN_POINT ( 'NONE',  ( 7.565086526745395723, 10.80938946696957004, -1.082531754730543083 ) ) ;
#112786 = CARTESIAN_POINT ( 'NONE',  ( 4.680490344776488065, 1.214988973509235848, -1.549875580164503663 ) ) ;
#112787 = CARTESIAN_POINT ( 'NONE',  ( -4.741601036477307574, 6.554953847355395880, 1.599625672291267398 ) ) ;
#112788 = AXIS2_PLACEMENT_3D ( 'NONE', #207396, #26509, #94745 ) ;
#112789 = CARTESIAN_POINT ( 'NONE',  ( 6.650331627364351128, -1.696677047125955795, 1.386650686450926484 ) ) ;
#112790 = CARTESIAN_POINT ( 'NONE',  ( 5.842784322950494769, 0.3761301977728331858, 1.889152344147272178 ) ) ;
#112791 = CARTESIAN_POINT ( 'NONE',  ( -7.477485413136760073, 8.682486722536401302, -1.199719254218446718 ) ) ;
#112792 = CARTESIAN_POINT ( 'NONE',  ( -0.9782388782689013240, 3.999999999999989786, -0.3999999999999993006 ) ) ;
#112793 = CARTESIAN_POINT ( 'NONE',  ( 2.139570144280181108, -1.970530345926827742, 0.9937953903183870397 ) ) ;
#112794 = CARTESIAN_POINT ( 'NONE',  ( -6.147147853355845015, 6.992553514990425434, 0.9364138244793998034 ) ) ;
#112795 = CARTESIAN_POINT ( 'NONE',  ( 0.3164790345465406385, -0.6463921985436006379, -1.799943259716822341 ) ) ;
#112796 = ORIENTED_EDGE ( 'NONE', *, *, #102912, .T. ) ;
#112797 = EDGE_LOOP ( 'NONE', ( #128249, #30017, #102654, #209249 ) ) ;
#112798 = CARTESIAN_POINT ( 'NONE',  ( 0.1390025477998011738, -0.1451226239368992033, -1.937570863154890688 ) ) ;
#112799 = CARTESIAN_POINT ( 'NONE',  ( 1.786567547031367775, 1.688677558619257058, -0.9590575663266877049 ) ) ;
#112800 = VERTEX_POINT ( 'NONE', #121987 ) ;
#112801 = CARTESIAN_POINT ( 'NONE',  ( 0.8255457999647041190, -1.462224166115761337, 1.388270745661695837 ) ) ;
#112803 = CARTESIAN_POINT ( 'NONE',  ( 5.242936282186112962, -0.2253732266207208457, -1.847139840844784775 ) ) ;
#112802 = CARTESIAN_POINT ( 'NONE',  ( -5.010620288702242853, 8.003418215864698482, -1.199719254218453823 ) ) ;
#112804 = CARTESIAN_POINT ( 'NONE',  ( 6.710359684120930091, 6.793450817754725257, 0.7998128361456352531 ) ) ;
#112805 = CARTESIAN_POINT ( 'NONE',  ( 1.499999999999993117, 11.35416666666666785, 0.8660254037844408170 ) ) ;
#112806 = CARTESIAN_POINT ( 'NONE',  ( 6.509000000000014552, 2.444259026362519904, 2.383015625331697862 ) ) ;
#112808 = B_SPLINE_CURVE_WITH_KNOTS ( 'NONE', 3,
 ( #174312, #138602, #55209, #156988, #141832, #187330, #58406, #54144, #5345, #71427, #153775, #40029, #121355, #155912, #73581, #105042 ),
 .UNSPECIFIED., .F., .F.,
 ( 4, 2, 2, 2, 2, 2, 2, 4 ),
 ( 0.9998645410539588330, 1.009348164353689681, 1.018831787653420529, 1.037799034252882224, 1.075733527451805616, 1.113668020650729007, 1.132635267250190703, 1.151602513849652398 ),
 .UNSPECIFIED. ) ;
#112807 = CARTESIAN_POINT ( 'NONE',  ( -4.717347382551060342, 7.590990148696470818, 1.199719254218464037 ) ) ;
#112809 = CARTESIAN_POINT ( 'NONE',  ( -6.749980374757255319, 8.968339418673846097, 1.599625672291269396 ) ) ;
#112810 = CARTESIAN_POINT ( 'NONE',  ( 1.839652601550560096, 0.8350199954420146620, -2.026445374841173930 ) ) ;
#112811 = CARTESIAN_POINT ( 'NONE',  ( 4.528060117284244512, 4.385084346360807572, 0.7216878364870317197 ) ) ;
#112812 = CARTESIAN_POINT ( 'NONE',  ( -10.50000000000000355, 12.59158320108480922, -3.600000000000000533 ) ) ;
#112813 = FACE_OUTER_BOUND ( 'NONE', #113847, .T. ) ;
#112814 = CARTESIAN_POINT ( 'NONE',  ( 2.086296903703276140, -1.790263230197926436, -0.3570169370194844483 ) ) ;
#112815 = CARTESIAN_POINT ( 'NONE',  ( -2.948008335967658322, 5.526761261015804116, 1.199719254218462483 ) ) ;
#112816 = CARTESIAN_POINT ( 'NONE',  ( -6.586110727467836767, 6.776993156853382771, -0.3129968654442937814 ) ) ;
#112817 = CARTESIAN_POINT ( 'NONE',  ( 6.509000000000015440, 0.001920477310516938412, 2.100274754360692331 ) ) ;
#112818 = CARTESIAN_POINT ( 'NONE',  ( 8.866142388332804103, 12.43125098877526113, -1.199719254218446718 ) ) ;
#112819 = CARTESIAN_POINT ( 'NONE',  ( 0.7328819429333592872, 0.1407736501095498138, 1.921419779381093207 ) ) ;
#112820 = CARTESIAN_POINT ( 'NONE',  ( 3.924618397835403893, -1.320764108826902428, 1.450678906977073579 ) ) ;
#112821 = CARTESIAN_POINT ( 'NONE',  ( -8.365544474831901667, 9.718555627847388578, 1.199719254218462483 ) ) ;
#112822 = CARTESIAN_POINT ( 'NONE',  ( 6.661133543015731462, 6.665743976473484267, -0.7998128361456281477 ) ) ;
#112823 = CARTESIAN_POINT ( 'NONE',  ( 4.915667883426772633, -1.172277214026868464, -1.851500752446763709 ) ) ;
#112824 = CARTESIAN_POINT ( 'NONE',  ( 3.472859903394816872, 7.203420320602604399, -0.7998128361456291469 ) ) ;
#112825 = CARTESIAN_POINT ( 'NONE',  ( 3.871986384844767315, -2.040452582458017083, 0.3490408808229996662 ) ) ;
#112827 = CARTESIAN_POINT ( 'NONE',  ( 1.364683531249986537, 1.717708333674749399, -0.7879004041258239610 ) ) ;
#112826 = CARTESIAN_POINT ( 'NONE',  ( 4.028659262336944380, 3.858644544030801704, 2.500000000000000000 ) ) ;
#112828 = ORIENTED_EDGE ( 'NONE', *, *, #156704, .T. ) ;
#112829 = CARTESIAN_POINT ( 'NONE',  ( 4.483195000112350392, -2.298113444969139607, -0.05724751674645797012 ) ) ;
#112831 = VERTEX_POINT ( 'NONE', #56900 ) ;
#112830 = CARTESIAN_POINT ( 'NONE',  ( 8.595506201384020883, 9.130438111143927671, 0.7216878364870438212 ) ) ;
#112833 = CARTESIAN_POINT ( 'NONE',  ( 3.285556943750000514, -1.013541666188710888, 1.896917185911906500 ) ) ;
#112832 = CARTESIAN_POINT ( 'NONE',  ( 4.746763178560241769, 8.551991118380046331, 0.7216878364870328300 ) ) ;
#112834 = CARTESIAN_POINT ( 'NONE',  ( 6.620655732516651071, 7.053049904137934867, 2.524417197114035005 ) ) ;
#112835 = CARTESIAN_POINT ( 'NONE',  ( -8.086512275908061653, 8.398962174839683215, 0.000000000000000000 ) ) ;
#112836 = CARTESIAN_POINT ( 'NONE',  ( 3.328005318368632892, 1.894807597966931878, 0.4246257584521081485 ) ) ;
#112837 = ORIENTED_EDGE ( 'NONE', *, *, #74029, .T. ) ;
#112838 = CARTESIAN_POINT ( 'NONE',  ( -7.642790800258748294E-15, -9.595263517168229228, 9.591985693221618092 ) ) ;
#112839 = CARTESIAN_POINT ( 'NONE',  ( 4.816621285000030284, -0.6497861859515661198, -1.798733151862880186 ) ) ;
#112840 = DIRECTION ( 'NONE',  ( -0.000000000000000000, -0.000000000000000000, -1.000000000000000000 ) ) ;
#112841 = CARTESIAN_POINT ( 'NONE',  ( 5.631808906544129911, -1.097478420741523575, -1.330571920265137376 ) ) ;
#112842 = CARTESIAN_POINT ( 'NONE',  ( 4.522672878804367969, 0.3494810548456111499, 1.985869246038343583 ) ) ;
#112843 = CARTESIAN_POINT ( 'NONE',  ( 5.098365541279441082, -0.3395090112114571013, 2.273368781073564993 ) ) ;
#112844 = CARTESIAN_POINT ( 'NONE',  ( -1.115562610750309283E-14, 9.812500000000000000, 1.500000000000001554 ) ) ;
#112845 = CARTESIAN_POINT ( 'NONE',  ( 1.049787907720298286, -1.741764784136769162, -1.355102641770723704 ) ) ;
#112847 = CARTESIAN_POINT ( 'NONE',  ( -4.882344714696960075, 5.829061934302122161, 1.082531754730549078 ) ) ;
#112846 = CARTESIAN_POINT ( 'NONE',  ( -3.839356663422469840, 7.492693387012709927, -0.03537628172997089177 ) ) ;
#112848 = CARTESIAN_POINT ( 'NONE',  ( 5.782415762239879520, -1.726843194930051562, -0.3863986657466413899 ) ) ;
#112849 = CARTESIAN_POINT ( 'NONE',  ( 6.205703963786828758, 1.882472927010571118, 0.7231429968634556227 ) ) ;
#112850 = EDGE_CURVE ( 'NONE', #13808, #108528, #153333, .T. ) ;
#112852 = CARTESIAN_POINT ( 'NONE',  ( 2.554944377107245757, -1.995129818168206226, -1.128553997664314412 ) ) ;
#112851 = CARTESIAN_POINT ( 'NONE',  ( 5.734172623936983904, 5.654565914206774124, 0.7998128361456352531 ) ) ;
#112853 = CARTESIAN_POINT ( 'NONE',  ( 1.253398004092287854, 0.7024035357156286352, 1.592479786115083229 ) ) ;
#112854 = DIRECTION ( 'NONE',  ( 0.000000000000000000, 0.000000000000000000, 1.000000000000000000 ) ) ;
#112855 = CARTESIAN_POINT ( 'NONE',  ( 1.176590053548575598, -0.7728590343649595074, -1.552129106697144989 ) ) ;
#112856 = CARTESIAN_POINT ( 'NONE',  ( -1.360316468750032204, 0.6718750003414097893, -2.081668171172168513E-14 ) ) ;
#112857 = CARTESIAN_POINT ( 'NONE',  ( -9.495347311156809411, -6.857257212219918685, 3.422217897015904270E-15 ) ) ;
#112858 = CARTESIAN_POINT ( 'NONE',  ( 1.346384888165049754, -0.9767783691352300846, 1.939140577548441380 ) ) ;
#112859 = CARTESIAN_POINT ( 'NONE',  ( 1.938685741270998797, -1.555697844595272716, 1.282991390469834458 ) ) ;
#112860 = CARTESIAN_POINT ( 'NONE',  ( 4.031250000000002665, -0.7852924748301974844, -1.895863743163994863 ) ) ;
#112861 = CARTESIAN_POINT ( 'NONE',  ( 0.7499999999999902300, 1.014583334016154526, 1.299038105676657340 ) ) ;
#112862 = CARTESIAN_POINT ( 'NONE',  ( 6.674445239480702341, -1.183187502913226608, 1.521125075997560527 ) ) ;
#112863 = CARTESIAN_POINT ( 'NONE',  ( -1.364683531250000748, 12.85937500034139980, 0.000000000000000000 ) ) ;
#112864 = CARTESIAN_POINT ( 'NONE',  ( 3.762163318865581640, 0.7457541186767223662, -2.092641825391368560 ) ) ;
#112865 = ORIENTED_EDGE ( 'NONE', *, *, #143867, .F. ) ;
#112866 = CARTESIAN_POINT ( 'NONE',  ( 4.495112795250098436, 8.049017979306480441, 2.444655174081866278 ) ) ;
#112867 = CARTESIAN_POINT ( 'NONE',  ( 1.499999999999987121, -0.7458333333333122539, 0.8660254037844524744 ) ) ;
#112868 = CARTESIAN_POINT ( 'NONE',  ( 7.377608144130607393, 11.75895993479440982, -0.7998128361456291469 ) ) ;
#112869 = CARTESIAN_POINT ( 'NONE',  ( 7.987161891782087686, 8.490979426600148372, -0.7216878364870317197 ) ) ;
#112870 =( LENGTH_UNIT ( ) NAMED_UNIT ( * ) SI_UNIT ( .MILLI., .METRE. ) );
#112871 = CARTESIAN_POINT ( 'NONE',  ( 5.161534370633450663, 0.8641669074914829496, 1.510678848428636201 ) ) ;
#112872 = CARTESIAN_POINT ( 'NONE',  ( 3.437899435096212208, 1.242623406730450686, 1.518177208742684803 ) ) ;
#112874 = CARTESIAN_POINT ( 'NONE',  ( -6.399085315970137522, 9.449054721065074602, -1.082531754730538864 ) ) ;
#112873 = CARTESIAN_POINT ( 'NONE',  ( 2.672928840188529609, 6.270167413528593414, 0.000000000000000000 ) ) ;
#112875 = CARTESIAN_POINT ( 'NONE',  ( -1.449478204280063576, 4.332514689554293419, 0.3909668688984575535 ) ) ;
#112876 = CARTESIAN_POINT ( 'NONE',  ( 4.358826825731692445, -1.680320932299755210, 1.515136896344573270 ) ) ;
#112877 = AXIS2_PLACEMENT_3D ( 'NONE', #207136, #89147, #138964 ) ;
#112878 = CARTESIAN_POINT ( 'NONE',  ( 1.891156856157749866, 0.2001100897341882012, 2.052929594394680812 ) ) ;
#112879 = CARTESIAN_POINT ( 'NONE',  ( -7.867809214632013770, 8.073532260025807261, 1.040834085586084257E-14 ) ) ;
#112880 = EDGE_CURVE ( 'NONE', #142386, #204338, #128616, .T. ) ;
#112881 = AXIS2_PLACEMENT_3D ( 'NONE', #210810, #62435, #46210 ) ;
#112882 = CARTESIAN_POINT ( 'NONE',  ( 2.255063695347800934, -1.748954272965432155, 1.435335380440343256 ) ) ;
#112883 = VERTEX_POINT ( 'NONE', #187953 ) ;
#112884 = CARTESIAN_POINT ( 'NONE',  ( -1.500000000000013101, 1.410416667349486008, -0.8660254037844313801 ) ) ;
#112885 = CARTESIAN_POINT ( 'NONE',  ( 3.391731324245280010, -0.7611128710301139355, 1.708892184765831157 ) ) ;
#112886 = CARTESIAN_POINT ( 'NONE',  ( 2.004178618920505972, -1.681731546479984463, 0.4224366712483189623 ) ) ;
#112887 = CARTESIAN_POINT ( 'NONE',  ( 6.356982542327763497, 0.3766756592470664744, -2.158781491689326426 ) ) ;
#112888 = CARTESIAN_POINT ( 'NONE',  ( 0.2709337360254741034, -1.439471777561899035, 1.672717458380864608 ) ) ;
#112889 = CARTESIAN_POINT ( 'NONE',  ( 3.872077330825273389, 1.198917189070296541, 1.798566189592496034 ) ) ;
#112890 = CARTESIAN_POINT ( 'NONE',  ( 4.646391893561965247, -1.558859349912258718, 1.157878524630775230 ) ) ;
#112891 = CARTESIAN_POINT ( 'NONE',  ( -3.809477975315625375, 4.507107728365378208, 1.082531754730558626 ) ) ;
#112893 = ORIENTED_EDGE ( 'NONE', *, *, #206691, .T. ) ;
#112892 = CARTESIAN_POINT ( 'NONE',  ( 6.468025801952650866, 0.9617254617904011926, 1.604207369834034669 ) ) ;
#112894 = CARTESIAN_POINT ( 'NONE',  ( 4.911299649074239326, 6.652374229206746037, 1.248453844233877286 ) ) ;
#112895 = DIRECTION ( 'NONE',  ( -0.6507913734559643837, -0.7592566023653002372, 0.000000000000000000 ) ) ;
#112896 = CARTESIAN_POINT ( 'NONE',  ( 3.119784744920330422, 6.653849612466795627, 0.7216878364870257245 ) ) ;
#112897 = DIRECTION ( 'NONE',  ( -0.000000000000000000, -1.000000000000000000, -0.000000000000000000 ) ) ;
#112898 = CARTESIAN_POINT ( 'NONE',  ( 5.485000066852382616, -2.016597020608828839, 0.002808655738886777897 ) ) ;
#112899 = CARTESIAN_POINT ( 'NONE',  ( -10.15522075183580419, 11.80651128435196462, 1.199719254218462483 ) ) ;
#112900 = CARTESIAN_POINT ( 'NONE',  ( 7.313733799568044702, 10.62010763521636214, 1.199719254218460707 ) ) ;
#112901 = CARTESIAN_POINT ( 'NONE',  ( 2.670845766169899438, -0.4339950243563576726, -0.1191324417346315279 ) ) ;
#112903 = CARTESIAN_POINT ( 'NONE',  ( -4.163660309340779797, 7.871692890607882021, 0.005041904348490143691 ) ) ;
#112902 = CARTESIAN_POINT ( 'NONE',  ( 3.527797039230845311, -1.088449851438414218, -1.465592618984489670 ) ) ;
#112904 = CARTESIAN_POINT ( 'NONE',  ( 11.89829993707161471, 9.770807717488739996, -1.561606677374349772 ) ) ;
#112905 = VERTEX_POINT ( 'NONE', #171712 ) ;
#112906 = CARTESIAN_POINT ( 'NONE',  ( -5.763624699140894592, 5.896852701852039580, -0.7216878364870338292 ) ) ;
#112907 = DIRECTION ( 'NONE',  ( -5.551115123125764829E-17, 0.000000000000000000, 1.000000000000000000 ) ) ;
#112908 = CARTESIAN_POINT ( 'NONE',  ( -7.374745490829552885, 10.69128794168811680, -1.199719254218446718 ) ) ;
#112909 = CARTESIAN_POINT ( 'NONE',  ( 6.340491327343366734, 1.161156619345372842, -1.652315300818160582 ) ) ;
#112910 = CARTESIAN_POINT ( 'NONE',  ( 0.8562900302464396818, 0.8558255631127342777, -1.940287777186230578 ) ) ;
#112911 = ORIENTED_EDGE ( 'NONE', *, *, #151435, .T. ) ;
#112912 = CARTESIAN_POINT ( 'NONE',  ( -4.990283058281743678, 7.979691447040783814, -1.199719254218453823 ) ) ;
#112913 = CARTESIAN_POINT ( 'NONE',  ( 2.324856365976185391, -1.699136111967664453, -0.7594513203179918959 ) ) ;
#112914 = CARTESIAN_POINT ( 'NONE',  ( 3.517450787741589036, 6.191110788085444128, -1.199719254218446718 ) ) ;
#112915 = CARTESIAN_POINT ( 'NONE',  ( 6.297740734744428970, -0.6968897171561654336, 1.939616516419547132 ) ) ;
#112916 = CARTESIAN_POINT ( 'NONE',  ( 6.328750030911493241, 0.7691242348151774433, -1.864167186630163009 ) ) ;
#112917 = ORIENTED_EDGE ( 'NONE', *, *, #170713, .F. ) ;
#112918 = CARTESIAN_POINT ( 'NONE',  ( -6.078132937628113908, 5.985576603521232109, 1.040834085586084257E-14 ) ) ;
#112919 = CARTESIAN_POINT ( 'NONE',  ( 0.08888683327021307257, 6.492044364012829583, -3.106763327641859362 ) ) ;
#112920 = FACE_OUTER_BOUND ( 'NONE', #75406, .T. ) ;
#112922 = CARTESIAN_POINT ( 'NONE',  ( -5.461413243215608837, 6.444398994036877326, -1.303746704243381238 ) ) ;
#112921 = CARTESIAN_POINT ( 'NONE',  ( -5.143339171537843590, 7.093924681584509173, 1.599625672291263179 ) ) ;
#112923 = CARTESIAN_POINT ( 'NONE',  ( 6.430738266435902517, 6.882057634903050669, 0.7203813067775278745 ) ) ;
#112924 = CARTESIAN_POINT ( 'NONE',  ( 6.046249930811113060, 1.863882344683247094, -0.7690052245405626374 ) ) ;
#112925 = CARTESIAN_POINT ( 'NONE',  ( 4.242028835625204053, 0.4931972713904734795, 1.773778790588397491 ) ) ;
#112926 = CARTESIAN_POINT ( 'NONE',  ( -0.02299388927992032997, 5.724334336916190757, -2.505015335112478425 ) ) ;
#112927 = CARTESIAN_POINT ( 'NONE',  ( 3.493080449939501619, -0.4495562565045966852, -2.263328358674908003 ) ) ;
#112928 = CARTESIAN_POINT ( 'NONE',  ( 4.694866332082116678, 8.699370830729650450, 0.7998128361456341429 ) ) ;
#112929 = CARTESIAN_POINT ( 'NONE',  ( 6.257120919624137301, -1.850417449585840313, -1.117149918570578437 ) ) ;
#112930 = CARTESIAN_POINT ( 'NONE',  ( 6.608709811657416999, 9.797579649320619311, -1.199719254218440723 ) ) ;
#112931 = CARTESIAN_POINT ( 'NONE',  ( 0.8373251867893832801, 0.7858318893144546902, -1.776134337346139125 ) ) ;
#112932 = CARTESIAN_POINT ( 'NONE',  ( -5.108724954250998707, 4.854600622914589714, -0.7998128361456221525 ) ) ;
#112933 = ORIENTED_EDGE ( 'NONE', *, *, #61052, .T. ) ;
#112934 = CIRCLE ( 'NONE', #178566, 0.8300000000000008482 ) ;
#112935 = CARTESIAN_POINT ( 'NONE',  ( 4.763194794223141848, -2.297684049645591919, -0.06285783202429616467 ) ) ;
#112936 = DIRECTION ( 'NONE',  ( -1.000000000000000000, 2.090028284309406390E-15, 0.000000000000000000 ) ) ;
#112937 = CARTESIAN_POINT ( 'NONE',  ( -5.327428015527048366, 5.180030537728460338, -0.7998128361456362523 ) ) ;
#112938 = CARTESIAN_POINT ( 'NONE',  ( 4.856247981345184428, 0.7163626499266174674, 1.728251504774950709 ) ) ;
#112941 = CARTESIAN_POINT ( 'NONE',  ( -5.798046968499580345, 6.793418213784815585, 1.199719254218452935 ) ) ;
#112940 = CARTESIAN_POINT ( 'NONE',  ( 1.499999999999989120, 0.5562500006828161592, 0.000000000000000000 ) ) ;
#112939 = CARTESIAN_POINT ( 'NONE',  ( 0.7383556378116812313, 1.137082172773289379, -1.537495029474859276 ) ) ;
#112942 = CARTESIAN_POINT ( 'NONE',  ( 2.614145488985010424, -2.182733025630137824, 0.3247920039054427721 ) ) ;
#112943 = CARTESIAN_POINT ( 'NONE',  ( 6.883263157960335832, 7.629137130509051623, 2.446189081643288521 ) ) ;
#112944 = CARTESIAN_POINT ( 'NONE',  ( 4.701980345841006326, 4.380065246436280368, 0.7998128361456341429 ) ) ;
#112945 = CARTESIAN_POINT ( 'NONE',  ( 7.322812364712459221, 7.715904978352238430, 0.000000000000000000 ) ) ;
#112946 = CARTESIAN_POINT ( 'NONE',  ( -3.541704441667874903, 5.155074486744371853, -1.599625672291256295 ) ) ;
#112947 = PRESENTATION_LAYER_ASSIGNMENT (  '', '', ( #50555 ) ) ;
#112948 = CARTESIAN_POINT ( 'NONE',  ( -6.739811759324831897, 7.996106819701333634, -1.082531754730549967 ) ) ;
#112949 = CARTESIAN_POINT ( 'NONE',  ( 1.721884408201577399, -1.091793429770457458, -1.641225607529321229 ) ) ;
#112950 = CARTESIAN_POINT ( 'NONE',  ( 1.237850453945861906, -2.084960033126967982, 0.9891342380793988198 ) ) ;
#112951 = CARTESIAN_POINT ( 'NONE',  ( 2.084357000244409175, 1.132115006494602394, -1.602057852124554316 ) ) ;
#112952 = CARTESIAN_POINT ( 'NONE',  ( 5.348506707712929575, -2.046340616697607473, -0.2579891923277094490 ) ) ;
#112953 = CARTESIAN_POINT ( 'NONE',  ( 4.744990575102895569, 5.598539094783909320, -1.082531754730548412 ) ) ;
#112954 = CARTESIAN_POINT ( 'NONE',  ( 4.044074958626150185, 7.940114228364351767, 0.7998128361456271485 ) ) ;
#112955 = ORIENTED_EDGE ( 'NONE', *, *, #177202, .F. ) ;
#112956 = CARTESIAN_POINT ( 'NONE',  ( -1.364683531249997417, 5.821875000341418804, 1.214306433183764966E-14 ) ) ;
#112957 = DIRECTION ( 'NONE',  ( 1.000000000000000000, 3.451266460341926649E-31, 8.638326563840809144E-31 ) ) ;
#112958 = CARTESIAN_POINT ( 'NONE',  ( 3.267151830768944443, 4.834763107362302748, -1.443375672974058777 ) ) ;
#112959 = CARTESIAN_POINT ( 'NONE',  ( 0.9366657375849207767, -1.207674400081097721, 1.803990093267322736 ) ) ;
#112961 = CARTESIAN_POINT ( 'NONE',  ( -2.788906526875773208E-15, 12.18750000000000178, -1.499999999999998446 ) ) ;
#112960 = CARTESIAN_POINT ( 'NONE',  ( 2.869309894402357841, 6.436557513332352265, -0.3339617207483085992 ) ) ;
#112962 = CARTESIAN_POINT ( 'NONE',  ( 11.52483635780546933, 11.37999991357535023, -3.345866325258015639 ) ) ;
#112963 = CARTESIAN_POINT ( 'NONE',  ( -1.737499999999997824, -1.691666666666667762, 3.009438278150925683 ) ) ;
#112964 = CARTESIAN_POINT ( 'NONE',  ( 2.723731132150861711, -1.073666234122659713, -1.531540996774889640 ) ) ;
#112965 = CARTESIAN_POINT ( 'NONE',  ( 6.397764797294555272, -0.7349420381566433846, 2.032942830986879557 ) ) ;
#112967 = CARTESIAN_POINT ( 'NONE',  ( 6.827182134110201694, 1.288579688585177685, 1.926502426867699569 ) ) ;
#112966 = CARTESIAN_POINT ( 'NONE',  ( 0.07735805125220260314, 1.351236195817316466, -2.344668200922094492 ) ) ;
#112968 = CARTESIAN_POINT ( 'NONE',  ( 0.6823417656249882723, -0.9072916663252494907, 1.181850606188755259 ) ) ;
#112969 = CARTESIAN_POINT ( 'NONE',  ( 2.438023429326571456, -1.102505324871098757, -1.562262158393577405 ) ) ;
#112970 = CARTESIAN_POINT ( 'NONE',  ( 4.205725695155067889, -1.765064932122958785, 0.1306522685067777467 ) ) ;
#112971 = CARTESIAN_POINT ( 'NONE',  ( 1.541514448083292965, -1.800223203088219481, 0.6453159242577054533 ) ) ;
#112972 = CARTESIAN_POINT ( 'NONE',  ( -4.218558352146454915, 8.073401844146177453, 1.040834085586084257E-14 ) ) ;
#112974 = CARTESIAN_POINT ( 'NONE',  ( 5.273012193977356432, 1.687281682853270848, -0.9070163062135666587 ) ) ;
#112973 = CARTESIAN_POINT ( 'NONE',  ( -10.98194350564911659, -7.666862915010147717, 0.6300133639306291222 ) ) ;
#112975 = CARTESIAN_POINT ( 'NONE',  ( 0.2739938332866619364, -2.030697503880642518, 0.4024348779970430834 ) ) ;
#112976 = CARTESIAN_POINT ( 'NONE',  ( -1.500000000000011324, 4.920833333333354709, 0.8660254037844403729 ) ) ;
#112977 = CARTESIAN_POINT ( 'NONE',  ( 1.969135536805465492, -1.636093909763213228, 1.349083368969570262 ) ) ;
#112978 =( NAMED_UNIT ( * ) SI_UNIT ( $, .STERADIAN. ) SOLID_ANGLE_UNIT ( ) );
#112979 = CARTESIAN_POINT ( 'NONE',  ( 4.645289301550183936, -1.446173438076237217, -1.186536486241091204 ) ) ;
#112981 = VERTEX_POINT ( 'NONE', #39581 ) ;
#112980 = CARTESIAN_POINT ( 'NONE',  ( 1.400715809426569702, 1.493624456287694358, -1.049586478250638999 ) ) ;
#112983 = CARTESIAN_POINT ( 'NONE',  ( -1.965118028437710995, -0.3835514080770054401, 0.6713998180129590043 ) ) ;
#112982 = CARTESIAN_POINT ( 'NONE',  ( 4.758537496233657293, 0.8426522330295079799, 2.039869969286691731 ) ) ;
#112984 = EDGE_CURVE ( 'NONE', #91093, #37173, #45672, .T. ) ;
#112985 = CARTESIAN_POINT ( 'NONE',  ( 0.6823417656249882723, -1.157291666325249713, 1.181850606188755259 ) ) ;
#112986 = CARTESIAN_POINT ( 'NONE',  ( 2.418490130824833440, 0.8798743164511336756, 1.865715637115851866 ) ) ;
#112987 = CARTESIAN_POINT ( 'NONE',  ( 6.368579470117202490, 8.453095353268645695, 1.599625672291281386 ) ) ;
#112988 = CARTESIAN_POINT ( 'NONE',  ( -6.516665389662827934, 10.75452672124865217, 0.000000000000000000 ) ) ;
#112989 = CARTESIAN_POINT ( 'NONE',  ( 0.000000000000000000, 8.600000000000017408, 0.4000000000000045186 ) ) ;
#112990 = CARTESIAN_POINT ( 'NONE',  ( 7.075376061485196821, 9.347967719856493218, 1.599625672291268286 ) ) ;
#112991 = ORIENTED_EDGE ( 'NONE', *, *, #131672, .T. ) ;
#112992 = CARTESIAN_POINT ( 'NONE',  ( 4.018080225218490398, 2.055083638104511223, -0.2504045000601487492 ) ) ;
#112993 = CARTESIAN_POINT ( 'NONE',  ( 1.364683531249984538, -1.032291666325247714, -0.7879004041258309554 ) ) ;
#112994 = CARTESIAN_POINT ( 'NONE',  ( 2.653791512158054200, 0.5793167894731532375, -2.082426382048585101 ) ) ;
#112995 = CARTESIAN_POINT ( 'NONE',  ( -6.259328228163411723, 6.916251825828671151, -0.7980491773402348388 ) ) ;
#112996 = CARTESIAN_POINT ( 'NONE',  ( 2.578776193315842846, -1.391201028639722281, 1.464365899026105700 ) ) ;
#112997 = CARTESIAN_POINT ( 'NONE',  ( 5.299301323368958094, 6.361497809228795930, -1.122821758042211959 ) ) ;
#112998 = PRODUCT_DEFINITION_SHAPE ( 'NONE', 'NONE',  #214421 ) ;
#112999 = ORIENTED_EDGE ( 'NONE', *, *, #178570, .T. ) ;
#113000 = ADVANCED_FACE ( 'NONE', ( #155468 ), #202040, .F. ) ;
#113002 = CARTESIAN_POINT ( 'NONE',  ( 8.446366511633696561, 8.956441806435218922, 1.040834085586084257E-14 ) ) ;
#113001 = CARTESIAN_POINT ( 'NONE',  ( -1.737499999999997824, -2.741666666666666696, 3.009438278150925683 ) ) ;
#113003 = CARTESIAN_POINT ( 'NONE',  ( -3.919715807682309094, 6.626733304721049933, 1.082531754730549967 ) ) ;
#113004 = CARTESIAN_POINT ( 'NONE',  ( 0.6203277878081385754, 1.987498645412737908, 0.3399528957561820386 ) ) ;
#113005 = B_SPLINE_CURVE_WITH_KNOTS ( 'NONE', 3,
 ( #41271, #206935, #9802, #75877, #190678, #141984, #42337, #176584, #8740, #107379 ),
 .UNSPECIFIED., .F., .F.,
 ( 4, 1, 1, 1, 1, 1, 1, 4 ),
 ( 0.000000000000000000, 0.09090790722575105287, 0.1825853934691276381, 0.2551728700554835028, 0.3603391217242263855, 0.5205903519787860034, 0.7335386666926504429, 0.9999999999999998890 ),
 .UNSPECIFIED. ) ;
#113006 = CARTESIAN_POINT ( 'NONE',  ( 4.880524338131243312, -0.2681524694418159216, -2.175044001020635331 ) ) ;
#113008 = VECTOR ( 'NONE', #49278, 1000.000000000000000 ) ;
#113007 = CARTESIAN_POINT ( 'NONE',  ( -1.201851678989727383E-14, 4.868750000682822154, -1.732050807568863648 ) ) ;
#113009 = CARTESIAN_POINT ( 'NONE',  ( 4.869353489999923568, -1.618680692612521455, -1.018082601613921723 ) ) ;
#113010 = CARTESIAN_POINT ( 'NONE',  ( -3.469997250093771246, 6.135748327496311383, -1.199719254218452935 ) ) ;
#113011 = CARTESIAN_POINT ( 'NONE',  ( 5.300874872818821082, 9.128178418356554857, 0.7216878364870438212 ) ) ;
#113013 = CARTESIAN_POINT ( 'NONE',  ( 2.267204043252795120, 1.842440753109304330, -0.8197907266209791821 ) ) ;
#113012 = CARTESIAN_POINT ( 'NONE',  ( -7.985389288324692636, 11.29974268881207067, -1.082531754730543083 ) ) ;
#113014 = CARTESIAN_POINT ( 'NONE',  ( -0.6823417656250003738, 11.71354166700806765, 1.181850606188754593 ) ) ;
#113015 = CARTESIAN_POINT ( 'NONE',  ( -6.563028877466991595, 9.814561569423593923, 1.199719254218452935 ) ) ;
#113016 = CARTESIAN_POINT ( 'NONE',  ( 5.491107761985050573, 1.519353413045966494, -0.8162815091526542943 ) ) ;
#113017 = CARTESIAN_POINT ( 'NONE',  ( 0.1405533004714097089, -0.003749010675423158478, -2.279853246149381452 ) ) ;
#113018 = CARTESIAN_POINT ( 'NONE',  ( 8.866669273657322492, 12.32790267170016207, -1.082531754730543083 ) ) ;
#113019 = DIRECTION ( 'NONE',  ( -0.000000000000000000, -1.000000000000000000, -0.000000000000000000 ) ) ;
#113020 = CARTESIAN_POINT ( 'NONE',  ( 3.167801447087334576, 6.847518788243868393, -0.7998128361456291469 ) ) ;
#113021 = FACE_OUTER_BOUND ( 'NONE', #86763, .T. ) ;
#113022 = ORIENTED_EDGE ( 'NONE', *, *, #188735, .T. ) ;
#113023 = CARTESIAN_POINT ( 'NONE',  ( 1.024380955673375393, 1.017105081308821379, 1.803069775380027995 ) ) ;
#113024 = B_SPLINE_CURVE_WITH_KNOTS ( 'NONE', 3,
 ( #181999, #213427, #49888, #50955, #149522, #65050, #17358, #163653 ),
 .UNSPECIFIED., .F., .F.,
 ( 4, 2, 2, 4 ),
 ( 0.000000000000000000, 0.003005455498261387637, 0.004508183247392082323, 0.006010910996522775274 ),
 .UNSPECIFIED. ) ;
#113025 = VERTEX_POINT ( 'NONE', #4907 ) ;
#113026 = CARTESIAN_POINT ( 'NONE',  ( 5.109926359719781708, -0.6467658019376655298, 1.692270648455761917 ) ) ;
#113027 = CARTESIAN_POINT ( 'NONE',  ( 3.867818961648523235, 7.734482231890414283, 1.040834085586084257E-14 ) ) ;
#113029 = ADVANCED_FACE ( 'NONE', ( #87267 ), #189030, .F. ) ;
#113028 = DIRECTION ( 'NONE',  ( 0.000000000000000000, -1.000000000000000000, -1.804652791718263484E-16 ) ) ;
#113030 = CARTESIAN_POINT ( 'NONE',  ( 5.760388245948376174, 1.809740711040405348, 0.08207984589548086851 ) ) ;
#113031 = CARTESIAN_POINT ( 'NONE',  ( 4.977251789548238214, 7.860525283564661514, -1.082531754730548412 ) ) ;
#113032 = CARTESIAN_POINT ( 'NONE',  ( -1.420000000000021911, 6.200000000000045475, 2.580000000000011173 ) ) ;
#113033 = CARTESIAN_POINT ( 'NONE',  ( 3.170069416559752273, -1.305109287949431929, 1.760291797049506446 ) ) ;
#113034 = EDGE_LOOP ( 'NONE', ( #187493, #134450, #90138, #62349 ) ) ;
#113035 = CIRCLE ( 'NONE', #19551, 10.75000000000000000 ) ;
#113037 = CARTESIAN_POINT ( 'NONE',  ( 8.320953590485093088, 10.73086516036454618, 1.599625672291281386 ) ) ;
#113036 = CARTESIAN_POINT ( 'NONE',  ( 0.9593383959572501229, 1.601786533887459507, 1.132500672181527168 ) ) ;
#113038 = CARTESIAN_POINT ( 'NONE',  ( 5.396063265741290138, -0.8654563178034151427, -1.709049623916969018 ) ) ;
#113039 = CARTESIAN_POINT ( 'NONE',  ( 7.065207446497155708, 9.336104335703744539, 0.000000000000000000 ) ) ;
#113040 = ADVANCED_FACE ( 'NONE', ( #5984 ), #90952, .T. ) ;
#113041 = CARTESIAN_POINT ( 'NONE',  ( -1.364683531250014514, -0.2197916663252438285, 0.7879004041258379498 ) ) ;
#113042 = CARTESIAN_POINT ( 'NONE',  ( 6.344852701515477200, 6.504675694630598137, -0.7216878364870257245 ) ) ;
#113043 = CARTESIAN_POINT ( 'NONE',  ( -7.348156068926747331, 11.51667314714914347, 0.7216878364870458196 ) ) ;
#113044 = CARTESIAN_POINT ( 'NONE',  ( 2.184651956524386041, -2.119909832212972578, -0.4221607449544013679 ) ) ;
#113045 = CARTESIAN_POINT ( 'NONE',  ( -5.144392941742557568, 4.966489618313220333, -0.7998128361456362523 ) ) ;
#113046 = CARTESIAN_POINT ( 'NONE',  ( 4.203910148689107729, 7.062256385849379647, -1.199719254218448494 ) ) ;
#113047 = CARTESIAN_POINT ( 'NONE',  ( 2.098414945899258033, -0.4839449910110822373, -1.760204267430766301 ) ) ;
#113048 = CARTESIAN_POINT ( 'NONE',  ( -4.874319919312905647, 5.645460313075203018, -1.199719254218446718 ) ) ;
#113049 = CARTESIAN_POINT ( 'NONE',  ( 4.928627555176230857, 1.747287423663802075, 0.5288322122747670662 ) ) ;
#113050 = CARTESIAN_POINT ( 'NONE',  ( 11.39652004212136838, 9.097555222845741696, 6.605822843452838100 ) ) ;
#113051 = CARTESIAN_POINT ( 'NONE',  ( 2.672007700615218528, 1.902801012812182169, -0.1915479950082218386 ) ) ;
#113052 = ORIENTED_EDGE ( 'NONE', *, *, #202198, .F. ) ;
#113053 = CARTESIAN_POINT ( 'NONE',  ( 3.947672784279113500, 1.424866277981166052, 1.359976495918001627 ) ) ;
#113054 = EDGE_LOOP ( 'NONE', ( #101128, #145510 ) ) ;
#113055 = CARTESIAN_POINT ( 'NONE',  ( 4.827648274430585751, 0.9952931021880854212, -1.667489682845281207 ) ) ;
#113056 = VERTEX_POINT ( 'NONE', #208367 ) ;
#113057 = CARTESIAN_POINT ( 'NONE',  ( -6.587282531393266360, 8.778525268082516320, 1.599625672291269396 ) ) ;
#113059 = CARTESIAN_POINT ( 'NONE',  ( 4.851869265964163347, -1.501451181749386743, -1.497782127133556518 ) ) ;
#113058 = CARTESIAN_POINT ( 'NONE',  ( 6.530187263637528439, 7.647581891445782709, -1.199719254218452047 ) ) ;
#113060 = DIRECTION ( 'NONE',  ( -3.330669073875481947E-16, 4.742150360713068815E-16, 1.000000000000000000 ) ) ;
#113062 = ORIENTED_EDGE ( 'NONE', *, *, #102667, .F. ) ;
#113061 = CARTESIAN_POINT ( 'NONE',  ( 2.666550042863625958, 0.6461651886627232111, 1.799920402468312197 ) ) ;
#113063 = CARTESIAN_POINT ( 'NONE',  ( 4.435735274902380176, 7.313263296268260660, -1.222879399185505367 ) ) ;
#113064 = DIRECTION ( 'NONE',  ( -0.000000000000000000, -1.000000000000000000, -0.000000000000000000 ) ) ;
#113065 = CARTESIAN_POINT ( 'NONE',  ( 4.415115299905642665, 5.179997933758551554, -1.199719254218450271 ) ) ;
#113066 = CARTESIAN_POINT ( 'NONE',  ( 5.443998933236983362, -1.278728028966215957, -1.554778559382914871 ) ) ;
#113067 = CARTESIAN_POINT ( 'NONE',  ( 11.06298660227979802, 12.34319600374733383, -0.9087478855431304625 ) ) ;
#113068 = CARTESIAN_POINT ( 'NONE',  ( 5.092344371507952161, -1.812320225013038133, -0.2200062734805732223 ) ) ;
#113069 = CARTESIAN_POINT ( 'NONE',  ( 1.047426762419433777, 1.826728496382063582, -0.9743617655595809834 ) ) ;
#113070 = CARTESIAN_POINT ( 'NONE',  ( -7.049876689426097798, 11.16868053773170821, -0.7216878364870267237 ) ) ;
#113071 = AXIS2_PLACEMENT_3D ( 'NONE', #193663, #108232, #174257 ) ;
#113072 = CARTESIAN_POINT ( 'NONE',  ( -6.419454189569741231, 6.887487763818779918, 0.7628848663763813098 ) ) ;
#113073 = CARTESIAN_POINT ( 'NONE',  ( 6.174654088403855212, -1.776896415251895789, -0.5849557326117056366 ) ) ;
#113074 = CARTESIAN_POINT ( 'NONE',  ( 6.531277313481192337, 8.642909503859968368, 1.599625672291281386 ) ) ;
#113075 = DIRECTION ( 'NONE',  ( 0.000000000000000000, 1.000000000000000000, 0.000000000000000000 ) ) ;
#113076 = CIRCLE ( 'NONE', #144139, 0.04999999999999989869 ) ;
#113077 = CARTESIAN_POINT ( 'NONE',  ( 4.539282502477016479, 4.190251095844947926, 0.7998128361456341429 ) ) ;
#113078 = CARTESIAN_POINT ( 'NONE',  ( -1.402160292154681736E-14, 9.734375000341399797, 1.575800808251682339 ) ) ;
#113079 = CARTESIAN_POINT ( 'NONE',  ( -5.412729640353771465, 7.337937218544611895, 1.599625672291269396 ) ) ;
#113080 = CARTESIAN_POINT ( 'NONE',  ( -5.139949632912262700, 5.169231791251960750, 0.7216878364870257245 ) ) ;
#113081 = CARTESIAN_POINT ( 'NONE',  ( -5.904739593951539689, 6.847616600153594746, 1.199719254218450271 ) ) ;
#113082 = CARTESIAN_POINT ( 'NONE',  ( 1.235311698660218838, -0.04697018572753957483, -2.069874154031334790 ) ) ;
#113083 = CARTESIAN_POINT ( 'NONE',  ( 2.425544100157220662, -1.571072031863307572, -1.419494070558358967 ) ) ;
#113084 = CARTESIAN_POINT ( 'NONE',  ( 7.214910300766615769, 11.56914578420308715, -0.7998128361456291469 ) ) ;
#113085 = CARTESIAN_POINT ( 'NONE',  ( 7.687279255399376694E-16, -0.02379966007286238305, 6.277139874739035896 ) ) ;
#113086 = CARTESIAN_POINT ( 'NONE',  ( 0.4089589639980686919, -1.585120765669449261, 1.168626392425928584 ) ) ;
#113087 = CARTESIAN_POINT ( 'NONE',  ( 4.035592002476674267, 7.779268892024251869, 0.4218195438757850191 ) ) ;
#113088 = CARTESIAN_POINT ( 'NONE',  ( 5.368665641331531013, 5.365790791082654998, -0.7216878364870207285 ) ) ;
#113090 = DIRECTION ( 'NONE',  ( -1.000000000000000000, -3.451266460341926649E-31, 0.000000000000000000 ) ) ;
#113089 = CARTESIAN_POINT ( 'NONE',  ( 3.475000000000000533, -3.645833333333333037, -2.006292185433951047 ) ) ;
#113091 = CARTESIAN_POINT ( 'NONE',  ( 2.660454013544113927, -1.579728858233371946, 1.661220326946882375 ) ) ;
#113092 = CARTESIAN_POINT ( 'NONE',  ( 0.8205984872286451459, 1.685833220154912881, 0.7012733028506010768 ) ) ;
#113093 = CARTESIAN_POINT ( 'NONE',  ( 1.898553772666348394, -1.876154101037771582, -0.3696338911259658411 ) ) ;
#113094 = AXIS2_PLACEMENT_3D ( 'NONE', #128344, #209468, #211607 ) ;
#113095 = CARTESIAN_POINT ( 'NONE',  ( 5.830888582329017744, 8.960397891762626799, -1.199719254218452047 ) ) ;
#113096 = CARTESIAN_POINT ( 'NONE',  ( 7.754900676892376055, 8.149731665903665601, 1.040834085586084257E-14 ) ) ;
#113097 = CARTESIAN_POINT ( 'NONE',  ( 1.476815932985692026, -1.420704281710112316, 1.426639689446000281 ) ) ;
#113098 = CARTESIAN_POINT ( 'NONE',  ( 2.360140415366944744, -1.961439503465340239, 0.04308618615556784187 ) ) ;
#113099 = CARTESIAN_POINT ( 'NONE',  ( -8.676328237741483207, 12.20980114641871062, -1.199719254218446718 ) ) ;
#113100 = CARTESIAN_POINT ( 'NONE',  ( -6.028571859570855729, 10.18508426947466816, 0.000000000000000000 ) ) ;
#113101 = DIRECTION ( 'NONE',  ( -1.000000000000000000, 0.000000000000000000, 0.000000000000000000 ) ) ;
#113103 = CARTESIAN_POINT ( 'NONE',  ( 3.994789325776046507, 1.495029845459275863, -0.9468837749658890468 ) ) ;
#113102 = CARTESIAN_POINT ( 'NONE',  ( 4.576172254314175625, -2.027756842407653082, -0.5083681234262329429 ) ) ;
#113104 = CARTESIAN_POINT ( 'NONE',  ( -11.35605497252127449, 13.61418145951644121, 3.553547709190206128 ) ) ;
#113105 = EDGE_CURVE ( 'NONE', #182472, #108640, #66332, .T. ) ;
#113107 = CARTESIAN_POINT ( 'NONE',  ( 6.597627758599571735, -2.291905675289906519, 0.04924309260747637695 ) ) ;
#113106 = FACE_OUTER_BOUND ( 'NONE', #127046, .T. ) ;
#113108 = CARTESIAN_POINT ( 'NONE',  ( 4.347407756490777153, 1.739891706657967552, -0.04609750694275702165 ) ) ;
#113109 = CARTESIAN_POINT ( 'NONE',  ( 8.565000355531088516, 11.01558638625153286, -1.599625672291257406 ) ) ;
#113110 = CARTESIAN_POINT ( 'NONE',  ( -1.249999999999964695, 8.500000000000000000, 11.02939254900287303 ) ) ;
#113111 = CARTESIAN_POINT ( 'NONE',  ( 4.956219290344169970, 1.285291309562084816, 1.163873732738918587 ) ) ;
#113112 = CARTESIAN_POINT ( 'NONE',  ( 4.721225823269111110, -1.937324205527543253, -0.9803755122778281539 ) ) ;
#113113 = CARTESIAN_POINT ( 'NONE',  ( 3.521367211247359741, 5.131347717920458962, -1.599625672291262513 ) ) ;
#113114 = CARTESIAN_POINT ( 'NONE',  ( 5.788296071918774821, -0.7303023681345042206, -1.879805717804765353 ) ) ;
#113115 = CARTESIAN_POINT ( 'NONE',  ( 5.000000000000003553, -2.717005030479747438E-13, -2.052068128417942727 ) ) ;
#113116 = CARTESIAN_POINT ( 'NONE',  ( -1.001543065824772872E-14, 4.993750000682814161, 1.732050807568877637 ) ) ;
#113117 = CARTESIAN_POINT ( 'NONE',  ( 2.713793335149127905, -1.905670363949378165, 0.2809714450454863233 ) ) ;
#113118 = CARTESIAN_POINT ( 'NONE',  ( 0.7500000000000006661, 10.11458333401612997, 1.299038105676657340 ) ) ;
#113119 = CARTESIAN_POINT ( 'NONE',  ( 6.504121277450023442, -0.9500910533294173455, 2.005660710250598555 ) ) ;
#113120 = ORIENTED_EDGE ( 'NONE', *, *, #174390, .T. ) ;
#113121 = CARTESIAN_POINT ( 'NONE',  ( 6.883263157960393563, 4.695771316066229772, 2.508818740863460572 ) ) ;
#113122 = CARTESIAN_POINT ( 'NONE',  ( -1.500000000000011324, 3.170833333333354265, 0.8660254037844403729 ) ) ;
#113123 = CARTESIAN_POINT ( 'NONE',  ( 5.799137018343234473, 7.788745826199009237, -1.599625672291262513 ) ) ;
#113124 = CARTESIAN_POINT ( 'NONE',  ( 1.383751715516433833, 0.1588885597470449385, -2.215665637441687430 ) ) ;
#113125 = CARTESIAN_POINT ( 'NONE',  ( 6.760214184729610665, -1.961454122871961747, 0.04698431645466792650 ) ) ;
#113126 = CARTESIAN_POINT ( 'NONE',  ( 6.453317930424781856, 10.47269531889685545, -0.7216878364870267237 ) ) ;
#113127 = PLANE ( 'NONE',  #145834 ) ;
#113128 = CARTESIAN_POINT ( 'NONE',  ( 3.393283585170187688, 7.180857625999046867, 0.7998128361456271485 ) ) ;
#113129 = CARTESIAN_POINT ( 'NONE',  ( -4.990809943606294929, 4.995235487061662205, -0.7216878364870338292 ) ) ;
#113131 = CARTESIAN_POINT ( 'NONE',  ( 5.020015070024019366, 2.040704184028362178, -0.2994381943521097766 ) ) ;
#113130 = CYLINDRICAL_SURFACE ( 'NONE', #178585, 0.7500000000000011102 ) ;
#113132 = CARTESIAN_POINT ( 'NONE',  ( 3.511198596259283544, 6.271927390929319834, 1.164732466530402855 ) ) ;
#113133 = CARTESIAN_POINT ( 'NONE',  ( -5.115504031057831469, 4.862509545855891346, 0.7998128361456341429 ) ) ;
#113134 = CARTESIAN_POINT ( 'NONE',  ( -0.7499999999999972244, 5.139583334016151639, -1.299038105676652899 ) ) ;
#113135 = CARTESIAN_POINT ( 'NONE',  ( -0.6823417656250246877, -0.6989583329919113464, 1.181850606188755259 ) ) ;
#113136 = CARTESIAN_POINT ( 'NONE',  ( 6.661405586796748324, 0.3194099797865917467, -1.842918054787325843 ) ) ;
#113137 = CARTESIAN_POINT ( 'NONE',  ( 6.029869095562110815, -1.459853974539515153, 0.9356793305193217281 ) ) ;
#113138 = CARTESIAN_POINT ( 'NONE',  ( 4.054071295385909934, -1.286197829845928675, 1.172710138673456415 ) ) ;
#113139 = CARTESIAN_POINT ( 'NONE',  ( 3.822509244049070887, 6.547012320444182798, -1.199719254218452047 ) ) ;
#113140 = CARTESIAN_POINT ( 'NONE',  ( 2.929518028021148357, -1.541346711875633435, -1.696969020646617476 ) ) ;
#113141 = CARTESIAN_POINT ( 'NONE',  ( 0.6823417656249899377, 5.488541667008087543, -1.181850606188754593 ) ) ;
#113142 = CARTESIAN_POINT ( 'NONE',  ( 1.095364067855080448, -1.841320589428995236, -0.001981933617903330457 ) ) ;
#113143 = EDGE_CURVE ( 'NONE', #138277, #65489, #66844, .T. ) ;
#113144 = CARTESIAN_POINT ( 'NONE',  ( 4.131884898838331210, 7.654771682445123737, 0.7704574788214838543 ) ) ;
#113145 = CARTESIAN_POINT ( 'NONE',  ( 9.367496997597603681, 3.999999999999998224, -7.499999999999998224 ) ) ;
#113146 = CARTESIAN_POINT ( 'NONE',  ( 2.344514592193002400, 0.3973361102717865023, 1.781653928021959432 ) ) ;
#113147 = CARTESIAN_POINT ( 'NONE',  ( 3.076796235938107138, -0.8146265060355701859, 1.844709937164576097 ) ) ;
#113148 = CARTESIAN_POINT ( 'NONE',  ( 1.711130781365449716, -0.2659051965858104660, 2.175189728913041964 ) ) ;
#113149 = CARTESIAN_POINT ( 'NONE',  ( 10.03198553058017772, 14.16803135393298874, -7.469060636793986241 ) ) ;
#113150 = CARTESIAN_POINT ( 'NONE',  ( 4.260836881943074417, -1.562014524604074861, 1.412707936923715879 ) ) ;
#113151 = CARTESIAN_POINT ( 'NONE',  ( -6.690058733339450114, 9.892486724616283311, 1.199719254218452047 ) ) ;
#113152 = CARTESIAN_POINT ( 'NONE',  ( 6.853823584984077399, 13.99925803066161478, 9.461486148285766618 ) ) ;
#113153 =( BOUNDED_SURFACE ( )  B_SPLINE_SURFACE ( 3, 2, ( 
 ( #64047, #97633, #178881 ),
 ( #44619, #81359, #144287 ),
 ( #177809, #65087, #160482 ),
 ( #30493, #61920, #96577 ),
 ( #164738, #130192, #14200 ),
 ( #69, #12089, #98682 ),
 ( #196185, #79229, #162624 ),
 ( #80293, #147439, #146391 ) ),
 .UNSPECIFIED., .F., .F., .T. ) 
 B_SPLINE_SURFACE_WITH_KNOTS ( ( 4, 2, 2, 4 ),
 ( 3, 3 ),
 ( -6.505213034913026604E-19, 0.0002575597274893380085, 0.0005151194549786766675, 0.001030238909957353986 ),
 ( 0.000000000000000000, 1.000000000000000000 ),
 .UNSPECIFIED. ) 
 GEOMETRIC_REPRESENTATION_ITEM ( )  RATIONAL_B_SPLINE_SURFACE ( (
 ( 1.000000000000000000, 0.9238795325112806323, 1.000000000000000000),
 ( 1.000000000000000000, 0.9228594682463592269, 1.000000000000000000),
 ( 1.000000000000000000, 0.9150875845227820493, 1.000000000000000000),
 ( 1.000000000000000000, 0.8905471774192091905, 1.000000000000000000),
 ( 1.000000000000000000, 0.8740340839248708082, 1.000000000000000000),
 ( 1.000000000000000000, 0.8160099319845808274, 1.000000000000000000),
 ( 1.000000000000000000, 0.7673743911479409263, 1.000000000000000000),
 ( 1.000000000000000000, 0.7100530722070714784, 1.000000000000000000) ) ) 
 REPRESENTATION_ITEM ( '' )  SURFACE ( )  );
#113154 = CARTESIAN_POINT ( 'NONE',  ( 1.873570696236816158, -0.2555354716398828274, 2.054483085851127377 ) ) ;
#113155 = CARTESIAN_POINT ( 'NONE',  ( 4.330940004561544043, 7.140181541042074365, -1.199719254218452047 ) ) ;
#113156 = CARTESIAN_POINT ( 'NONE',  ( -3.355169270512988773E-14, -0.6406249996585449136, -1.570758158831794260 ) ) ;
#113157 = CARTESIAN_POINT ( 'NONE',  ( 3.106218681870171139, -0.8574772492565513327, 1.939554460742904274 ) ) ;
#113158 = AXIS2_PLACEMENT_3D ( 'NONE', #71635, #72716, #6637 ) ;
#113159 = CARTESIAN_POINT ( 'NONE',  ( 6.674438497507635404, -1.118711561685633349, 1.443368817030561635 ) ) ;
#113160 = EDGE_LOOP ( 'NONE', ( #203905, #59749, #25009 ) ) ;
#113161 = CARTESIAN_POINT ( 'NONE',  ( -4.294900800479008574, 8.232744377192641849, 0.000000000000000000 ) ) ;
#113162 = CARTESIAN_POINT ( 'NONE',  ( 8.561083932025322696, 12.07534945641652158, -1.199719254218446718 ) ) ;
#113163 = CARTESIAN_POINT ( 'NONE',  ( 5.343321937117211817, 9.247976336696488886, 0.000000000000000000 ) ) ;
#113164 = CARTESIAN_POINT ( 'NONE',  ( 1.001543065824772753E-15, -2.668749999044085719, 4.012584370867899430 ) ) ;
#113165 = CARTESIAN_POINT ( 'NONE',  ( -6.254388934605767503, 6.191208599995166040, 0.7998128361456341429 ) ) ;
#113166 = CARTESIAN_POINT ( 'NONE',  ( 5.994406619193555663, -1.133004004027007294, 1.792352430775605798 ) ) ;
#113167 = CARTESIAN_POINT ( 'NONE',  ( 1.518734001684220347, 1.414770742371696644, -1.560122519311944345 ) ) ;
#113168 = CARTESIAN_POINT ( 'NONE',  ( -5.468734858265826837, 7.473552982767158070, 1.599625672291263179 ) ) ;
#113169 = CARTESIAN_POINT ( 'NONE',  ( 7.730120138085914583, 12.17022392774227768, 0.7998128361456462443 ) ) ;
#113170 = CARTESIAN_POINT ( 'NONE',  ( 5.330833089851809703, -1.751472900985746373, -0.6291486930528921162 ) ) ;
#113171 = CARTESIAN_POINT ( 'NONE',  ( 6.889514614038635187, 11.18951748302043114, -0.7998128361456291469 ) ) ;
#113172 =( BOUNDED_SURFACE ( )  B_SPLINE_SURFACE ( 3, 3, ( 
 ( #196333, #97782, #45832, #17541, #47977, #210428, #46903, #32757, #164889, #161712 ),
 ( #79377, #64203, #180084, #145496, #65235, #63128, #16483, #66287, #131385, #129292 ),
 ( #113017, #197381, #115141, #96728, #162777, #14355, #82564, #51143, #150791, #120486 ),
 ( #121558, #1293, #200562, #135602, #71628, #2354, #19693, #137741, #149713, #70553 ),
 ( #134559, #20744, #184321, #68430, #21799, #202697, #4482, #69495, #54347, #136672 ),
 ( #55404, #18625, #186458, #53272, #87907, #199499, #35946, #34869, #86839, #3428 ),
 ( #169151, #52209, #117267, #118336, #183265, #201623, #203761, #100943, #38095, #67351 ) ),
 .UNSPECIFIED., .T., .F., .T. ) 
 B_SPLINE_SURFACE_WITH_KNOTS ( ( 4, 3, 4 ),
 ( 4, 1, 1, 1, 1, 1, 1, 4 ),
 ( 0.000000000000000000, 0.5000000000000000000, 1.000000000000000000 ),
 ( 0.000000000000000000, 0.09487947018404768729, 0.1878442364269655440, 0.2584026419818104547, 0.3617053504666527530, 0.5211417612611924932, 0.7337075935910832847, 1.000000000000000000 ),
 .UNSPECIFIED. ) 
 GEOMETRIC_REPRESENTATION_ITEM ( )  RATIONAL_B_SPLINE_SURFACE ( (
 ( 1.000000000000000000, 1.000000000000000000, 1.000000000000000000, 0.9999999999999996669, 1.000000000000000222, 1.000000000000000000, 1.000000000000000222, 0.9999999999999997780, 1.000000000000000000, 1.000000000000000000),
 ( 0.3333333333333333703, 0.3333333333333333703, 0.3333333333333334259, 0.3333333333333332593, 0.3333333333333334814, 0.3333333333333333148, 0.3333333333333334259, 0.3333333333333333148, 0.3333333333333333703, 0.3333333333333333703),
 ( 0.3333333333333333703, 0.3333333333333333703, 0.3333333333333334259, 0.3333333333333332593, 0.3333333333333334814, 0.3333333333333333148, 0.3333333333333334259, 0.3333333333333333148, 0.3333333333333333703, 0.3333333333333333703),
 ( 1.000000000000000000, 1.000000000000000000, 1.000000000000000000, 0.9999999999999996669, 1.000000000000000222, 1.000000000000000000, 1.000000000000000222, 0.9999999999999997780, 1.000000000000000000, 1.000000000000000000),
 ( 0.3333333333333333703, 0.3333333333333333703, 0.3333333333333334259, 0.3333333333333332593, 0.3333333333333334814, 0.3333333333333333148, 0.3333333333333334259, 0.3333333333333333148, 0.3333333333333333703, 0.3333333333333333703),
 ( 0.3333333333333333703, 0.3333333333333333703, 0.3333333333333334259, 0.3333333333333332593, 0.3333333333333334814, 0.3333333333333333148, 0.3333333333333334259, 0.3333333333333333148, 0.3333333333333333703, 0.3333333333333333703),
 ( 1.000000000000000000, 1.000000000000000000, 1.000000000000000000, 0.9999999999999996669, 1.000000000000000222, 1.000000000000000000, 1.000000000000000222, 0.9999999999999997780, 1.000000000000000000, 1.000000000000000000) ) ) 
 REPRESENTATION_ITEM ( '' )  SURFACE ( )  );
#113173 = DIRECTION ( 'NONE',  ( 1.000000000000000000, 0.000000000000000000, 0.000000000000000000 ) ) ;
#113174 = CARTESIAN_POINT ( 'NONE',  ( -5.008811405605897882, 4.808311159487113073, 0.7998128361456281477 ) ) ;
#113175 = CARTESIAN_POINT ( 'NONE',  ( -8.676855123066012254, 12.10645282934361866, -1.082531754730543971 ) ) ;
#113177 = CARTESIAN_POINT ( 'NONE',  ( 2.734756269166933151, -1.876540383875524576, -0.5722209215143353456 ) ) ;
#113176 = CARTESIAN_POINT ( 'NONE',  ( -6.181627972826976958, 9.299317504018391745, 1.199719254218452047 ) ) ;
#113178 = CARTESIAN_POINT ( 'NONE',  ( 1.428841412761387986, 2.083414371474631377, 0.5762002773818803991 ) ) ;
#113180 = CARTESIAN_POINT ( 'NONE',  ( -5.460715490240072079, 6.444878312648672392, 1.304320558087665782 ) ) ;
#113179 = CARTESIAN_POINT ( 'NONE',  ( -5.424143973919053785, 8.485862515284315677, 1.199719254218454489 ) ) ;
#113181 = CARTESIAN_POINT ( 'NONE',  ( 0.6823417656249882723, 0.4260416670080896528, -1.181850606188749264 ) ) ;
#113182 = CARTESIAN_POINT ( 'NONE',  ( 2.618122797784384836, 0.4666061159355525678, -1.669766330342295158 ) ) ;
#113183 = CARTESIAN_POINT ( 'NONE',  ( 2.835604015501072439, 1.727201357243525637, 0.2126739171897980840 ) ) ;
#113185 = CARTESIAN_POINT ( 'NONE',  ( 6.453317930424781856, 10.47269531889685545, -0.7216878364870267237 ) ) ;
#113184 = CARTESIAN_POINT ( 'NONE',  ( 6.463506322211490129, 0.4017315814064837953, -2.272322137143814480 ) ) ;
#113186 = CARTESIAN_POINT ( 'NONE',  ( -11.50375155617990686, 6.427325993555151662, 3.051984382272954210 ) ) ;
#113187 = CARTESIAN_POINT ( 'NONE',  ( 3.022786435837477637, 1.939216523002813997, 0.6976457746366692136 ) ) ;
#113188 = CARTESIAN_POINT ( 'NONE',  ( 0.6321852052597470850, 0.2004073784105386835, -2.006138679842318862 ) ) ;
#113189 = CARTESIAN_POINT ( 'NONE',  ( 6.925078400183521055, 4.691537398408025972, 2.606905763235977336 ) ) ;
#113190 = CARTESIAN_POINT ( 'NONE',  ( -4.390861645979385663, 6.216034235099629157, -1.599625672291271394 ) ) ;
#113191 = CARTESIAN_POINT ( 'NONE',  ( 1.217580299722145210, -1.923910348332603881, 0.4297500124877791650 ) ) ;
#113192 =( GEOMETRIC_REPRESENTATION_CONTEXT ( 3 ) GLOBAL_UNCERTAINTY_ASSIGNED_CONTEXT ( ( #204428 ) ) GLOBAL_UNIT_ASSIGNED_CONTEXT ( ( #33353, #195864, #31239 ) ) REPRESENTATION_CONTEXT ( 'NONE', 'WORKASPACE' ) );
#113194 = CARTESIAN_POINT ( 'NONE',  ( -4.800995793014949165, 8.615262501910491366, 0.7216878364870267237 ) ) ;
#113193 = CARTESIAN_POINT ( 'NONE',  ( 5.361546783204238942, -1.511448857895525855, -1.171587532507123441 ) ) ;
#113195 = CARTESIAN_POINT ( 'NONE',  ( -6.089020385868862739, 8.197219431637373432, -1.443375672974066548 ) ) ;
#113196 = CARTESIAN_POINT ( 'NONE',  ( 7.038618024149998043, 8.240751112043669835, -1.199719254218452047 ) ) ;
#113197 = CARTESIAN_POINT ( 'NONE',  ( -5.932574734431526942, 9.079031735882207244, 1.199719254218454489 ) ) ;
#113198 = CARTESIAN_POINT ( 'NONE',  ( 1.365885014167470546, 0.5842608817006667010, -1.933330045775418116 ) ) ;
#113199 = PRESENTATION_STYLE_ASSIGNMENT (( #126264 ) ) ;
#113200 = CARTESIAN_POINT ( 'NONE',  ( 4.876155869083551586, 1.324110019830313734, 1.889726917317616328 ) ) ;
#113201 = CARTESIAN_POINT ( 'NONE',  ( 5.494571831323358246, 1.932540981948445147, 0.3370517209014682325 ) ) ;
#113202 = CARTESIAN_POINT ( 'NONE',  ( 1.586688997538304058, 1.889165970957426444, 0.5283831072378852856 ) ) ;
#113203 = CARTESIAN_POINT ( 'NONE',  ( 9.531545685607134999, 11.07889037375188401, 1.199719254218450271 ) ) ;
#113204 = CARTESIAN_POINT ( 'NONE',  ( -0.1399997263889594112, -0.002789056014654289761, -2.000146600338557956 ) ) ;
#113205 = ORIENTED_EDGE ( 'NONE', *, *, #137027, .T. ) ;
#113206 = CARTESIAN_POINT ( 'NONE',  ( 1.095081093118466908, 1.870138624552514006, 0.9927810678921239473 ) ) ;
#113208 = CARTESIAN_POINT ( 'NONE',  ( -7.019370843573183194, 9.212351955633947043, 1.599625672291283607 ) ) ;
#113207 = CARTESIAN_POINT ( 'NONE',  ( -6.098470168048611306, 6.009303372345148553, 1.040834085586084257E-14 ) ) ;
#113209 = CARTESIAN_POINT ( 'NONE',  ( 0.9898993202219902310, -0.4452471680344311511, -1.786356756097874587 ) ) ;
#113210 = ORIENTED_EDGE ( 'NONE', *, *, #182043, .T. ) ;
#113211 = CARTESIAN_POINT ( 'NONE',  ( 4.258752264053907055, -0.6753675163390076008, -2.063452119831588494 ) ) ;
#113212 = CARTESIAN_POINT ( 'NONE',  ( 11.90231137465227285, 7.647702690253872504, -1.097913969704247927 ) ) ;
#113213 = CARTESIAN_POINT ( 'NONE',  ( 1.582450481569739331, 1.094613367649547309, 1.816135667671102016 ) ) ;
#113214 = CARTESIAN_POINT ( 'NONE',  ( -1.402160292154681736E-14, 2.618750000682819490, -1.732050807568863648 ) ) ;
#113215 = CARTESIAN_POINT ( 'NONE',  ( 7.553864141108259211, 11.96459193126834464, 1.040834085586084257E-14 ) ) ;
#113216 = CARTESIAN_POINT ( 'NONE',  ( -1.862912430430173627, 2.484159785402544784, -2.477813002740275827 ) ) ;
#113217 = CARTESIAN_POINT ( 'NONE',  ( 2.952472966291960876, 0.6911811108033919515, 1.941568756818631725 ) ) ;
#113219 = CARTESIAN_POINT ( 'NONE',  ( 0.5207438388301621757, -1.748553680932497745, 0.5769860859521497298 ) ) ;
#113218 = CARTESIAN_POINT ( 'NONE',  ( -7.991641480251377772, 11.41099992934688956, 1.199719254218453823 ) ) ;
#113220 = CARTESIAN_POINT ( 'NONE',  ( 1.364683531249988535, 3.405208333674749621, -0.7879004041258239610 ) ) ;
#113221 = CARTESIAN_POINT ( 'NONE',  ( 0.07755575628181145265, 7.629137130509078268, -2.788902932953695846 ) ) ;
#113222 = CARTESIAN_POINT ( 'NONE',  ( 1.493068410184935191, 4.435370284924327500, -0.1642227666888356197 ) ) ;
#113223 =( BOUNDED_SURFACE ( )  B_SPLINE_SURFACE ( 1, 2, ( 
 ( #38585, #51643, #167515, #68916, #135036, #103587, #201049, #118821, #169644, #21229, #22294, #36437, #102512, #20175, #87333, #4971, #120985, #170709, #154475, #166447, #18039, #157681, #189098, #191212, #27658, #92689, #59091, #9279, #141464, #75350, #155542, #42875, #122054, #142513, #188018, #105754, #205329, #90550, #206403, #172868, #58028, #108983, #207472, #175002, #26588, #140384, #158735, #156614, #176062, #10330, #171781, #173948, #56967, #73194, #192273, #125251, #138231, #40731, #41810, #24439, #7121, #23377, #76404, #123140, #43934, #208522, #60157, #89487, #126313, #93754, #110049, #124192, #6053, #39646, #72124, #55897, #139300, #106837, #204245, #190155, #8204, #74289, #107923, #25521, #91629, #197612, #65462, #210670, #49256, #46066, #115377, #160869, #31937, #113254, #129521, #127385, #144655, #12463, #111112, #28733, #62298, #15656, #179259, #177116, #145727, #196565, #94818, #159792, #131613, #13538, #163008, #30881, #130575, #193358, #80687, #213843, #212793, #48207, #96960, #146778, #79608, #11395, #14590, #64431, #195501, #194425, #81743, #181371, #77473, #47137, #143592, #112187, #32995, #128457, #78538, #178191, #29807, #95893, #209584, #161946, #211727, #114319, #63365, #180317, #61230, #164076, #98021, #147825, #45002, #68663, #67587, #19923, #100124, #53506, #36178, #87072, #82801, #133732, #169390, #165125, #16716, #51385, #117506, #166186, #153142, #135835, #185624, #148877, #134787, #86009, #199739, #450, #83863, #136905, #152083, #17775, #70792, #149954, #151025, #119641, #37257, #3653, #66518, #132661, #103327, #198665, #20975, #167267, #1523, #35107, #4717, #183498, #34051, #69731, #101178, #2594, #102254, #99072, #50313, #18852, #201860, #200794, #116431, #182424, #168328, #52445, #84936, #118571, #184557, #202932, #54575, #120723, #186696, #206149, #74032, #91369, #108731, #121794, #71862, #89230, #55638, #187762, #156357, #76158, #23113, #42621, #122882, #173692, #203990, #57777, #155282, #105487, #10084, #25268, #170450, #72942, #140123, #56713, #39392, #171520, #75098, #6863, #142263, #26332, #124999, #139045, #189906, #59906, #41551, #24184, #208274, #154213, #126060, #88146, #5785, #205071, #157430, #172608, #40476, #137971, #188840, #158485, #106580, #123938, #107664, #9023, #174758, #90288, #7942, #141208, #207219, #58842, #190956, #38325, #92446, #104401, #22035, #111940, #145482, #193104, #192023, #175812, #45819, #65218, #31693, #97768, #27405, #79364, #29556, #194174, #177942, #44754, #62057, #43685, #179013, #162764, #94570, #159544, #95647, #160614, #161698, #80430, #110861, #143337, #130329, #176867, #144413, #93503, #11141, #12215, #163828, #78286, #28479, #210415, #128212, #13291, #77218, #211478, #209331, #30629, #63114, #129279, #213594, #196318, #113002, #195253, #109803, #46889, #96715, #14341, #146530, #212547, #64188, #180069, #60979, #47962, #114078, #127133, #15406, #81497, #147575, #132419, #119386, #168077, #3412, #115126, #100928, #118319, #99880, #197367, #116187, #169133, #184305, #50064, #103078, #198420, #183250, #85755, #69478, #35929, #49008, #32742, #151836, #98824, #135586, #199483, #182172, #67336, #201607, #149697, #66271, #102007, #133481, #34853, #68415, #131370, #82548, #51129, #19675, #167016, #148635, #164873, #134542, #18609, #117251, #84689, #150776, #2338, #53256, #185374, #201, #16468, #33801, #165942, #17527, #200547, #20728, #83615, #52193, #1278, #36994, #86823, #152887, #181122, #4465, #138788, #158240, #124744, #190703, #120469, #172347, #122621, #72693, #204808, #137724, #155028, #136656, #57529, #41299, #187514, #38078, #188582, #39145, #56459, #173430, #203743, #21782, #8766, #55388, #22860, #54330, #186441, #105226, #42365, #171266, #121543, #88973, #6613, #40215, #104150, #106324, #87891, #123686, #23937, #90041, #92191, #74848, #205895, #156099, #70537, #7684, #73768, #189648, #71611, #25010, #139864, #58589, #170198, #107407, #140947, #202681, #153964, #91111, #157171, #206960, #108476, #174499, #26077, #5531, #193912, #211220, #192834, #75905, #209076, #47695, #62846, #143082, #196065, #10882, #61791, #178752 ),
 ( #160356, #127958, #161437, #9829, #175555, #78032, #46620, #45559, #27145, #43426, #13018, #111674, #11959, #177681, #144157, #191771, #109550, #130070, #76957, #212280, #208024, #44493, #80163, #142009, #59650, #176610, #28222, #60713, #63914, #112741, #96452, #125809, #29293, #129007, #110610, #93249, #126877, #113809, #194984, #94315, #179810, #210148, #95385, #30365, #162503, #14073, #159283, #79095, #146268, #145213, #31429, #97506, #164616, #99615, #184047, #181910, #98555, #2075, #165681, #1012, #100672, #163563, #114859, #17269, #200287, #199218, #180859, #197106, #166750, #50865, #83345, #116987, #149430, #131118, #48746, #69214, #16201, #182987, #34604, #68149, #19412, #32481, #82283, #214377, #148376, #66007, #67077, #201347, #132157, #133212, #198162, #18345, #84425, #49796, #15147, #147315, #150514, #36729, #3145, #135333, #213342, #134282, #51938, #118062, #35665, #115922, #33542, #81233, #101744, #167812, #85490, #151577, #52987, #119123, #185103, #64965, #169935, #54067, #43968, #87630, #55132, #86562, #152624, #137464, #11431, #71347, #21519, #153702, #203479, #5270, #4211, #121277, #120202, #89790, #38880, #6352, #127422, #110083, #23679, #122359, #193394, #72423, #187253, #155836, #103887, #60189, #39957, #77507, #104964, #56197, #138525, #7420, #176095, #186177, #136395, #171006, #37811, #22603, #204548, #143627, #88710, #188316, #154769, #106064, #172087, #73502, #102816, #70279, #139604, #168871, #159830, #209621, #202411, #205628, #126349, #192308, #27694, #93792, #61263, #20475, #31971, #15690, #161980, #12499, #96993, #13571, #47174, #147858, #112221, #210705, #197646, #29843, #211760, #28770, #94852, #79644, #165156, #145760, #178228, #95925, #63398, #129552, #160903, #195537, #62333, #98052, #113287, #163045, #66549, #49292, #180348, #64466, #132692, #14624, #179293, #164106, #46103, #213874, #196596, #33027, #78572, #30917, #115409, #111151, #177151, #80719, #146809, #212828, #99105, #81776, #131644, #144692, #130608, #65496, #48239, #128492, #114352, #82834, #181402, #16749, #148909, #483, #45038, #194458, #70821, #185654, #116464, #100156, #153170, #166219, #136937, #52472, #199769, #134816, #4746, #2622, #133761, #37285, #200821, #36204, #135865, #198699, #149983, #118597, #21004, #19952, #1555, #17809, #201885, #86036, #184586, #152112, #102280, #83892, #67617, #34084, #3683, #168357, #69760, #53535, #51414, #68693, #50343, #103358, #169421, #101209, #117535, #119667, #167296, #87101, #202964, #183530, #35136, #54604, #18882, #151059, #182456, #84967, #120752, #104431, #186730, #38353, #170478, #22064, #88175, #154247, #5819, #71894, #125031, #74061, #41581, #159577, #142297, #58875, #157461, #11174, #107696, #106611, #190988, #139076, #92476, #75131, #126092, #121823, #172638, #208307, #204019, #55667, #90316, #156387, #205099, #192053, #174787, #10114, #187792, #173722, #42652, #24214, #39421, #122909, #175844, #108762, #56741, #109834, #188867, #189936, #158516, #76189, #26362, #105515, #171549, #59937, #23144, #43718, #206178, #40507, #140153, #27435, #7971, #72971, #93533, #57807, #25299, #141240, #138002, #89260, #123968, #155310, #91401, #6893, #9056, #207249, #179043, #79394, #30661, #145512, #44786, #176899, #197398, #78319, #96745, #113037, #130362, #147608, #160644, #110892, #128242, #94602, #12244, #195287, #115161, #62084, #46919, #111971, #211511, #162795, #144443, #77250, #61010, #63147, #164907, #131401, #49041, #210446, #196351, #13321, #129309, #14372, #143367, #28512, #80462, #114109, #146561, #194206, #45851, #212581, #64221, #47994, #180101, #31727, #177974, #29587, #181155, #95675, #97800, #163859, #15439, #213627, #161729, #81528, #65252, #32778, #98856, #209364, #127167, #193138, #134581, #51166, #150810, #184344, #17561, #16502, #236, #84722, #104186, #70573, #136691, #66309, #118357, #68452, #18643, #2374, #83647, #100962, #82583, #3447, #201644, #133515, #198455, #200581, #199521, #52229, #119424, #149733, #182212, #169172, #1311, #183285, #132456, #50100, #117288, #202716, #34890, #67373, #167051, #35967, #102045, #116221, #168114, #33836, #69514 ) ),
 .UNSPECIFIED., .F., .F., .T. ) 
 B_SPLINE_SURFACE_WITH_KNOTS ( ( 2, 2 ),
 ( 3, 2, 2, 2, 2, 2, 2, 2, 2, 2, 2, 2, 2, 2, 2, 2, 2, 2, 2, 2, 2, 2, 2, 2, 2, 2, 2, 2, 2, 2, 2, 2, 2, 2, 2, 2, 2, 2, 2, 2, 2, 2, 2, 2, 2, 2, 2, 2, 2, 2, 2, 2, 2, 2, 2, 2, 2, 2, 2, 2, 2, 2, 2, 2, 2, 2, 2, 2, 2, 2, 2, 2, 2, 2, 2, 2, 2, 2, 2, 2, 2, 2, 2, 2, 2, 2, 2, 2, 2, 2, 2, 2, 2, 2, 2, 2, 2, 2, 2, 2, 2, 2, 2, 2, 2, 2, 2, 2, 2, 2, 2, 2, 2, 2, 2, 2, 2, 2, 2, 2, 2, 2, 2, 2, 2, 2, 2, 2, 2, 2, 2, 2, 2, 2, 2, 2, 2, 2, 2, 2, 2, 2, 2, 2, 2, 2, 2, 2, 2, 2, 2, 2, 2, 2, 2, 2, 2, 2, 2, 2, 2, 2, 2, 2, 2, 2, 2, 2, 2, 2, 2, 2, 2, 2, 2, 2, 2, 2, 2, 2, 2, 2, 2, 2, 2, 2, 2, 2, 2, 2, 2, 2, 2, 2, 2, 2, 2, 2, 2, 2, 2, 2, 2, 2, 2, 2, 2, 2, 2, 2, 2, 2, 2, 2, 2, 2, 2, 2, 2, 2, 2, 2, 2, 2, 2, 2, 2, 2, 2, 2, 2, 2, 2, 2, 2, 2, 2, 2, 2, 2, 3 ),
 ( 0.000000000000000000, 1.000000000000000000 ),
 ( 0.000000000000000000, 0.004166666666666666609, 0.008333333333333333218, 0.01250000000000000069, 0.01666666666666666644, 0.02083333333333333218, 0.02500000000000000139, 0.02916666666666666713, 0.03333333333333333287, 0.03749999999999999861, 0.04166666666666666435, 0.04583333333333333010, 0.05000000000000000278, 0.05416666666666666852, 0.05833333333333333426, 0.06250000000000000000, 0.06666666666666666574, 0.07083333333333333148, 0.07499999999999999722, 0.07916666666666666297, 0.08333333333333332871, 0.08749999999999999445, 0.09166666666666666019, 0.09583333333333333981, 0.1000000000000000056, 0.1041666666666666713, 0.1083333333333333370, 0.1125000000000000028, 0.1166666666666666685, 0.1208333333333333343, 0.1250000000000000000, 0.1291666666666666796, 0.1333333333333333315, 0.1375000000000000111, 0.1416666666666666630, 0.1458333333333333426, 0.1499999999999999944, 0.1541666666666666741, 0.1583333333333333259, 0.1625000000000000056, 0.1666666666666666574, 0.1708333333333333370, 0.1749999999999999889, 0.1791666666666666685, 0.1833333333333333204, 0.1875000000000000000, 0.1916666666666666796, 0.1958333333333333315, 0.2000000000000000111, 0.2041666666666666630, 0.2083333333333333426, 0.2124999999999999944, 0.2166666666666666741, 0.2208333333333333259, 0.2250000000000000056, 0.2291666666666666574, 0.2333333333333333370, 0.2374999999999999889, 0.2416666666666666685, 0.2458333333333333204, 0.2500000000000000000, 0.2541666666666666519, 0.2583333333333333592, 0.2625000000000000111, 0.2666666666666666630, 0.2708333333333333148, 0.2750000000000000222, 0.2791666666666666741, 0.2833333333333333259, 0.2874999999999999778, 0.2916666666666666852, 0.2958333333333333370, 0.2999999999999999889, 0.3041666666666666408, 0.3083333333333333481, 0.3125000000000000000, 0.3166666666666666519, 0.3208333333333333592, 0.3250000000000000111, 0.3291666666666666630, 0.3333333333333333148, 0.3375000000000000222, 0.3416666666666666741, 0.3458333333333333259, 0.3499999999999999778, 0.3541666666666666852, 0.3583333333333333370, 0.3624999999999999889, 0.3666666666666666408, 0.3708333333333333481, 0.3750000000000000000, 0.3791666666666666519, 0.3833333333333333592, 0.3875000000000000111, 0.3916666666666666630, 0.3958333333333333148, 0.4000000000000000222, 0.4041666666666666741, 0.4083333333333333259, 0.4124999999999999778, 0.4166666666666666852, 0.4208333333333333370, 0.4249999999999999889, 0.4291666666666666408, 0.4333333333333333481, 0.4375000000000000000, 0.4416666666666666519, 0.4458333333333333592, 0.4500000000000000111, 0.4541666666666666630, 0.4583333333333333148, 0.4625000000000000222, 0.4666666666666666741, 0.4708333333333333259, 0.4749999999999999778, 0.4791666666666666852, 0.4833333333333333370, 0.4874999999999999889, 0.4916666666666666408, 0.4958333333333333481, 0.5000000000000000000, 0.5041666666666666519, 0.5083333333333333037, 0.5124999999999999556, 0.5166666666666667185, 0.5208333333333333703, 0.5250000000000000222, 0.5291666666666666741, 0.5333333333333333259, 0.5374999999999999778, 0.5416666666666666297, 0.5458333333333332815, 0.5500000000000000444, 0.5541666666666666963, 0.5583333333333333481, 0.5625000000000000000, 0.5666666666666666519, 0.5708333333333333037, 0.5749999999999999556, 0.5791666666666667185, 0.5833333333333333703, 0.5875000000000000222, 0.5916666666666666741, 0.5958333333333333259, 0.5999999999999999778, 0.6041666666666666297, 0.6083333333333332815, 0.6125000000000000444, 0.6166666666666666963, 0.6208333333333333481, 0.6250000000000000000, 0.6291666666666666519, 0.6333333333333333037, 0.6374999999999999556, 0.6416666666666667185, 0.6458333333333333703, 0.6500000000000000222, 0.6541666666666666741, 0.6583333333333333259, 0.6624999999999999778, 0.6666666666666666297, 0.6708333333333332815, 0.6750000000000000444, 0.6791666666666666963, 0.6833333333333333481, 0.6875000000000000000, 0.6916666666666666519, 0.6958333333333333037, 0.6999999999999999556, 0.7041666666666667185, 0.7083333333333333703, 0.7125000000000000222, 0.7166666666666666741, 0.7208333333333333259, 0.7249999999999999778, 0.7291666666666666297, 0.7333333333333332815, 0.7375000000000000444, 0.7416666666666666963, 0.7458333333333333481, 0.7500000000000000000, 0.7541666666666666519, 0.7583333333333333037, 0.7624999999999999556, 0.7666666666666667185, 0.7708333333333333703, 0.7750000000000000222, 0.7791666666666666741, 0.7833333333333333259, 0.7874999999999999778, 0.7916666666666666297, 0.7958333333333332815, 0.8000000000000000444, 0.8041666666666666963, 0.8083333333333333481, 0.8125000000000000000, 0.8166666666666666519, 0.8208333333333333037, 0.8249999999999999556, 0.8291666666666667185, 0.8333333333333333703, 0.8375000000000000222, 0.8416666666666666741, 0.8458333333333333259, 0.8499999999999999778, 0.8541666666666666297, 0.8583333333333332815, 0.8625000000000000444, 0.8666666666666666963, 0.8708333333333333481, 0.8750000000000000000, 0.8791666666666666519, 0.8833333333333333037, 0.8874999999999999556, 0.8916666666666667185, 0.8958333333333333703, 0.9000000000000000222, 0.9041666666666666741, 0.9083333333333333259, 0.9124999999999999778, 0.9166666666666666297, 0.9208333333333332815, 0.9250000000000000444, 0.9291666666666666963, 0.9333333333333333481, 0.9375000000000000000, 0.9416666666666666519, 0.9458333333333333037, 0.9499999999999999556, 0.9541666666666667185, 0.9583333333333333703, 0.9625000000000000222, 0.9666666666666666741, 0.9708333333333333259, 0.9749999999999999778, 0.9791666666666666297, 0.9833333333333332815, 0.9875000000000000444, 0.9916666666666666963, 0.9958333333333333481, 1.000000000000000000 ),
 .UNSPECIFIED. ) 
 GEOMETRIC_REPRESENTATION_ITEM ( )  RATIONAL_B_SPLINE_SURFACE ( (
 ( 1.000000000000000000, 0.8660254037844387076, 1.000000000000000000, 0.8660254037844387076, 1.000000000000000000, 0.8660254037844387076, 1.000000000000000000, 0.8660254037844387076, 1.000000000000000000, 0.8660254037844387076, 1.000000000000000000, 0.8660254037844387076, 1.000000000000000000, 0.8660254037844387076, 1.000000000000000000, 0.8660254037844387076, 1.000000000000000000, 0.8660254037844387076, 1.000000000000000000, 0.8660254037844387076, 1.000000000000000000, 0.8660254037844387076, 1.000000000000000000, 0.8660254037844387076, 1.000000000000000000, 0.8660254037844387076, 1.000000000000000000, 0.8660254037844387076, 1.000000000000000000, 0.8660254037844387076, 1.000000000000000000, 0.8660254037844387076, 1.000000000000000000, 0.8660254037844387076, 1.000000000000000000, 0.8660254037844387076, 1.000000000000000000, 0.8660254037844387076, 1.000000000000000000, 0.8660254037844387076, 1.000000000000000000, 0.8660254037844387076, 1.000000000000000000, 0.8660254037844387076, 1.000000000000000000, 0.8660254037844387076, 1.000000000000000000, 0.8660254037844387076, 1.000000000000000000, 0.8660254037844387076, 1.000000000000000000, 0.8660254037844387076, 1.000000000000000000, 0.8660254037844387076, 1.000000000000000000, 0.8660254037844387076, 1.000000000000000000, 0.8660254037844387076, 1.000000000000000000, 0.8660254037844387076, 1.000000000000000000, 0.8660254037844387076, 1.000000000000000000, 0.8660254037844387076, 1.000000000000000000, 0.8660254037844387076, 1.000000000000000000, 0.8660254037844387076, 1.000000000000000000, 0.8660254037844387076, 1.000000000000000000, 0.8660254037844387076, 1.000000000000000000, 0.8660254037844387076, 1.000000000000000000, 0.8660254037844387076, 1.000000000000000000, 0.8660254037844387076, 1.000000000000000000, 0.8660254037844387076, 1.000000000000000000, 0.8660254037844387076, 1.000000000000000000, 0.8660254037844387076, 1.000000000000000000, 0.8660254037844387076, 1.000000000000000000, 0.8660254037844387076, 1.000000000000000000, 0.8660254037844387076, 1.000000000000000000, 0.8660254037844387076, 1.000000000000000000, 0.8660254037844387076, 1.000000000000000000, 0.8660254037844387076, 1.000000000000000000, 0.8660254037844387076, 1.000000000000000000, 0.8660254037844387076, 1.000000000000000000, 0.8660254037844387076, 1.000000000000000000, 0.8660254037844387076, 1.000000000000000000, 0.8660254037844387076, 1.000000000000000000, 0.8660254037844387076, 1.000000000000000000, 0.8660254037844387076, 1.000000000000000000, 0.8660254037844387076, 1.000000000000000000, 0.8660254037844387076, 1.000000000000000000, 0.8660254037844387076, 1.000000000000000000, 0.8660254037844387076, 1.000000000000000000, 0.8660254037844387076, 1.000000000000000000, 0.8660254037844387076, 1.000000000000000000, 0.8660254037844387076, 1.000000000000000000, 0.8660254037844387076, 1.000000000000000000, 0.8660254037844387076, 1.000000000000000000, 0.8660254037844387076, 1.000000000000000000, 0.8660254037844387076, 1.000000000000000000, 0.8660254037844387076, 1.000000000000000000, 0.8660254037844387076, 1.000000000000000000, 0.8660254037844387076, 1.000000000000000000, 0.8660254037844387076, 1.000000000000000000, 0.8660254037844387076, 1.000000000000000000, 0.8660254037844387076, 1.000000000000000000, 0.8660254037844387076, 1.000000000000000000, 0.8660254037844387076, 1.000000000000000000, 0.8660254037844387076, 1.000000000000000000, 0.8660254037844387076, 1.000000000000000000, 0.8660254037844387076, 1.000000000000000000, 0.8660254037844387076, 1.000000000000000000, 0.8660254037844387076, 1.000000000000000000, 0.8660254037844387076, 1.000000000000000000, 0.8660254037844387076, 1.000000000000000000, 0.8660254037844387076, 1.000000000000000000, 0.8660254037844387076, 1.000000000000000000, 0.8660254037844387076, 1.000000000000000000, 0.8660254037844387076, 1.000000000000000000, 0.8660254037844387076, 1.000000000000000000, 0.8660254037844387076, 1.000000000000000000, 0.8660254037844387076, 1.000000000000000000, 0.8660254037844387076, 1.000000000000000000, 0.8660254037844387076, 1.000000000000000000, 0.8660254037844387076, 1.000000000000000000, 0.8660254037844387076, 1.000000000000000000, 0.8660254037844387076, 1.000000000000000000, 0.8660254037844387076, 1.000000000000000000, 0.8660254037844387076, 1.000000000000000000, 0.8660254037844387076, 1.000000000000000000, 0.8660254037844387076, 1.000000000000000000, 0.8660254037844387076, 1.000000000000000000, 0.8660254037844387076, 1.000000000000000000, 0.8660254037844387076, 1.000000000000000000, 0.8660254037844387076, 1.000000000000000000, 0.8660254037844387076, 1.000000000000000000, 0.8660254037844387076, 1.000000000000000000, 0.8660254037844387076, 1.000000000000000000, 0.8660254037844387076, 1.000000000000000000, 0.8660254037844387076, 1.000000000000000000, 0.8660254037844387076, 1.000000000000000000, 0.8660254037844387076, 1.000000000000000000, 0.8660254037844387076, 1.000000000000000000, 0.8660254037844387076, 1.000000000000000000, 0.8660254037844387076, 1.000000000000000000, 0.8660254037844387076, 1.000000000000000000, 0.8660254037844387076, 1.000000000000000000, 0.8660254037844387076, 1.000000000000000000, 0.8660254037844387076, 1.000000000000000000, 0.8660254037844387076, 1.000000000000000000, 0.8660254037844387076, 1.000000000000000000, 0.8660254037844387076, 1.000000000000000000, 0.8660254037844387076, 1.000000000000000000, 0.8660254037844387076, 1.000000000000000000, 0.8660254037844387076, 1.000000000000000000, 0.8660254037844387076, 1.000000000000000000, 0.8660254037844387076, 1.000000000000000000, 0.8660254037844387076, 1.000000000000000000, 0.8660254037844387076, 1.000000000000000000, 0.8660254037844387076, 1.000000000000000000, 0.8660254037844387076, 1.000000000000000000, 0.8660254037844387076, 1.000000000000000000, 0.8660254037844387076, 1.000000000000000000, 0.8660254037844387076, 1.000000000000000000, 0.8660254037844387076, 1.000000000000000000, 0.8660254037844387076, 1.000000000000000000, 0.8660254037844387076, 1.000000000000000000, 0.8660254037844387076, 1.000000000000000000, 0.8660254037844387076, 1.000000000000000000, 0.8660254037844387076, 1.000000000000000000, 0.8660254037844387076, 1.000000000000000000, 0.8660254037844387076, 1.000000000000000000, 0.8660254037844387076, 1.000000000000000000, 0.8660254037844387076, 1.000000000000000000, 0.8660254037844387076, 1.000000000000000000, 0.8660254037844387076, 1.000000000000000000, 0.8660254037844387076, 1.000000000000000000, 0.8660254037844387076, 1.000000000000000000, 0.8660254037844387076, 1.000000000000000000, 0.8660254037844387076, 1.000000000000000000, 0.8660254037844387076, 1.000000000000000000, 0.8660254037844387076, 1.000000000000000000, 0.8660254037844387076, 1.000000000000000000, 0.8660254037844387076, 1.000000000000000000, 0.8660254037844387076, 1.000000000000000000, 0.8660254037844387076, 1.000000000000000000, 0.8660254037844387076, 1.000000000000000000, 0.8660254037844387076, 1.000000000000000000, 0.8660254037844387076, 1.000000000000000000, 0.8660254037844387076, 1.000000000000000000, 0.8660254037844387076, 1.000000000000000000, 0.8660254037844387076, 1.000000000000000000, 0.8660254037844387076, 1.000000000000000000, 0.8660254037844387076, 1.000000000000000000, 0.8660254037844387076, 1.000000000000000000, 0.8660254037844387076, 1.000000000000000000, 0.8660254037844387076, 1.000000000000000000, 0.8660254037844387076, 1.000000000000000000, 0.8660254037844387076, 1.000000000000000000, 0.8660254037844387076, 1.000000000000000000, 0.8660254037844387076, 1.000000000000000000, 0.8660254037844387076, 1.000000000000000000, 0.8660254037844387076, 1.000000000000000000, 0.8660254037844387076, 1.000000000000000000, 0.8660254037844387076, 1.000000000000000000, 0.8660254037844387076, 1.000000000000000000, 0.8660254037844387076, 1.000000000000000000, 0.8660254037844387076, 1.000000000000000000, 0.8660254037844387076, 1.000000000000000000, 0.8660254037844387076, 1.000000000000000000, 0.8660254037844387076, 1.000000000000000000, 0.8660254037844387076, 1.000000000000000000, 0.8660254037844387076, 1.000000000000000000, 0.8660254037844387076, 1.000000000000000000, 0.8660254037844387076, 1.000000000000000000, 0.8660254037844387076, 1.000000000000000000, 0.8660254037844387076, 1.000000000000000000, 0.8660254037844387076, 1.000000000000000000, 0.8660254037844387076, 1.000000000000000000, 0.8660254037844387076, 1.000000000000000000, 0.8660254037844387076, 1.000000000000000000, 0.8660254037844387076, 1.000000000000000000, 0.8660254037844387076, 1.000000000000000000, 0.8660254037844387076, 1.000000000000000000, 0.8660254037844387076, 1.000000000000000000, 0.8660254037844387076, 1.000000000000000000, 0.8660254037844387076, 1.000000000000000000, 0.8660254037844387076, 1.000000000000000000, 0.8660254037844387076, 1.000000000000000000, 0.8660254037844387076, 1.000000000000000000, 0.8660254037844387076, 1.000000000000000000, 0.8660254037844387076, 1.000000000000000000, 0.8660254037844387076, 1.000000000000000000, 0.8660254037844387076, 1.000000000000000000, 0.8660254037844387076, 1.000000000000000000, 0.8660254037844387076, 1.000000000000000000, 0.8660254037844387076, 1.000000000000000000, 0.8660254037844387076, 1.000000000000000000, 0.8660254037844387076, 1.000000000000000000, 0.8660254037844387076, 1.000000000000000000, 0.8660254037844387076, 1.000000000000000000, 0.8660254037844387076, 1.000000000000000000, 0.8660254037844387076, 1.000000000000000000, 0.8660254037844387076, 1.000000000000000000, 0.8660254037844387076, 1.000000000000000000, 0.8660254037844387076, 1.000000000000000000, 0.8660254037844387076, 1.000000000000000000, 0.8660254037844387076, 1.000000000000000000, 0.8660254037844387076, 1.000000000000000000, 0.8660254037844387076, 1.000000000000000000, 0.8660254037844387076, 1.000000000000000000, 0.8660254037844387076, 1.000000000000000000, 0.8660254037844387076, 1.000000000000000000, 0.8660254037844387076, 1.000000000000000000, 0.8660254037844387076, 1.000000000000000000, 0.8660254037844387076, 1.000000000000000000, 0.8660254037844387076, 1.000000000000000000, 0.8660254037844387076, 1.000000000000000000, 0.8660254037844387076, 1.000000000000000000, 0.8660254037844387076, 1.000000000000000000, 0.8660254037844387076, 1.000000000000000000, 0.8660254037844387076, 1.000000000000000000, 0.8660254037844387076, 1.000000000000000000, 0.8660254037844387076, 1.000000000000000000, 0.8660254037844387076, 1.000000000000000000, 0.8660254037844387076, 1.000000000000000000, 0.8660254037844387076, 1.000000000000000000, 0.8660254037844387076, 1.000000000000000000, 0.8660254037844387076, 1.000000000000000000, 0.8660254037844387076, 1.000000000000000000, 0.8660254037844387076, 1.000000000000000000, 0.8660254037844387076, 1.000000000000000000, 0.8660254037844387076, 1.000000000000000000, 0.8660254037844387076, 1.000000000000000000),
 ( 1.000000000000000000, 0.8660254037844387076, 1.000000000000000000, 0.8660254037844387076, 1.000000000000000000, 0.8660254037844387076, 1.000000000000000000, 0.8660254037844387076, 1.000000000000000000, 0.8660254037844387076, 1.000000000000000000, 0.8660254037844387076, 1.000000000000000000, 0.8660254037844387076, 1.000000000000000000, 0.8660254037844387076, 1.000000000000000000, 0.8660254037844387076, 1.000000000000000000, 0.8660254037844387076, 1.000000000000000000, 0.8660254037844387076, 1.000000000000000000, 0.8660254037844387076, 1.000000000000000000, 0.8660254037844387076, 1.000000000000000000, 0.8660254037844387076, 1.000000000000000000, 0.8660254037844387076, 1.000000000000000000, 0.8660254037844387076, 1.000000000000000000, 0.8660254037844387076, 1.000000000000000000, 0.8660254037844387076, 1.000000000000000000, 0.8660254037844387076, 1.000000000000000000, 0.8660254037844387076, 1.000000000000000000, 0.8660254037844387076, 1.000000000000000000, 0.8660254037844387076, 1.000000000000000000, 0.8660254037844387076, 1.000000000000000000, 0.8660254037844387076, 1.000000000000000000, 0.8660254037844387076, 1.000000000000000000, 0.8660254037844387076, 1.000000000000000000, 0.8660254037844387076, 1.000000000000000000, 0.8660254037844387076, 1.000000000000000000, 0.8660254037844387076, 1.000000000000000000, 0.8660254037844387076, 1.000000000000000000, 0.8660254037844387076, 1.000000000000000000, 0.8660254037844387076, 1.000000000000000000, 0.8660254037844387076, 1.000000000000000000, 0.8660254037844387076, 1.000000000000000000, 0.8660254037844387076, 1.000000000000000000, 0.8660254037844387076, 1.000000000000000000, 0.8660254037844387076, 1.000000000000000000, 0.8660254037844387076, 1.000000000000000000, 0.8660254037844387076, 1.000000000000000000, 0.8660254037844387076, 1.000000000000000000, 0.8660254037844387076, 1.000000000000000000, 0.8660254037844387076, 1.000000000000000000, 0.8660254037844387076, 1.000000000000000000, 0.8660254037844387076, 1.000000000000000000, 0.8660254037844387076, 1.000000000000000000, 0.8660254037844387076, 1.000000000000000000, 0.8660254037844387076, 1.000000000000000000, 0.8660254037844387076, 1.000000000000000000, 0.8660254037844387076, 1.000000000000000000, 0.8660254037844387076, 1.000000000000000000, 0.8660254037844387076, 1.000000000000000000, 0.8660254037844387076, 1.000000000000000000, 0.8660254037844387076, 1.000000000000000000, 0.8660254037844387076, 1.000000000000000000, 0.8660254037844387076, 1.000000000000000000, 0.8660254037844387076, 1.000000000000000000, 0.8660254037844387076, 1.000000000000000000, 0.8660254037844387076, 1.000000000000000000, 0.8660254037844387076, 1.000000000000000000, 0.8660254037844387076, 1.000000000000000000, 0.8660254037844387076, 1.000000000000000000, 0.8660254037844387076, 1.000000000000000000, 0.8660254037844387076, 1.000000000000000000, 0.8660254037844387076, 1.000000000000000000, 0.8660254037844387076, 1.000000000000000000, 0.8660254037844387076, 1.000000000000000000, 0.8660254037844387076, 1.000000000000000000, 0.8660254037844387076, 1.000000000000000000, 0.8660254037844387076, 1.000000000000000000, 0.8660254037844387076, 1.000000000000000000, 0.8660254037844387076, 1.000000000000000000, 0.8660254037844387076, 1.000000000000000000, 0.8660254037844387076, 1.000000000000000000, 0.8660254037844387076, 1.000000000000000000, 0.8660254037844387076, 1.000000000000000000, 0.8660254037844387076, 1.000000000000000000, 0.8660254037844387076, 1.000000000000000000, 0.8660254037844387076, 1.000000000000000000, 0.8660254037844387076, 1.000000000000000000, 0.8660254037844387076, 1.000000000000000000, 0.8660254037844387076, 1.000000000000000000, 0.8660254037844387076, 1.000000000000000000, 0.8660254037844387076, 1.000000000000000000, 0.8660254037844387076, 1.000000000000000000, 0.8660254037844387076, 1.000000000000000000, 0.8660254037844387076, 1.000000000000000000, 0.8660254037844387076, 1.000000000000000000, 0.8660254037844387076, 1.000000000000000000, 0.8660254037844387076, 1.000000000000000000, 0.8660254037844387076, 1.000000000000000000, 0.8660254037844387076, 1.000000000000000000, 0.8660254037844387076, 1.000000000000000000, 0.8660254037844387076, 1.000000000000000000, 0.8660254037844387076, 1.000000000000000000, 0.8660254037844387076, 1.000000000000000000, 0.8660254037844387076, 1.000000000000000000, 0.8660254037844387076, 1.000000000000000000, 0.8660254037844387076, 1.000000000000000000, 0.8660254037844387076, 1.000000000000000000, 0.8660254037844387076, 1.000000000000000000, 0.8660254037844387076, 1.000000000000000000, 0.8660254037844387076, 1.000000000000000000, 0.8660254037844387076, 1.000000000000000000, 0.8660254037844387076, 1.000000000000000000, 0.8660254037844387076, 1.000000000000000000, 0.8660254037844387076, 1.000000000000000000, 0.8660254037844387076, 1.000000000000000000, 0.8660254037844387076, 1.000000000000000000, 0.8660254037844387076, 1.000000000000000000, 0.8660254037844387076, 1.000000000000000000, 0.8660254037844387076, 1.000000000000000000, 0.8660254037844387076, 1.000000000000000000, 0.8660254037844387076, 1.000000000000000000, 0.8660254037844387076, 1.000000000000000000, 0.8660254037844387076, 1.000000000000000000, 0.8660254037844387076, 1.000000000000000000, 0.8660254037844387076, 1.000000000000000000, 0.8660254037844387076, 1.000000000000000000, 0.8660254037844387076, 1.000000000000000000, 0.8660254037844387076, 1.000000000000000000, 0.8660254037844387076, 1.000000000000000000, 0.8660254037844387076, 1.000000000000000000, 0.8660254037844387076, 1.000000000000000000, 0.8660254037844387076, 1.000000000000000000, 0.8660254037844387076, 1.000000000000000000, 0.8660254037844387076, 1.000000000000000000, 0.8660254037844387076, 1.000000000000000000, 0.8660254037844387076, 1.000000000000000000, 0.8660254037844387076, 1.000000000000000000, 0.8660254037844387076, 1.000000000000000000, 0.8660254037844387076, 1.000000000000000000, 0.8660254037844387076, 1.000000000000000000, 0.8660254037844387076, 1.000000000000000000, 0.8660254037844387076, 1.000000000000000000, 0.8660254037844387076, 1.000000000000000000, 0.8660254037844387076, 1.000000000000000000, 0.8660254037844387076, 1.000000000000000000, 0.8660254037844387076, 1.000000000000000000, 0.8660254037844387076, 1.000000000000000000, 0.8660254037844387076, 1.000000000000000000, 0.8660254037844387076, 1.000000000000000000, 0.8660254037844387076, 1.000000000000000000, 0.8660254037844387076, 1.000000000000000000, 0.8660254037844387076, 1.000000000000000000, 0.8660254037844387076, 1.000000000000000000, 0.8660254037844387076, 1.000000000000000000, 0.8660254037844387076, 1.000000000000000000, 0.8660254037844387076, 1.000000000000000000, 0.8660254037844387076, 1.000000000000000000, 0.8660254037844387076, 1.000000000000000000, 0.8660254037844387076, 1.000000000000000000, 0.8660254037844387076, 1.000000000000000000, 0.8660254037844387076, 1.000000000000000000, 0.8660254037844387076, 1.000000000000000000, 0.8660254037844387076, 1.000000000000000000, 0.8660254037844387076, 1.000000000000000000, 0.8660254037844387076, 1.000000000000000000, 0.8660254037844387076, 1.000000000000000000, 0.8660254037844387076, 1.000000000000000000, 0.8660254037844387076, 1.000000000000000000, 0.8660254037844387076, 1.000000000000000000, 0.8660254037844387076, 1.000000000000000000, 0.8660254037844387076, 1.000000000000000000, 0.8660254037844387076, 1.000000000000000000, 0.8660254037844387076, 1.000000000000000000, 0.8660254037844387076, 1.000000000000000000, 0.8660254037844387076, 1.000000000000000000, 0.8660254037844387076, 1.000000000000000000, 0.8660254037844387076, 1.000000000000000000, 0.8660254037844387076, 1.000000000000000000, 0.8660254037844387076, 1.000000000000000000, 0.8660254037844387076, 1.000000000000000000, 0.8660254037844387076, 1.000000000000000000, 0.8660254037844387076, 1.000000000000000000, 0.8660254037844387076, 1.000000000000000000, 0.8660254037844387076, 1.000000000000000000, 0.8660254037844387076, 1.000000000000000000, 0.8660254037844387076, 1.000000000000000000, 0.8660254037844387076, 1.000000000000000000, 0.8660254037844387076, 1.000000000000000000, 0.8660254037844387076, 1.000000000000000000, 0.8660254037844387076, 1.000000000000000000, 0.8660254037844387076, 1.000000000000000000, 0.8660254037844387076, 1.000000000000000000, 0.8660254037844387076, 1.000000000000000000, 0.8660254037844387076, 1.000000000000000000, 0.8660254037844387076, 1.000000000000000000, 0.8660254037844387076, 1.000000000000000000, 0.8660254037844387076, 1.000000000000000000, 0.8660254037844387076, 1.000000000000000000, 0.8660254037844387076, 1.000000000000000000, 0.8660254037844387076, 1.000000000000000000, 0.8660254037844387076, 1.000000000000000000, 0.8660254037844387076, 1.000000000000000000, 0.8660254037844387076, 1.000000000000000000, 0.8660254037844387076, 1.000000000000000000, 0.8660254037844387076, 1.000000000000000000, 0.8660254037844387076, 1.000000000000000000, 0.8660254037844387076, 1.000000000000000000, 0.8660254037844387076, 1.000000000000000000, 0.8660254037844387076, 1.000000000000000000, 0.8660254037844387076, 1.000000000000000000, 0.8660254037844387076, 1.000000000000000000, 0.8660254037844387076, 1.000000000000000000, 0.8660254037844387076, 1.000000000000000000, 0.8660254037844387076, 1.000000000000000000, 0.8660254037844387076, 1.000000000000000000, 0.8660254037844387076, 1.000000000000000000, 0.8660254037844387076, 1.000000000000000000, 0.8660254037844387076, 1.000000000000000000, 0.8660254037844387076, 1.000000000000000000, 0.8660254037844387076, 1.000000000000000000, 0.8660254037844387076, 1.000000000000000000, 0.8660254037844387076, 1.000000000000000000, 0.8660254037844387076, 1.000000000000000000, 0.8660254037844387076, 1.000000000000000000, 0.8660254037844387076, 1.000000000000000000, 0.8660254037844387076, 1.000000000000000000, 0.8660254037844387076, 1.000000000000000000, 0.8660254037844387076, 1.000000000000000000, 0.8660254037844387076, 1.000000000000000000, 0.8660254037844387076, 1.000000000000000000, 0.8660254037844387076, 1.000000000000000000, 0.8660254037844387076, 1.000000000000000000, 0.8660254037844387076, 1.000000000000000000, 0.8660254037844387076, 1.000000000000000000, 0.8660254037844387076, 1.000000000000000000, 0.8660254037844387076, 1.000000000000000000, 0.8660254037844387076, 1.000000000000000000, 0.8660254037844387076, 1.000000000000000000, 0.8660254037844387076, 1.000000000000000000, 0.8660254037844387076, 1.000000000000000000, 0.8660254037844387076, 1.000000000000000000, 0.8660254037844387076, 1.000000000000000000, 0.8660254037844387076, 1.000000000000000000, 0.8660254037844387076, 1.000000000000000000, 0.8660254037844387076, 1.000000000000000000, 0.8660254037844387076, 1.000000000000000000, 0.8660254037844387076, 1.000000000000000000, 0.8660254037844387076, 1.000000000000000000) ) ) 
 REPRESENTATION_ITEM ( '' )  SURFACE ( )  );
#113224 = CARTESIAN_POINT ( 'NONE',  ( 0.3818278861203865393, 2.057605126571937060, -0.7983354260262252033 ) ) ;
#113225 = CARTESIAN_POINT ( 'NONE',  ( 2.900009951539525677, -0.7123764238676842941, 2.147366075387107553 ) ) ;
#113226 = CARTESIAN_POINT ( 'NONE',  ( -8.297226821883391779, 11.66355314463053006, 1.082531754730549967 ) ) ;
#113227 = CARTESIAN_POINT ( 'NONE',  ( 2.250024469429566132, 0.8508988043372580634, -1.599271047475413932 ) ) ;
#113228 = EDGE_CURVE ( 'NONE', #73672, #144836, #143899, .T. ) ;
#113229 = CARTESIAN_POINT ( 'NONE',  ( 1.815515222670351259, -1.254507992466627808, -1.447865379607627512 ) ) ;
#113230 = CARTESIAN_POINT ( 'NONE',  ( 3.508316276398337319, 2.070544812355082254, 0.002818362966339192730 ) ) ;
#113231 = CARTESIAN_POINT ( 'NONE',  ( -1.402160292154681736E-14, 1.509375000341420359, -1.575800808251659024 ) ) ;
#113232 = AXIS2_PLACEMENT_3D ( 'NONE', #136307, #37725, #120115 ) ;
#113233 = CARTESIAN_POINT ( 'NONE',  ( 1.323050886902911616, -0.05057411593789931659, 1.970981584096524575 ) ) ;
#113234 = CARTESIAN_POINT ( 'NONE',  ( 6.656866507323381477, -1.487278495449697147, 1.224136630395280534 ) ) ;
#113235 = CARTESIAN_POINT ( 'NONE',  ( 2.729206520949432946, -1.746158693253213379, 0.6715030345267187784 ) ) ;
#113237 = CARTESIAN_POINT ( 'NONE',  ( 5.170590401584001405, 7.751911629329717002, -1.182414590771277085 ) ) ;
#113236 = CARTESIAN_POINT ( 'NONE',  ( 0.9092882892361430214, 1.744143012382966207, -1.511207573902007884 ) ) ;
#113238 = CARTESIAN_POINT ( 'NONE',  ( 2.400643840759258740, 0.4042734059873221986, 1.816444493264858906 ) ) ;
#113239 = CARTESIAN_POINT ( 'NONE',  ( 1.364683531249986537, 2.405208333674752286, -0.7879004041258239610 ) ) ;
#113240 = CARTESIAN_POINT ( 'NONE',  ( 5.125460521936802571, 0.2056810312900352600, -2.052415479088207650 ) ) ;
#113241 = CARTESIAN_POINT ( 'NONE',  ( -5.545448523189368650, 6.428443684264421698, -1.199719254218446718 ) ) ;
#113242 = CARTESIAN_POINT ( 'NONE',  ( 6.238723240582662477, 10.43026088065513513, -0.7998128361456291469 ) ) ;
#113243 = CARTESIAN_POINT ( 'NONE',  ( 10.87634538855762401, 3.956598013261174884, -3.867819554622535350 ) ) ;
#113244 = CARTESIAN_POINT ( 'NONE',  ( 6.563511373971260277, 0.3638278135829931537, -2.074131770586047363 ) ) ;
#113245 = CARTESIAN_POINT ( 'NONE',  ( -1.364683531249997417, 3.321875000341423245, 1.214306433183764966E-14 ) ) ;
#113246 = CARTESIAN_POINT ( 'NONE',  ( 6.345025448074324892, -1.829860219143174982, 1.150409744987097804 ) ) ;
#113247 = CARTESIAN_POINT ( 'NONE',  ( 6.586581121665559202, -1.240835222743674526, 1.594039115436784337 ) ) ;
#113248 = CARTESIAN_POINT ( 'NONE',  ( 1.364683531249986537, -0.6364583329919177856, 0.7879004041258500513 ) ) ;
#113249 = AXIS2_PLACEMENT_3D ( 'NONE', #24845, #5367, #89882 ) ;
#113250 = CARTESIAN_POINT ( 'NONE',  ( -5.802526556968872207, 6.832331073627524454, 1.082531754730548412 ) ) ;
#113251 = EDGE_CURVE ( 'NONE', #97972, #79300, #42713, .T. ) ;
#113254 = CARTESIAN_POINT ( 'NONE',  ( 4.365362273920244007, 6.116008624372160973, 1.443375672974062551 ) ) ;
#113253 = CARTESIAN_POINT ( 'NONE',  ( 6.925078400183578786, 2.094238355957972253, 2.065574651578235610 ) ) ;
#113252 = CARTESIAN_POINT ( 'NONE',  ( 6.723917837734620484, 6.809268663637336516, 0.000000000000000000 ) ) ;
#113255 = CARTESIAN_POINT ( 'NONE',  ( -5.306037014901836990, 7.283738832175834510, 1.599625672291263179 ) ) ;
#113256 = CARTESIAN_POINT ( 'NONE',  ( 4.839077477813122918, -1.706110771555340744, -1.074664961451990308 ) ) ;
#113257 = CARTESIAN_POINT ( 'NONE',  ( -8.365544474831901667, 9.718555627847388578, 1.199719254218462483 ) ) ;
#113259 = CARTESIAN_POINT ( 'NONE',  ( -6.522881301506166629, 9.663759714182251770, 1.082531754730549967 ) ) ;
#113258 = CARTESIAN_POINT ( 'NONE',  ( -4.627410500965859264, 4.293067094081919777, 0.7998128361456341429 ) ) ;
#113260 = CARTESIAN_POINT ( 'NONE',  ( -1.201851678989727383E-14, 5.696875000341416140, -1.575800808251660134 ) ) ;
#113262 = CARTESIAN_POINT ( 'NONE',  ( 0.6823417656249969321, 9.276041667008065872, -1.181850606188757036 ) ) ;
#113261 = CARTESIAN_POINT ( 'NONE',  ( 5.506754051192107369, 1.639644015412666800, -1.408845030788405506 ) ) ;
#113263 = CARTESIAN_POINT ( 'NONE',  ( -11.84101807917483740, 13.61021500260875428, 1.444039656437077879 ) ) ;
#113264 = CARTESIAN_POINT ( 'NONE',  ( -11.95450533369660917, 8.100191672919370589, 0.5443015705738691867 ) ) ;
#113265 = B_SPLINE_CURVE_WITH_KNOTS ( 'NONE', 3,
 ( #54255, #106252, #172276, #5460 ),
 .UNSPECIFIED., .F., .F.,
 ( 4, 4 ),
 ( 0.8646637866085976620, 1.000000000000000000 ),
 .UNSPECIFIED. ) ;
#113267 = CARTESIAN_POINT ( 'NONE',  ( 5.519157712072518152, -1.821736412749059397, 0.8647389720048551665 ) ) ;
#113266 = CARTESIAN_POINT ( 'NONE',  ( -5.490689023410187275, 8.389259046411751797, 1.082531754730548412 ) ) ;
#113268 = CARTESIAN_POINT ( 'NONE',  ( 1.364683531249988757, -0.8031249996585804185, 0.000000000000000000 ) ) ;
#113269 = CARTESIAN_POINT ( 'NONE',  ( 1.927930615940620873, 0.9947386370207593753, -1.408936266059911624 ) ) ;
#113270 = CARTESIAN_POINT ( 'NONE',  ( 4.050854035433010480, 7.948023151305657841, 0.000000000000000000 ) ) ;
#113272 = CARTESIAN_POINT ( 'NONE',  ( 8.018721507839716267, 8.319872945426633137, -0.7998128361456341429 ) ) ;
#113271 = CARTESIAN_POINT ( 'NONE',  ( 7.456621297836082185, 7.801739057004660971, 0.7216878364870317197 ) ) ;
#113273 = CARTESIAN_POINT ( 'NONE',  ( -10.79669699716785480, 6.389081389852535153, -5.150160299006881992 ) ) ;
#113274 = CARTESIAN_POINT ( 'NONE',  ( 6.819622122755134797, -1.814287395386984691, 0.4549875680220638596 ) ) ;
#113275 = CARTESIAN_POINT ( 'NONE',  ( 0.4693897461072121802, -1.701762708260607715, -1.075143862628368474 ) ) ;
#113276 = FACE_BOUND ( 'NONE', #1571, .T. ) ;
#113277 = CARTESIAN_POINT ( 'NONE',  ( 2.837189949676882428, 0.2689455771197127310, 2.190246129917215789 ) ) ;
#113278 = CARTESIAN_POINT ( 'NONE',  ( 5.243124948155760912, -0.2588677773407067617, -2.155501751117256948 ) ) ;
#113279 = VERTEX_POINT ( 'NONE', #174846 ) ;
#113280 = CARTESIAN_POINT ( 'NONE',  ( 5.273195401072370281, 5.116759154198018855, -0.7998128361456481317 ) ) ;
#113281 = CARTESIAN_POINT ( 'NONE',  ( 8.717529583462638954, 12.15390636647303069, 1.082531754730546636 ) ) ;
#113283 = CARTESIAN_POINT ( 'NONE',  ( 1.687125285987755019, 1.678019391100945779, 1.117813378161469418 ) ) ;
#113282 = CARTESIAN_POINT ( 'NONE',  ( 3.615986862044855421, -0.6139777315949943581, 2.029667854546577388 ) ) ;
#113285 = ORIENTED_EDGE ( 'NONE', *, *, #168663, .F. ) ;
#113284 = CARTESIAN_POINT ( 'NONE',  ( 2.601584773815317497, 1.283861566028346779, 1.278364218381728090 ) ) ;
#113286 = CARTESIAN_POINT ( 'NONE',  ( 7.388267364804250725, 7.584343111885245570, -0.7998128361456341429 ) ) ;
#113287 = CARTESIAN_POINT ( 'NONE',  ( 6.474182045725470402, 7.511966127223233869, -1.199719254218446718 ) ) ;
#113289 = CARTESIAN_POINT ( 'NONE',  ( 1.305720528479116682, -1.067273574023764438, -1.590657944389769707 ) ) ;
#113288 = CARTESIAN_POINT ( 'NONE',  ( -4.416205349749324327, 6.175325546172740765, 1.599625672291267398 ) ) ;
#113290 = CARTESIAN_POINT ( 'NONE',  ( 0.07479286986305370977, 0.004866263145587856019, -1.855573292446038414 ) ) ;
#113291 = CARTESIAN_POINT ( 'NONE',  ( -1.119339255005453736E-13, 13.28612805825129151, 1.454322456996997470 ) ) ;
#113292 = CARTESIAN_POINT ( 'NONE',  ( 4.161989969270883272, 7.799479364217271282, 0.7216878364870317197 ) ) ;
#113293 = ADVANCED_FACE ( 'NONE', ( #142357 ), #26423, .T. ) ;
#113294 = CARTESIAN_POINT ( 'NONE',  ( -0.6823417656250003738, 0.03020833367475134201, -1.181850606188749264 ) ) ;
#113295 = DIRECTION ( 'NONE',  ( -2.345077562848777574E-16, -0.000000000000000000, -1.000000000000000000 ) ) ;
#113296 = CARTESIAN_POINT ( 'NONE',  ( -9.484092147959342967, 11.02352791316275216, 1.199719254218462483 ) ) ;
#113297 = CARTESIAN_POINT ( 'NONE',  ( 4.979442225389012933, 2.018306902694905425, -0.7746836383674888804 ) ) ;
#113298 = ADVANCED_FACE ( 'NONE', ( #6947 ), #106669, .T. ) ;
#113299 = CARTESIAN_POINT ( 'NONE',  ( -5.072158865288277418, 7.010880990960010273, 1.443375672974058777 ) ) ;
#113300 = CARTESIAN_POINT ( 'NONE',  ( 5.614485009834906393, 6.683225611963085733, -1.082531754730548412 ) ) ;
#113301 = CARTESIAN_POINT ( 'NONE',  ( 1.389100911873580646, -2.015333191458138273, -0.6601287711371638389 ) ) ;
#113303 = CARTESIAN_POINT ( 'NONE',  ( -11.30309668167796922, 5.150585336095397260, -5.742054036728555744 ) ) ;
#113302 = CARTESIAN_POINT ( 'NONE',  ( -0.1298852118744100725, 6.948705093303869873, -2.321530996463050389 ) ) ;
#113304 = CARTESIAN_POINT ( 'NONE',  ( 3.831288253049653481, -1.822718488796180925, 0.7514253593702052703 ) ) ;
#113305 = CARTESIAN_POINT ( 'NONE',  ( 5.590081826628392925, 1.144292256163012667, 1.532101299821154949 ) ) ;
#113306 = ORIENTED_EDGE ( 'NONE', *, *, #157961, .T. ) ;
#113307 = CIRCLE ( 'NONE', #182328, 0.4999999999999995559 ) ;
#113308 = CARTESIAN_POINT ( 'NONE',  ( -1.499999999999997780, 4.650000000000022560, 1.214306433183765124E-14 ) ) ;
#113309 = CARTESIAN_POINT ( 'NONE',  ( 0.1333692844072559280, 0.001398348041498076455, -2.053671342968105051 ) ) ;
#113310 = CARTESIAN_POINT ( 'NONE',  ( 2.361185668158103379, 1.904436331314839137, -0.3790439726399745246 ) ) ;
#113311 = VERTEX_POINT ( 'NONE', #105574 ) ;
#113312 = CARTESIAN_POINT ( 'NONE',  ( -4.267173273579143000, 7.298649460985302539, -0.9221393241729136658 ) ) ;
#113314 = CARTESIAN_POINT ( 'NONE',  ( 1.833030277982334422, 2.531131934864056632, -2.500000000000000444 ) ) ;
#113313 = CARTESIAN_POINT ( 'NONE',  ( -5.804299160426224624, 9.785783097223662352, -0.7216878364870338292 ) ) ;
#113316 = CARTESIAN_POINT ( 'NONE',  ( 6.331821432781979730, 7.345878745455822312, -1.199719254218445830 ) ) ;
#113315 = CARTESIAN_POINT ( 'NONE',  ( 2.959016038526005143, 0.3060221511422682727, -2.067984839732572855 ) ) ;
#113317 = CARTESIAN_POINT ( 'NONE',  ( 5.858531774436539052, 6.007577623030311287, 0.000000000000000000 ) ) ;
#113319 = ORIENTED_EDGE ( 'NONE', *, *, #77746, .T. ) ;
#113318 = CARTESIAN_POINT ( 'NONE',  ( 5.988906256519173077, -1.817303134770717588, -0.5954205699960082310 ) ) ;
#113320 = CARTESIAN_POINT ( 'NONE',  ( 4.600333186373093852, -2.206333364838486411, -0.05604163552313382035 ) ) ;
#113321 = CARTESIAN_POINT ( 'NONE',  ( 2.661379449941482012, -1.919611247835448342, -1.088434722066232485 ) ) ;
#113322 = CARTESIAN_POINT ( 'NONE',  ( 7.934546212495622086, 10.28005655271014795, -1.599625672291262513 ) ) ;
#113323 = CARTESIAN_POINT ( 'NONE',  ( -15.75000000000000000, 10.19999999999998153, 1.799999999999999600 ) ) ;
#113324 = CARTESIAN_POINT ( 'NONE',  ( 1.611815888142430264, -0.6431676737995162263, 1.801018335096972400 ) ) ;
#113325 = CARTESIAN_POINT ( 'NONE',  ( -8.917737905728749581, 3.447199233515649386, -8.029567276306266876 ) ) ;
#113326 = CARTESIAN_POINT ( 'NONE',  ( 10.01963921569910632, 11.64833282552586091, 1.199719254218450271 ) ) ;
#113327 = CARTESIAN_POINT ( 'NONE',  ( 4.439934286204096914, 1.349936692791346093, 1.569845735447549906 ) ) ;
#113329 = CARTESIAN_POINT ( 'NONE',  ( 2.061604318190731533, 0.3698614785779800185, -2.129673623264888960 ) ) ;
#113328 = CARTESIAN_POINT ( 'NONE',  ( -4.288456660624211381, 3.897620947016656956, 1.214306433183764966E-14 ) ) ;
#113330 = CARTESIAN_POINT ( 'NONE',  ( 4.212563348414651188, 2.004022095860341413, 0.8874167208733558798 ) ) ;
#113331 = CARTESIAN_POINT ( 'NONE',  ( 9.642873567817520808, 12.27310513391906532, 1.599625672291279388 ) ) ;
#113332 = CARTESIAN_POINT ( 'NONE',  ( 0.000000000000000000, 3.400000000000000355, 0.000000000000000000 ) ) ;
#113333 = CARTESIAN_POINT ( 'NONE',  ( -7.789436271558764169, 15.44814005990453865, 9.080438957707684722 ) ) ;
#113334 = CARTESIAN_POINT ( 'NONE',  ( 4.064412189046650248, 7.963840997188264659, 0.7998128361456271485 ) ) ;
#113335 = CARTESIAN_POINT ( 'NONE',  ( 0.6823417656249934904, 14.00520833367473195, 1.181850606188764807 ) ) ;
#113336 = CARTESIAN_POINT ( 'NONE',  ( -5.652823702255029836, 5.559658838911111900, -0.7998128361456362523 ) ) ;
#113337 = PRODUCT_DEFINITION_CONTEXT ( 'detailed design', #169602, 'design' ) ;
#113338 = CARTESIAN_POINT ( 'NONE',  ( 0.1236729436712938751, 0.3474707636354073537, 1.986100063511665237 ) ) ;
#113339 = CARTESIAN_POINT ( 'NONE',  ( -9.015808963407680565, 9.620791333504852716, 1.040834085586084257E-14 ) ) ;
#113340 = CIRCLE ( 'NONE', #206784, 6.449999999999992184 ) ;
#113341 = CARTESIAN_POINT ( 'NONE',  ( 4.768459183169745152, -0.8803848081004579385, -1.873848736155204087 ) ) ;
#113342 = CARTESIAN_POINT ( 'NONE',  ( 3.158729500758109765, -1.458545141725621219, 1.258684350631077642 ) ) ;
#113343 = CARTESIAN_POINT ( 'NONE',  ( 5.607064690329227830, -0.05131010805739347896, 2.116756054987908531 ) ) ;
#113344 = CARTESIAN_POINT ( 'NONE',  ( 6.322179702674084467, 6.270297829408224111, 1.040834085586084257E-14 ) ) ;
#113345 = CARTESIAN_POINT ( 'NONE',  ( 4.690609020473775814, 8.361801240329816309, 0.7176157125430505657 ) ) ;
#113346 = CARTESIAN_POINT ( 'NONE',  ( 4.117982337901913148, 1.955079553045156127, -0.2365992483164043592 ) ) ;
#113347 = CARTESIAN_POINT ( 'NONE',  ( 6.421853422025334268, 1.325270252340422061, -1.870170258788282247 ) ) ;
#113348 = CARTESIAN_POINT ( 'NONE',  ( 4.301258635363705451, 1.467727663998198206, 1.085573330547324744 ) ) ;
#113349 = CARTESIAN_POINT ( 'NONE',  ( 7.363486825997814123, 7.763358516518489516, 0.000000000000000000 ) ) ;
#113350 = CARTESIAN_POINT ( 'NONE',  ( 3.836594282542909795, 6.459481848733281240, 1.082531754730558626 ) ) ;
#113351 = CARTESIAN_POINT ( 'NONE',  ( -7.119966945832006289, 8.335658187339330283, 1.199719254218452047 ) ) ;
#113352 = CARTESIAN_POINT ( 'NONE',  ( 4.206772801990143584, 8.129928378955675328, 0.7998128361456271485 ) ) ;
#113353 = ORIENTED_EDGE ( 'NONE', *, *, #24957, .T. ) ;
#113355 = CARTESIAN_POINT ( 'NONE',  ( 4.834244255588106221, -1.080646305101562232, -1.698427166264226518 ) ) ;
#113354 = CARTESIAN_POINT ( 'NONE',  ( 1.294213439101927321, 1.504999338701202394, -1.060447551955064016 ) ) ;
#113356 = CARTESIAN_POINT ( 'NONE',  ( 6.047535252586548893, -1.628406021067085874, 1.622660289872903006 ) ) ;
#113357 = CARTESIAN_POINT ( 'NONE',  ( 5.576992410575341452, 1.811172876804711507, 0.7542287045681006497 ) ) ;
#113358 = CARTESIAN_POINT ( 'NONE',  ( -7.542413527904030524, 7.693903958843159252, 1.040834085586084257E-14 ) ) ;
#113359 = CARTESIAN_POINT ( 'NONE',  ( -4.843287188579803448, 6.673587691474970107, -1.599625672291256295 ) ) ;
#113360 = CARTESIAN_POINT ( 'NONE',  ( -9.796090618744084821, 3.974415841077576950, -6.102288299938490646 ) ) ;
#113361 = CARTESIAN_POINT ( 'NONE',  ( -4.423703259808839938, 8.383013913077441259, 0.7998128361456352531 ) ) ;
#113363 = CARTESIAN_POINT ( 'NONE',  ( 0.4439547499465161251, 1.865322535695708606, 0.1421067652795371117 ) ) ;
#113362 = CARTESIAN_POINT ( 'NONE',  ( 1.382492367555522295, -0.3100735531622924035, -2.067509394536557021 ) ) ;
#113364 = CARTESIAN_POINT ( 'NONE',  ( -0.6311622855796755749, 3.299999999999955858, -0.4000000000000444311 ) ) ;
#113365 = CARTESIAN_POINT ( 'NONE',  ( 5.683525053321154985, -0.8713906080477454852, 1.735537339962249792 ) ) ;
#113366 = CARTESIAN_POINT ( 'NONE',  ( -0.2104748580754408904, 1.337026610731705700, -2.356057411969681326 ) ) ;
#113367 = CARTESIAN_POINT ( 'NONE',  ( 0.3798832434597871344, -0.2101876225509922147, -1.727645577085941353 ) ) ;
#113368 = CARTESIAN_POINT ( 'NONE',  ( 5.961834861707224320, 7.978559976790334574, -1.599625672291262513 ) ) ;
#113369 = FACE_OUTER_BOUND ( 'NONE', #33781, .T. ) ;
#113370 = CARTESIAN_POINT ( 'NONE',  ( 1.418105696869888410, 1.160834107949513472, -1.275986549933407543 ) ) ;
#113371 = CARTESIAN_POINT ( 'NONE',  ( 1.224469250947546328, 2.113408192816915943, 0.5798510048089372537 ) ) ;
#113372 = CARTESIAN_POINT ( 'NONE',  ( 3.739080281021701868, 0.3231575147602770426, 2.182976880621155136 ) ) ;
#113373 = DIRECTION ( 'NONE',  ( -1.000000000000000000, 0.000000000000000000, 0.000000000000000000 ) ) ;
#113374 = AXIS2_PLACEMENT_3D ( 'NONE', #63821, #128904, #129979 ) ;
#113375 = CARTESIAN_POINT ( 'NONE',  ( 1.428853742479018862, -1.379120938454091227, 1.676725645940212894 ) ) ;
#113376 = CARTESIAN_POINT ( 'NONE',  ( 1.177073619093308432, 3.131928502340592058, -0.7749999999999910294 ) ) ;
#113377 = CARTESIAN_POINT ( 'NONE',  ( 1.727892286414894674, 0.8051050731917328562, -1.958494560251317740 ) ) ;
#113378 = CARTESIAN_POINT ( 'NONE',  ( 6.639320575229263888, 6.039109382135522175, 2.391643382086404923 ) ) ;
#113379 = VERTEX_POINT ( 'NONE', #171606 ) ;
#113381 = CARTESIAN_POINT ( 'NONE',  ( -0.6823417656250246877, 0.6135416670080897639, 1.181850606188755259 ) ) ;
#113380 = CARTESIAN_POINT ( 'NONE',  ( 2.683473709500754367, 1.623236604230539282, 1.618912294457574674 ) ) ;
#113382 = CARTESIAN_POINT ( 'NONE',  ( 3.994848817520957773, 7.812407387083109001, 1.040834085586084257E-14 ) ) ;
#113383 = CARTESIAN_POINT ( 'NONE',  ( 4.547657996348432263, -2.031006315926532135, 0.8999586162586125093 ) ) ;
#113384 = CARTESIAN_POINT ( 'NONE',  ( -6.887178846062116833, 9.058127958537705027, -1.443375672974059665 ) ) ;
#113385 = CARTESIAN_POINT ( 'NONE',  ( 4.365362273920238678, 7.076377838673507448, 1.082531754730558626 ) ) ;
#113386 = CARTESIAN_POINT ( 'NONE',  ( -7.985389288324710400, 8.418635045908049008, -0.7216878364870267237 ) ) ;
#113387 = CARTESIAN_POINT ( 'NONE',  ( 3.594320121398666856, 7.207474218358159490, -1.734723475976807094E-15 ) ) ;
#113388 = EDGE_LOOP ( 'NONE', ( #74240, #200269 ) ) ;
#113389 = CARTESIAN_POINT ( 'NONE',  ( 2.602185585689294367, -0.1948409242511044692, 2.006959980107574371 ) ) ;
#113391 = CARTESIAN_POINT ( 'NONE',  ( 1.955997896808071568, -0.6987562721488985717, 1.940702610317937671 ) ) ;
#113390 = CARTESIAN_POINT ( 'NONE',  ( 7.124973419181436007, 8.271222729588529887, -1.199719254218446718 ) ) ;
#113392 = CARTESIAN_POINT ( 'NONE',  ( -11.91826848330638455, 13.50729645956978331, 1.400000080589927753 ) ) ;
#113393 = CARTESIAN_POINT ( 'NONE',  ( 6.197485614778188712, 6.403023770095574108, -0.7216878364870458196 ) ) ;
#113394 = ORIENTED_EDGE ( 'NONE', *, *, #62155, .T. ) ;
#113395 = CARTESIAN_POINT ( 'NONE',  ( -7.728718841140393536, -6.124285369217662200, -7.728718841140358897 ) ) ;
#113396 = CARTESIAN_POINT ( 'NONE',  ( -1.201851678989727383E-14, 5.446875000341422357, -1.575800808251660134 ) ) ;
#113397 = CARTESIAN_POINT ( 'NONE',  ( 4.716832014018703667, -0.1092502567305031480, 2.188841582221649595 ) ) ;
#113398 = CARTESIAN_POINT ( 'NONE',  ( 2.004529941291322448, -1.955172360644286789, 0.4926429297785542283 ) ) ;
#113399 = CARTESIAN_POINT ( 'NONE',  ( 2.524749765808989466, -1.717266272480859834, 0.6646640004178904215 ) ) ;
#113400 = AXIS2_PLACEMENT_3D ( 'NONE', #59537, #9723, #146158 ) ;
#113401 = EDGE_CURVE ( 'NONE', #1642, #27161, #97919, .T. ) ;
#113402 = CARTESIAN_POINT ( 'NONE',  ( 6.448874621594486989, 10.67543749183559143, 0.7998128361456462443 ) ) ;
#113403 =( NAMED_UNIT ( * ) SI_UNIT ( $, .STERADIAN. ) SOLID_ANGLE_UNIT ( ) );
#113404 = CARTESIAN_POINT ( 'NONE',  ( 4.946237996787820279, 1.820793779319082706, 0.1331645236858983172 ) ) ;
#113405 = CARTESIAN_POINT ( 'NONE',  ( 5.555314621531947772, -1.277044735018734833, 1.560499014526220307 ) ) ;
#113406 = CARTESIAN_POINT ( 'NONE',  ( -8.877891658850122880, 9.251961778280284321, 0.7998128361456462443 ) ) ;
#113408 = CARTESIAN_POINT ( 'NONE',  ( -6.981522756394290319, 7.109807735406931783, 0.7998128361456341429 ) ) ;
#113407 = CARTESIAN_POINT ( 'NONE',  ( 5.489262863951156923, 1.998152018339900415, -1.061309651537506227 ) ) ;
#113409 = CARTESIAN_POINT ( 'NONE',  ( 0.6804681372492230595, -1.168251705716750299, 1.752132397912719242 ) ) ;
#113410 = CARTESIAN_POINT ( 'NONE',  ( -7.262327558775498737, 8.501745569106741840, 1.199719254218452047 ) ) ;
#113411 = CARTESIAN_POINT ( 'NONE',  ( 8.041957671200231417, 12.53403438304231976, 1.040834085586084257E-14 ) ) ;
#113412 = FILL_AREA_STYLE ('',( #64587 ) ) ;
#113413 = CARTESIAN_POINT ( 'NONE',  ( 8.378074386687000441, 10.50815134976859255, 15.76159487570644124 ) ) ;
#113414 = CARTESIAN_POINT ( 'NONE',  ( -8.365544474831901667, 9.718555627847388578, 1.199719254218462483 ) ) ;
#113415 = CARTESIAN_POINT ( 'NONE',  ( 11.07123322939518673, 11.29999999999999716, 0.8055995038523129370 ) ) ;
#113416 = CARTESIAN_POINT ( 'NONE',  ( 5.826972158823246595, 10.02016096192762085, -0.7998128361456481317 ) ) ;
#113417 = CARTESIAN_POINT ( 'NONE',  ( 4.778452461313970723, 6.762070782353614362, -1.245597109521460633 ) ) ;
#113418 = CARTESIAN_POINT ( 'NONE',  ( -9.381879110976678149, 11.00824238663667565, 1.082531754730558626 ) ) ;
#113420 = CARTESIAN_POINT ( 'NONE',  ( 2.971146563671855034, -1.679565462486251048, 1.453923022682623856 ) ) ;
#113419 = CARTESIAN_POINT ( 'NONE',  ( 1.723052270212792836, 1.567896913533245229, -1.427966198690698851 ) ) ;
#113421 = CARTESIAN_POINT ( 'NONE',  ( 0.07999999999999327094, -9.999999999999994671, 10.91970695577496286 ) ) ;
#113422 = CARTESIAN_POINT ( 'NONE',  ( -4.586401103172829785, 8.572828063668767484, 0.7998128361456281477 ) ) ;
#113423 = CARTESIAN_POINT ( 'NONE',  ( 5.717788096661236885, 7.693838750903348789, 1.599625672291267398 ) ) ;
#113424 = CARTESIAN_POINT ( 'NONE',  ( 2.805073129645048624, -1.632656238785214597, 1.087510969322850629 ) ) ;
#113425 = CARTESIAN_POINT ( 'NONE',  ( 6.159481859310094620, 6.080483678816896109, 1.040834085586084257E-14 ) ) ;
#113426 = CARTESIAN_POINT ( 'NONE',  ( -4.138143308069708759, 7.456237844118314584, -0.6866288536411498944 ) ) ;
#113427 = CARTESIAN_POINT ( 'NONE',  ( 2.361091307074211887, 5.906356958228550447, 0.7998128361456462443 ) ) ;
#113428 = CARTESIAN_POINT ( 'NONE',  ( -5.329763783947941036, 5.390681634126922361, 0.000000000000000000 ) ) ;
#113429 = CARTESIAN_POINT ( 'NONE',  ( -6.236387472606145010, 9.259240570473746601, -1.082531754730538864 ) ) ;
#113430 = CARTESIAN_POINT ( 'NONE',  ( 1.969135536805465492, -1.636093909763213228, 1.349083368969570262 ) ) ;
#113431 = CARTESIAN_POINT ( 'NONE',  ( -4.111865726694519552, 8.019203457777400956, 0.000000000000000000 ) ) ;
#113432 = CARTESIAN_POINT ( 'NONE',  ( 4.891577088959510711, 1.599438101461609918, 1.454397306527709155 ) ) ;
#113433 = CARTESIAN_POINT ( 'NONE',  ( 2.788419073117563762, 1.577926727847511312, -0.9486480243563880643 ) ) ;
#113434 = CARTESIAN_POINT ( 'NONE',  ( -4.836546220603817225, 6.746162335969787094, 1.249072166269946216 ) ) ;
#113435 = CARTESIAN_POINT ( 'NONE',  ( -0.6823417656250003738, 0.03020833367475134201, -1.181850606188749264 ) ) ;
#113436 = CARTESIAN_POINT ( 'NONE',  ( 5.472502228039195060, -0.04848951148075366507, -1.739831344048385908 ) ) ;
#113437 = CARTESIAN_POINT ( 'NONE',  ( 1.479373551132449505, 3.300000000000025135, 0.2478989637125245671 ) ) ;
#113438 = CARTESIAN_POINT ( 'NONE',  ( 5.517805331081858888, 5.539787095791365523, 1.040834085586084257E-14 ) ) ;
#113439 = CARTESIAN_POINT ( 'NONE',  ( -1.192622389734054877E-15, -8.605993949662202880, 10.72098668450195369 ) ) ;
#113440 = CARTESIAN_POINT ( 'NONE',  ( 2.606508400632711719, -0.8264410288459265175, -1.997682696722333784 ) ) ;
#113441 = EDGE_CURVE ( 'NONE', #148246, #163352, #16555, .T. ) ;
#113442 = CARTESIAN_POINT ( 'NONE',  ( 4.446638634790680555, 1.314796391739967207, 1.528506369862133285 ) ) ;
#113443 = CARTESIAN_POINT ( 'NONE',  ( -9.124274191872640216, 10.70770331434866485, -1.082531754730537976 ) ) ;
#113444 = CARTESIAN_POINT ( 'NONE',  ( 1.991316529349271836, 1.880942973025516940, -1.065213018539921563 ) ) ;
#113445 = CARTESIAN_POINT ( 'NONE',  ( 3.040257615459122320, 1.956033444698499268, 0.2450028794991568337 ) ) ;
#113446 = CARTESIAN_POINT ( 'NONE',  ( -0.9311234436981496998, -2.684380368602567568, 3.475000000000000977 ) ) ;
#113447 = B_SPLINE_CURVE_WITH_KNOTS ( 'NONE', 3,
 ( #166255, #17844, #133795, #4777, #171583, #37316, #70855, #103391, #201918, #36238, #188898, #136969, #102316 ),
 .UNSPECIFIED., .F., .F.,
 ( 4, 3, 3, 3, 4 ),
 ( -1.794875636224401991E-06, 0.000000000000000000, 4.600594404842603212E-05, 8.489997069011644972E-05, 0.0001121994717586669222 ),
 .UNSPECIFIED. ) ;
#113448 = CARTESIAN_POINT ( 'NONE',  ( 4.862805241732807815, 0.1868221656222105176, -1.933040885264789122 ) ) ;
#113451 = ORIENTED_EDGE ( 'NONE', *, *, #22766, .T. ) ;
#113450 = CARTESIAN_POINT ( 'NONE',  ( 8.064677165291197269, -5.223431457505083308, -7.446209719563361418 ) ) ;
#113449 = CARTESIAN_POINT ( 'NONE',  ( -7.809133291347029271, 12.05447990663947877, 0.000000000000000000 ) ) ;
#113452 = CARTESIAN_POINT ( 'NONE',  ( -5.935437387732586778, 10.14670372898850381, -0.7998128361456362523 ) ) ;
#113453 = CARTESIAN_POINT ( 'NONE',  ( 3.237364818613055473, 6.998952398349030268, -1.734723475976807094E-15 ) ) ;
#113455 = EDGE_LOOP ( 'NONE', ( #179397, #206601, #146458 ) ) ;
#113454 = CARTESIAN_POINT ( 'NONE',  ( -4.294900800479008574, 8.232744377192641849, 0.000000000000000000 ) ) ;
#113456 = CARTESIAN_POINT ( 'NONE',  ( -8.636180661780660017, 11.09863007687603087, -1.443375672974058777 ) ) ;
#113457 = CARTESIAN_POINT ( 'NONE',  ( 1.097021799178355739, -0.5375665728563282508, -2.140183485690804410 ) ) ;
#113458 = CARTESIAN_POINT ( 'NONE',  ( -3.285556943749998737, -2.180208332855376518, 1.896917185911908499 ) ) ;
#113459 = CARTESIAN_POINT ( 'NONE',  ( 4.715648799723409113, 0.4337510919622395988, -1.913030730064477769 ) ) ;
#113460 = CARTESIAN_POINT ( 'NONE',  ( -1.364683531250012516, 4.801041667008083991, -0.7879004041258300672 ) ) ;
#113461 = CARTESIAN_POINT ( 'NONE',  ( -1.201851678989727383E-14, 2.743750000682820378, 1.732050807568877637 ) ) ;
#113462 = CARTESIAN_POINT ( 'NONE',  ( 5.456969279648811622, 6.453098228331718644, -1.278498092073777626 ) ) ;
#113464 = CARTESIAN_POINT ( 'NONE',  ( -6.240830780992103755, 6.175390754112560110, 1.040834085586084257E-14 ) ) ;
#113463 = CARTESIAN_POINT ( 'NONE',  ( 9.333041836227053523, 4.446947634372834912, 7.472413793103392265 ) ) ;
#113465 = CARTESIAN_POINT ( 'NONE',  ( 3.749809578975582536, 0.6641696684822319119, 1.717346325712478583 ) ) ;
#113466 = EDGE_LOOP ( 'NONE', ( #93790, #72997, #162677, #150802, #89287, #43957, #109576, #195157 ) ) ;
#113467 = CARTESIAN_POINT ( 'NONE',  ( -1.225000000000050271, 2.583333334016200578, 0.7072540797572757221 ) ) ;
#113468 = CARTESIAN_POINT ( 'NONE',  ( -8.128276786592724790, 9.441743324901704426, -1.199719254218446718 ) ) ;
#113469 = CARTESIAN_POINT ( 'NONE',  ( 0.000000000000000000, 1.000000000000000888, 0.000000000000000000 ) ) ;
#113470 = CARTESIAN_POINT ( 'NONE',  ( 5.502226937873657242, -0.9515977829631333540, 1.895136135177949877 ) ) ;
#113471 = CARTESIAN_POINT ( 'NONE',  ( 8.836922018362429299, 13.05625752930196448, 8.050375269625257957 ) ) ;
#113472 = CARTESIAN_POINT ( 'NONE',  ( 6.634017235788401301, 6.634108284708264414, 0.7998128361456341429 ) ) ;
#113473 = CARTESIAN_POINT ( 'NONE',  ( 6.327427223165448922, -1.941958050844143413, 0.6900897555163245656 ) ) ;
#113476 = CARTESIAN_POINT ( 'NONE',  ( 4.001369526190221571, -1.836035423186295201, 0.1395379388276704880 ) ) ;
#113475 = CARTESIAN_POINT ( 'NONE',  ( 1.539268068193447858, 1.721329529071988107, -0.7080023387807417024 ) ) ;
#113474 = CARTESIAN_POINT ( 'NONE',  ( -9.695354081530210166, -7.357813805514500594, 1.138412281109779656E-15 ) ) ;
#113477 = CARTESIAN_POINT ( 'NONE',  ( 8.067265095331215718, 9.370563018429956870, 1.199719254218462483 ) ) ;
#113478 = CARTESIAN_POINT ( 'NONE',  ( 9.093502852636627054, 1.000000000000000888, 7.666967846417570343 ) ) ;
#113479 = CARTESIAN_POINT ( 'NONE',  ( -7.781453819600577582, 8.043060642480948985, 0.000000000000000000 ) ) ;
#113480 = DIRECTION ( 'NONE',  ( 1.000000000000000000, -5.578564026256504688E-16, 0.000000000000000000 ) ) ;
#113481 = CARTESIAN_POINT ( 'NONE',  ( 3.176612885197922953, -1.314426786483071208, 1.772596291930063739 ) ) ;
#113482 = CARTESIAN_POINT ( 'NONE',  ( 5.483742561420515749, 1.513553928502100465, 1.681752807289581986 ) ) ;
#113483 = CARTESIAN_POINT ( 'NONE',  ( -5.856759171423528088, 8.816340885760650892, 1.082531754730548412 ) ) ;
#113484 = CARTESIAN_POINT ( 'NONE',  ( 6.029554192727712980, -0.2124046070472781211, 1.799012333733180702 ) ) ;
#113485 = CARTESIAN_POINT ( 'NONE',  ( 5.524599559428126305, 0.3805214045222211627, 1.877366190154891701 ) ) ;
#113486 = CARTESIAN_POINT ( 'NONE',  ( -1.201851678989727383E-14, 5.759375000341417028, -1.575800808251660801 ) ) ;
#113487 = CARTESIAN_POINT ( 'NONE',  ( 6.385618529757402406, 1.291587659170100766, 1.353439767483602285 ) ) ;
#113488 = CARTESIAN_POINT ( 'NONE',  ( 5.775803124993572624, -1.815561990025884143, 0.4082129570420859888 ) ) ;
#113489 = CARTESIAN_POINT ( 'NONE',  ( 8.500000000000000000, 6.200000000000038369, -2.873333333333334405 ) ) ;
#113490 = CARTESIAN_POINT ( 'NONE',  ( 6.754783849477350444, -1.364574176550734208, 1.126888093558385817 ) ) ;
#113492 = VECTOR ( 'NONE', #156431, 1000.000000000000000 ) ;
#113491 = PRESENTATION_LAYER_ASSIGNMENT (  '', '', ( #109931 ) ) ;
#113493 = CARTESIAN_POINT ( 'NONE',  ( 1.622280145275534435, 1.995268681201247452, 0.2910785328335343536 ) ) ;
#113495 = CARTESIAN_POINT ( 'NONE',  ( 2.403073576612833939, 1.690916729301103594, -1.255302274246564043 ) ) ;
#113494 = CARTESIAN_POINT ( 'NONE',  ( -7.831806290188425557, 12.28885777186185990, -0.7998128361456281477 ) ) ;
#113496 = CARTESIAN_POINT ( 'NONE',  ( 8.341290820905593151, 10.75459192918846618, 1.599625672291281386 ) ) ;
#113498 = CARTESIAN_POINT ( 'NONE',  ( -9.154780037725563702, 11.70366268214508487, 1.599625672291281386 ) ) ;
#113497 = FACE_OUTER_BOUND ( 'NONE', #73372, .T. ) ;
#113499 = CARTESIAN_POINT ( 'NONE',  ( 3.287372214357705325, 0.04529362468645367623, -2.019439401957975111 ) ) ;
#113500 = CARTESIAN_POINT ( 'NONE',  ( 1.364683531249990311, 3.634375000341416584, 1.214306433183764966E-14 ) ) ;
#113501 = CARTESIAN_POINT ( 'NONE',  ( 3.602716132929354664, 5.226254793216122074, 1.599625672291267398 ) ) ;
#113502 = EDGE_CURVE ( 'NONE', #21324, #41604, #205103, .T. ) ;
#113503 = CARTESIAN_POINT ( 'NONE',  ( 3.216266648612066792, -1.062311135343798618, -1.882447817163131587 ) ) ;
#113504 = CARTESIAN_POINT ( 'NONE',  ( 7.862802741282558294, 8.137967717776607657, 0.000000000000000000 ) ) ;
#113506 = LINE ( 'NONE', #148078, #10298 ) ;
#113505 = CARTESIAN_POINT ( 'NONE',  ( 5.494797395288433250, 9.632623737803665875, 0.000000000000000000 ) ) ;
#113507 = CARTESIAN_POINT ( 'NONE',  ( 8.825994812371966702, 12.28044913353391898, -1.082531754730543083 ) ) ;
#113509 = CARTESIAN_POINT ( 'NONE',  ( 7.721398836998350390, -5.907420853759296264, -7.721398836998385917 ) ) ;
#113508 = CARTESIAN_POINT ( 'NONE',  ( 0.7839114044838908502, -2.061656150924387365, 0.6811309647984428173 ) ) ;
#113510 = CARTESIAN_POINT ( 'NONE',  ( -7.727784370109414880, 8.118095974656867497, 0.7216878364870578100 ) ) ;
#113511 = CARTESIAN_POINT ( 'NONE',  ( -1.201851678989727383E-14, 1.321875000341419248, 1.575800808251672791 ) ) ;
#113512 = CARTESIAN_POINT ( 'NONE',  ( 1.857222401600963302, 0.3706860215506869172, -2.159823580554325329 ) ) ;
#113513 = CARTESIAN_POINT ( 'NONE',  ( 0.06360284778251625026, 7.077111424252135130, 2.121658048142260444 ) ) ;
#113514 = CARTESIAN_POINT ( 'NONE',  ( 2.870297354751516039, 1.209492683862042339, 1.911920897162355582 ) ) ;
#113515 = CARTESIAN_POINT ( 'NONE',  ( -6.482770005628665011, 10.71498210654212002, 0.7998128361456481317 ) ) ;
#113516 = CARTESIAN_POINT ( 'NONE',  ( -2.616360457312984167, 5.996244933599686355, -0.7216878364870257245 ) ) ;
#113517 = CARTESIAN_POINT ( 'NONE',  ( -0.6823417656250212460, 2.863541667008084879, 1.181850606188767472 ) ) ;
#113518 = CARTESIAN_POINT ( 'NONE',  ( 5.975194856099406593, 7.098212677808693805, 1.080521340106417982 ) ) ;
#113519 = CARTESIAN_POINT ( 'NONE',  ( -1.402160292154681736E-14, 11.56249999999999822, 1.732050807568881190 ) ) ;
#113520 = CARTESIAN_POINT ( 'NONE',  ( 6.482206841109512396, 9.616306177052839743, -1.082531754730548412 ) ) ;
#113521 = EDGE_CURVE ( 'NONE', #94066, #187973, #18333, .T. ) ;
#113522 = CARTESIAN_POINT ( 'NONE',  ( 2.846658922380195911, -1.473647421164023141, 0.9796213258056789552 ) ) ;
#113523 = B_SPLINE_CURVE_WITH_KNOTS ( 'NONE', 3,
 ( #153358, #56922, #38541, #189052, #171733, #172820, #123095, #120936 ),
 .UNSPECIFIED., .F., .F.,
 ( 4, 2, 2, 4 ),
 ( 3.127317220692749988E-18, 0.003096353334791363508, 0.004644530002187043094, 0.006192706669582721812 ),
 .UNSPECIFIED. ) ;
#113524 = CIRCLE ( 'NONE', #172373, 11.89429233241351902 ) ;
#113525 = CARTESIAN_POINT ( 'NONE',  ( 6.809632187368197087, -0.4906261968062891055, 2.159508175712351541 ) ) ;
#113526 = CARTESIAN_POINT ( 'NONE',  ( 1.364683531249996529, 9.463541667008062319, 0.7879004041258405033 ) ) ;
#113527 = CARTESIAN_POINT ( 'NONE',  ( -4.749098946536820520, 8.762642214260091933, 0.7998128361456281477 ) ) ;
#113528 = CARTESIAN_POINT ( 'NONE',  ( 5.202749988929913805, 1.864175517894875789, 0.7691070904374335271 ) ) ;
#113529 = ORIENTED_EDGE ( 'NONE', *, *, #172644, .T. ) ;
#113530 = TOROIDAL_SURFACE ( 'NONE', #92767, 0.8299999999999999600, 0.08000000000000000167 ) ;
#113531 = CARTESIAN_POINT ( 'NONE',  ( 3.432352559540859271, 1.824792983844251371, 0.4109263881779609551 ) ) ;
#113532 = CARTESIAN_POINT ( 'NONE',  ( 2.922783962489564846, -1.430918204188264875, 1.496350883549990129 ) ) ;
#113533 = CARTESIAN_POINT ( 'NONE',  ( -7.580417283372126391, 8.016444050121833698, 0.7216878364870317197 ) ) ;
#113534 = DIRECTION ( 'NONE',  ( 0.000000000000000000, -1.000000000000000000, 0.000000000000000000 ) ) ;
#113535 = LINE ( 'NONE', #14870, #40862 ) ;
#113536 = CARTESIAN_POINT ( 'NONE',  ( -4.005587769924587427, 7.671888287421506192, 0.1631757730154441144 ) ) ;
#113537 = EDGE_CURVE ( 'NONE', #140937, #47720, #167100, .T. ) ;
#113538 = CARTESIAN_POINT ( 'NONE',  ( 1.364683531249988535, 3.676041667008087099, 0.7879004041258500513 ) ) ;
#113539 = CARTESIAN_POINT ( 'NONE',  ( 1.336036003918249948, -1.064896177285217016, -1.588262137521757822 ) ) ;
#113540 = CARTESIAN_POINT ( 'NONE',  ( 2.541395235131336694, 1.794889867694851260, -0.7924082849640816661 ) ) ;
#113541 = ADVANCED_FACE ( 'NONE', ( #14428 ), #79450, .T. ) ;
#113542 = CARTESIAN_POINT ( 'NONE',  ( 1.423203639035979906, 0.8144988626696235690, 1.844428818423976546 ) ) ;
#113543 = CARTESIAN_POINT ( 'NONE',  ( -5.093022980588950865, 5.970890227889075419, -1.199719254218453823 ) ) ;
#113545 = LINE ( 'NONE', #62579, #39896 ) ;
#113544 = CARTESIAN_POINT ( 'NONE',  ( 8.422639742587595180, 10.84949900448412130, -1.599625672291268286 ) ) ;
#113546 = CARTESIAN_POINT ( 'NONE',  ( 6.309841845984305309, -1.956726702252456596, 0.2390368442499128110 ) ) ;
#113547 = CARTESIAN_POINT ( 'NONE',  ( -1.364683531250014514, 1.988541667008086655, -0.7879004041258289570 ) ) ;
#113548 = CARTESIAN_POINT ( 'NONE',  ( 2.302991897352596684, -0.3483681713834784199, -1.982697776695659053 ) ) ;
#113550 = CARTESIAN_POINT ( 'NONE',  ( 2.407945773967453462, -1.221608841751795405, -1.729074501506906225 ) ) ;
#113549 = CARTESIAN_POINT ( 'NONE',  ( -6.480434237652138663, 8.583592582059388576, 1.443375672974078761 ) ) ;
#113551 = CARTESIAN_POINT ( 'NONE',  ( 0.000000000000000000, 6.487495393664096888, -3.100011470320000573 ) ) ;
#113552 = CARTESIAN_POINT ( 'NONE',  ( 4.264170421968140445, -2.065031762457261610, 0.1491743435546449281 ) ) ;
#113553 = CARTESIAN_POINT ( 'NONE',  ( 4.706615602599436343, 5.520081620234675412, 1.199719254218452935 ) ) ;
#113555 = CARTESIAN_POINT ( 'NONE',  ( 2.693266070609028784, 6.293894182352508970, 0.000000000000000000 ) ) ;
#113554 = CARTESIAN_POINT ( 'NONE',  ( 5.560518711993346130, -1.889693770910952253, -0.8946095687128383656 ) ) ;
#113557 = ORIENTED_EDGE ( 'NONE', *, *, #180876, .F. ) ;
#113556 = CARTESIAN_POINT ( 'NONE',  ( 4.330939430599492823, 0.08983702179986638447, 1.823481399301421169 ) ) ;
#113558 = CARTESIAN_POINT ( 'NONE',  ( 9.999301985278609806, 11.62460605670194447, 1.199719254218452047 ) ) ;
#113559 = CARTESIAN_POINT ( 'NONE',  ( 6.890000000000015667, 0.5768591945385994624, 2.052260346930290247 ) ) ;
#113560 = CARTESIAN_POINT ( 'NONE',  ( 12.55138299807035551, 7.397854759914610057, -0.9335798560614338992 ) ) ;
#113561 = CARTESIAN_POINT ( 'NONE',  ( 6.176841753231244958, -2.093540797633717254, -0.6980159708611932690 ) ) ;
#113562 = CARTESIAN_POINT ( 'NONE',  ( -1.364683531250010740, 10.44270833367473195, 0.7879004041258445001 ) ) ;
#113563 = EDGE_LOOP ( 'NONE', ( #23586, #136229, #89884 ) ) ;
#113564 = CARTESIAN_POINT ( 'NONE',  ( 5.022078740994724733, -1.902695638548990820, 0.1913334245251183119 ) ) ;
#113565 = CARTESIAN_POINT ( 'NONE',  ( -10.14557902172788495, 10.73093036830436553, 1.040834085586084257E-14 ) ) ;
#113566 = CARTESIAN_POINT ( 'NONE',  ( 7.202405917357655341, 9.425892875049191488, 1.599625672291281386 ) ) ;
#113567 = CARTESIAN_POINT ( 'NONE',  ( -1.360316468750002672, 1.921875000341424666, -3.642919299551294898E-14 ) ) ;
#113568 = CARTESIAN_POINT ( 'NONE',  ( 4.378920427089557421, 5.171457255435017331, -1.082531754730548412 ) ) ;
#113569 = CARTESIAN_POINT ( 'NONE',  ( 9.579665964948885559, -7.473374494045003757, -1.531435568635775013E-15 ) ) ;
#113570 = CARTESIAN_POINT ( 'NONE',  ( 6.928203230275524760, 14.48154074412736847, -9.797958971132700867 ) ) ;
#113571 = CARTESIAN_POINT ( 'NONE',  ( 0.8723036553972833840, -0.04505207493780279820, -1.840872848514919280 ) ) ;
#113572 = VERTEX_POINT ( 'NONE', #178030 ) ;
#113573 = TOROIDAL_SURFACE ( 'NONE', #210283, 0.8299999999999998490, 0.08000000000000000167 ) ;
#113574 = CARTESIAN_POINT ( 'NONE',  ( -6.050681693448748177, 10.28115541899069463, 0.7998128361456291469 ) ) ;
#113575 = CARTESIAN_POINT ( 'NONE',  ( 5.167206475355686557, 0.1846639555213614448, -1.861428779493356167 ) ) ;
#113576 = CARTESIAN_POINT ( 'NONE',  ( 10.99681319029664728, -5.196788179137230124, -0.2733121965684300325 ) ) ;
#113577 = CARTESIAN_POINT ( 'NONE',  ( 7.028976294042106332, 7.165170195996068969, 0.000000000000000000 ) ) ;
#113578 = CARTESIAN_POINT ( 'NONE',  ( -1.499999999998706812, 7.854386371690043056, -3.680172642286362983 ) ) ;
#113579 = CARTESIAN_POINT ( 'NONE',  ( -5.171754443046126859, 7.767122556988016235, 1.178735681042131667 ) ) ;
#113580 = CARTESIAN_POINT ( 'NONE',  ( -6.561783159334145132, 6.757761228752363181, -0.7216878364870278340 ) ) ;
#113581 = CARTESIAN_POINT ( 'NONE',  ( 3.974511587100456822, 7.788680618259193444, 1.040834085586084257E-14 ) ) ;
#113582 = CARTESIAN_POINT ( 'NONE',  ( 1.621857603371698708, 1.941177911247515375, -0.3314221829187612989 ) ) ;
#113583 = CARTESIAN_POINT ( 'NONE',  ( 2.302361438560030393, 1.314982760645909465, -1.528754769246756018 ) ) ;
#113584 = CARTESIAN_POINT ( 'NONE',  ( -6.835281999583978418, 11.12624609948998966, -0.7998128361456291469 ) ) ;
#113585 = CARTESIAN_POINT ( 'NONE',  ( 5.204350862799327793, 7.165104988056252289, -1.599625672291281386 ) ) ;
#113586 = CARTESIAN_POINT ( 'NONE',  ( -11.89942855770814134, 13.88000000000000078, -0.7000000000000009548 ) ) ;
#113587 = CARTESIAN_POINT ( 'NONE',  ( 2.765787700092982693, 1.173089151190203294, 1.850848517565194751 ) ) ;
#113588 = CARTESIAN_POINT ( 'NONE',  ( -8.296699936558862731, 11.76690146170562201, 1.199719254218453823 ) ) ;
#113589 = CARTESIAN_POINT ( 'NONE',  ( 1.419999999999990603, 6.280000000000042881, 2.873333333333337070 ) ) ;
#113590 = CARTESIAN_POINT ( 'NONE',  ( 0.9782388782688926643, 3.999999999999968914, 0.3999999999999576672 ) ) ;
#113591 = CARTESIAN_POINT ( 'NONE',  ( 2.929970594329034395, 6.432399770110250437, -0.7216878364870338292 ) ) ;
#113592 = CARTESIAN_POINT ( 'NONE',  ( 7.750457368506414646, 12.19395069656619945, 0.7998128361456462443 ) ) ;
#113593 = CARTESIAN_POINT ( 'NONE',  ( -9.495238110454886638, 15.17156879113547241, 7.231499654889550044 ) ) ;
#113594 = CARTESIAN_POINT ( 'NONE',  ( 6.916067756746836714, 8.201738816693689316, -1.082531754730548412 ) ) ;
#113595 = EDGE_LOOP ( 'NONE', ( #143671, #168774 ) ) ;
#113597 = CARTESIAN_POINT ( 'NONE',  ( 2.350245942676463695, 0.9471468416194218642, -1.776342852653712168 ) ) ;
#113596 = CARTESIAN_POINT ( 'NONE',  ( 4.476008884455379366, -1.787108923542475525, -0.4427587100873929815 ) ) ;
#113598 = CARTESIAN_POINT ( 'NONE',  ( 3.093437905492165907, 1.279035344561373355, -1.909460003155829311 ) ) ;
#113600 = CARTESIAN_POINT ( 'NONE',  ( 2.166652004499136197, 1.382927810177040584, -1.245475062859234372 ) ) ;
#113599 = CARTESIAN_POINT ( 'NONE',  ( -1.115562610750309283E-14, 10.06250000000000000, 1.500000000000001554 ) ) ;
#113601 = CARTESIAN_POINT ( 'NONE',  ( -3.285556943750000514, -1.888541666188711110, -1.896917185911906500 ) ) ;
#113602 = CARTESIAN_POINT ( 'NONE',  ( 6.152599605923961157, 1.892562589925715466, 0.2737767527046449101 ) ) ;
#113603 = CARTESIAN_POINT ( 'NONE',  ( -8.453672473320708036, 9.821371626084353323, -1.199719254218446718 ) ) ;
#113604 = CARTESIAN_POINT ( 'NONE',  ( -5.804299160426242388, 6.904675454319632699, -1.082531754730549967 ) ) ;
#113606 = CARTESIAN_POINT ( 'NONE',  ( 3.291731440620565330, -0.7593194595177065187, 1.709801165022284408 ) ) ;
#113605 = CARTESIAN_POINT ( 'NONE',  ( 4.757415945720180339, 2.067795187486476394, -0.3081579728113920669 ) ) ;
#113607 = CARTESIAN_POINT ( 'NONE',  ( 7.049876689426101350, 9.247942109129029475, -1.443375672974057666 ) ) ;
#113608 = CARTESIAN_POINT ( 'NONE',  ( 5.776868925826902590, 1.698781319366513998, -0.7106697882480541573 ) ) ;
#113609 = CARTESIAN_POINT ( 'NONE',  ( 4.304877467538922531, 4.981110786005563007, 1.199719254218464037 ) ) ;
#113611 = CARTESIAN_POINT ( 'NONE',  ( 5.355634372598031767, 6.206993841907870291, -1.199719254218445830 ) ) ;
#113610 = DIRECTION ( 'NONE',  ( 0.5005768354468328463, 0.8656921114426504582, -5.551115123125790098E-17 ) ) ;
#113612 = CARTESIAN_POINT ( 'NONE',  ( 5.268053373232242542, 0.8548693298336268453, 1.498049451945895116 ) ) ;
#113613 = CARTESIAN_POINT ( 'NONE',  ( -7.400052914960538963, 7.527816577075747695, 1.040834085586084257E-14 ) ) ;
#113614 = CARTESIAN_POINT ( 'NONE',  ( 3.511198596259283544, 6.271927390929319834, 1.164732466530402855 ) ) ;
#113615 = CARTESIAN_POINT ( 'NONE',  ( 1.907713928855335972, 3.283019769909846897, 0.4154771360143372783 ) ) ;
#113616 = ADVANCED_FACE ( 'NONE', ( #96801 ), #48051, .F. ) ;
#113617 = CIRCLE ( 'NONE', #92866, 2.025000000000006573 ) ;
#113618 = LINE ( 'NONE', #193723, #155400 ) ;
#113619 = CARTESIAN_POINT ( 'NONE',  ( 4.293918747171243666, -1.492831977124044363, -1.576629974643141363 ) ) ;
#113620 = CARTESIAN_POINT ( 'NONE',  ( 3.475057130574196407, 0.04366187338752242769, -1.825333387291371512 ) ) ;
#113621 = CARTESIAN_POINT ( 'NONE',  ( 1.129655866247070595, 1.892139549451707037, -0.5178372573612435303 ) ) ;
#113622 = CARTESIAN_POINT ( 'NONE',  ( 5.753141757616087482, 0.1533694674813860792, -2.111807561841658742 ) ) ;
#113624 = CARTESIAN_POINT ( 'NONE',  ( -0.6823417656250212460, 4.113541667008085767, 1.181850606188767472 ) ) ;
#113623 = CARTESIAN_POINT ( 'NONE',  ( 5.355124402800013783, 0.4497703203518633175, -2.247661708361737620 ) ) ;
#113625 = CARTESIAN_POINT ( 'NONE',  ( 9.512045263456263555, -8.176568542494905500, -0.4655551865852067817 ) ) ;
#113626 = CARTESIAN_POINT ( 'NONE',  ( 8.483651433849084711, 10.92067931095586886, 1.599625672291281386 ) ) ;
#113627 = CARTESIAN_POINT ( 'NONE',  ( 2.332823983099761911, 1.383068002389773454, -1.607457772141835717 ) ) ;
#113628 = CARTESIAN_POINT ( 'NONE',  ( -3.307826292054304673, 6.802955074131234348, -0.7216878364870267237 ) ) ;
#113629 = CARTESIAN_POINT ( 'NONE',  ( -3.917943204224913156, 7.514758138330285497, -0.7216878364870257245 ) ) ;
#113631 = CIRCLE ( 'NONE', #188542, 0.08000000000000020983 ) ;
#113630 = MECHANICAL_DESIGN_GEOMETRIC_PRESENTATION_REPRESENTATION (  '', ( #137711 ), #103068 ) ;
#113632 = CARTESIAN_POINT ( 'NONE',  ( 6.227409518260961896, 0.1680337313966096258, -2.164657318592048352 ) ) ;
#113634 = CARTESIAN_POINT ( 'NONE',  ( -0.7500000000000179856, 14.07291666734946567, 1.299038105676658228 ) ) ;
#113633 = CARTESIAN_POINT ( 'NONE',  ( 6.983263157960355016, 2.444413620957446742, 2.336241774956763884 ) ) ;
#113636 = EDGE_LOOP ( 'NONE', ( #148394, #200840, #133982, #53565 ) ) ;
#113635 = CARTESIAN_POINT ( 'NONE',  ( 2.789914007569836318, 2.108506539658880907, -0.6989939510357189301 ) ) ;
#113637 = CARTESIAN_POINT ( 'NONE',  ( 0.1066027571702803795, -0.1042336552941041522, 2.296444677329109840 ) ) ;
#113639 = CARTESIAN_POINT ( 'NONE',  ( 5.612196365462351011, 2.060443358388251323, -0.09580443939274756182 ) ) ;
#113638 = CARTESIAN_POINT ( 'NONE',  ( 2.683624340501134853, 5.218313266304903664, -1.199719254218446718 ) ) ;
#113641 = CARTESIAN_POINT ( 'NONE',  ( -3.474999999999998312, -1.720833333333333881, 2.006292185433951047 ) ) ;
#113640 = CARTESIAN_POINT ( 'NONE',  ( 3.881377115262159894, 7.750300077773022878, 0.7998128361456271485 ) ) ;
#113642 = CARTESIAN_POINT ( 'NONE',  ( 5.899733120602060232, 6.912052057904395141, -1.199719254218452047 ) ) ;
#113643 = CARTESIAN_POINT ( 'NONE',  ( 3.285556943749998737, -0.2552083328553768071, -1.896917185911906500 ) ) ;
#113644 = CARTESIAN_POINT ( 'NONE',  ( 0.1333542156527140476, 0.7077123155428012291, -2.127987941987404596 ) ) ;
#113645 = CARTESIAN_POINT ( 'NONE',  ( 6.005383971424570255, -1.826508537601937432, 0.2321369796495567073 ) ) ;
#113647 = ORIENTED_EDGE ( 'NONE', *, *, #59329, .T. ) ;
#113646 = CARTESIAN_POINT ( 'NONE',  ( 5.168682875307768931, 7.053215992657626110, -1.599625672291256295 ) ) ;
#113648 = CARTESIAN_POINT ( 'NONE',  ( -4.909967638851771454, 4.671257834700952571, -0.2941531795261614346 ) ) ;
#113649 = CARTESIAN_POINT ( 'NONE',  ( 1.553258647468837461, 0.5056154618373939202, -1.648988316134043286 ) ) ;
#113650 = CARTESIAN_POINT ( 'NONE',  ( 1.464077725791514517, -1.074659653367866952, 1.706114136832518779 ) ) ;
#113651 = CARTESIAN_POINT ( 'NONE',  ( 1.741309990946012132, 2.292119649597070374, -0.1747640694012199680 ) ) ;
#113652 = CARTESIAN_POINT ( 'NONE',  ( -0.6823417656249969321, 4.030208333674754506, -1.181850606188749264 ) ) ;
#113653 = CARTESIAN_POINT ( 'NONE',  ( 1.933286576697599513, 0.2207578219815004572, 2.251582216785783075 ) ) ;
#113654 = CARTESIAN_POINT ( 'NONE',  ( 4.670599442626208742, -1.376304852316366789, 1.594240983682773782 ) ) ;
#113655 = CARTESIAN_POINT ( 'NONE',  ( -5.144392941742557568, 4.966489618313220333, -0.7998128361456362523 ) ) ;
#113656 = CARTESIAN_POINT ( 'NONE',  ( 2.125891686596991903, 1.023501848097716493, -1.443529828085978739 ) ) ;
#113657 = CARTESIAN_POINT ( 'NONE',  ( 5.503720292143644777, 8.508425209887878538, 1.199719254218462483 ) ) ;
#113658 = CARTESIAN_POINT ( 'NONE',  ( 5.031484404002879884, 6.963427452793765404, 1.443375672974065660 ) ) ;
#113659 = CARTESIAN_POINT ( 'NONE',  ( -3.899941742225307539, 7.701682465904834629, 0.7998128361456341429 ) ) ;
#113660 = CARTESIAN_POINT ( 'NONE',  ( -0.7500000000000215383, 2.191666666666689078, 1.299038105676671107 ) ) ;
#113661 = EDGE_CURVE ( 'NONE', #202706, #40283, #39378, .T. ) ;
#113662 = CARTESIAN_POINT ( 'NONE',  ( 6.504121277450023442, -0.9500910533294173455, 2.005660710250598555 ) ) ;
#113663 = CARTESIAN_POINT ( 'NONE',  ( 3.029421956395737858, -1.472182739719897215, -1.623467934892895759 ) ) ;
#113664 = CARTESIAN_POINT ( 'NONE',  ( -4.273844736805832767, 6.009238164405336313, 1.599625672291267398 ) ) ;
#113665 = CARTESIAN_POINT ( 'NONE',  ( 0.1598595594940413200, 7.033953395470825321, -1.994736385849473104 ) ) ;
#113666 = CARTESIAN_POINT ( 'NONE',  ( 0.000000000000000000, 4.518459255872631530, 0.000000000000000000 ) ) ;
#113667 = CARTESIAN_POINT ( 'NONE',  ( -0.6823417656250003738, 2.717708333674753618, -1.181850606188749264 ) ) ;
#113668 = CARTESIAN_POINT ( 'NONE',  ( -0.6823417656250039265, 9.067708333674733723, -1.181850606188755259 ) ) ;
#113669 = CARTESIAN_POINT ( 'NONE',  ( -3.795919822146283540, 6.412028311603867436, -1.082531754730549967 ) ) ;
#113670 = CARTESIAN_POINT ( 'NONE',  ( 5.941668366282724101, -1.996146358238064522, 0.7160658055916299114 ) ) ;
#113671 = CARTESIAN_POINT ( 'NONE',  ( -6.292392690518214593, 7.474117906093608710, -1.082531754730549967 ) ) ;
#113672 = ORIENTED_EDGE ( 'NONE', *, *, #111152, .T. ) ;
#113674 = CARTESIAN_POINT ( 'NONE',  ( -5.287316719649554742, 5.270883715786981227, 0.7216878364870288332 ) ) ;
#113673 = CARTESIAN_POINT ( 'NONE',  ( -6.156811154381562012, 6.355570232966157640, 0.7216878364870257245 ) ) ;
#113675 = CARTESIAN_POINT ( 'NONE',  ( 4.171104814498611368, 8.018039383557042044, 0.7998128361456321445 ) ) ;
#113676 = CARTESIAN_POINT ( 'NONE',  ( 1.084637062511527361, 3.057371192708035146, -1.105835307554789759 ) ) ;
#113677 = CARTESIAN_POINT ( 'NONE',  ( -1.115562610750309283E-14, 11.09375000068279427, 1.500000000000001554 ) ) ;
#113678 = CARTESIAN_POINT ( 'NONE',  ( 0.3903331447352873518, 6.430882250648634724, -3.207843000864786465 ) ) ;
#113679 = CARTESIAN_POINT ( 'NONE',  ( 1.364683531249990311, 4.196875000341417028, 1.214306433183764966E-14 ) ) ;
#113680 = CARTESIAN_POINT ( 'NONE',  ( 2.313636755748917473, 1.135937956827288042, -1.318730690005095241 ) ) ;
#113681 = CARTESIAN_POINT ( 'NONE',  ( -5.571360081631161698, 7.090533140868425122, -1.217465838365646258 ) ) ;
#113684 = EDGE_CURVE ( 'NONE', #12264, #147312, #25454, .T. ) ;
#113683 = CARTESIAN_POINT ( 'NONE',  ( 11.84101807917483740, 12.48978499739120629, 1.444039656437077657 ) ) ;
#113682 =( GEOMETRIC_REPRESENTATION_CONTEXT ( 3 ) GLOBAL_UNCERTAINTY_ASSIGNED_CONTEXT ( ( #48658 ) ) GLOBAL_UNIT_ASSIGNED_CONTEXT ( ( #131175, #2, #117047 ) ) REPRESENTATION_CONTEXT ( 'NONE', 'WORKASPACE' ) );
#113685 = CARTESIAN_POINT ( 'NONE',  ( -1.402160292154681736E-14, -0.2406249996585799189, -1.575800808251665908 ) ) ;
#113686 = CARTESIAN_POINT ( 'NONE',  ( 6.789893189004300389, -0.9291300992274166282, 1.949920244826188309 ) ) ;
#113687 = EDGE_CURVE ( 'NONE', #40132, #201589, #4702, .T. ) ;
#113688 = B_SPLINE_CURVE_WITH_KNOTS ( 'NONE', 3,
 ( #36332, #2748, #54729, #168478, #135991, #21126 ),
 .UNSPECIFIED., .F., .F.,
 ( 4, 2, 4 ),
 ( 0.001279092382393100377, 0.001599469101539997178, 0.001919845820686893979 ),
 .UNSPECIFIED. ) ;
#113689 = CARTESIAN_POINT ( 'NONE',  ( -7.974166903131914452, 12.45494515362926435, -0.7998128361456281477 ) ) ;
#113690 = CARTESIAN_POINT ( 'NONE',  ( -6.683806541412776525, 7.860491055478785682, -1.082531754730543083 ) ) ;
#113691 = CARTESIAN_POINT ( 'NONE',  ( 6.069229152942410721, 0.1638285306290178100, -2.155560115052157055 ) ) ;
#113693 = VERTEX_POINT ( 'NONE', #144500 ) ;
#113692 = DIRECTION ( 'NONE',  ( 0.000000000000000000, -1.000000000000000000, 0.000000000000000000 ) ) ;
#113694 = CARTESIAN_POINT ( 'NONE',  ( -1.364683531249997417, 4.509375000341424133, 1.214306433183764966E-14 ) ) ;
#113695 = CARTESIAN_POINT ( 'NONE',  ( 5.835224730271552751, -1.783237572924928127, 0.8406590917669158891 ) ) ;
#113696 = CARTESIAN_POINT ( 'NONE',  ( 4.903498277369322977, 0.2971982615034232111, 1.707963748468165122 ) ) ;
#113698 = CARTESIAN_POINT ( 'NONE',  ( 2.507599501126521524, -2.167277876680247850, 0.3246147914140809498 ) ) ;
#113697 = CARTESIAN_POINT ( 'NONE',  ( -1.360316468750026653, -0.1302083329919105914, -0.7853790794159422051 ) ) ;
#113699 = CARTESIAN_POINT ( 'NONE',  ( 3.698509654486553000, -2.304784958540738060, -0.1161927354758583580 ) ) ;
#113700 = CARTESIAN_POINT ( 'NONE',  ( 6.327427223165448922, -1.941958050844143413, 0.6900897555163245656 ) ) ;
#113701 = CARTESIAN_POINT ( 'NONE',  ( 1.622886899410342254, -1.828648197406743670, 0.6539591521299585875 ) ) ;
#113702 = CARTESIAN_POINT ( 'NONE',  ( -5.707619481228822345, 7.681975366232176583, -1.443375672974051449 ) ) ;
#113703 = CARTESIAN_POINT ( 'NONE',  ( -3.644109427023046521, 7.473487774827342278, 0.000000000000000000 ) ) ;
#113704 = CARTESIAN_POINT ( 'NONE',  ( 4.991989969715248776, 4.726297878971393196, -2.500000000000000444 ) ) ;
#113705 = CARTESIAN_POINT ( 'NONE',  ( 3.885109016898561585, -1.979880364965879380, -0.7601140796509860964 ) ) ;
#113706 =( NAMED_UNIT ( * ) PLANE_ANGLE_UNIT ( ) SI_UNIT ( $, .RADIAN. ) );
#113707 = CARTESIAN_POINT ( 'NONE',  ( 2.039685609654022347, -1.556907966322677472, 1.281362143053674130 ) ) ;
#113708 = CARTESIAN_POINT ( 'NONE',  ( -5.002595493318215070, 7.819816594637776674, 1.082531754730560403 ) ) ;
#113709 = CARTESIAN_POINT ( 'NONE',  ( 4.805825877545530922, -0.5924843665619135002, 2.125676689404366826 ) ) ;
#113710 = CARTESIAN_POINT ( 'NONE',  ( -4.725311769113643479, 5.222111817384738508, 1.090456963845821914 ) ) ;
#113711 = CARTESIAN_POINT ( 'NONE',  ( -10.38614328979761403, 3.507114751586604129, 5.996442624206741456 ) ) ;
#113712 = CARTESIAN_POINT ( 'NONE',  ( -0.005637892868452093476, -0.3948761927005627337, -1.788892068844874395 ) ) ;
#113713 = CARTESIAN_POINT ( 'NONE',  ( -6.074935347375019390, 9.245119117649618801, 1.199719254218452047 ) ) ;
#113715 = DIRECTION ( 'NONE',  ( -0.000000000000000000, -1.000000000000000000, -0.000000000000000000 ) ) ;
#113714 = CARTESIAN_POINT ( 'NONE',  ( -4.587973201513257493, 8.494803767824503637, 0.1163994284540965235 ) ) ;
#113716 = CARTESIAN_POINT ( 'NONE',  ( -1.162044386198238837E-16, 2.062499999999991562, 1.224999999999974332 ) ) ;
#113717 = ORIENTED_EDGE ( 'NONE', *, *, #142095, .T. ) ;
#113718 = CARTESIAN_POINT ( 'NONE',  ( 4.803620198249330286, -0.5517947341296326469, 1.985563166520041278 ) ) ;
#113719 = CARTESIAN_POINT ( 'NONE',  ( -6.061904078641520144, 10.08632216847484031, 0.7216878364870267237 ) ) ;
#113720 = DIRECTION ( 'NONE',  ( -0.000000000000000000, 1.000000000000000000, -0.000000000000000000 ) ) ;
#113721 = CARTESIAN_POINT ( 'NONE',  ( -5.850506979496850057, 6.784345216623154151, -1.199719254218446718 ) ) ;
#113722 = CARTESIAN_POINT ( 'NONE',  ( -5.652823702255029836, 5.559658838911111900, -0.7998128361456362523 ) ) ;
#113723 = CARTESIAN_POINT ( 'NONE',  ( 3.527994226718012438, -1.989412488823691483, 0.3473740275561196245 ) ) ;
#113724 = CARTESIAN_POINT ( 'NONE',  ( -0.7500000000000215383, 0.4416666666666874130, 1.299038105676659116 ) ) ;
#113725 = CARTESIAN_POINT ( 'NONE',  ( 9.408995418203963013, 12.00024729270324286, 1.443375672974076540 ) ) ;
#113726 = CARTESIAN_POINT ( 'NONE',  ( 7.806797523370503811, 8.002351953554066810, 1.040834085586084257E-14 ) ) ;
#113727 = CARTESIAN_POINT ( 'NONE',  ( 3.450122203709057533, 2.061077815303002936, 0.001625369314967386580 ) ) ;
#113728 = CARTESIAN_POINT ( 'NONE',  ( 0.000000000000000000, 9.799999999999998934, 0.000000000000000000 ) ) ;
#113729 = CARTESIAN_POINT ( 'NONE',  ( 5.681030059326015014, 6.586622143090519188, -1.199719254218445830 ) ) ;
#113730 = CARTESIAN_POINT ( 'NONE',  ( -0.2409995289980246813, 5.721856934700204178, -2.594540323675114113 ) ) ;
#113731 = CARTESIAN_POINT ( 'NONE',  ( 1.728195974063054141, 0.1793598003074353686, 1.832383557197496460 ) ) ;
#113732 = CARTESIAN_POINT ( 'NONE',  ( 6.621690180768193379, -2.141820631849135292, 0.5315211216728524812 ) ) ;
#113733 = CARTESIAN_POINT ( 'NONE',  ( 6.249382461256315580, 6.255644057745969988, -0.7998128361456481317 ) ) ;
#113734 = CARTESIAN_POINT ( 'NONE',  ( 2.460438939752377152, 0.9218109643280818499, 1.955300211207489758 ) ) ;
#113735 = CARTESIAN_POINT ( 'NONE',  ( -4.012850279964973232, 4.744375417122949301, 1.082531754730560403 ) ) ;
#113736 = CARTESIAN_POINT ( 'NONE',  ( 1.446500318503377125, -1.422605717829699801, 1.429450658469958668 ) ) ;
#113737 = CARTESIAN_POINT ( 'NONE',  ( 2.513387927098627905, 2.297807174607501057, 0.05796762653747893068 ) ) ;
#113738 = CARTESIAN_POINT ( 'NONE',  ( 6.509799877575611404, 5.178456542363087500, -2.499999999999995559 ) ) ;
#113739 = CARTESIAN_POINT ( 'NONE',  ( 0.1263921868141482663, 7.050106634747087320, 4.033475512996064438 ) ) ;
#113740 = SHAPE_REPRESENTATION ( 'positive coil', ( #200407 ), #124605 ) ;
#113741 = CARTESIAN_POINT ( 'NONE',  ( 5.049669536805332370, 0.6190787695102616395, -1.871797661314599015 ) ) ;
#113742 = CARTESIAN_POINT ( 'NONE',  ( 4.100796195634116792, 1.845626398921360822, 0.8128187495666516771 ) ) ;
#113744 = CARTESIAN_POINT ( 'NONE',  ( 8.066738210006668908, 12.35501897840907581, 0.7216878364870438212 ) ) ;
#113743 = CARTESIAN_POINT ( 'NONE',  ( 1.364683531249988535, 3.363541667008084879, 0.7879004041258500513 ) ) ;
#113746 = CARTESIAN_POINT ( 'NONE',  ( 6.674446291637649686, -1.297315479741867117, 1.659578660624160706 ) ) ;
#113745 = CARTESIAN_POINT ( 'NONE',  ( -5.852315862593199469, 9.979452273000736895, 0.7998128361456481317 ) ) ;
#113747 = B_SPLINE_CURVE_WITH_KNOTS ( 'NONE', 3,
 ( #121260, #90830, #187233, #8480, #74567, #140666, #206681, #75632, #42084, #9556, #76684, #30078, #29012, #62564 ),
 .UNSPECIFIED., .F., .F.,
 ( 4, 2, 2, 2, 2, 2, 4 ),
 ( 0.001720018798322440947, 0.002147110083253096074, 0.002360655725718421687, 0.002574201368183750335, 0.003001292653114406763, 0.003214838295579734977, 0.003428383938045063192 ),
 .UNSPECIFIED. ) ;
#113748 = CARTESIAN_POINT ( 'NONE',  ( 6.883263157960362477, -0.004191378316371896506, 2.053658919477070910 ) ) ;
#113749 = CARTESIAN_POINT ( 'NONE',  ( 5.035963992472171746, 7.962709526937818083, 1.199719254218462483 ) ) ;
#113750 = CARTESIAN_POINT ( 'NONE',  ( -6.093499974338126179, 9.196501505781426999, -1.199719254218440723 ) ) ;
#113751 = FACE_OUTER_BOUND ( 'NONE', #141990, .T. ) ;
#113752 = CARTESIAN_POINT ( 'NONE',  ( 4.276219423538512032, -1.135946514926335915, 1.611120745738093385 ) ) ;
#113753 = CARTESIAN_POINT ( 'NONE',  ( 6.469012451414649867, -1.558587985773008278, 1.284399031846704009 ) ) ;
#113754 = CARTESIAN_POINT ( 'NONE',  ( 0.7499999999999885647, 0.8479166673494853423, -1.299038105676652899 ) ) ;
#113755 = CARTESIAN_POINT ( 'NONE',  ( 4.494930827260392725, -0.5027447494639860626, -2.252120713733107404 ) ) ;
#113756 = CARTESIAN_POINT ( 'NONE',  ( 2.465751394709358113, -0.4561089685623443968, 2.011347002571160836 ) ) ;
#113757 = CARTESIAN_POINT ( 'NONE',  ( 6.290620087060792009, 10.28288116830553101, -0.7216878364870267237 ) ) ;
#113758 = EDGE_CURVE ( 'NONE', #139509, #74995, #105103, .T. ) ;
#113759 = CARTESIAN_POINT ( 'NONE',  ( 4.681308178468477799, 8.683552984847038303, 0.000000000000000000 ) ) ;
#113760 = CARTESIAN_POINT ( 'NONE',  ( 3.874598038455354665, 7.742391154831717692, -0.7998128361456362523 ) ) ;
#113761 = CARTESIAN_POINT ( 'NONE',  ( 1.364683531249988757, 0.6968750003414209138, 0.000000000000000000 ) ) ;
#113762 = CARTESIAN_POINT ( 'NONE',  ( 3.067887898442204442, 6.801229324816399746, 0.7998128361456271485 ) ) ;
#113763 = CARTESIAN_POINT ( 'NONE',  ( 6.521108698048765362, 8.631046119188804155, -1.443375672974058777 ) ) ;
#113764 = CARTESIAN_POINT ( 'NONE',  ( 3.736941271748619009, -2.091586689864731063, -0.5821943698010292323 ) ) ;
#113765 = DIRECTION ( 'NONE',  ( 0.000000000000000000, 1.000000000000000000, 0.000000000000000000 ) ) ;
#113767 = CARTESIAN_POINT ( 'NONE',  ( 2.735704033801298785, 1.827604811068459956, 0.2230458208379028362 ) ) ;
#113766 = CARTESIAN_POINT ( 'NONE',  ( -3.958617665510283601, 4.681104033592509595, -1.082531754730549967 ) ) ;
#113768 = CARTESIAN_POINT ( 'NONE',  ( -1.364683531249997417, 4.759375000341424133, 1.214306433183764966E-14 ) ) ;
#113769 = CARTESIAN_POINT ( 'NONE',  ( 5.829655996829377962, 1.081331853127937448, -1.906115348727636549 ) ) ;
#113770 = CARTESIAN_POINT ( 'NONE',  ( 6.902720145100436078, 14.55347103577509138, 9.761920446467003742 ) ) ;
#113771 = CARTESIAN_POINT ( 'NONE',  ( 5.559536883401111851, 0.4474127746876849221, -2.217688626266269392 ) ) ;
#113772 = CARTESIAN_POINT ( 'NONE',  ( -4.976004696740268685, 6.814476922186354813, -1.450531527366223372 ) ) ;
#113773 = CARTESIAN_POINT ( 'NONE',  ( 4.597876849858236525, 8.486543085689454813, -0.1053875944492469602 ) ) ;
#113774 = CARTESIAN_POINT ( 'NONE',  ( -4.787437638956927977, 7.639075441208117212, -1.082531754730549967 ) ) ;
#113775 = CARTESIAN_POINT ( 'NONE',  ( -2.978854731913820775, 6.490225589564778019, 0.1926073594339854922 ) ) ;
#113776 = CARTESIAN_POINT ( 'NONE',  ( 6.538360807962172672, 1.750891970090788119, 0.2567797125347607845 ) ) ;
#113777 = CARTESIAN_POINT ( 'NONE',  ( -1.402160292154681736E-14, 11.92187500034140157, 1.575800808251682339 ) ) ;
#113778 = CARTESIAN_POINT ( 'NONE',  ( 4.494793336055456834, -1.953237823851183164, -0.4868166104980836684 ) ) ;
#113779 = CARTESIAN_POINT ( 'NONE',  ( 6.307567778855705853, 8.381915046796901692, -1.599625672291262513 ) ) ;
#113780 = CARTESIAN_POINT ( 'NONE',  ( 3.294068349240862226, -0.8549715976811816942, 1.924793576080959578 ) ) ;
#113781 = CARTESIAN_POINT ( 'NONE',  ( 2.249496223418820939, 1.878159554852454338, -0.3759676508649934523 ) ) ;
#113782 = CARTESIAN_POINT ( 'NONE',  ( 4.033714395265605823, 4.664753868353354704, -1.199719254218446718 ) ) ;
#113783 = CARTESIAN_POINT ( 'NONE',  ( 2.805082309988204514, -1.639025760435019130, 1.091792480472515647 ) ) ;
#113784 = CARTESIAN_POINT ( 'NONE',  ( 1.147088892781012781, -1.472398045354219365, -1.153743250124287689 ) ) ;
#113785 = CARTESIAN_POINT ( 'NONE',  ( 1.609737659951641309, 0.5726723138891121057, -1.876404140693301414 ) ) ;
#113788 = ORIENTED_EDGE ( 'NONE', *, *, #9722, .F. ) ;
#113787 = CARTESIAN_POINT ( 'NONE',  ( 0.2461629937395051204, 0.9812432698282257393, -1.641294572782559413 ) ) ;
#113786 = CARTESIAN_POINT ( 'NONE',  ( 3.545241905100663615, -1.307145164029408502, -1.125523404956897178 ) ) ;
#113790 = CARTESIAN_POINT ( 'NONE',  ( 4.351804120306567825, 8.020929207092235558, 1.040834085586084257E-14 ) ) ;
#113789 = CARTESIAN_POINT ( 'NONE',  ( 1.102499568101540817, -2.207063161980229005, 0.003256074490760872773 ) ) ;
#113791 = CARTESIAN_POINT ( 'NONE',  ( -1.364683531250014514, 0.05104166700808546175, -0.7879004041258359514 ) ) ;
#113792 = CARTESIAN_POINT ( 'NONE',  ( 6.596569749568344854, -0.5012203084251048990, -1.802199723311518786 ) ) ;
#113793 = CARTESIAN_POINT ( 'NONE',  ( -1.201851678989727383E-14, 3.196875000341421025, -1.575800808251660134 ) ) ;
#113794 = CARTESIAN_POINT ( 'NONE',  ( 6.999862025036645008, -6.532648833121171172, -6.392587740394702678 ) ) ;
#113795 = FACE_OUTER_BOUND ( 'NONE', #196997, .T. ) ;
#113796 = PRESENTATION_LAYER_ASSIGNMENT (  '', '', ( #92881 ) ) ;
#113797 = CARTESIAN_POINT ( 'NONE',  ( 0.9946828900261883710, 2.039433816042154124, 0.3556643922909968891 ) ) ;
#113798 = CARTESIAN_POINT ( 'NONE',  ( -0.7500000000000006661, 2.358333333333358262, -1.299038105676652011 ) ) ;
#113799 = CARTESIAN_POINT ( 'NONE',  ( 7.396136491454752715, 8.587579647240744407, 1.199719254218462483 ) ) ;
#113800 = CARTESIAN_POINT ( 'NONE',  ( -7.015454420067433361, 10.27211502579893754, 1.199719254218453823 ) ) ;
#113801 = CARTESIAN_POINT ( 'NONE',  ( 5.285699784481295183, 7.260012063351913625, 1.599625672291268286 ) ) ;
#113802 = CARTESIAN_POINT ( 'NONE',  ( 5.356147330077114077, 0.8591290142025626020, -1.938821108677920346 ) ) ;
#113803 = CARTESIAN_POINT ( 'NONE',  ( 3.074666975249065626, 6.809138247757705820, 0.000000000000000000 ) ) ;
#113804 = ADVANCED_FACE ( 'NONE', ( #49096 ), #160705, .T. ) ;
#113805 = CARTESIAN_POINT ( 'NONE',  ( 1.364683531249988535, 1.863541667008086211, 0.7879004041258500513 ) ) ;
#113806 = ORIENTED_EDGE ( 'NONE', *, *, #210461, .F. ) ;
#113807 = CARTESIAN_POINT ( 'NONE',  ( -0.7500000000000215383, 1.941666666666688634, 1.299038105676659116 ) ) ;
#113809 = CARTESIAN_POINT ( 'NONE',  ( 4.708759422647839976, 4.387974169377582001, -0.7998128361456211532 ) ) ;
#113808 = CARTESIAN_POINT ( 'NONE',  ( 6.760214184729610665, -1.961454122871961747, 0.04698431645466792650 ) ) ;
#113810 = EDGE_CURVE ( 'NONE', #155586, #144610, #143170, .T. ) ;
#113811 = CARTESIAN_POINT ( 'NONE',  ( 4.727888646976695419, -1.799647678597478206, -0.9090046787488814672 ) ) ;
#113812 = CARTESIAN_POINT ( 'NONE',  ( 4.188635153834672664, 1.476993813991718918, -1.219978962091677221 ) ) ;
#113813 = CARTESIAN_POINT ( 'NONE',  ( 11.84668730067608244, 10.19999999999999929, -1.400000000000001688 ) ) ;
#113814 = CARTESIAN_POINT ( 'NONE',  ( 2.015410700679621137, -2.124826835150806392, 0.5361769018528695918 ) ) ;
#113815 = CARTESIAN_POINT ( 'NONE',  ( -1.772826578343177140, 3.950000000000023714, 0.3999999999999835354 ) ) ;
#113816 = CARTESIAN_POINT ( 'NONE',  ( 3.356579238971897805, -1.418645411611328067, 1.219307012350186126 ) ) ;
#113817 = CARTESIAN_POINT ( 'NONE',  ( -0.7500000000000215383, 0.7229166673494852313, 1.299038105676659116 ) ) ;
#113818 = CARTESIAN_POINT ( 'NONE',  ( -5.520141099058386125, 9.591915048876776595, 0.000000000000000000 ) ) ;
#113819 = EDGE_CURVE ( 'NONE', #60282, #93441, #18484, .T. ) ;
#113821 = CARTESIAN_POINT ( 'NONE',  ( 5.413701396201449079, -1.343708383727526101, -1.636158592728423455 ) ) ;
#113820 = CARTESIAN_POINT ( 'NONE',  ( -4.826339496784927796, 5.693446170079573321, 1.082531754730560403 ) ) ;
#113822 = CARTESIAN_POINT ( 'NONE',  ( 0.6823417656249934904, 8.505208333674733723, 1.181850606188764807 ) ) ;
#113824 = CARTESIAN_POINT ( 'NONE',  ( -7.930593509350902792, 8.217056947189661287, -0.7998128361456362523 ) ) ;
#113823 = CARTESIAN_POINT ( 'NONE',  ( 2.841443172333203204, 0.7501175549536406306, -1.951742197369815912 ) ) ;
#113826 = ORIENTED_EDGE ( 'NONE', *, *, #176689, .F. ) ;
#113825 = CARTESIAN_POINT ( 'NONE',  ( 1.184105695005283287, -1.681391461502951046, -0.3836232258775870152 ) ) ;
#113827 = CARTESIAN_POINT ( 'NONE',  ( 6.531277313481192337, 8.642909503859968368, 1.599625672291281386 ) ) ;
#113828 = CARTESIAN_POINT ( 'NONE',  ( -7.667935170093251429, -6.766388843766943495, -7.887197531381546334 ) ) ;
#113829 = CARTESIAN_POINT ( 'NONE',  ( 6.856061878569608298E-15, 0.9375000000000238698, -1.225000000000010303 ) ) ;
#113830 = VECTOR ( 'NONE', #107058, 1000.000000000000000 ) ;
#113831 = CARTESIAN_POINT ( 'NONE',  ( -9.340702556249551591, 14.55305236562982607, 7.462845556860540519 ) ) ;
#113833 = CARTESIAN_POINT ( 'NONE',  ( 8.066738210006668908, 12.35501897840907581, 0.7216878364870438212 ) ) ;
#113832 = CARTESIAN_POINT ( 'NONE',  ( 6.174848896020108668, 9.291408581077091000, 1.199719254218460707 ) ) ;
#113834 = ORIENTED_EDGE ( 'NONE', *, *, #81943, .F. ) ;
#113836 =( BOUNDED_CURVE ( )  B_SPLINE_CURVE ( 2, ( #52413, #87040, #168296, #6832, #118539, #71831, #170415 ),
 .UNSPECIFIED., .F., .T. ) 
 B_SPLINE_CURVE_WITH_KNOTS ( ( 3, 2, 2, 3 ),
 ( 0.05357142857142838110, 0.05952380952380941642, 0.06547619047619046562, 0.07142857142857149400 ),
 .UNSPECIFIED. ) 
 CURVE ( )  GEOMETRIC_REPRESENTATION_ITEM ( )  RATIONAL_B_SPLINE_CURVE ( ( 1.000000000000004219, 0.8660254037844345998, 1.000000000000000000, 0.8660254037844387076, 1.000000000000000000, 0.8660254037844371533, 1.000000000000001554 ) ) 
 REPRESENTATION_ITEM ( '' )  );
#113835 = CARTESIAN_POINT ( 'NONE',  ( -1.878188943807090672, 3.299815425349210685, 0.3999999999999993006 ) ) ;
#113837 = ORIENTED_EDGE ( 'NONE', *, *, #45569, .T. ) ;
#113839 = CARTESIAN_POINT ( 'NONE',  ( 1.980848084912645524, -1.656539610615878955, -0.7334085510423118404 ) ) ;
#113838 = CARTESIAN_POINT ( 'NONE',  ( 5.234329823327693809, 8.264412672927770487, 1.199719254218451159 ) ) ;
#113840 = CARTESIAN_POINT ( 'NONE',  ( -5.910464900553636269, 8.982960586366182554, -1.199719254218440723 ) ) ;
#113841 = CARTESIAN_POINT ( 'NONE',  ( 5.355634372598031767, 6.206993841907870291, -1.199719254218445830 ) ) ;
#113842 = CARTESIAN_POINT ( 'NONE',  ( 6.737475991348287785, 6.825086509519945999, -0.7998128361456481317 ) ) ;
#113843 = CARTESIAN_POINT ( 'NONE',  ( 6.539320575229250032, 4.701774335136183147, 2.359470009949143243 ) ) ;
#113844 = LINE ( 'NONE', #81265, #10964 ) ;
#113845 = CARTESIAN_POINT ( 'NONE',  ( 4.589221341884758942, 6.929947237659640713, 1.197292633685101748 ) ) ;
#113846 = CARTESIAN_POINT ( 'NONE',  ( 8.595506201384004896, 12.01154575404795466, 1.082531754730546636 ) ) ;
#113847 = EDGE_LOOP ( 'NONE', ( #129209, #209937, #56920, #58690, #117637, #155235 ) ) ;
#113848 = CARTESIAN_POINT ( 'NONE',  ( 3.138934141195717675, -0.1340819638860979157, -1.856265897873999426 ) ) ;
#113849 = CIRCLE ( 'NONE', #131152, 11.99999999999999112 ) ;
#113850 = CARTESIAN_POINT ( 'NONE',  ( 0.9662486314009374189, -1.869180826568194398, -0.4184218257623931181 ) ) ;
#113851 = CARTESIAN_POINT ( 'NONE',  ( 6.739296538182359519, -1.720230304288400625, 0.8672215684524892110 ) ) ;
#113852 = CARTESIAN_POINT ( 'NONE',  ( -1.890105089649204206, 8.991484090553308661, 0.7750000000000013545 ) ) ;
#113853 = ADVANCED_FACE ( 'NONE', ( #95733 ), #115216, .T. ) ;
#113854 = CARTESIAN_POINT ( 'NONE',  ( 4.664027441776592120, 8.287593892024585074, -0.5126927951675692707 ) ) ;
#113855 = FILL_AREA_STYLE_COLOUR ( '', #60697 ) ;
#113856 = CARTESIAN_POINT ( 'NONE',  ( -3.145128448690323264, 4.692402494937224056, -1.443375672974059665 ) ) ;
#113857 = CARTESIAN_POINT ( 'NONE',  ( 9.110716038703335684, 9.731516254683127087, -0.7216878364870197293 ) ) ;
#113858 = CARTESIAN_POINT ( 'NONE',  ( 4.768383308330760961, -0.8382467442454040185, -1.782262242837754807 ) ) ;
#113859 = CARTESIAN_POINT ( 'NONE',  ( 1.946092837771850492, -1.387361170020007695, -1.603719225630481970 ) ) ;
#113860 = CARTESIAN_POINT ( 'NONE',  ( -4.205000198532790279, 8.057583998263570635, 0.7998128361456341429 ) ) ;
#113861 = CARTESIAN_POINT ( 'NONE',  ( -11.86161086955307198, 8.823445149503903906, 1.515882294691715204 ) ) ;
#113862 = CARTESIAN_POINT ( 'NONE',  ( 4.095971805104268171, 7.792734516014752977, 0.7216878364870203955 ) ) ;
#113863 = CARTESIAN_POINT ( 'NONE',  ( 5.525378525699438548, -1.388074942811763357, -1.695776126864618316 ) ) ;
#113864 = CARTESIAN_POINT ( 'NONE',  ( 4.700175447307747945, -1.925963193209312418, -0.04779502591981815707 ) ) ;
#113865 = CARTESIAN_POINT ( 'NONE',  ( -5.520141099058386125, 9.591915048876776595, 0.000000000000000000 ) ) ;
#113866 = CARTESIAN_POINT ( 'NONE',  ( 0.5162701059127188241, 1.262803565755654001, -1.318596375272471199 ) ) ;
#113867 = CARTESIAN_POINT ( 'NONE',  ( 1.243116305521356990, 0.4334984505205765060, 2.163720904216937857 ) ) ;
#113868 = CARTESIAN_POINT ( 'NONE',  ( -6.001249869575842943, 7.094842513680024609, 1.067311936143347406 ) ) ;
#113869 = CARTESIAN_POINT ( 'NONE',  ( 0.01762790050853849447, -0.5081247445114078776, 1.843608005305336528 ) ) ;
#113870 = VERTEX_POINT ( 'NONE', #15494 ) ;
#113871 = CARTESIAN_POINT ( 'NONE',  ( 1.499999999999996891, 10.67708333401613530, -0.8660254037844378194 ) ) ;
#113872 = EDGE_LOOP ( 'NONE', ( #159386, #164266, #111463, #10119, #36712 ) ) ;
#113873 = CARTESIAN_POINT ( 'NONE',  ( 6.508657463561863921, 0.6146053541861602465, 1.871187945041019152 ) ) ;
#113874 = CARTESIAN_POINT ( 'NONE',  ( 2.032666248472639214, -1.733752323498815029, 0.8752225562490000277 ) ) ;
#113875 = CARTESIAN_POINT ( 'NONE',  ( 6.345094440775825184, -1.237889906630392334, 1.936425090000978289 ) ) ;
#113877 = CARTESIAN_POINT ( 'NONE',  ( 5.735155330654303718, -0.04388460642621531960, -1.860581820771879835 ) ) ;
#113876 = CARTESIAN_POINT ( 'NONE',  ( -6.631873415740034083, 7.766215735565355160, 1.199719254218452047 ) ) ;
#113878 = CARTESIAN_POINT ( 'NONE',  ( 5.794130544993763898, 7.853181283949808744, 1.599625672291269396 ) ) ;
#113879 = CARTESIAN_POINT ( 'NONE',  ( 9.093502852636627054, 1.000000000000000888, 7.666967846417570343 ) ) ;
#113880 = CARTESIAN_POINT ( 'NONE',  ( 3.791513125430877373, 7.352524219418101303, -0.3677586026353037996 ) ) ;
#113881 = CARTESIAN_POINT ( 'NONE',  ( -6.338600509588822263, 7.353787668397130162, -1.199719254218446718 ) ) ;
#113882 = CARTESIAN_POINT ( 'NONE',  ( -6.668631453075260396, 8.873432343378178544, -1.599625672291271394 ) ) ;
#113883 = CARTESIAN_POINT ( 'NONE',  ( 1.048660896456204528, -1.724490848714568259, 1.352309724062021878 ) ) ;
#113884 = CARTESIAN_POINT ( 'NONE',  ( 3.714570900464274850, 6.317121236308204324, 1.082531754730558626 ) ) ;
#113885 = CIRCLE ( 'NONE', #127661, 2.000000000000000000 ) ;
#113886 = CARTESIAN_POINT ( 'NONE',  ( 10.85353573482940526, -6.836568542494932288, -0.4635785636673656063 ) ) ;
#113887 = CARTESIAN_POINT ( 'NONE',  ( -4.370663978927099791, 5.060324124126027279, 7.500000000000000000 ) ) ;
#113888 = CARTESIAN_POINT ( 'NONE',  ( 1.857752496991037061, 1.820901040755190214, -0.1330985588276211995 ) ) ;
#113889 = CARTESIAN_POINT ( 'NONE',  ( -0.4702634422557508409, 7.494255424136805566, 4.464191613400292802 ) ) ;
#113890 = CARTESIAN_POINT ( 'NONE',  ( -6.555587544261016753, 6.796970737185429989, -0.4399619850315484859 ) ) ;
#113891 = CARTESIAN_POINT ( 'NONE',  ( 6.609000000000018638, 2.976782768882420438, 2.353557172130323227 ) ) ;
#113892 = EDGE_CURVE ( 'NONE', #148658, #1199, #70415, .T. ) ;
#113893 = CARTESIAN_POINT ( 'NONE',  ( 9.890836756369282057, 11.49806328964105617, -1.199719254218440723 ) ) ;
#113894 = CARTESIAN_POINT ( 'NONE',  ( 6.621730190220365131, -1.769489810573118049, 0.4491385735008179836 ) ) ;
#113895 = CARTESIAN_POINT ( 'NONE',  ( 4.205873059901494848, 0.6649649114027419428, -1.845726756006949909 ) ) ;
#113896 = CIRCLE ( 'NONE', #196832, 10.99999999999718980 ) ;
#113897 = CARTESIAN_POINT ( 'NONE',  ( -6.855619230004478482, 11.14997286831390788, -0.7998128361456291469 ) ) ;
#113898 = CARTESIAN_POINT ( 'NONE',  ( 6.959412922516382771, 7.013736585890911535, 0.7998128361456341429 ) ) ;
#113899 = CARTESIAN_POINT ( 'NONE',  ( 4.388337494309430653, -0.4807229498768311182, -2.138019847805587403 ) ) ;
#113900 = CARTESIAN_POINT ( 'NONE',  ( 4.741601036477289810, 6.554953847355395880, 1.599625672291267175 ) ) ;
#113901 = CARTESIAN_POINT ( 'NONE',  ( 4.258688845354158481, -0.6446009455991276171, -1.967446834807617284 ) ) ;
#113903 = CARTESIAN_POINT ( 'NONE',  ( -1.364683531250012516, 1.842708333674749843, 0.7879004041258379498 ) ) ;
#113902 = CYLINDRICAL_SURFACE ( 'NONE', #71942, 0.07999999999999998779 ) ;
#113904 = ORIENTED_EDGE ( 'NONE', *, *, #42520, .T. ) ;
#113905 = CARTESIAN_POINT ( 'NONE',  ( 4.061395409788411293, -1.323216277904919691, 1.879509618897465817 ) ) ;
#113906 = CARTESIAN_POINT ( 'NONE',  ( 7.700668062882064291, 10.00719871149432549, -1.443375672974057666 ) ) ;
#113908 = CARTESIAN_POINT ( 'NONE',  ( 3.285556943750000514, -0.3135416661887098777, 1.896917185911906500 ) ) ;
#113907 = CARTESIAN_POINT ( 'NONE',  ( 6.590672070018850803, 7.822110515511036866, -1.082531754730548412 ) ) ;
#113909 = CARTESIAN_POINT ( 'NONE',  ( 6.620655732516644854, 2.103946135090263514, 2.037628900882877847 ) ) ;
#113910 = CARTESIAN_POINT ( 'NONE',  ( -0.4635785636673758758, -6.836568542495036205, -10.85353573482950829 ) ) ;
#113911 = CARTESIAN_POINT ( 'NONE',  ( 3.679572934066538181, -0.9564393601015194202, 1.690012426612282681 ) ) ;
#113912 = ORIENTED_EDGE ( 'NONE', *, *, #20338, .T. ) ;
#113913 = CARTESIAN_POINT ( 'NONE',  ( 9.910647101465253073, 11.62513837554007168, -1.082531754730537088 ) ) ;
#113914 = CARTESIAN_POINT ( 'NONE',  ( 3.656429697474584017, 1.903630103707624865, 0.1825790434749063051 ) ) ;
#113915 = CARTESIAN_POINT ( 'NONE',  ( 0.000000000000000000, 1.000000000000000888, 0.000000000000000000 ) ) ;
#113916 = CARTESIAN_POINT ( 'NONE',  ( 5.719686907728898539, -1.681737053624256628, 0.3821217278023018582 ) ) ;
#113917 = CARTESIAN_POINT ( 'NONE',  ( 4.030482632556767975, 0.5424685788828055300, 1.942097399793737411 ) ) ;
#113918 = CARTESIAN_POINT ( 'NONE',  ( 4.606216143772843274, -0.1140155944862955434, 2.295953707746749117 ) ) ;
#113919 = CARTESIAN_POINT ( 'NONE',  ( 4.907688418466886304, 5.788353245375237321, -1.082531754730548412 ) ) ;
#113920 = CARTESIAN_POINT ( 'NONE',  ( 1.155211076828046579, -1.737760091701185505, 1.360235214042208263 ) ) ;
#113922 = CARTESIAN_POINT ( 'NONE',  ( -4.990809943606281607, 6.915973915664348937, -1.443375672974066548 ) ) ;
#113921 = CARTESIAN_POINT ( 'NONE',  ( -10.32861409551237486, 10.94447128771960287, 1.040834085586084257E-14 ) ) ;
#113923 = CARTESIAN_POINT ( 'NONE',  ( 5.993352163831329626, 1.341162022463908032, 1.154712335393495160 ) ) ;
#113925 = CARTESIAN_POINT ( 'NONE',  ( 1.641004737452517626, -1.934627630680013199, 1.229243952562808939 ) ) ;
#113924 = CARTESIAN_POINT ( 'NONE',  ( 5.037736595929563244, 8.035053907629919223, -1.199719254218452047 ) ) ;
#113926 = CARTESIAN_POINT ( 'NONE',  ( 1.235833198037468827, 0.3363826672934740469, 1.707315539672292104 ) ) ;
#113927 = CARTESIAN_POINT ( 'NONE',  ( 0.000000000000000000, 15.00000000000000000, -12.18000000000000149 ) ) ;
#113928 = CARTESIAN_POINT ( 'NONE',  ( 0.7019813383442319310, -1.220362748482771487, -1.231932065070516558 ) ) ;
#113929 = CARTESIAN_POINT ( 'NONE',  ( -1.360316468750019991, 0.4218750003414165062, -4.336808689942017736E-14 ) ) ;
#113930 = CARTESIAN_POINT ( 'NONE',  ( -11.88234649872613602, 13.75660782916751579, -0.9090484974825174813 ) ) ;
#113931 = CARTESIAN_POINT ( 'NONE',  ( 1.100314673101766338, 0.8801652113111978482, -1.984954624234806175 ) ) ;
#113932 = CARTESIAN_POINT ( 'NONE',  ( 2.114470590943520634, 1.957170936680457052, 0.4852650170619755565 ) ) ;
#113933 = CARTESIAN_POINT ( 'NONE',  ( -0.7500000000000215383, 0.4729166673494850093, 1.299038105676659116 ) ) ;
#113934 = CARTESIAN_POINT ( 'NONE',  ( 0.1648913374791864117, -1.719061530832368234, -0.8695707864920312335 ) ) ;
#113936 = B_SPLINE_CURVE_WITH_KNOTS ( 'NONE', 3,
 ( #87033, #36137, #4680, #182383, #167226, #17735 ),
 .UNSPECIFIED., .F., .F.,
 ( 4, 2, 4 ),
 ( 0.000000000000000000, 0.0003157158648874031190, 0.0006314317297748062380 ),
 .UNSPECIFIED. ) ;
#113935 = CARTESIAN_POINT ( 'NONE',  ( -1.364683531250014514, 13.58854166700806587, -0.7879004041258335089 ) ) ;
#113937 = CARTESIAN_POINT ( 'NONE',  ( 1.828696429707490578, -1.052382519090878654, -1.956348917980913260 ) ) ;
#113938 = ORIENTED_EDGE ( 'NONE', *, *, #29580, .F. ) ;
#113939 = CARTESIAN_POINT ( 'NONE',  ( -9.578206935422358015, -9.907361015872668375, 0.1671882239541429838 ) ) ;
#113940 = CARTESIAN_POINT ( 'NONE',  ( -1.500000000000015099, -0.3708333333333105331, -0.8660254037844383745 ) ) ;
#113941 = CARTESIAN_POINT ( 'NONE',  ( 9.264299036839600987, 9.702770385934682551, -0.7998128361456281477 ) ) ;
#113942 = FILL_AREA_STYLE ('',( #46759 ) ) ;
#113943 = CARTESIAN_POINT ( 'NONE',  ( 5.583501753226309816, -0.7750115735715494836, 1.558442325393385897 ) ) ;
#113945 = EDGE_CURVE ( 'NONE', #54853, #2091, #1154, .T. ) ;
#113944 = CARTESIAN_POINT ( 'NONE',  ( 3.560947883890089649, 1.548132398191165882, -1.204989647596923730 ) ) ;
#113947 = CARTESIAN_POINT ( 'NONE',  ( -7.388830529767770550, 7.722649827591604677, 1.040834085586084257E-14 ) ) ;
#113946 = CARTESIAN_POINT ( 'NONE',  ( 2.835626683552519012, 6.459981564119914310, 0.000000000000000000 ) ) ;
#113948 = CARTESIAN_POINT ( 'NONE',  ( -1.446621748570337429, 4.325121051142003736, -0.4012476001784824331 ) ) ;
#113949 = CARTESIAN_POINT ( 'NONE',  ( 5.149841461411730492, 0.7164311094934887603, -2.146032026599023812 ) ) ;
#113950 = CARTESIAN_POINT ( 'NONE',  ( 1.275913394178169957, -2.012872700982801355, 0.4499014461352250360 ) ) ;
#113951 = CARTESIAN_POINT ( 'NONE',  ( -7.542413527904030524, 7.693903958843159252, 1.040834085586084257E-14 ) ) ;
#113952 = CARTESIAN_POINT ( 'NONE',  ( 1.991474686832030994, 1.968180706754483644, -1.115757519136374221 ) ) ;
#113953 = VERTEX_POINT ( 'NONE', #183342 ) ;
#113954 = CARTESIAN_POINT ( 'NONE',  ( -0.7500000000000006661, 1.389583334016154748, -1.299038105676652011 ) ) ;
#113955 = CARTESIAN_POINT ( 'NONE',  ( 2.864352374448192240, -1.292745417840788003, 1.352161534859085412 ) ) ;
#113956 = CARTESIAN_POINT ( 'NONE',  ( 1.336079928753497681, 0.5043104442001166143, -1.659204044645303355 ) ) ;
#113957 = CARTESIAN_POINT ( 'NONE',  ( 5.249643141573060667, 2.189086832579402842, -0.1069518675670885766 ) ) ;
#113958 = CARTESIAN_POINT ( 'NONE',  ( 6.598638948628339662, -0.6063221841578874116, -2.226463007350306444 ) ) ;
#113959 = CARTESIAN_POINT ( 'NONE',  ( 4.223607183596161718, -2.069420184152844566, 0.6248923283326962563 ) ) ;
#113960 = CARTESIAN_POINT ( 'NONE',  ( 4.206929537583108392, -0.3307808895044571651, 1.913420690662092305 ) ) ;
#113961 = CARTESIAN_POINT ( 'NONE',  ( -10.50487009249003378, 11.15010328419353947, 0.7998128361456462443 ) ) ;
#113962 = CARTESIAN_POINT ( 'NONE',  ( 6.362560269511371658, -1.322780316340057549, 1.322825847358683138 ) ) ;
#113963 = CARTESIAN_POINT ( 'NONE',  ( 1.843750000000001332, 1.895863743164127868, 0.7852924748298895086 ) ) ;
#113964 = CARTESIAN_POINT ( 'NONE',  ( 4.128212683569056018, 7.424016784313646866, 0.7064205832574363964 ) ) ;
#113965 = DIRECTION ( 'NONE',  ( -0.6507913734559640506, -0.7592566023653003482, 0.000000000000000000 ) ) ;
#113967 = EDGE_CURVE ( 'NONE', #126795, #196229, #19931, .T. ) ;
#113966 = CARTESIAN_POINT ( 'NONE',  ( 4.095971805104288599, 5.871996087412059140, 1.443375672974058777 ) ) ;
#113968 = CARTESIAN_POINT ( 'NONE',  ( 0.6801582343749952297, 2.807291667008070313, -1.178068619123883165 ) ) ;
#113969 = CARTESIAN_POINT ( 'NONE',  ( 5.537732479266092689, -1.587839044716709669, 1.242724925242834066 ) ) ;
#113970 = CARTESIAN_POINT ( 'NONE',  ( -9.829825065107822724, 11.42688298316931572, 1.199719254218462483 ) ) ;
#113971 = CARTESIAN_POINT ( 'NONE',  ( 8.555358625423188812, 9.940005470203933768, 1.199719254218462483 ) ) ;
#113972 = CARTESIAN_POINT ( 'NONE',  ( 2.680411860343932862, -0.4909739067630093379, -0.09999999999832692721 ) ) ;
#113974 = CARTESIAN_POINT ( 'NONE',  ( -4.163738354385607465, 7.871795561280641174, 0.001129208541240749085 ) ) ;
#113973 = CARTESIAN_POINT ( 'NONE',  ( 3.686012862905340803, -0.8985999850123352894, 1.589152278004740237 ) ) ;
#113975 = CARTESIAN_POINT ( 'NONE',  ( 11.92619526913699879, 10.19999999999999929, -1.328859060402686199 ) ) ;
#113976 = VERTEX_POINT ( 'NONE', #51221 ) ;
#113977 = CARTESIAN_POINT ( 'NONE',  ( -5.655159470231558849, 6.730679149092498648, 1.082531754730549078 ) ) ;
#113978 = FACE_OUTER_BOUND ( 'NONE', #158938, .T. ) ;
#113979 = CARTESIAN_POINT ( 'NONE',  ( -9.982881178363895103, 10.54111621771303753, 1.040834085586084257E-14 ) ) ;
#113980 = CARTESIAN_POINT ( 'NONE',  ( 6.463536886191197262, -1.623326069159360063, -1.201424211086026261 ) ) ;
#113981 = CARTESIAN_POINT ( 'NONE',  ( 0.6102159345307588412, -0.7594153588383574238, 1.980023364433493693 ) ) ;
#113982 = ORIENTED_EDGE ( 'NONE', *, *, #152126, .F. ) ;
#113983 = CARTESIAN_POINT ( 'NONE',  ( -4.936050443827081580, 7.916420063510339666, 1.199719254218452935 ) ) ;
#113984 = CARTESIAN_POINT ( 'NONE',  ( 4.111146893441827821, 5.819424013814004759, 1.599625672291267398 ) ) ;
#113985 = AXIS2_PLACEMENT_3D ( 'NONE', #3619, #134752, #18816 ) ;
#113986 = CARTESIAN_POINT ( 'NONE',  ( 6.754767742037871336, -1.594745458351163103, 1.305156173170081813 ) ) ;
#113987 = CARTESIAN_POINT ( 'NONE',  ( 0.000000000000000000, -0.5000000000000004441, 0.000000000000000000 ) ) ;
#113988 = EDGE_LOOP ( 'NONE', ( #143624, #30677 ) ) ;
#113989 = ORIENTED_EDGE ( 'NONE', *, *, #45431, .F. ) ;
#113990 = VERTEX_POINT ( 'NONE', #149792 ) ;
#113991 = CARTESIAN_POINT ( 'NONE',  ( -8.123306592882240551, 12.62894145833798376, 0.000000000000000000 ) ) ;
#113992 = CARTESIAN_POINT ( 'NONE',  ( -0.3282377607281447562, 0.3638354509981936991, 1.224999999999983658 ) ) ;
#113995 = ORIENTED_EDGE ( 'NONE', *, *, #101713, .F. ) ;
#113994 = DIRECTION ( 'NONE',  ( -0.000000000000000000, 1.000000000000000000, -0.000000000000000000 ) ) ;
#113993 = CARTESIAN_POINT ( 'NONE',  ( -6.168033539574333979, 6.160736982450306876, 0.7998128361456281477 ) ) ;
#113996 = CARTESIAN_POINT ( 'NONE',  ( 5.997720278586790243, 7.186234674792547850, 1.197368251494409286 ) ) ;
#113997 = CARTESIAN_POINT ( 'NONE',  ( 5.747422657745248742, -1.966344092054626680, -0.4444320411668146731 ) ) ;
#113998 = CARTESIAN_POINT ( 'NONE',  ( 5.226429366918344144, 0.1390423275269437320, 1.835946739075666745 ) ) ;
#113999 = CARTESIAN_POINT ( 'NONE',  ( 2.975845599428874610, 6.509329181731200009, 0.4525212045368381952 ) ) ;
#114000 = CARTESIAN_POINT ( 'NONE',  ( 3.036059619770274498, -1.550059391276232601, -1.709768245815939780 ) ) ;
#114001 = CARTESIAN_POINT ( 'NONE',  ( 7.028976294042106332, 7.165170195996068969, 0.000000000000000000 ) ) ;
#114002 = CARTESIAN_POINT ( 'NONE',  ( 6.028642311625867833, 2.081422104948245533, 0.5829617784755269927 ) ) ;
#114003 = CARTESIAN_POINT ( 'NONE',  ( 5.933664784275179294, 10.07435934829639912, -0.7998128361456291469 ) ) ;
#114004 = CARTESIAN_POINT ( 'NONE',  ( 1.048265877425518688, -1.530107816300673829, 1.195853197770081255 ) ) ;
#114005 = CARTESIAN_POINT ( 'NONE',  ( -4.029797971759847997, 5.724516938518342535, -1.599625672291256295 ) ) ;
#114006 = ORIENTED_EDGE ( 'NONE', *, *, #102642, .F. ) ;
#114007 = AXIS2_PLACEMENT_3D ( 'NONE', #114641, #115689, #33309 ) ;
#114008 = CARTESIAN_POINT ( 'NONE',  ( 4.640180047935675844, 0.006009439367033602396, -2.298542322207643984 ) ) ;
#114009 = CYLINDRICAL_SURFACE ( 'NONE', #103430, 0.07999999999999998779 ) ;
#114010 = CARTESIAN_POINT ( 'NONE',  ( -5.815521545619021460, 5.749472989502435460, -0.7998128361456362523 ) ) ;
#114011 = CARTESIAN_POINT ( 'NONE',  ( 4.240975883383619305, -1.627667033997456381, 0.9218181776217827528 ) ) ;
#114014 = CARTESIAN_POINT ( 'NONE',  ( -7.449279056065764237, 7.655523418356991350, 0.7998128361456341429 ) ) ;
#114013 = CARTESIAN_POINT ( 'NONE',  ( 1.499999999999989120, 0.3062500006828158816, 0.000000000000000000 ) ) ;
#114012 = CARTESIAN_POINT ( 'NONE',  ( 0.9668906521006037647, -1.505869814250645478, 1.178657042999963878 ) ) ;
#114015 = CARTESIAN_POINT ( 'NONE',  ( 2.561379550486083012, -1.920685204893451292, -1.086737900330703166 ) ) ;
#114016 = CARTESIAN_POINT ( 'NONE',  ( -1.533805080507057772, 8.737074443703342297, -2.508413646267452890 ) ) ;
#114017 = CARTESIAN_POINT ( 'NONE',  ( 2.920892028740289081, 5.495125569250587816, 1.199719254218452047 ) ) ;
#114018 = CARTESIAN_POINT ( 'NONE',  ( 6.658462837642799670, 7.901199744405670522, 1.082531754730549967 ) ) ;
#114019 = CARTESIAN_POINT ( 'NONE',  ( -2.761056838677368397, 6.372983411765559048, 0.7998128361456341429 ) ) ;
#114020 = CARTESIAN_POINT ( 'NONE',  ( -5.926322542504860458, 9.928143709648733051, -0.7216878364870338292 ) ) ;
#114021 = CARTESIAN_POINT ( 'NONE',  ( 1.510939727685528311, 1.736590689682067756, 0.9330581202648262629 ) ) ;
#114022 = CARTESIAN_POINT ( 'NONE',  ( 1.220229771213819481, -2.250799921053967090, 0.5081616799173671595 ) ) ;
#114023 = CARTESIAN_POINT ( 'NONE',  ( 1.926150285298435572, 1.005797860886543660, 1.684270608208485065 ) ) ;
#114024 = CARTESIAN_POINT ( 'NONE',  ( 5.453991371731997440, -0.7473993133914544895, 1.922551457666883401 ) ) ;
#114025 = CARTESIAN_POINT ( 'NONE',  ( 4.039966587192257208, 6.696749537490852333, 1.082531754730558626 ) ) ;
#114026 = ADVANCED_FACE ( 'NONE', ( #36019 ), #191497, .T. ) ;
#114027 = CARTESIAN_POINT ( 'NONE',  ( 6.391743074199808916, 6.421731439513382433, -0.7998128361456481317 ) ) ;
#114028 = ORIENTED_EDGE ( 'NONE', *, *, #106621, .F. ) ;
#114029 =( BOUNDED_CURVE ( )  B_SPLINE_CURVE ( 2, ( #55934, #171817, #43972, #9315, #204278, #172901, #88446, #141503, #173984 ),
 .UNSPECIFIED., .F., .T. ) 
 B_SPLINE_CURVE_WITH_KNOTS ( ( 3, 2, 2, 2, 3 ),
 ( 0.9553571428571427937, 0.9583333333333333703, 0.9642857142857143016, 0.9702380952380952328, 0.9732142857142856984 ),
 .UNSPECIFIED. ) 
 CURVE ( )  GEOMETRIC_REPRESENTATION_ITEM ( )  RATIONAL_B_SPLINE_CURVE ( ( 0.9330127018922194093, 0.9330127018922180770, 1.000000000000000000, 0.8660254037844387076, 1.000000000000000000, 0.8660254037844387076, 1.000000000000000000, 0.9330127018922194093, 0.9330127018922194093 ) ) 
 REPRESENTATION_ITEM ( '' )  );
#114030 = CARTESIAN_POINT ( 'NONE',  ( -0.6823417656249969321, 5.530208333674756283, -1.181850606188749264 ) ) ;
#114031 = CARTESIAN_POINT ( 'NONE',  ( -4.936355671280336921, 4.883780760425392664, 0.5269810592589857512 ) ) ;
#114032 = CARTESIAN_POINT ( 'NONE',  ( 3.294268137996273715, 5.826768013428865522, -1.082531754730543971 ) ) ;
#114033 = CARTESIAN_POINT ( 'NONE',  ( 0.3390589225593713674, -2.105617620008819468, -0.5285623031292383533 ) ) ;
#114035 = CARTESIAN_POINT ( 'NONE',  ( 6.374545129912787544, -0.09763137639631430664, -1.838803627010993313 ) ) ;
#114034 = CARTESIAN_POINT ( 'NONE',  ( 11.06305611892948448, 13.75761539554391533, 0.9079708613958296093 ) ) ;
#114036 = CARTESIAN_POINT ( 'NONE',  ( -1.926047848156435149, 3.520667328686782671, 0.3999999999999993006 ) ) ;
#114037 = CARTESIAN_POINT ( 'NONE',  ( -7.047919420689663816, -8.186910006423165242, 6.389500220311202128 ) ) ;
#114038 = CARTESIAN_POINT ( 'NONE',  ( 1.229531971273215341, -1.182229855178434930, -1.449605969065965949 ) ) ;
#114039 = AXIS2_PLACEMENT_3D ( 'NONE', #181584, #96114, #196786 ) ;
#114040 = CARTESIAN_POINT ( 'NONE',  ( 5.554052124568397808, 2.159397089200214559, -0.09991998142631913771 ) ) ;
#114041 = CARTESIAN_POINT ( 'NONE',  ( -5.511734814698080243, 6.408623376260899285, 1.272316098655206229 ) ) ;
#114042 = FACE_OUTER_BOUND ( 'NONE', #97492, .T. ) ;
#114043 = CARTESIAN_POINT ( 'NONE',  ( 0.6823417656249864960, -0.8239583329919114574, -1.181850606188749264 ) ) ;
#114044 = CARTESIAN_POINT ( 'NONE',  ( 1.928230879603441750, -0.9027140558476205445, -1.685813393195116694 ) ) ;
#114045 = CARTESIAN_POINT ( 'NONE',  ( 3.555294528146099697, 0.4307136429906773256, -1.716485385381610662 ) ) ;
#114046 = CARTESIAN_POINT ( 'NONE',  ( 0.9789966485893276671, -1.729064073676725544, -0.8170501332188941923 ) ) ;
#114048 = CARTESIAN_POINT ( 'NONE',  ( 4.974201611368001430, -1.901669438865726924, -0.2299391999119395624 ) ) ;
#114047 = CARTESIAN_POINT ( 'NONE',  ( 2.978798704061872193, -3.177366733903203233, -1.522944741273397407 ) ) ;
#114049 = VECTOR ( 'NONE', #75727, 1000.000000000000000 ) ;
#114050 = CARTESIAN_POINT ( 'NONE',  ( 6.232857221494619182, -1.869652508273983882, -0.6194465747909986275 ) ) ;
#114051 = CARTESIAN_POINT ( 'NONE',  ( 1.499999999999989120, 5.045833333333354709, -0.8660254037844323793 ) ) ;
#114052 = CARTESIAN_POINT ( 'NONE',  ( 1.230900525853476868, 1.420129835883350955, -1.575055732827963295 ) ) ;
#114053 = CARTESIAN_POINT ( 'NONE',  ( -9.499606442108964544, -9.900000000000005684, 0.08647222121513538362 ) ) ;
#114054 = CARTESIAN_POINT ( 'NONE',  ( 4.574985519202336981, -0.0001439422951596270033, -1.870836309977530920 ) ) ;
#114056 = ORIENTED_EDGE ( 'NONE', *, *, #21279, .T. ) ;
#114055 = CARTESIAN_POINT ( 'NONE',  ( 0.1526014871912773629, -1.468541917219987836, 1.084465738218153064 ) ) ;
#114058 = CARTESIAN_POINT ( 'NONE',  ( 4.664027441776592120, 8.287593892024585074, -0.5126927951675692707 ) ) ;
#114057 = CARTESIAN_POINT ( 'NONE',  ( 5.039771180630152614, -1.558841386063321455, -1.562417271110942307 ) ) ;
#114059 = PRESENTATION_LAYER_ASSIGNMENT (  '', '', ( #89724 ) ) ;
#114060 = CARTESIAN_POINT ( 'NONE',  ( -1.364683531250014514, -1.011458332991911568, -0.7879004041258359514 ) ) ;
#114061 = CARTESIAN_POINT ( 'NONE',  ( 1.592308366680051490, 1.018618965756763473, -1.793563681512408525 ) ) ;
#114062 = CARTESIAN_POINT ( 'NONE',  ( 5.126954644262057492, 9.133197518281081173, 0.7998128361456462443 ) ) ;
#114063 = CARTESIAN_POINT ( 'NONE',  ( -8.341290820905609138, 10.75459192918846618, 1.599625672291269396 ) ) ;
#114064 = CARTESIAN_POINT ( 'NONE',  ( 10.38962578677386084, 11.01565159419135043, 0.000000000000000000 ) ) ;
#114065 = CARTESIAN_POINT ( 'NONE',  ( -3.425644128314343728, -0.02016143452187105223, -0.4179710227418531598 ) ) ;
#114066 = CARTESIAN_POINT ( 'NONE',  ( 0.000000000000000000, 7.849261790823902629, 0.000000000000000000 ) ) ;
#114067 = CARTESIAN_POINT ( 'NONE',  ( 7.614839552730775729, 8.913009562054615031, 1.199719254218452047 ) ) ;
#114068 = VERTEX_POINT ( 'NONE', #186540 ) ;
#114069 = CARTESIAN_POINT ( 'NONE',  ( 3.754400092289136737, -2.067862582909282487, -0.1045053291982081939 ) ) ;
#114070 = CARTESIAN_POINT ( 'NONE',  ( -1.500000000000011324, 5.629166666666693963, -0.8660254037844313801 ) ) ;
#114071 = CARTESIAN_POINT ( 'NONE',  ( 1.106953007505812492, 1.637591863572019690, -1.411084338363017832 ) ) ;
#114072 = CARTESIAN_POINT ( 'NONE',  ( -5.056216892478136771, 7.878110338051091510, -1.109312559570382550 ) ) ;
#114073 = CARTESIAN_POINT ( 'NONE',  ( 2.156904581142269350, 0.4447176379400120672, 1.969927323211942083 ) ) ;
#114074 = CARTESIAN_POINT ( 'NONE',  ( -3.285556943750000070, -0.1112512837626866702, 0.000000000000000000 ) ) ;
#114075 = EDGE_CURVE ( 'NONE', #155317, #18633, #201611, .T. ) ;
#114076 = EDGE_LOOP ( 'NONE', ( #753, #183229, #61253, #90057 ) ) ;
#114078 = CARTESIAN_POINT ( 'NONE',  ( 8.609064354997688184, 9.146255957026539818, 1.040834085586084257E-14 ) ) ;
#114077 = CARTESIAN_POINT ( 'NONE',  ( 3.475000000000000533, -3.004166666666665542, 2.006292185433948827 ) ) ;
#114079 = CARTESIAN_POINT ( 'NONE',  ( 0.01291931824900593301, 14.54921173327639217, 11.96434918058137242 ) ) ;
#114080 = CARTESIAN_POINT ( 'NONE',  ( -5.628043163004235794, 5.738674243025936761, 0.7216878364870257245 ) ) ;
#114081 = CARTESIAN_POINT ( 'NONE',  ( 0.2511858651975951151, 0.1928294586405615574, -2.007256720055437871 ) ) ;
#114082 = CARTESIAN_POINT ( 'NONE',  ( 5.091441847573507040, -0.7891374179831471825, 2.044738775321436997 ) ) ;
#114083 = CARTESIAN_POINT ( 'NONE',  ( -0.7499999999999972244, 4.389583334016150751, -1.299038105676652899 ) ) ;
#114084 = CARTESIAN_POINT ( 'NONE',  ( 4.781465250580236415, 0.1816826923375300662, -1.903719681147630016 ) ) ;
#114085 = CARTESIAN_POINT ( 'NONE',  ( -4.776550190716183586, 4.467063398790632966, 1.214306433183764966E-14 ) ) ;
#114086 = ADVANCED_FACE ( 'NONE', ( #166033 ), #135678, .F. ) ;
#114087 = CARTESIAN_POINT ( 'NONE',  ( 4.812781342726850653, 8.558735966582574406, 0.7216878364870438212 ) ) ;
#114088 = CARTESIAN_POINT ( 'NONE',  ( 2.724232643812212196, 2.001515029240468646, 0.2440086781289458329 ) ) ;
#114089 = CARTESIAN_POINT ( 'NONE',  ( 1.364683531249997417, 12.29687500034139980, 2.602085213965210642E-15 ) ) ;
#114091 = CARTESIAN_POINT ( 'NONE',  ( -5.029148636026397945, 4.832037928311032182, 0.7998128361456281477 ) ) ;
#114090 = CARTESIAN_POINT ( 'NONE',  ( 0.02941885139840036759, -2.092310700284722103, 0.9370380844745775928 ) ) ;
#114092 = CARTESIAN_POINT ( 'NONE',  ( 4.102375631063598149, -0.5418327121037533889, -1.637530703111476305 ) ) ;
#114093 = CARTESIAN_POINT ( 'NONE',  ( 5.826972158823246595, 10.02016096192762085, -0.7998128361456481317 ) ) ;
#114094 = CARTESIAN_POINT ( 'NONE',  ( 3.602716132929354664, 5.226254793216122074, 1.599625672291267398 ) ) ;
#114095 = CARTESIAN_POINT ( 'NONE',  ( -6.710127771514629025, -7.162053774861991684, -6.725445687907746439 ) ) ;
#114096 = ORIENTED_EDGE ( 'NONE', *, *, #23441, .F. ) ;
#114097 = PLANE ( 'NONE',  #54555 ) ;
#114098 = VERTEX_POINT ( 'NONE', #157265 ) ;
#114099 = CARTESIAN_POINT ( 'NONE',  ( 5.356058406599743194, 0.7285399314688314476, -1.658701577940960847 ) ) ;
#114100 = VERTEX_POINT ( 'NONE', #171360 ) ;
#114101 = CARTESIAN_POINT ( 'NONE',  ( 7.716561984472250835, 12.15440608185967086, 1.040834085586084257E-14 ) ) ;
#114102 = CARTESIAN_POINT ( 'NONE',  ( 4.854701522145073334, 7.821512988214679218, -1.199719254218450271 ) ) ;
#114103 = CARTESIAN_POINT ( 'NONE',  ( -11.07790593930098311, 13.79999999999999893, 0.6999999999999992895 ) ) ;
#114104 = CARTESIAN_POINT ( 'NONE',  ( 5.707607943424125807, 1.375951858612366019, 1.178334608346263579 ) ) ;
#114105 = CARTESIAN_POINT ( 'NONE',  ( 7.471952054462756010, 7.889901283060952508, 0.7216878364870267237 ) ) ;
#114106 = CARTESIAN_POINT ( 'NONE',  ( 2.277964293776285842, 5.617064315955532905, -0.5754907707892011892 ) ) ;
#114107 = CARTESIAN_POINT ( 'NONE',  ( 3.275498427308475069, 1.390425696708731396, 1.693851754907250928 ) ) ;
#114109 = CARTESIAN_POINT ( 'NONE',  ( 8.727698198895078363, 11.20540053684285553, -1.599625672291257406 ) ) ;
#114108 = CARTESIAN_POINT ( 'NONE',  ( 5.758217292028081857, -1.861241882002647285, 0.0004304118630827496474 ) ) ;
#114110 = CARTESIAN_POINT ( 'NONE',  ( 3.919475720687201736, -1.323675617205988475, -1.384941642318695987 ) ) ;
#114111 = CYLINDRICAL_SURFACE ( 'NONE', #76587, 10.99999999999999112 ) ;
#114112 = EDGE_CURVE ( 'NONE', #115710, #73128, #132788, .T. ) ;
#114113 = CARTESIAN_POINT ( 'NONE',  ( -3.602337597214539753E-15, 12.06250000000000178, 1.500000000000001554 ) ) ;
#114114 = CARTESIAN_POINT ( 'NONE',  ( 1.364683531249988757, 0.1343750003414204142, 0.000000000000000000 ) ) ;
#114115 = CARTESIAN_POINT ( 'NONE',  ( 5.504247177468179153, 7.444707678511436555, 1.443375672974062551 ) ) ;
#114116 = CARTESIAN_POINT ( 'NONE',  ( -9.490344339885981029, 10.17441593939621924, -0.7216878364870267237 ) ) ;
#114118 = CARTESIAN_POINT ( 'NONE',  ( 0.3214396764580421118, -0.1044536432763705502, 2.159311484102262479 ) ) ;
#114117 = B_SPLINE_CURVE_WITH_KNOTS ( 'NONE', 3,
 ( #10116, #55671, #72975, #76191, #107699, #202968, #54608, #25302, #121827, #105519 ),
 .UNSPECIFIED., .F., .F.,
 ( 4, 3, 3, 4 ),
 ( 1.053630326498184013E-17, 4.407003120538926870E-05, 8.609159171476572650E-05, 0.0001625397904729946610 ),
 .UNSPECIFIED. ) ;
#114119 = CARTESIAN_POINT ( 'NONE',  ( -6.134138155540168391, 6.121192367743780949, 0.000000000000000000 ) ) ;
#114120 = CARTESIAN_POINT ( 'NONE',  ( 4.228163802615382494, 6.026220084508304708, -1.599625672291269396 ) ) ;
#114121 = CARTESIAN_POINT ( 'NONE',  ( 2.520284954824199453, 1.194270260598716771, -1.380820861806408617 ) ) ;
#114122 = CARTESIAN_POINT ( 'NONE',  ( -2.767835915484202047, 6.380892334706859792, -0.7998128361456281477 ) ) ;
#114123 = CARTESIAN_POINT ( 'NONE',  ( 4.014527796464135712, 1.291161025869846712, -1.290856679043244970 ) ) ;
#114124 = CARTESIAN_POINT ( 'NONE',  ( 9.542125166518260926, 12.19240180423196485, 8.745854086120228743 ) ) ;
#114125 = ORIENTED_EDGE ( 'NONE', *, *, #186592, .F. ) ;
#114126 = CARTESIAN_POINT ( 'NONE',  ( 3.684007040126308752, -1.171275171843730867, -1.583282632743492790 ) ) ;
#114127 = ORIENTED_EDGE ( 'NONE', *, *, #510, .T. ) ;
#114128 = CARTESIAN_POINT ( 'NONE',  ( 4.634287131779754709, 0.3355949523314147309, 1.912704035658734592 ) ) ;
#114129 = ORIENTED_EDGE ( 'NONE', *, *, #154365, .F. ) ;
#114130 = CARTESIAN_POINT ( 'NONE',  ( -7.045397100956844127, 8.248660034984974132, -1.199719254218452047 ) ) ;
#114132 = CARTESIAN_POINT ( 'NONE',  ( 5.502226937873657242, -0.9515977829631333540, 1.895136135177949877 ) ) ;
#114131 = CARTESIAN_POINT ( 'NONE',  ( 7.015418140428412386, 7.149352350113456822, 0.7998128361456331437 ) ) ;
#114133 = CARTESIAN_POINT ( 'NONE',  ( -4.613268803136618246, 8.378775596900176481, 0.2107346534404584415 ) ) ;
#114134 = CARTESIAN_POINT ( 'NONE',  ( 2.596233987490266681, -0.9813665562012074961, 1.641104690102652919 ) ) ;
#114135 = CARTESIAN_POINT ( 'NONE',  ( 5.506841003474272966, 6.417672382999444203, -1.246111810019270738 ) ) ;
#114136 = DIRECTION ( 'NONE',  ( -1.000000000000000000, 5.578564026256490882E-16, -1.264049978315544409E-61 ) ) ;
#114137 = CARTESIAN_POINT ( 'NONE',  ( 3.528865121306874464, 7.339036084825155015, -0.7998128361456362523 ) ) ;
#114138 = CIRCLE ( 'NONE', #145178, 1.962502847949850526 ) ;
#114139 = CARTESIAN_POINT ( 'NONE',  ( 4.600248117428091810, -0.9470982757478171310, 1.776368884175743235 ) ) ;
#114140 = CARTESIAN_POINT ( 'NONE',  ( 0.08228926980217896037, -9.910743320677063650, 9.499643698783458490 ) ) ;
#114141 = CARTESIAN_POINT ( 'NONE',  ( 4.934128534657983067, 0.9357288403324083292, -1.567518238613223813 ) ) ;
#114142 = CARTESIAN_POINT ( 'NONE',  ( 0.3442982867475213871, -0.9772804826688463731, 1.825211318103404867 ) ) ;
#114143 = CARTESIAN_POINT ( 'NONE',  ( -7.049876689426103127, 10.20831132343037062, -1.082531754730537976 ) ) ;
#114144 = CARTESIAN_POINT ( 'NONE',  ( -5.873358954868365345, 7.276917811852929852, 1.275545277584020365 ) ) ;
#114145 = CARTESIAN_POINT ( 'NONE',  ( -0.4499999960735077686, 3.999999999999980904, -0.9281957781481916525 ) ) ;
#114146 = CARTESIAN_POINT ( 'NONE',  ( 6.069203928793593050, 0.1358119448514639727, -1.865795782587629681 ) ) ;
#114147 = CARTESIAN_POINT ( 'NONE',  ( 6.693975156845185737, 8.832723654451292816, 1.599625672291281386 ) ) ;
#114148 = CARTESIAN_POINT ( 'NONE',  ( -3.249150368769345043, 6.942425863539538611, 0.7998128361456341429 ) ) ;
#114149 = CARTESIAN_POINT ( 'NONE',  ( 2.517010073631369860, 6.088262185878572375, -0.7998128361456281477 ) ) ;
#114150 = CARTESIAN_POINT ( 'NONE',  ( 0.6823417656249969321, 10.33854166700806587, -1.181850606188757036 ) ) ;
#114151 = CARTESIAN_POINT ( 'NONE',  ( -4.062639585589296942, 7.891496616496157301, 0.7998128361456341429 ) ) ;
#114153 = CARTESIAN_POINT ( 'NONE',  ( -4.136646265500970365, 5.919449624541475607, -1.443375672974066548 ) ) ;
#114152 = DIRECTION ( 'NONE',  ( 1.000000000000000000, -0.000000000000000000, -0.000000000000000000 ) ) ;
#114154 = AXIS2_PLACEMENT_3D ( 'NONE', #176613, #63917, #130073 ) ;
#114155 = CARTESIAN_POINT ( 'NONE',  ( -5.311043488251275591, 7.219303374425030562, -1.599625672291256295 ) ) ;
#114156 = CARTESIAN_POINT ( 'NONE',  ( 0.9892257793299992219, 0.1485654903058269416, 2.064951490685583924 ) ) ;
#114157 = CARTESIAN_POINT ( 'NONE',  ( 1.880608475893473353, -0.5680388087716014001, -2.039528425668888811 ) ) ;
#114158 = CARTESIAN_POINT ( 'NONE',  ( 7.377608144130607393, 11.75895993479440982, -0.7998128361456291469 ) ) ;
#114159 = CARTESIAN_POINT ( 'NONE',  ( 1.068589661201713072E-16, 3.400000000000000355, -1.925000000000005818 ) ) ;
#114160 = CARTESIAN_POINT ( 'NONE',  ( 0.7780955915308949145, -1.048793665676364562, -1.666747765972796946 ) ) ;
#114161 = CARTESIAN_POINT ( 'NONE',  ( 4.849937260509308956, 6.926242028416789154, 1.417063245053858722 ) ) ;
#114162 = CARTESIAN_POINT ( 'NONE',  ( 4.609409038966229666, 6.400729850259146758, -1.443375672974051449 ) ) ;
#114164 = DIRECTION ( 'NONE',  ( 1.000000000000000000, -5.782411586589355667E-16, 0.000000000000000000 ) ) ;
#114163 = CARTESIAN_POINT ( 'NONE',  ( 0.000000000000000000, -2.887499999999999289, -4.012584370867899430 ) ) ;
#114165 = CARTESIAN_POINT ( 'NONE',  ( 2.502247188656173016, -0.8787990176886916194, -2.117303525603573267 ) ) ;
#114166 = CARTESIAN_POINT ( 'NONE',  ( 1.066719475142904994, -1.649486405746130258, -0.7827983987617056494 ) ) ;
#114167 = CARTESIAN_POINT ( 'NONE',  ( 2.056764645581514728, 0.4224895836346024280, 1.864965418913032913 ) ) ;
#114168 = VERTEX_POINT ( 'NONE', #189738 ) ;
#114169 = CARTESIAN_POINT ( 'NONE',  ( 8.066738210006692000, 8.513542121203711233, 0.7216878364870458196 ) ) ;
#114170 = CARTESIAN_POINT ( 'NONE',  ( 1.371341259694250247, -1.728764894987804057, -1.031425992479652720 ) ) ;
#114171 = CARTESIAN_POINT ( 'NONE',  ( 1.129655866247070595, 1.892139549451707037, -0.5178372573612434193 ) ) ;
#114172 = CARTESIAN_POINT ( 'NONE',  ( -7.960608749518247151, 12.43912730774665576, 0.000000000000000000 ) ) ;
#114173 = CARTESIAN_POINT ( 'NONE',  ( -5.865874016206865882, 9.995270118883347266, 0.000000000000000000 ) ) ;
#114174 = CARTESIAN_POINT ( 'NONE',  ( -7.721398836998398352, -5.907420853759296264, -7.721398836998357496 ) ) ;
#114176 = CARTESIAN_POINT ( 'NONE',  ( 2.008344819247428248, 1.313797796480600244, -1.186068062872788209 ) ) ;
#114175 = CARTESIAN_POINT ( 'NONE',  ( 4.347661206880347073, 2.090185315053775472, -0.05106478779118817091 ) ) ;
#114177 = CARTESIAN_POINT ( 'NONE',  ( -1.420000000000001039, 6.280000000000042881, -2.873333333333329520 ) ) ;
#114179 = CARTESIAN_POINT ( 'NONE',  ( 5.244168061255013669, 0.6613091839676830119, 2.194790591360805898 ) ) ;
#114178 = CARTESIAN_POINT ( 'NONE',  ( -11.82533409993242834, 7.631798484810768279, 2.053971879869906036 ) ) ;
#114180 = CARTESIAN_POINT ( 'NONE',  ( 4.997892061590047952, -0.5910035050068825901, -1.637047790839076589 ) ) ;
#114181 = CARTESIAN_POINT ( 'NONE',  ( 10.06423010004587759, 10.63602329300870153, 0.000000000000000000 ) ) ;
#114182 = CARTESIAN_POINT ( 'NONE',  ( 4.165211049733441584, -0.5436426828948260903, -1.646488866570811060 ) ) ;
#114183 = CARTESIAN_POINT ( 'NONE',  ( 4.193918837840154623, -1.494357529231920889, -1.575321265833210305 ) ) ;
#114184 = CARTESIAN_POINT ( 'NONE',  ( 4.359110081993588182, 5.044382169536003602, -1.199719254218452047 ) ) ;
#114185 = CARTESIAN_POINT ( 'NONE',  ( 6.122279814772176643, 1.995267444086584296, 0.2910868170948808786 ) ) ;
#114186 = CARTESIAN_POINT ( 'NONE',  ( 1.156250000000000888, -1.895863743164063031, 0.7852924748300492697 ) ) ;
#114187 = CARTESIAN_POINT ( 'NONE',  ( -0.7499999999999972244, 5.139583334016151639, -1.299038105676652899 ) ) ;
#114188 = CARTESIAN_POINT ( 'NONE',  ( 3.750929837476246753, -1.575545889128293853, 1.108190883620339795 ) ) ;
#114189 = CARTESIAN_POINT ( 'NONE',  ( 1.499999999999993117, 10.38541666734946212, 0.8660254037844409281 ) ) ;
#114190 = CARTESIAN_POINT ( 'NONE',  ( 5.818639523836858451, -0.7989930759073891053, -2.072897825184773168 ) ) ;
#114191 = EDGE_LOOP ( 'NONE', ( #126780, #211041, #135081, #111501 ) ) ;
#114192 = CARTESIAN_POINT ( 'NONE',  ( 6.983263157960378997, 2.960795523694306652, 2.498903865360342369 ) ) ;
#114193 = CARTESIAN_POINT ( 'NONE',  ( -1.201851678989727383E-14, 3.337500000000019007, -1.732050807568863648 ) ) ;
#114194 = CARTESIAN_POINT ( 'NONE',  ( 4.137209430464448445, 7.978494768850520558, 1.040834085586084257E-14 ) ) ;
#114195 = CARTESIAN_POINT ( 'NONE',  ( 1.278328015487300462, 2.187630646761177466, -0.3845124374818161828 ) ) ;
#114198 = EDGE_CURVE ( 'NONE', #65494, #189704, #63500, .T. ) ;
#114197 = DIRECTION ( 'NONE',  ( 0.000000000000000000, 0.000000000000000000, 1.000000000000000000 ) ) ;
#114196 = CIRCLE ( 'NONE', #48436, 0.6500000000000000222 ) ;
#114199 = CARTESIAN_POINT ( 'NONE',  ( 7.537970219518073556, 9.817384560903001045, -1.443375672974057666 ) ) ;
#114200 = CARTESIAN_POINT ( 'NONE',  ( -9.937763408692596556, 11.65677406730528887, -1.082531754730537976 ) ) ;
#114201 = CARTESIAN_POINT ( 'NONE',  ( 3.390420931869152721, 6.113185632892752075, -1.199719254218452047 ) ) ;
#114202 = CARTESIAN_POINT ( 'NONE',  ( -3.851925040058345573, 5.587274861525073355, -1.443375672974078761 ) ) ;
#114204 = CARTESIAN_POINT ( 'NONE',  ( 4.475086314992714698, 1.884572246790953365, 0.8388810360253369236 ) ) ;
#114203 = CARTESIAN_POINT ( 'NONE',  ( -3.189213936345670852, 2.817530495244580102, -2.450448857954567572 ) ) ;
#114205 = CARTESIAN_POINT ( 'NONE',  ( -4.172158584703340445, 5.890604320285754980, -1.599625672291256295 ) ) ;
#114206 = CARTESIAN_POINT ( 'NONE',  ( -1.500000000000011324, 4.660416667349484676, -0.8660254037844313801 ) ) ;
#114207 = CARTESIAN_POINT ( 'NONE',  ( -1.402160292154681736E-14, -0.4281249996585808071, 1.575800808251672791 ) ) ;
#114208 = CARTESIAN_POINT ( 'NONE',  ( 0.5964902553294594290, 1.476022596236561846, -0.9760666246667221158 ) ) ;
#114209 = CARTESIAN_POINT ( 'NONE',  ( 5.309090426574582189, 1.026673973311197585, -1.397408945856312590 ) ) ;
#114210 = CARTESIAN_POINT ( 'NONE',  ( 4.651753270297207976, 0.6719488171132372845, 1.605710474869048499 ) ) ;
#114211 = CARTESIAN_POINT ( 'NONE',  ( 4.090809663021327758, 5.795697244990093644, 1.599625672291267398 ) ) ;
#114212 = CARTESIAN_POINT ( 'NONE',  ( 2.806493257264990326, 1.658461721128750677, -1.582772817771603169 ) ) ;
#114213 = CARTESIAN_POINT ( 'NONE',  ( -0.6823417656250212460, 4.863541667008086655, 1.181850606188767472 ) ) ;
#114214 = CARTESIAN_POINT ( 'NONE',  ( 1.482094074889642288, -0.2687121449159133313, -1.821302815977184686 ) ) ;
#114215 = CARTESIAN_POINT ( 'NONE',  ( 1.500000000000007105, 10.64264068711930733, 1.214306433183764966E-14 ) ) ;
#114216 = CARTESIAN_POINT ( 'NONE',  ( 1.535882326342351334, 0.9031702520058831896, -1.586444745400449108 ) ) ;
#114217 = CARTESIAN_POINT ( 'NONE',  ( 2.549454116737331244, -1.388485404012842261, 1.462446031800922253 ) ) ;
#114218 = CARTESIAN_POINT ( 'NONE',  ( 1.500213180713722450, -0.7911926984936793472, -2.043816727864488314 ) ) ;
#114219 = CARTESIAN_POINT ( 'NONE',  ( 6.743451144134844810, 16.00000000000000000, -9.536680065235829673 ) ) ;
#114220 = CARTESIAN_POINT ( 'NONE',  ( 4.788165231579453618, -0.9949995658048852443, 1.856088619770781989 ) ) ;
#114221 = CARTESIAN_POINT ( 'NONE',  ( -6.256197817702116026, 9.386315656372753224, -1.199719254218440723 ) ) ;
#114222 = CARTESIAN_POINT ( 'NONE',  ( 8.344038675336102884, 13.15493340621088336, 8.539968482448076159 ) ) ;
#114223 = CARTESIAN_POINT ( 'NONE',  ( 1.240778115703184303, -2.019486815914430355, -0.4554155650244652853 ) ) ;
#114224 = CARTESIAN_POINT ( 'NONE',  ( 6.179819089730593795, 6.104210447640811665, 1.040834085586084257E-14 ) ) ;
#114225 = CARTESIAN_POINT ( 'NONE',  ( -1.752700365193352367E-14, -0.2656249996585993145, 1.570758158831780271 ) ) ;
#114226 = CARTESIAN_POINT ( 'NONE',  ( 3.229257539231108698, 1.917844101178723504, 0.9048822562475050679 ) ) ;
#114227 = CARTESIAN_POINT ( 'NONE',  ( 1.364683531249988757, 0.1343750003414204142, 0.000000000000000000 ) ) ;
#114228 = CARTESIAN_POINT ( 'NONE',  ( 6.709597972018079837, -0.3944863986210072060, 1.789098616620278470 ) ) ;
#114229 = EDGE_LOOP ( 'NONE', ( #21617, #143982, #133460, #112646, #8403 ) ) ;
#114230 = CARTESIAN_POINT ( 'NONE',  ( -4.956387674247580755, 7.940146832334256111, 1.199719254218452935 ) ) ;
#114231 = CARTESIAN_POINT ( 'NONE',  ( 9.236128959407556849, 11.79856975744075598, -1.599625672291262513 ) ) ;
#114232 = CARTESIAN_POINT ( 'NONE',  ( 5.302647476276220573, 8.240153584747313076, -1.082531754730548412 ) ) ;
#114233 = CARTESIAN_POINT ( 'NONE',  ( 1.737500000000001155, -1.939583332377418978, 3.009438278150922130 ) ) ;
#114234 = CARTESIAN_POINT ( 'NONE',  ( -5.717788096661253761, 7.693838750903348789, 1.599625672291269396 ) ) ;
#114235 = CARTESIAN_POINT ( 'NONE',  ( 3.041275741140234246, 0.05373089442234183638, 2.019258232931480546 ) ) ;
#114236 = CARTESIAN_POINT ( 'NONE',  ( 0.6750070354940709283, -1.982970624965023410, -0.7094951434080811747 ) ) ;
#114237 = CARTESIAN_POINT ( 'NONE',  ( -7.279802135894939852, 7.457800344824362604, -0.7998128361456362523 ) ) ;
#114238 = CARTESIAN_POINT ( 'NONE',  ( 8.320953590485093088, 10.73086516036454618, 1.599625672291281386 ) ) ;
#114239 = CARTESIAN_POINT ( 'NONE',  ( 5.471493298581291853, -0.2749614684036653656, 1.840407035693031546 ) ) ;
#114240 = CARTESIAN_POINT ( 'NONE',  ( 7.065770611016287006, 11.39514947949436774, 1.040834085586084257E-14 ) ) ;
#114241 = CARTESIAN_POINT ( 'NONE',  ( 4.894543267554960053, 4.887125941896303338, -0.6895117023006970269 ) ) ;
#114242 = CARTESIAN_POINT ( 'NONE',  ( -8.324343129110692630, 12.65555805069709550, 0.7216878364870338292 ) ) ;
#114243 = STYLED_ITEM ( 'NONE', ( #212687 ), #24096 ) ;
#114244 = CARTESIAN_POINT ( 'NONE',  ( -5.533699252672048985, 9.607732894759390518, -0.7998128361456231517 ) ) ;
#114245 = CARTESIAN_POINT ( 'NONE',  ( 6.438362351209899082, 2.038089008908655853, 0.3048918457534201543 ) ) ;
#114247 = CARTESIAN_POINT ( 'NONE',  ( -5.337630915675663168, 6.534101986612459001, 1.368282111488251074 ) ) ;
#114246 = CARTESIAN_POINT ( 'NONE',  ( -6.784929528996132220, 6.880448970109080520, 0.000000000000000000 ) ) ;
#114249 = EDGE_CURVE ( 'NONE', #131458, #39437, #106420, .T. ) ;
#114248 = CARTESIAN_POINT ( 'NONE',  ( -0.6823417656250003738, 0.2177083336747515085, -1.181850606188749264 ) ) ;
#114250 = CARTESIAN_POINT ( 'NONE',  ( 2.389626358114539162, -0.004507738041977306029, 1.734034291262590788 ) ) ;
#114251 = CARTESIAN_POINT ( 'NONE',  ( 0.8666887897643248406, 1.678224016273874852, -0.4604494717724941233 ) ) ;
#114253 = CARTESIAN_POINT ( 'NONE',  ( 6.480434237652115570, 10.50433101066207442, 0.7216878364870438212 ) ) ;
#114252 = CARTESIAN_POINT ( 'NONE',  ( 0.2535066641492569883, -1.850528970283831010, 1.378429844982787422 ) ) ;
#114254 = CARTESIAN_POINT ( 'NONE',  ( -10.90754186426655004, 4.636108433425617292, 4.485516275142084730 ) ) ;
#114255 = CARTESIAN_POINT ( 'NONE',  ( 2.284514177335088991, -2.020382039854185408, -0.4051362335234820478 ) ) ;
#114256 = CARTESIAN_POINT ( 'NONE',  ( 4.330940004561544043, 7.140181541042074365, -1.199719254218452047 ) ) ;
#114257 = CARTESIAN_POINT ( 'NONE',  ( 1.722029606037442040, -1.727736752315935265, -1.038835718801443653 ) ) ;
#114258 = DIRECTION ( 'NONE',  ( 0.000000000000000000, -1.000000000000000000, 0.000000000000000000 ) ) ;
#114259 = CARTESIAN_POINT ( 'NONE',  ( -6.069210040772897052, 7.109775131437022999, -1.199719254218453823 ) ) ;
#114260 = CARTESIAN_POINT ( 'NONE',  ( 1.340630715518615679, 0.3825088487559283323, 1.933841885654476567 ) ) ;
#114262 = CARTESIAN_POINT ( 'NONE',  ( -5.966997003790217136, 9.975597247814986801, -0.7216878364870338292 ) ) ;
#114261 = CARTESIAN_POINT ( 'NONE',  ( 4.886922752366290368, -1.802716094696995786, -0.6387714794457154399 ) ) ;
#114263 = B_SPLINE_CURVE_WITH_KNOTS ( 'NONE', 3,
 ( #55420, #89008, #72726, #138820, #204841, #122652, #7717, #143117, #142037, #94347, #174530, #208053, #26108, #124775, #173462, #62875, #129042, #127989 ),
 .UNSPECIFIED., .F., .F.,
 ( 4, 2, 2, 2, 2, 2, 2, 2, 4 ),
 ( 0.001640627021451589824, 0.001845642838648680652, 0.002050658655845771696, 0.002255674473042862307, 0.002460690290239953351, 0.002665706107437043962, 0.002870721924634134573, 0.003075737741831225183, 0.003280753559028315794 ),
 .UNSPECIFIED. ) ;
#114264 = CARTESIAN_POINT ( 'NONE',  ( 6.305322857734435793, 1.832379230283949667, 1.229636283518860118 ) ) ;
#114265 = CARTESIAN_POINT ( 'NONE',  ( -5.261973015435229328, 9.153069261400824885, 0.000000000000000000 ) ) ;
#114266 = CARTESIAN_POINT ( 'NONE',  ( 7.713663051532233972, 7.963971413067895355, -0.7998128361456341429 ) ) ;
#114267 = CARTESIAN_POINT ( 'NONE',  ( -6.688968683495758683, 8.897159112202094988, -1.599625672291271394 ) ) ;
#114268 = CARTESIAN_POINT ( 'NONE',  ( 0.5045642862554244878, -2.004696059604444081, -0.2448167134727705085 ) ) ;
#114269 = CARTESIAN_POINT ( 'NONE',  ( 4.243447643126375013, -2.009724547103900250, 1.133870999951855696 ) ) ;
#114270 = CARTESIAN_POINT ( 'NONE',  ( 6.268018250734934682, -1.947192974725008963, 0.2387856323943157166 ) ) ;
#114271 = CARTESIAN_POINT ( 'NONE',  ( 1.498799732657706718, 0.3773721054241683248, 1.924948185394937283 ) ) ;
#114272 = CARTESIAN_POINT ( 'NONE',  ( -4.911752498546916534, 4.707425932596564166, -0.3822207396134598145 ) ) ;
#114273 = CARTESIAN_POINT ( 'NONE',  ( -9.434262096661420571, 14.57949301904344885, 7.415936068925672586 ) ) ;
#114274 = ORIENTED_EDGE ( 'NONE', *, *, #134227, .T. ) ;
#114275 = CARTESIAN_POINT ( 'NONE',  ( 0.1283146926199127957, 2.112135570198115708, 0.1490006669643220705 ) ) ;
#114277 = CARTESIAN_POINT ( 'NONE',  ( -6.886651960737580680, 10.12184548991413457, -1.199719254218440723 ) ) ;
#114276 = CARTESIAN_POINT ( 'NONE',  ( -5.111587607552082524, 5.922272616020886282, 1.199719254218450271 ) ) ;
#114278 = CARTESIAN_POINT ( 'NONE',  ( 0.9195641160042143936, 1.098457714822091091, -1.477412082521646575 ) ) ;
#114279 = EDGE_LOOP ( 'NONE', ( #44912, #10650, #195307, #22091 ) ) ;
#114280 = CARTESIAN_POINT ( 'NONE',  ( 4.452125263715247527, -0.8365346480432279686, 2.003629037444945471 ) ) ;
#114281 = B_SPLINE_CURVE_WITH_KNOTS ( 'NONE', 3,
 ( #185658, #154251, #122913, #9059, #58878, #88180, #7976, #207251, #125034, #157464 ),
 .UNSPECIFIED., .F., .F.,
 ( 4, 2, 2, 2, 4 ),
 ( 0.000000000000000000, 0.0009122422346014731880, 0.001824484469202946376, 0.002736726703804419347, 0.003648968938405892752 ),
 .UNSPECIFIED. ) ;
#114282 = CARTESIAN_POINT ( 'NONE',  ( 11.09214416354366861, 9.059100286490975762, -4.456786335284255607 ) ) ;
#114283 = CARTESIAN_POINT ( 'NONE',  ( 1.476976393720278002, -1.495863523836362896, 1.503369785937097136 ) ) ;
#114284 = CARTESIAN_POINT ( 'NONE',  ( 0.7499999999999902300, 3.014583334016149418, 1.299038105676669330 ) ) ;
#114285 = CARTESIAN_POINT ( 'NONE',  ( 8.565000355531088516, 11.01558638625153286, -1.599625672291257406 ) ) ;
#114286 = CARTESIAN_POINT ( 'NONE',  ( -1.835699054053199664, 2.512084418327853008, -2.498041437723068636 ) ) ;
#114287 = CARTESIAN_POINT ( 'NONE',  ( 2.864585088123726919, -1.423607738919046906, 1.490243374215278971 ) ) ;
#114289 = CARTESIAN_POINT ( 'NONE',  ( 0.5382993156314471728, -1.579489783069366604, 0.9460463261394758128 ) ) ;
#114288 = CARTESIAN_POINT ( 'NONE',  ( -9.338868881714763148, 9.789768538289042255, -0.7998128361456291469 ) ) ;
#114290 = CARTESIAN_POINT ( 'NONE',  ( 0.6823417656249899377, 3.092708333674754062, 1.181850606188765695 ) ) ;
#114291 = CARTESIAN_POINT ( 'NONE',  ( 0.07775346131144718342, 5.719027203068962173, -2.882954358279002260 ) ) ;
#114292 = CARTESIAN_POINT ( 'NONE',  ( 1.436275828743645011, 4.080015253042389212, -0.4487520553618615793 ) ) ;
#114293 = DIRECTION ( 'NONE',  ( 0.000000000000000000, 0.000000000000000000, 1.000000000000000000 ) ) ;
#114294 = CARTESIAN_POINT ( 'NONE',  ( 1.458695031449417590, 0.9167444482420561425, 2.068505399879524642 ) ) ;
#114295 = CARTESIAN_POINT ( 'NONE',  ( -8.337901282724359930, 12.67137589657970409, 1.040834085586084257E-14 ) ) ;
#114296 = CARTESIAN_POINT ( 'NONE',  ( 1.160107992948592237, 1.809582681877516697, 0.08717244660690416647 ) ) ;
#114297 = CARTESIAN_POINT ( 'NONE',  ( 2.325271742496349159, -1.422496398144998508, -1.283381434195222326 ) ) ;
#114298 = CARTESIAN_POINT ( 'NONE',  ( 3.297389726143421740, -1.827171938055579536, 0.9735347560282039403 ) ) ;
#114299 = CARTESIAN_POINT ( 'NONE',  ( 0.6823417656249882723, 1.988541667008083991, -1.181850606188749264 ) ) ;
#114300 = CARTESIAN_POINT ( 'NONE',  ( 2.114083122616668309, -0.9278515453300213434, -1.739463596305758974 ) ) ;
#114301 = CARTESIAN_POINT ( 'NONE',  ( 5.320897925068237555, 1.780805307305334040, 0.7354040419824976471 ) ) ;
#114302 = TOROIDAL_SURFACE ( 'NONE', #86545, 0.8300000000000010703, 0.08000000000000000167 ) ;
#114304 = CARTESIAN_POINT ( 'NONE',  ( 6.176125489850557315, 6.957122458884915872, -0.8945188991977878201 ) ) ;
#114303 = CARTESIAN_POINT ( 'NONE',  ( 1.155362744787872931, -1.816424715318950112, 1.423309470994944537 ) ) ;
#114305 = CARTESIAN_POINT ( 'NONE',  ( 1.364683531249988535, 3.363541667008084879, 0.7879004041258500513 ) ) ;
#114306 = CARTESIAN_POINT ( 'NONE',  ( 4.984863162817260829, 1.972918577937707196, 0.6018043753471848945 ) ) ;
#114307 = CARTESIAN_POINT ( 'NONE',  ( -5.331380718671772101, 7.243030143248949670, -1.599625672291256295 ) ) ;
#114308 = CARTESIAN_POINT ( 'NONE',  ( 7.233438648090761980, 8.397765496649418182, 1.199719254218462483 ) ) ;
#114309 = CARTESIAN_POINT ( 'NONE',  ( 10.95308175811721085, 13.79999999999998295, 1.799999999999999600 ) ) ;
#114310 = CARTESIAN_POINT ( 'NONE',  ( 6.018611168240656006, 1.417078199399327332, -1.558035186251781612 ) ) ;
#114311 = CARTESIAN_POINT ( 'NONE',  ( -1.364683531250012516, 3.342708333674756727, 0.7879004041258379498 ) ) ;
#114312 = CARTESIAN_POINT ( 'NONE',  ( 4.710339443014814442, -0.9195336665917231977, -1.956380038831563972 ) ) ;
#114313 = CARTESIAN_POINT ( 'NONE',  ( 4.969401683643670076, -1.707372507963246022, -1.078548144515010909 ) ) ;
#114314 = CARTESIAN_POINT ( 'NONE',  ( -1.364683531250014514, -1.219791666325248602, 0.7879004041258379498 ) ) ;
#114315 = CARTESIAN_POINT ( 'NONE',  ( -5.504247177468192476, 7.444707678511436555, 1.443375672974064550 ) ) ;
#114316 = B_SPLINE_SURFACE_WITH_KNOTS ( 'NONE', 1, 3, ( 
 ( #107049, #190356, #187163, #55044, #138440, #59301, #121194, #191421, #38792, #189303, #204458, #26795, #170916, #56112, #42018, #188227, #123339, #39867, #108127, #105976, #174154, #23590, #89698, #155748, #205540, #73410, #139513, #40943, #143805, #145926, #142728, #192488, #60364, #28945, #93968, #162154, #12669, #211938, #128665, #44140, #63573, #110261, #129729, #126527, #45213, #76615, #27872, #112391, #31092, #13741, #79814, #78744, #113462, #178403, #193570, #144868, #195713, #210875, #47348, #61438, #95029, #62500, #96099, #127604, #161079, #46275, #194633, #30015, #179467, #176270, #10541, #160009, #97164, #92900, #163219, #11610, #158946, #77684, #208737, #209802, #177331, #111328, #158572, #189988, #56795, #58930, #175901, #75186, #73027, #141298, #71948, #23199, #171605, #76245, #138058, #205152, #59995, #40561, #42711, #55723, #207307, #125088, #191046, #89314, #122964, #155361, #6946, #204071, #105573, #172692, #142354, #41639, #157515, #91454, #26420, #108819, #208364, #126148, #74118, #159636, #121877, #174843, #187848, #92532, #106668, #188923, #39474, #90375, #57860, #206233, #192111, #109888, #43775, #107753, #9110, #24270, #10171, #139125, #156444, #140214, #8028, #124022, #25354, #173779, #27492, #93592, #95730, #79447, #197452, #162847, #12296, #179093, #30715, #77312, #176955, #115213, #78376, #14425, #63197, #45907, #61066, #96798, #114161, #127225, #144496, #196403, #194261, #49093, #143425, #62139, #211562, #147662, #210504, #161782, #213679, #11233, #146612, #181203, #81579, #13373, #180154, #128299, #80515, #212630, #64271, #130416, #48048, #31780, #193194, #97852, #163915, #112025, #131451, #15491, #178027, #110948, #98908, #32831, #94659, #44842, #65302, #209421, #29645, #28571, #160702, #145564, #129361, #195339, #46971, #113087, #133568, #34944, #37084, #3494, #186536, #151921, #101016, #184395, #152980, #70629, #33887, #69564, #68502, #103163, #289, #199574, #183339, #18694, #150863, #135674, #36015, #149789, #66360, #1363, #169224, #99965, #136740, #117342, #84776, #50149, #168164, #19762, #167107, #2425, #134630, #52282, #20816, #201699 ),
 ( #200634, #83701, #53342, #16552, #85844, #86912, #119476, #51218, #118409, #102094, #202766, #182262, #185464, #4555, #132506, #166030, #198504, #54416, #120557, #38165, #17615, #164960, #82635, #148719, #116273, #67425, #82579, #102043, #135621, #18641, #104184, #148667, #119422, #233, #201641, #51162, #133513, #198452, #34886, #2371, #150807, #70570, #54365, #4501, #200579, #168112, #117285, #19711, #33833, #16498, #84720, #100959, #17559, #184342, #134579, #68449, #149731, #53289, #66305, #85790, #103111, #185409, #183281, #52226, #118354, #120505, #99913, #167049, #169170, #132454, #165973, #50098, #35965, #1309, #37027, #151871, #20764, #3445, #83644, #86858, #67369, #152923, #182207, #69512, #116219, #199517, #136689, #186478, #202714, #38113, #205928, #208055, #157201, #106359, #123718, #42399, #189680, #158273, #188617, #73803, #173464, #58622, #40249, #139897, #91145, #57561, #41331, #107440, #203778, #153997, #171302, #92221, #21818, #75938, #55422, #25044, #105261, #108508, #9861, #87923, #8798, #174531, #74877, #155062, #140983, #59682, #206992, #22893, #124777, #170234, #121576, #187547, #26110, #5566, #89010, #142039, #138822, #190736, #71645, #125842, #191799, #43462, #39177, #6650, #72728, #204843, #172383, #137758, #56496, #122654, #23972, #90074, #156137, #7719, #15179, #192869, #14107, #13052, #196096, #159319, #144192, #80195, #64995, #46653, #47728, #129045, #94348, #10915, #160390, #113845, #44525, #81266, #61824, #177717, #209110, #112776, #178787, #127990, #193945, #45591, #211254, #179840, #146299, #30401, #79130, #197138, #76992, #111708, #145247, #210184, #29326, #60748, #143119, #195021, #11991, #109583, #78066, #95420, #62877, #93281, #163596, #212312, #161472, #31463, #126910, #63947, #97538, #96486, #110642, #162534, #130102, #147345, #213372, #176644, #131149, #175587, #27177, #28256, #152657, #115954, #51970, #100706, #83381, #98588, #2107, #151605, #164650, #49829, #19439, #17302, #20505, #114892, #99646, #34635, #185134, #181944, #133245, #36760, #48777, #184080, #4239, #119151, #50897, #3173, #165713, #134312, #68181, #118095 ) ),
 .UNSPECIFIED., .F., .T., .F.,
 ( 2, 2 ),
 ( 4, 2, 2, 2, 2, 2, 2, 2, 2, 2, 2, 2, 2, 2, 2, 2, 2, 2, 2, 2, 2, 2, 2, 2, 2, 2, 2, 2, 2, 2, 2, 2, 2, 2, 2, 2, 2, 2, 2, 2, 2, 2, 2, 2, 2, 2, 2, 2, 2, 2, 2, 2, 2, 2, 2, 2, 2, 2, 2, 2, 2, 2, 2, 2, 2, 2, 2, 2, 2, 2, 2, 2, 2, 2, 2, 2, 2, 2, 2, 2, 2, 2, 2, 2, 2, 2, 2, 2, 2, 2, 2, 2, 2, 2, 2, 2, 2, 2, 2, 2, 2, 2, 2, 2, 2, 2, 2, 2, 2, 2, 2, 2, 2, 2, 2, 2, 2, 2, 2, 2, 2, 2, 2, 4 ),
 ( 0.000000000000000000, 1.000000000000000000 ),
 ( 0.0003308050673979778117, 0.0003990699536394003003, 0.0004673348398808227890, 0.0005355997261222453319, 0.0006038646123636677663, 0.0007403943848465126352, 0.0008769241573293576125, 0.0009110566004500689381, 0.0009451890435707801554, 0.001013453929812202590, 0.001081718816053625024, 0.001149983702295047459, 0.001286513474777892328, 0.001354778361019314762, 0.001388910804140025979, 0.001423043247260737413, 0.001491308133502160065, 0.001559573019743582499, 0.001696102792226427368, 0.001764367678467849802, 0.001832632564709272237, 0.001900897450950694671, 0.001969162337192117106, 0.002037427223433539540, 0.002105692109674961975, 0.002173956995916384409, 0.002242221882157806843, 0.002310486768399229278, 0.002344619211519940495, 0.002378751654640651712, 0.002515281427123497015, 0.002651811199606342317, 0.002720076085847764752, 0.002788340972089187186, 0.002856605858330609621, 0.002924870744572032055, 0.003061400517054876924, 0.003129665403296299359, 0.003197930289537721793, 0.003266195175779144227, 0.003334460062020566662, 0.003402724948261989096, 0.003470989834503411531, 0.003607519606986256400, 0.003675784493227678834, 0.003709916936348390051, 0.003744049379469101269, 0.003812314265710523703, 0.003880579151951946137, 0.004017108924434791006, 0.004085373810676213441, 0.004153638696917635875, 0.004187771140038347092, 0.004221903583159058310, 0.004290168469400480744, 0.004358433355641903179, 0.004426698241883325613, 0.004494963128124748047, 0.004529095571245459265, 0.004563228014366170482, 0.004631492900607592916, 0.004699757786849016218, 0.004836287559331861954, 0.004904552445573284389, 0.004972817331814706823, 0.005041082218056129258, 0.005109347104297551692, 0.005177611990538974127, 0.005245876876780396561, 0.005314141763021818995, 0.005382406649263241430, 0.005450671535504663864, 0.005518936421746086299, 0.005587201307987508733, 0.005655466194228931168, 0.005791995966711776037, 0.005860260852953198471, 0.005928525739194620905, 0.005962658182315332123, 0.005996790625436043340, 0.006065055511677465774, 0.006133320397918888209, 0.006201585284160310643, 0.006269850170401733078, 0.006338115056643155512, 0.006406379942884577947, 0.006440512386005289164, 0.006474644829126000381, 0.006611174601608845250, 0.006747704374091690119, 0.006815969260333112553, 0.006850101703453823770, 0.006884234146574534988, 0.006952499032815957422, 0.007020763919057379857, 0.007157293691540224725, 0.007225558577781647160, 0.007293823464023069594, 0.007327955907143780812, 0.007362088350264492029, 0.007430353236505915331, 0.007498618122747338632, 0.007566883008988761067, 0.007635147895230183501, 0.007703412781471605936, 0.007771677667713028370, 0.007805810110833739587, 0.007839942553954450805, 0.007908207440195873239, 0.007976472326437295673, 0.008113002098920140542, 0.008181266985161562977, 0.008249531871402985411, 0.008317796757644407846, 0.008386061643885830280, 0.008454326530127252715, 0.008522591416368675149, 0.008590856302610097583, 0.008659121188851520018, 0.008727386075092942452, 0.008761518518213653670, 0.008795650961334364887, 0.008932180733817209756, 0.009068710506300054625 ),
 .UNSPECIFIED. ) ;
#114319 = CARTESIAN_POINT ( 'NONE',  ( 5.016153647376205171, 6.875265226737464985, 1.443375672974062551 ) ) ;
#114318 = CARTESIAN_POINT ( 'NONE',  ( 1.001543065824772753E-15, -2.471874999522041705, 3.793834371823811669 ) ) ;
#114317 = CARTESIAN_POINT ( 'NONE',  ( 7.147083253059300922, 8.367293879104554577, 1.199719254218452935 ) ) ;
#114320 = CARTESIAN_POINT ( 'NONE',  ( -3.955946960137363799, 7.837298230127379917, 0.7998128361456352531 ) ) ;
#114321 = CARTESIAN_POINT ( 'NONE',  ( 4.118375227313908482, 1.978554835517082555, 0.3886342876525810119 ) ) ;
#114322 = CARTESIAN_POINT ( 'NONE',  ( -7.771848369131641121, 10.09024240211882351, -1.599625672291263179 ) ) ;
#114324 = FILL_AREA_STYLE ('',( #134792 ) ) ;
#114323 = CARTESIAN_POINT ( 'NONE',  ( -3.277320446201389181, 4.846626492033466072, 1.599625672291267398 ) ) ;
#114325 = CARTESIAN_POINT ( 'NONE',  ( 0.6823417656249917140, 5.592708333674749177, 1.181850606188765695 ) ) ;
#114327 = CARTESIAN_POINT ( 'NONE',  ( -1.364683531250000748, 9.609375000341396245, 0.000000000000000000 ) ) ;
#114326 = CARTESIAN_POINT ( 'NONE',  ( 5.348557406608104969, 0.6236849695623291057, 2.069784783864880851 ) ) ;
#114328 = DIRECTION ( 'NONE',  ( 0.6123724356957896964, 0.7071067811865539010, 0.3535533905932691789 ) ) ;
#114329 = CARTESIAN_POINT ( 'NONE',  ( -11.95656167602934161, 7.981505742835744321, -1.053473157398042037 ) ) ;
#114330 = EDGE_CURVE ( 'NONE', #58795, #144319, #22193, .T. ) ;
#114332 = CARTESIAN_POINT ( 'NONE',  ( 5.325796065338770369, 0.8146125389149364571, -1.844717355016491478 ) ) ;
#114331 = CARTESIAN_POINT ( 'NONE',  ( -6.195713011320795438, 8.251417818006149929, -1.443375672974058777 ) ) ;
#114333 = CARTESIAN_POINT ( 'NONE',  ( -1.364683531250014514, -1.157291666325248158, 0.7879004041258379498 ) ) ;
#114334 = CARTESIAN_POINT ( 'NONE',  ( 1.699380632523245449, -0.5835770076011400631, 1.623301926564212794 ) ) ;
#114335 = CARTESIAN_POINT ( 'NONE',  ( 4.980641328173811999, 6.904110530993182948, 1.599625672291269396 ) ) ;
#114337 = CARTESIAN_POINT ( 'NONE',  ( 7.679767667498067496, 7.924426798361372093, 0.000000000000000000 ) ) ;
#114336 = CARTESIAN_POINT ( 'NONE',  ( 6.616015773788773480, 10.66250946948817813, -0.7216878364870267237 ) ) ;
#114338 = CARTESIAN_POINT ( 'NONE',  ( -11.81223854822482622, 8.717195842676252582, -2.135728645746848287 ) ) ;
#114339 = CARTESIAN_POINT ( 'NONE',  ( 6.520764494017629254, 1.745421825204738431, 0.6730592012400560264 ) ) ;
#114340 = CARTESIAN_POINT ( 'NONE',  ( 0.7857919059152475016, 1.939557017834290020, -0.5388494671653855095 ) ) ;
#114341 = CARTESIAN_POINT ( 'NONE',  ( -4.733481511527885210, 4.890303307122107590, -0.5491554243041256722 ) ) ;
#114342 = CARTESIAN_POINT ( 'NONE',  ( 2.889901548669851383, 1.559680528474843841, 1.561422205034967314 ) ) ;
#114343 = CARTESIAN_POINT ( 'NONE',  ( -6.170369307550858551, 8.292126506933035657, 1.443375672974058777 ) ) ;
#114344 = ORIENTED_EDGE ( 'NONE', *, *, #37148, .F. ) ;
#114345 = CARTESIAN_POINT ( 'NONE',  ( 9.720832950873944611, 10.44331931888218001, -0.7216878364870257245 ) ) ;
#114347 = CARTESIAN_POINT ( 'NONE',  ( 1.388296234047466049, -0.7283980888908546669, -1.880428666220852696 ) ) ;
#114346 = CARTESIAN_POINT ( 'NONE',  ( 1.981254353800803836, -1.939921095825656305, -0.8566514584813913480 ) ) ;
#114349 = ORIENTED_EDGE ( 'NONE', *, *, #24376, .F. ) ;
#114348 = CARTESIAN_POINT ( 'NONE',  ( 2.373076535756658778, -1.577936908029322849, -0.8897043057118164677 ) ) ;
#114350 = CARTESIAN_POINT ( 'NONE',  ( 5.515134625708930649, 9.656350506627580543, 0.000000000000000000 ) ) ;
#114351 = CIRCLE ( 'NONE', #86593, 0.04999999999999970440 ) ;
#114352 = CARTESIAN_POINT ( 'NONE',  ( 5.829115978871627135, 8.888053511070525659, 1.199719254218462483 ) ) ;
#114354 = CARTESIAN_POINT ( 'NONE',  ( -0.1357414145864926924, -1.858833624763186032, -0.4630600859806994762 ) ) ;
#114353 = CARTESIAN_POINT ( 'NONE',  ( -5.264643720808155791, 5.036505850564608089, 0.000000000000000000 ) ) ;
#114355 = LINE ( 'NONE', #98055, #52316 ) ;
#114356 = CARTESIAN_POINT ( 'NONE',  ( 9.606148981167590861, -6.583980363595129504, -0.4355862708379804604 ) ) ;
#114357 = ADVANCED_FACE ( 'NONE', ( #9924 ), #56545, .T. ) ;
#114358 = CARTESIAN_POINT ( 'NONE',  ( 6.629573926958101993, 6.836850457647000390, -0.7216878364870257245 ) ) ;
#114359 = CARTESIAN_POINT ( 'NONE',  ( 0.6823417656249882723, 0.2385416670080825474, -1.181850606188749264 ) ) ;
#114360 = CARTESIAN_POINT ( 'NONE',  ( 0.000000000000000000, 5.499999999999998224, 0.000000000000000000 ) ) ;
#114361 = CARTESIAN_POINT ( 'NONE',  ( -8.286004436246233951, 12.81875560892930466, 1.040834085586084257E-14 ) ) ;
#114362 = CARTESIAN_POINT ( 'NONE',  ( 4.716029918043215474, 1.032482702726954527, -1.731993998903176957 ) ) ;
#114363 = CARTESIAN_POINT ( 'NONE',  ( 4.698204674003193304, -2.161138953124014161, -0.05634304724232848394 ) ) ;
#114364 = CARTESIAN_POINT ( 'NONE',  ( -4.963693636378939011, 8.805076652501815815, 0.7216878364870267237 ) ) ;
#114365 = CARTESIAN_POINT ( 'NONE',  ( 6.048345925472191631, 6.229027465905275562, 0.7216878364870328300 ) ) ;
#114366 = CARTESIAN_POINT ( 'NONE',  ( 2.057031522680652369, 0.4693188842763912905, 2.067847215655476578 ) ) ;
#114367 = DIRECTION ( 'NONE',  ( -0.04888523518676873847, 0.000000000000000000, -0.9988044021632734859 ) ) ;
#114368 = CARTESIAN_POINT ( 'NONE',  ( 3.005103179519866607, 1.663439489741199928, 1.057676205593648167 ) ) ;
#114369 = EDGE_LOOP ( 'NONE', ( #121112, #158257, #6479 ) ) ;
#114370 = CARTESIAN_POINT ( 'NONE',  ( -2.039928227386959669, 3.162178953954597471, 11.45750328113832062 ) ) ;
#114371 = CARTESIAN_POINT ( 'NONE',  ( 6.742638201966631328, -1.931250359857048515, -0.3855633916233728309 ) ) ;
#114372 = CARTESIAN_POINT ( 'NONE',  ( 1.534995247775998939, -1.406442930887800813, -1.339296560326202146 ) ) ;
#114373 = ORIENTED_EDGE ( 'NONE', *, *, #392, .F. ) ;
#114374 = CARTESIAN_POINT ( 'NONE',  ( -4.233785845893567767, 7.337832232212887718, -0.8726355574809127047 ) ) ;
#114376 = CARTESIAN_POINT ( 'NONE',  ( 8.188198428010544205, 8.517596018959260107, 0.000000000000000000 ) ) ;
#114375 = CARTESIAN_POINT ( 'NONE',  ( -7.119440060951841787, 7.478637290631501067, 0.000000000000000000 ) ) ;
#114378 = CARTESIAN_POINT ( 'NONE',  ( 5.798083248138522272, 9.916180889470295412, 0.7998128361456462443 ) ) ;
#114377 = CARTESIAN_POINT ( 'NONE',  ( 2.220754083240178645, 0.001034992482759621978, 2.090823719040376893 ) ) ;
#114380 = CARTESIAN_POINT ( 'NONE',  ( 5.736508391913541338, 6.825586224388162648, -1.082531754730548412 ) ) ;
#114379 = CARTESIAN_POINT ( 'NONE',  ( 5.849453209292126310, 8.911780279894442103, 1.199719254218462483 ) ) ;
#114382 = ORIENTED_EDGE ( 'NONE', *, *, #94657, .F. ) ;
#114381 = CARTESIAN_POINT ( 'NONE',  ( 6.428373272941257710, -0.9058926715965059939, -1.684108486221975953 ) ) ;
#114383 = CARTESIAN_POINT ( 'NONE',  ( 4.354274438496381627, 2.206422198305586058, -0.05263853172451230661 ) ) ;
#114384 = CARTESIAN_POINT ( 'NONE',  ( 1.975870009618452050, 2.111717515986545113, -0.6407313945460398896 ) ) ;
#114385 = DIRECTION ( 'NONE',  ( 0.6507913734559641616, -0.7592566023653004592, 0.000000000000000000 ) ) ;
#114386 = CARTESIAN_POINT ( 'NONE',  ( 0.9086806230526077721, -0.4651930584498394916, -1.854694524013176693 ) ) ;
#114387 = LINE ( 'NONE', #80755, #62812 ) ;
#114388 = CARTESIAN_POINT ( 'NONE',  ( 10.58621901417202515, 11.24501035948919991, -0.7998128361456281477 ) ) ;
#114389 = CARTESIAN_POINT ( 'NONE',  ( 4.123533666479628046, 0.2564666318346648377, -2.054367117340555549 ) ) ;
#114391 = CARTESIAN_POINT ( 'NONE',  ( 1.235488887756378551, -1.954010380348418119, 0.9248176494114216384 ) ) ;
#114390 = CARTESIAN_POINT ( 'NONE',  ( -3.440018289565379028, 5.036440642624797626, 1.599625672291267398 ) ) ;
#114392 = CARTESIAN_POINT ( 'NONE',  ( 3.351304529449970371, 0.5305821810032870234, -2.126252377916526992 ) ) ;
#114393 = CARTESIAN_POINT ( 'NONE',  ( 11.86145016429272836, 10.19999999999999929, 1.179999999999997051 ) ) ;
#114394 = CARTESIAN_POINT ( 'NONE',  ( -11.04536101718726293, 13.40000000000000036, -1.100000000000002087 ) ) ;
#114395 = CARTESIAN_POINT ( 'NONE',  ( -0.5601741628962252362, 7.746630099212525877, 1.919951735362938505 ) ) ;
#114396 = CARTESIAN_POINT ( 'NONE',  ( 0.6823417656249934904, 14.50520833367473195, 1.181850606188764807 ) ) ;
#114397 = CARTESIAN_POINT ( 'NONE',  ( -4.492547798081878874, 6.334668079219206049, 1.599625672291263179 ) ) ;
#114398 = CARTESIAN_POINT ( 'NONE',  ( 6.539718741795587320, -1.333554142906383744, 1.108523769342983689 ) ) ;
#114399 = CARTESIAN_POINT ( 'NONE',  ( -9.978437869977950569, 11.70422760547153906, -1.082531754730539753 ) ) ;
#114400 = CARTESIAN_POINT ( 'NONE',  ( 4.504778988403771223, 0.5471568804141565545, 1.996604337080605474 ) ) ;
#114401 = CARTESIAN_POINT ( 'NONE',  ( 2.930207584894477080, 1.069882305642521514, -1.601919868193351082 ) ) ;
#114402 = CARTESIAN_POINT ( 'NONE',  ( 6.116841120987044356, 0.2079722402913257440, 2.107011275531808003 ) ) ;
#114403 = CARTESIAN_POINT ( 'NONE',  ( 5.438792177376376991, 9.497007973581119700, 1.040834085586084257E-14 ) ) ;
#114404 = CARTESIAN_POINT ( 'NONE',  ( 1.364683531249988535, 5.405208333674750953, -0.7879004041258300672 ) ) ;
#114405 = CARTESIAN_POINT ( 'NONE',  ( 4.504722179138310523, 0.5213129852876841053, 1.899149332505256638 ) ) ;
#114406 = CARTESIAN_POINT ( 'NONE',  ( 5.912145817070847187, 1.543564834742835234, -1.694840376948128391 ) ) ;
#114407 = CARTESIAN_POINT ( 'NONE',  ( 3.932112477472641920, 0.9751300899686901058, -1.543267412809447681 ) ) ;
#114408 = CARTESIAN_POINT ( 'NONE',  ( 3.542423274920540432, 7.354853930707762721, -1.734723475976807094E-15 ) ) ;
#114409 = CARTESIAN_POINT ( 'NONE',  ( 5.300874872818843286, 5.286701561151180506, 0.7216878364870317197 ) ) ;
#114410 = CARTESIAN_POINT ( 'NONE',  ( -6.282224075085783177, 8.422623735723785643, 1.599625672291269396 ) ) ;
#114411 = CARTESIAN_POINT ( 'NONE',  ( 5.342795052237045539, 8.390955439988655229, -1.199719254218450271 ) ) ;
#114412 = ORIENTED_EDGE ( 'NONE', *, *, #199113, .T. ) ;
#114413 = CARTESIAN_POINT ( 'NONE',  ( 5.045186288489547977, 0.1525188484602090777, 2.007510047055609093 ) ) ;
#114414 = CARTESIAN_POINT ( 'NONE',  ( 6.504485943970635731, -2.231000991611901352, 0.5533298437200293574 ) ) ;
#114415 = CARTESIAN_POINT ( 'NONE',  ( 4.909014596843685574, -1.577992517845404619, 1.165349624694256958 ) ) ;
#114416 = CARTESIAN_POINT ( 'NONE',  ( -6.235860587281615075, 9.362588887548838557, -1.199719254218440723 ) ) ;
#114417 = CARTESIAN_POINT ( 'NONE',  ( -5.596818484342970912, 5.424043074688562172, -0.7998128361456221525 ) ) ;
#114418 = DIRECTION ( 'NONE',  ( -0.7071067811865497932, -0.7071067811865452413, 8.659560562354947649E-17 ) ) ;
#114419 = CARTESIAN_POINT ( 'NONE',  ( -6.394605727500880299, 7.489403432619674561, -1.199719254218452047 ) ) ;
#114421 = CARTESIAN_POINT ( 'NONE',  ( 6.086734230332795370, -0.2636980280019511902, -1.749942407053702409 ) ) ;
#114420 = CARTESIAN_POINT ( 'NONE',  ( 0.2926706434557576064, 1.735970642146159371, -1.164857044846574707 ) ) ;
#114422 = DIRECTION ( 'NONE',  ( 3.497202527569253358E-15, -0.000000000000000000, 1.000000000000000000 ) ) ;
#114423 = CARTESIAN_POINT ( 'NONE',  ( 5.894467665742915585, 1.586334124781592969, -1.119885764912365467 ) ) ;
#114424 = CARTESIAN_POINT ( 'NONE',  ( 1.834175572193702530, 2.167931929539984814, 0.3193665180123914094 ) ) ;
#114425 = CARTESIAN_POINT ( 'NONE',  ( 0.5732861554464663278, -0.9687841611035786782, 1.445654263422226027 ) ) ;
#114426 = CARTESIAN_POINT ( 'NONE',  ( 5.503720292143644777, 8.508425209887878538, 1.199719254218462483 ) ) ;
#114427 =( LENGTH_UNIT ( ) NAMED_UNIT ( * ) SI_UNIT ( .MILLI., .METRE. ) );
#114428 = CARTESIAN_POINT ( 'NONE',  ( 1.506044924156377807, -0.6181864485952697219, -1.610478869194363227 ) ) ;
#114429 =( BOUNDED_CURVE ( )  B_SPLINE_CURVE ( 3, ( #185124, #81252, #83364, #149449 ),
 .UNSPECIFIED., .F., .T. ) 
 B_SPLINE_CURVE_WITH_KNOTS ( ( 4, 4 ),
 ( 0.000000000000000000, 0.5000000000000011102 ),
 .UNSPECIFIED. ) 
 CURVE ( )  GEOMETRIC_REPRESENTATION_ITEM ( )  RATIONAL_B_SPLINE_CURVE ( ( 1.000000000000000000, 0.3333333333333318715, 0.3333333333333333703, 1.000000000000001554 ) ) 
 REPRESENTATION_ITEM ( '' )  );
#114430 = CARTESIAN_POINT ( 'NONE',  ( 1.382659466718983543, -0.3261178763579902218, -2.167053615394160637 ) ) ;
#114431 = CARTESIAN_POINT ( 'NONE',  ( 4.037865812933420173, -1.521084700717803884, -1.599171214764223636 ) ) ;
#114432 = CARTESIAN_POINT ( 'NONE',  ( 1.288188150525194642, -1.375441891341127265, -1.679832657438373511 ) ) ;
#114433 = CARTESIAN_POINT ( 'NONE',  ( -1.257518954445029147, 2.966479010054028365, 0.7750000000000170086 ) ) ;
#114434 = CARTESIAN_POINT ( 'NONE',  ( 2.712237125307418228, 1.172176456337461037, -1.763091465072692987 ) ) ;
#114435 = CARTESIAN_POINT ( 'NONE',  ( 6.661184041420942670, -7.246166700180828535, -6.773376349083129355 ) ) ;
#114436 = ORIENTED_EDGE ( 'NONE', *, *, #24579, .F. ) ;
#114438 = CARTESIAN_POINT ( 'NONE',  ( -1.364683531250014514, -0.4489583329919089039, -0.7879004041258359514 ) ) ;
#114437 = CARTESIAN_POINT ( 'NONE',  ( 2.894357049080374278, -0.6678387144627718763, -2.192917219349885816 ) ) ;
#114439 = CARTESIAN_POINT ( 'NONE',  ( 3.195971524519376494, 4.751719416737803847, -1.599625672291262513 ) ) ;
#114440 = CARTESIAN_POINT ( 'NONE',  ( 3.520313441042647540, 7.258782781191745137, 0.7998128361456321445 ) ) ;
#114441 = CARTESIAN_POINT ( 'NONE',  ( 4.635507155980078231, -0.1095829440264598081, 2.218699120425669413 ) ) ;
#114442 = CARTESIAN_POINT ( 'NONE',  ( -7.212574532790102744, 8.477387045419011002, -1.082531754730550855 ) ) ;
#114444 = EDGE_CURVE ( 'NONE', #93128, #108753, #38418, .T. ) ;
#114443 = CARTESIAN_POINT ( 'NONE',  ( -0.4373225248172993851, -5.223431457505089526, -10.96785329849811497 ) ) ;
#114445 = CARTESIAN_POINT ( 'NONE',  ( 4.311129659465574804, 7.013106455143060636, -1.082531754730548412 ) ) ;
#114446 = CARTESIAN_POINT ( 'NONE',  ( -7.714226216051410567, 9.062647342557177410, 1.082531754730558626 ) ) ;
#114447 = CIRCLE ( 'NONE', #111050, 0.8299999999999999600 ) ;
#114448 = CARTESIAN_POINT ( 'NONE',  ( 4.746763178560254204, 6.631252689777363152, 1.443375672974065660 ) ) ;
#114449 = ORIENTED_EDGE ( 'NONE', *, *, #76301, .F. ) ;
#114450 = CARTESIAN_POINT ( 'NONE',  ( 2.567029916978436077, -1.034165006014248211, 1.730866473406714068 ) ) ;
#114452 = CARTESIAN_POINT ( 'NONE',  ( 2.694246160070143503, 0.9763755106866910394, -1.816870488346455037 ) ) ;
#114451 = CARTESIAN_POINT ( 'NONE',  ( 7.287671262545424966, 8.461036880179857889, -1.199719254218451159 ) ) ;
#114453 = CARTESIAN_POINT ( 'NONE',  ( 0.000000000000000000, 5.999999999999998224, -10.25000000000000000 ) ) ;
#114454 = CARTESIAN_POINT ( 'NONE',  ( 3.865483193227626124, 7.523831135491951372, -0.7216878364870338292 ) ) ;
#114455 = CARTESIAN_POINT ( 'NONE',  ( -5.585596099150257565, 5.618876325204375632, -0.7216878364869792062 ) ) ;
#114456 = CARTESIAN_POINT ( 'NONE',  ( 0.6823417656249899377, 3.926041667008085767, -1.181850606188754593 ) ) ;
#114457 = CARTESIAN_POINT ( 'NONE',  ( 4.541096662771787251, -1.693051203114638525, -1.391418086139440957 ) ) ;
#114458 = CARTESIAN_POINT ( 'NONE',  ( 2.074842474778653134, -0.8596299393073093542, 1.824119475507138821 ) ) ;
#114459 = CARTESIAN_POINT ( 'NONE',  ( 1.434833617064284805, -1.334073193498284793, -1.269287082821937362 ) ) ;
#114460 = ADVANCED_FACE ( 'NONE', ( #137817 ), #175649, .T. ) ;
#114461 = CARTESIAN_POINT ( 'NONE',  ( 6.272618624616828953, 10.46980549536166016, 1.040834085586084257E-14 ) ) ;
#114462 = CARTESIAN_POINT ( 'NONE',  ( 4.875911338656576888, 1.051942333337583468, 1.491839654383666947 ) ) ;
#114463 = CARTESIAN_POINT ( 'NONE',  ( 6.205703963786828758, 1.882472927010571118, 0.7231429968634556227 ) ) ;
#114464 = CARTESIAN_POINT ( 'NONE',  ( -7.340850106795412167, 10.65174332698158643, 1.199719254218453823 ) ) ;
#114466 = CARTESIAN_POINT ( 'NONE',  ( -5.094831863685302942, 9.165997284266655498, 0.7998128361456291469 ) ) ;
#114465 = CARTESIAN_POINT ( 'NONE',  ( 4.540055829149266309, 0.9713072833863345412, -2.043554373614121289 ) ) ;
#114467 = CARTESIAN_POINT ( 'NONE',  ( 0.8914058518391498875, 1.856551077915175707, -0.9943519572734434986 ) ) ;
#114468 = CARTESIAN_POINT ( 'NONE',  ( -7.449279056065764237, 7.655523418356991350, 0.7998128361456341429 ) ) ;
#114469 = CARTESIAN_POINT ( 'NONE',  ( 5.230950013807261101, -1.948248037745937022, -0.7008574099531189594 ) ) ;
#114470 = CARTESIAN_POINT ( 'NONE',  ( 7.553864141108259211, 11.96459193126834464, 1.040834085586084257E-14 ) ) ;
#114471 = CARTESIAN_POINT ( 'NONE',  ( -1.360316468750038643, 2.901041667008071645, -0.7853790794159161148 ) ) ;
#114472 = DIRECTION ( 'NONE',  ( -1.000000000000000000, -4.643935581739670507E-17, 2.220446049250313081E-16 ) ) ;
#114473 = CARTESIAN_POINT ( 'NONE',  ( -9.365985188942097750, 9.821404230054264772, 0.7998128361456462443 ) ) ;
#114474 = UNCERTAINTY_MEASURE_WITH_UNIT (LENGTH_MEASURE( 1.000000000000000082E-05 ), #130764, 'distance_accuracy_value', 'NONE');
#114475 = SURFACE_SIDE_STYLE ('',( #34206 ) ) ;
#114476 = B_SPLINE_CURVE_WITH_KNOTS ( 'NONE', 3,
 ( #201626, #119406, #98841, #167032, #17543, #1295 ),
 .UNSPECIFIED., .F., .F.,
 ( 4, 2, 4 ),
 ( 0.000000000000000000, 0.0003155923098472862933, 0.0006311846196945722614 ),
 .UNSPECIFIED. ) ;
#114477 = CARTESIAN_POINT ( 'NONE',  ( 6.688968683495743583, 8.897159112202094988, -1.599625672291283607 ) ) ;
#114478 = CARTESIAN_POINT ( 'NONE',  ( 5.160031065370225711, 6.461479299918838848, -1.191482946479218485 ) ) ;
#114479 = CARTESIAN_POINT ( 'NONE',  ( -8.622622508611375025, 12.04318144581317895, 1.082531754730560403 ) ) ;
#114481 = CARTESIAN_POINT ( 'NONE',  ( 1.371645089906252446, -1.908569115047893394, -1.136440837462453723 ) ) ;
#114480 = CARTESIAN_POINT ( 'NONE',  ( 1.582450481569739331, 1.094613367649547309, 1.816135667671102016 ) ) ;
#114482 = CARTESIAN_POINT ( 'NONE',  ( 4.960800185296459830, 8.075801985472857325, -1.085925974634168290 ) ) ;
#114483 = CARTESIAN_POINT ( 'NONE',  ( -6.668631453075260396, 8.873432343378178544, -1.599625672291271394 ) ) ;
#114484 = CARTESIAN_POINT ( 'NONE',  ( 5.276094334012385367, 9.307193822989793475, 1.040834085586084257E-14 ) ) ;
#114485 = CARTESIAN_POINT ( 'NONE',  ( 3.121486724888074882, 0.2905151309811822569, -1.940125473959073421 ) ) ;
#114486 = CARTESIAN_POINT ( 'NONE',  ( 4.961394147597008697, 7.875711374583454827, -1.199719254218452047 ) ) ;
#114487 = CARTESIAN_POINT ( 'NONE',  ( -4.088066877127150001, 7.522549914775793489, 0.5433784229755319606 ) ) ;
#114488 = CARTESIAN_POINT ( 'NONE',  ( 2.846322183865124700, 5.408127416896231665, -1.199719254218446718 ) ) ;
#114489 = CARTESIAN_POINT ( 'NONE',  ( -4.828112100242279325, 8.646898193675708555, -0.7216878364870338292 ) ) ;
#114490 = CARTESIAN_POINT ( 'NONE',  ( -7.863365906246074566, 8.276274433482971205, -0.7216878364870278340 ) ) ;
#114491 =( BOUNDED_CURVE ( )  B_SPLINE_CURVE ( 1, ( #124547, #40016 ),
 .UNSPECIFIED., .F., .T. ) 
 B_SPLINE_CURVE_WITH_KNOTS ( ( 2, 2 ),
 ( 0.000000000000000000, 4.605265433281100981E-05 ),
 .UNSPECIFIED. ) 
 CURVE ( )  GEOMETRIC_REPRESENTATION_ITEM ( )  RATIONAL_B_SPLINE_CURVE ( ( 0.9345202395942924234, 0.9345202395942924234 ) ) 
 REPRESENTATION_ITEM ( '' )  );
#114492 = CARTESIAN_POINT ( 'NONE',  ( 2.426173717206762781, -2.096881089210366422, 0.3156149858808757203 ) ) ;
#114493 = CARTESIAN_POINT ( 'NONE',  ( -5.936491157937300756, 8.019268665717216749, 1.599625672291263179 ) ) ;
#114494 = CARTESIAN_POINT ( 'NONE',  ( 5.283633159863808437, -1.863482887291990409, 0.6137318589548645953 ) ) ;
#114495 = CARTESIAN_POINT ( 'NONE',  ( 3.344745324850742385, 0.5235245934552492653, 2.097234944377385002 ) ) ;
#114496 = CARTESIAN_POINT ( 'NONE',  ( 3.280630368989821743, 1.663260157205956657, -0.7901080472864712156 ) ) ;
#114497 = CARTESIAN_POINT ( 'NONE',  ( -4.037324417950741484, 7.593329901778307800, 0.3124507474575183297 ) ) ;
#114498 = EDGE_CURVE ( 'NONE', #204806, #158047, #7776, .T. ) ;
#114499 = CARTESIAN_POINT ( 'NONE',  ( 1.364683531249986537, -0.5322916663252452718, -0.7879004041258309554 ) ) ;
#114500 = CARTESIAN_POINT ( 'NONE',  ( 4.452888953083543377, 0.3777208849818362579, -1.698664142626307383 ) ) ;
#114501 = FACE_OUTER_BOUND ( 'NONE', #200056, .T. ) ;
#114502 = CARTESIAN_POINT ( 'NONE',  ( 4.907688418466886304, 5.788353245375237321, -1.082531754730548412 ) ) ;
#114503 = FACE_OUTER_BOUND ( 'NONE', #67363, .T. ) ;
#114504 = AXIS2_PLACEMENT_3D ( 'NONE', #21352, #151398, #5096 ) ;
#114505 = CARTESIAN_POINT ( 'NONE',  ( 2.518638242371186386, 1.412657066830936392, -1.636333507658905173 ) ) ;
#114506 = CARTESIAN_POINT ( 'NONE',  ( 4.499374939222855474, 1.976653413780619761, 0.3960398538903551757 ) ) ;
#114507 = CARTESIAN_POINT ( 'NONE',  ( -9.341204649691320583, 10.96078884847042545, 1.082531754730558626 ) ) ;
#114508 = CARTESIAN_POINT ( 'NONE',  ( 1.463986924769441478, 2.129665692569195024, -0.3698555562515608020 ) ) ;
#114509 = CARTESIAN_POINT ( 'NONE',  ( 2.442595505675814405, 0.4281495253689853175, 1.924161874619955359 ) ) ;
#114510 = EDGE_CURVE ( 'NONE', #107434, #144331, #125904, .T. ) ;
#114511 = CARTESIAN_POINT ( 'NONE',  ( 3.878411472391342318, -0.1936643080829789088, -1.932398009575059472 ) ) ;
#114514 = ORIENTED_EDGE ( 'NONE', *, *, #124881, .T. ) ;
#114513 = CARTESIAN_POINT ( 'NONE',  ( 10.91804383151479740, -8.407420853759283830, -0.1905751639681655396 ) ) ;
#114512 = DIRECTION ( 'NONE',  ( 0.7592566023653016805, -0.6507913734559627184, 0.000000000000000000 ) ) ;
#114516 = EDGE_CURVE ( 'NONE', #97523, #207276, #198457, .T. ) ;
#114515 = CARTESIAN_POINT ( 'NONE',  ( -3.594320120954326292, 6.247105003538398371, 1.082531754730549967 ) ) ;
#114517 = CARTESIAN_POINT ( 'NONE',  ( 3.400062661977048428, 7.188766548940353829, -1.734723475976807094E-15 ) ) ;
#114519 = VERTEX_POINT ( 'NONE', #74935 ) ;
#114518 = CARTESIAN_POINT ( 'NONE',  ( -6.414942957921379474, 7.513130201443591005, -1.199719254218452047 ) ) ;
#114520 = CARTESIAN_POINT ( 'NONE',  ( -8.310784975052682100, 10.71900177569337487, -1.443375672974058777 ) ) ;
#114521 = CARTESIAN_POINT ( 'NONE',  ( 0.7806487521475922176, -1.224371414366259847, 1.835764474286231129 ) ) ;
#114522 = CARTESIAN_POINT ( 'NONE',  ( -3.285556943750000070, -1.159374999522042815, 0.000000000000000000 ) ) ;
#114523 = CARTESIAN_POINT ( 'NONE',  ( 5.471523917629521172, -0.2915489554583711174, 1.939870717765689534 ) ) ;
#114524 = CARTESIAN_POINT ( 'NONE',  ( -0.6823417656249969321, 5.280208333674756283, -1.181850606188749264 ) ) ;
#114525 = CARTESIAN_POINT ( 'NONE',  ( 1.499999999999990896, 3.556250000682818602, 1.214306433183764966E-14 ) ) ;
#114526 = CARTESIAN_POINT ( 'NONE',  ( 5.900277318768097246, 7.249539301847896411, -1.301905728482563251 ) ) ;
#114527 = CARTESIAN_POINT ( 'NONE',  ( 4.663899394030392997, -1.200468288914667614, 1.396033019000951336 ) ) ;
#114528 = ORIENTED_EDGE ( 'NONE', *, *, #10408, .F. ) ;
#114529 = CARTESIAN_POINT ( 'NONE',  ( -7.694415870955439551, 8.935572256658169010, 1.199719254218462483 ) ) ;
#114530 = DIRECTION ( 'NONE',  ( 0.000000000000000000, 0.000000000000000000, -1.000000000000000000 ) ) ;
#114531 = CARTESIAN_POINT ( 'NONE',  ( 4.693665235656380830, 1.977662049654808740, -0.7657889336421249693 ) ) ;
#114532 = DIRECTION ( 'NONE',  ( 0.000000000000000000, -1.000000000000000000, -0.000000000000000000 ) ) ;
#114533 = CARTESIAN_POINT ( 'NONE',  ( 4.937140493670735708, 8.911747675924535983, -0.7998128361456281477 ) ) ;
#114534 = VERTEX_POINT ( 'NONE', #24030 ) ;
#114535 = CARTESIAN_POINT ( 'NONE',  ( 6.608673410152685612, 1.530114183832030905, -1.380643333410998430 ) ) ;
#114538 = CARTESIAN_POINT ( 'NONE',  ( 3.790429961727882713, 1.553415782126759792, -0.9881970032953185656 ) ) ;
#114537 = CARTESIAN_POINT ( 'NONE',  ( 1.363465259770980209, -0.4569337200135030197, 1.803945581614458282 ) ) ;
#114536 = CARTESIAN_POINT ( 'NONE',  ( -4.288456660624211381, 3.897620947016656956, 1.214306433183764966E-14 ) ) ;
#114539 = CARTESIAN_POINT ( 'NONE',  ( 8.457588896826466751, 8.761608555919362828, 1.040834085586084257E-14 ) ) ;
#114540 = CARTESIAN_POINT ( 'NONE',  ( -11.01135777277262129, 10.19999999999999929, -1.400000000000001910 ) ) ;
#114541 =( NAMED_UNIT ( * ) PLANE_ANGLE_UNIT ( ) SI_UNIT ( $, .RADIAN. ) );
#114542 = CARTESIAN_POINT ( 'NONE',  ( -6.851666526859749418, 9.086973262793417661, -1.599625672291271394 ) ) ;
#114543 = DIRECTION ( 'NONE',  ( 0.000000000000000000, 8.546850786086437571E-32, 1.000000000000000000 ) ) ;
#114544 = CIRCLE ( 'NONE', #21042, 4.500000000000000000 ) ;
#114545 = CARTESIAN_POINT ( 'NONE',  ( 3.071135375186518690, -2.039199700013223815, -0.8442704067812344393 ) ) ;
#114546 = CARTESIAN_POINT ( 'NONE',  ( 5.237693395785977479, -1.594672120175673946, -1.605097536805524916 ) ) ;
#114547 = CIRCLE ( 'NONE', #104122, 11.67999999982603576 ) ;
#114548 = CARTESIAN_POINT ( 'NONE',  ( -6.887178846062123938, 8.097758744236356776, -1.082531754730544860 ) ) ;
#114549 = CARTESIAN_POINT ( 'NONE',  ( 5.994382934279598452, -0.9612500426990595592, 1.535330125949084135 ) ) ;
#114550 = CARTESIAN_POINT ( 'NONE',  ( 5.243340954880816973, 0.3670949043641066889, -1.880036887305686966 ) ) ;
#114551 = CARTESIAN_POINT ( 'NONE',  ( 1.364683531249990311, 4.946875000341417916, 1.214306433183764966E-14 ) ) ;
#114552 = CARTESIAN_POINT ( 'NONE',  ( 5.787941465827733722, -0.8397648285632768328, 1.671655200917811168 ) ) ;
#114553 = CARTESIAN_POINT ( 'NONE',  ( 6.127394093140170916, 0.1359088500606409067, -1.856169418941427729 ) ) ;
#114554 = LINE ( 'NONE', #113489, #43604 ) ;
#114555 = CARTESIAN_POINT ( 'NONE',  ( 6.297684251969362101, -0.5920937881782936119, 1.667988322058571393 ) ) ;
#114556 = CARTESIAN_POINT ( 'NONE',  ( 1.112517963266421939, 1.944731545904467396, 0.5331650539944567946 ) ) ;
#114558 = CARTESIAN_POINT ( 'NONE',  ( 2.596425589483622787, -2.100489730888196238, -0.1540555546653120389 ) ) ;
#114557 = CARTESIAN_POINT ( 'NONE',  ( -4.243338890952911058, 5.013278796608906518, -1.082531754730543971 ) ) ;
#114559 = CARTESIAN_POINT ( 'NONE',  ( 9.447334110624092673, 9.916311305349925220, -0.7998128361456281477 ) ) ;
#114561 = CARTESIAN_POINT ( 'NONE',  ( -7.967387826325084355, 12.44703623068796361, 0.7998128361456481317 ) ) ;
#114560 = CARTESIAN_POINT ( 'NONE',  ( 1.500000000000001332, 11.90625000068279427, 0.000000000000000000 ) ) ;
#114562 = PLANE ( 'NONE',  #110165 ) ;
#114563 = CARTESIAN_POINT ( 'NONE',  ( 2.320574876688247024, -0.7769297766534470906, -1.864587897788829718 ) ) ;
#114564 = CARTESIAN_POINT ( 'NONE',  ( -1.364683531249997417, 2.509375000341422357, 1.214306433183764966E-14 ) ) ;
#114565 = CARTESIAN_POINT ( 'NONE',  ( 2.683624340501134853, 5.218313266304903664, -1.199719254218446718 ) ) ;
#114566 = CARTESIAN_POINT ( 'NONE',  ( 3.374459016379764087, -1.290570702369205014, 1.733878788530068160 ) ) ;
#114567 = CARTESIAN_POINT ( 'NONE',  ( 6.889999999999973035, 7.629137130509064946, 2.879999999999991456 ) ) ;
#114570 = CARTESIAN_POINT ( 'NONE',  ( 3.375617060122621194, 6.882044303544283537, 1.040834085586084257E-14 ) ) ;
#114569 = CARTESIAN_POINT ( 'NONE',  ( 0.7500000000000006661, 13.19791666734946389, -1.299038105676657340 ) ) ;
#114568 = CARTESIAN_POINT ( 'NONE',  ( 3.400062661977048428, 7.188766548940353829, -1.734723475976807094E-15 ) ) ;
#114571 = CARTESIAN_POINT ( 'NONE',  ( 9.883530794237934458, 10.63313346947350269, -0.7216878364870257245 ) ) ;
#114572 = CARTESIAN_POINT ( 'NONE',  ( -2.298420387838187473, 5.509269730139584986, -0.7346435760097105305 ) ) ;
#114573 = CARTESIAN_POINT ( 'NONE',  ( -6.073689629242151611, 10.02979563418376685, -0.7216878364870278340 ) ) ;
#114574 = CARTESIAN_POINT ( 'NONE',  ( 1.364683531249986537, 0.9052083336747533959, -0.7879004041258239610 ) ) ;
#114575 = CARTESIAN_POINT ( 'NONE',  ( 1.259612756803454525, 2.158328104161820526, -0.3793702838810895095 ) ) ;
#114576 = CARTESIAN_POINT ( 'NONE',  ( 0.1332994001262571560, 7.096108761198728132, 2.115961662170631197 ) ) ;
#114577 = CARTESIAN_POINT ( 'NONE',  ( 2.167197484064213420, -2.068651741926224474, -0.9167319039211866416 ) ) ;
#114578 = CARTESIAN_POINT ( 'NONE',  ( -8.507905087775398556, 9.884643009614800135, 1.199719254218462483 ) ) ;
#114579 = EDGE_CURVE ( 'NONE', #76194, #173148, #205256, .T. ) ;
#114580 = CARTESIAN_POINT ( 'NONE',  ( -2.426546306721660606, 5.774795091243142053, 0.7216878364870317197 ) ) ;
#114581 = CARTESIAN_POINT ( 'NONE',  ( -1.364683531250012516, 4.051041667008088432, -0.7879004041258300672 ) ) ;
#114582 = CARTESIAN_POINT ( 'NONE',  ( 11.04536101718726293, 10.90000000000000036, 1.099999999999996758 ) ) ;
#114583 = CARTESIAN_POINT ( 'NONE',  ( -0.7500000000000006661, 10.45833333333333393, -1.299038105676657340 ) ) ;
#114584 = CARTESIAN_POINT ( 'NONE',  ( 6.780486220610169035, 9.003929572168926754, -1.443375672974078761 ) ) ;
#114585 = CARTESIAN_POINT ( 'NONE',  ( 3.391635040236582022, -0.7200671834438672203, 1.616821809559340517 ) ) ;
#114586 = CARTESIAN_POINT ( 'NONE',  ( 3.158842756365538129, 0.4911626674463653863, 1.952128870646198555 ) ) ;
#114587 = CARTESIAN_POINT ( 'NONE',  ( 8.723781775389312543, 12.26516360700784958, -1.199719254218446718 ) ) ;
#114588 = CARTESIAN_POINT ( 'NONE',  ( 6.791986947960565679, -0.9495855537378705691, 1.990061496475347802 ) ) ;
#114589 = CARTESIAN_POINT ( 'NONE',  ( -0.6823417656250003738, 8.901041667008065872, 1.181850606188754593 ) ) ;
#114590 = ORIENTED_EDGE ( 'NONE', *, *, #120681, .T. ) ;
#114591 = CARTESIAN_POINT ( 'NONE',  ( -4.288121723672178476, 8.224835454251337552, -0.7998128361456362523 ) ) ;
#114592 = CARTESIAN_POINT ( 'NONE',  ( 4.605092316430917876, -0.09611821078869468848, 2.014234682242924457 ) ) ;
#114593 = ORIENTED_EDGE ( 'NONE', *, *, #210514, .T. ) ;
#114594 = CARTESIAN_POINT ( 'NONE',  ( 2.342468781959532453, 0.4075140148256419792, 1.825566309089213579 ) ) ;
#114595 = CARTESIAN_POINT ( 'NONE',  ( 3.520434184366732389, 0.9265386974339048232, 1.851387837889128640 ) ) ;
#114596 = CARTESIAN_POINT ( 'NONE',  ( -5.587368702163209910, 9.532697562583475559, 0.000000000000000000 ) ) ;
#114597 = CARTESIAN_POINT ( 'NONE',  ( 1.863391182279940494, -1.538030936729195552, -1.136358088520472931 ) ) ;
#114598 = DIRECTION ( 'NONE',  ( 0.000000000000000000, 0.000000000000000000, -1.000000000000000000 ) ) ;
#114599 = CARTESIAN_POINT ( 'NONE',  ( -10.43233925736708301, 5.066585305077033752, -5.254699789447807134 ) ) ;
#114600 = CARTESIAN_POINT ( 'NONE',  ( -4.001049302594738677, 7.679299581788098017, 0.07148048886325740481 ) ) ;
#114601 = CARTESIAN_POINT ( 'NONE',  ( -1.201851678989727383E-14, 4.509375000341417916, -1.575800808251660134 ) ) ;
#114602 = CARTESIAN_POINT ( 'NONE',  ( 1.019614524654769872, -0.4619345408787678964, 1.855657206939323789 ) ) ;
#114603 = CARTESIAN_POINT ( 'NONE',  ( 3.367582429956605061, -0.3852447139683997657, 1.923494667983568718 ) ) ;
#114604 = CARTESIAN_POINT ( 'NONE',  ( 0.4212496859960760953, 0.7689994822442263178, 1.863884711849304487 ) ) ;
#114605 = CARTESIAN_POINT ( 'NONE',  ( -5.255720823952942489, 6.160704378480398979, -1.199719254218453823 ) ) ;
#114607 = CARTESIAN_POINT ( 'NONE',  ( -11.97929049433705373, 13.88000000000000078, -0.7046979865771834106 ) ) ;
#114606 = CARTESIAN_POINT ( 'NONE',  ( 8.259941899223605333, 10.65968485389279508, -1.599625672291268286 ) ) ;
#114608 = CARTESIAN_POINT ( 'NONE',  ( 6.608667082420285332, 1.462428336960637676, -1.322156044359092064 ) ) ;
#114609 = CARTESIAN_POINT ( 'NONE',  ( -0.6823417656250212460, 2.301041667008084435, 1.181850606188767472 ) ) ;
#114610 = CARTESIAN_POINT ( 'NONE',  ( 2.320566727126192053, -0.7743817983801875027, -1.858503283895854841 ) ) ;
#114612 = CARTESIAN_POINT ( 'NONE',  ( 2.618900020153229757, 0.2622993368636802325, 2.100875384797147305 ) ) ;
#114611 = CARTESIAN_POINT ( 'NONE',  ( -5.748293942514169252, 9.650167333001109071, -0.7216878364870207285 ) ) ;
#114613 = CARTESIAN_POINT ( 'NONE',  ( 1.426714497268818382, 7.396188545894305300, 4.272650097712511474 ) ) ;
#114614 = CARTESIAN_POINT ( 'NONE',  ( 4.123533666479628046, 0.2564666318346648377, -2.054367117340555549 ) ) ;
#114615 = CARTESIAN_POINT ( 'NONE',  ( 3.725458348705031231, 7.568394850123006279, -1.734723475976807094E-15 ) ) ;
#114617 = CARTESIAN_POINT ( 'NONE',  ( 3.734381245560244089, 6.444196322207211836, 1.199719254218462483 ) ) ;
#114616 = CARTESIAN_POINT ( 'NONE',  ( 6.087849878328269071, -2.080457216024658607, -0.2059406971956292964 ) ) ;
#114619 = ORIENTED_EDGE ( 'NONE', *, *, #140892, .T. ) ;
#114618 = CARTESIAN_POINT ( 'NONE',  ( 3.698116152863577977, -1.823479002399010396, -0.09026698595545472326 ) ) ;
#114620 = CARTESIAN_POINT ( 'NONE',  ( 9.297140650669039275, 11.86975006391249643, 1.599625672291281386 ) ) ;
#114621 = SURFACE_STYLE_FILL_AREA ( #167572 ) ;
#114622 = CARTESIAN_POINT ( 'NONE',  ( 9.266412064734856457, 13.60091921773422641, 6.823019651404623964 ) ) ;
#114623 = AXIS2_PLACEMENT_3D ( 'NONE', #73228, #110090, #62337 ) ;
#114624 = CARTESIAN_POINT ( 'NONE',  ( 6.563508857876433567, 0.3837567690821128696, -2.173003994120882076 ) ) ;
#114625 = CARTESIAN_POINT ( 'NONE',  ( 1.364683531250000748, 10.81770833367473195, -0.7879004041258355073 ) ) ;
#114626 = ORIENTED_EDGE ( 'NONE', *, *, #66088, .F. ) ;
#114627 = CARTESIAN_POINT ( 'NONE',  ( 4.846305138012901637, 0.9798207982155520135, -1.642033262021398654 ) ) ;
#114628 = CARTESIAN_POINT ( 'NONE',  ( -2.272963308585411735, 5.803540959991587478, 0.7998128361456341429 ) ) ;
#114629 = CARTESIAN_POINT ( 'NONE',  ( 6.109920781252839994, 10.27999134477033216, 1.040834085586084257E-14 ) ) ;
#114630 = CARTESIAN_POINT ( 'NONE',  ( -0.6801582343750177673, 0.9635416670080582113, 1.178068619123796568 ) ) ;
#114631 = CARTESIAN_POINT ( 'NONE',  ( 4.107757354816228279, 6.775838766385488654, -1.082531754730548412 ) ) ;
#114632 = FACE_OUTER_BOUND ( 'NONE', #132331, .T. ) ;
#114633 = CARTESIAN_POINT ( 'NONE',  ( 8.116463737798994771, 14.26148076985399982, -8.779171398687106276 ) ) ;
#114634 = CARTESIAN_POINT ( 'NONE',  ( 0.2922019606856861018, 1.531309713818730822, -1.022077305420886040 ) ) ;
#114635 = ORIENTED_EDGE ( 'NONE', *, *, #167055, .F. ) ;
#114636 = AXIS2_PLACEMENT_3D ( 'NONE', #56495, #73802, #40248 ) ;
#114637 = CARTESIAN_POINT ( 'NONE',  ( -7.761116589180078407, 8.019333873657032541, 0.000000000000000000 ) ) ;
#114638 = EDGE_CURVE ( 'NONE', #153954, #112800, #111892, .T. ) ;
#114639 = CARTESIAN_POINT ( 'NONE',  ( 5.044154037833219029, 1.865456107639616556, 0.1390639465682907416 ) ) ;
#114640 = CARTESIAN_POINT ( 'NONE',  ( -1.841702881098853162, 0.1987311101661545787, 0.6151380925063570926 ) ) ;
#114641 = CARTESIAN_POINT ( 'NONE',  ( 0.000000000000000000, 13.49999999999999822, 0.000000000000000000 ) ) ;
#114642 = CARTESIAN_POINT ( 'NONE',  ( -7.049876689426106680, 9.247942109129029475, -1.443375672974059665 ) ) ;
#114643 = CARTESIAN_POINT ( 'NONE',  ( 3.662674053986138656, 7.424870162959149589, 0.7998128361456321445 ) ) ;
#114644 = CARTESIAN_POINT ( 'NONE',  ( 0.7780955915308949145, -1.048793665676364562, -1.666747765972796946 ) ) ;
#114645 = CARTESIAN_POINT ( 'NONE',  ( 2.144157856786413241, 0.8647422840215597262, 1.821734841475818101 ) ) ;
#114646 = CARTESIAN_POINT ( 'NONE',  ( -8.616370316684697883, 10.01118577667568132, -1.199719254218446718 ) ) ;
#114647 = CARTESIAN_POINT ( 'NONE',  ( 3.881377115262159894, 7.750300077773022878, 0.7998128361456271485 ) ) ;
#114648 = CARTESIAN_POINT ( 'NONE',  ( 6.716119544743627934, -7.217450603038206403, 6.719405205104847845 ) ) ;
#114649 = CARTESIAN_POINT ( 'NONE',  ( 2.027518650255655253, -1.432890729411402830, -1.658174735819065049 ) ) ;
#114650 = CARTESIAN_POINT ( 'NONE',  ( 1.214306433183764966E-14, 2.428612866367529932E-14, 1.500000000000001332 ) ) ;
#114651 = CARTESIAN_POINT ( 'NONE',  ( -8.435144125996554720, 12.99275191363802229, 0.7998128361456341429 ) ) ;
#114652 = CARTESIAN_POINT ( 'NONE',  ( 0.6823417656249899377, 3.092708333674754062, 1.181850606188765695 ) ) ;
#114653 = DIRECTION ( 'NONE',  ( 0.0006885664517736132502, 0.9962285034897219171, -0.08676574618402704830 ) ) ;
#114654 = CARTESIAN_POINT ( 'NONE',  ( 3.879041347285658414, 6.579279767591636130, -1.082531754730548412 ) ) ;
#114655 = CARTESIAN_POINT ( 'NONE',  ( 8.555358625423188812, 9.940005470203933768, 1.199719254218462483 ) ) ;
#114656 = CARTESIAN_POINT ( 'NONE',  ( -9.445420027513430128, 14.68120331434907300, 7.300025634049736922 ) ) ;
#114657 = CARTESIAN_POINT ( 'NONE',  ( 6.455090533882185788, 8.624301270986276080, -1.443375672974078761 ) ) ;
#114658 = ORIENTED_EDGE ( 'NONE', *, *, #32785, .F. ) ;
#114660 = CARTESIAN_POINT ( 'NONE',  ( 2.156891369321057628, 0.4431265858878992159, 1.963560470019373172 ) ) ;
#114659 = CARTESIAN_POINT ( 'NONE',  ( 4.388128076750056117, -0.4078595375654435751, -1.795341762384855544 ) ) ;
#114661 = CARTESIAN_POINT ( 'NONE',  ( 3.357065504480163387, -0.9345643552367989271, 2.099969358187879109 ) ) ;
#114663 = CARTESIAN_POINT ( 'NONE',  ( 1.041598845562411890, 1.244476351500271472, 1.383831004058704961 ) ) ;
#114662 = CARTESIAN_POINT ( 'NONE',  ( -1.500000000000008216, 10.00000000000000178, 3.469446951953614189E-15 ) ) ;
#114664 = CARTESIAN_POINT ( 'NONE',  ( -3.285556943750000070, -1.859374999522041882, 0.000000000000000000 ) ) ;
#114665 = CARTESIAN_POINT ( 'NONE',  ( 6.983263157960365675, -0.006178392973848687020, 2.053544886540019210 ) ) ;
#114666 = CARTESIAN_POINT ( 'NONE',  ( 5.748291730981218706, 0.9368611416523886515, -1.667099895225135686 ) ) ;
#114667 = CARTESIAN_POINT ( 'NONE',  ( -8.320953590485107298, 10.73086516036454618, 1.599625672291269396 ) ) ;
#114668 = CARTESIAN_POINT ( 'NONE',  ( -5.804299160426229953, 8.825413882922319431, -1.082531754730549967 ) ) ;
#114670 = CARTESIAN_POINT ( 'NONE',  ( 3.748781033766034998, -1.529746656882627454, 1.076398355447941491 ) ) ;
#114669 = CARTESIAN_POINT ( 'NONE',  ( 5.038659576058011957, -1.792549807278142726, 1.075873411605046348 ) ) ;
#114671 = CARTESIAN_POINT ( 'NONE',  ( 7.795575138177731844, 8.197185204069915798, 1.040834085586084257E-14 ) ) ;
#114672 = EDGE_CURVE ( 'NONE', #87474, #185401, #9326, .T. ) ;
#114673 = CARTESIAN_POINT ( 'NONE',  ( 5.337399561049260832, 0.7408347518493042516, -1.685818907712175019 ) ) ;
#114674 = CARTESIAN_POINT ( 'NONE',  ( 5.007038802148489509, 4.735966778795008381, 0.7998128361456341429 ) ) ;
#114675 = CARTESIAN_POINT ( 'NONE',  ( -5.151735183512911043, 6.073074471262228435, 1.082531754730548412 ) ) ;
#114676 = CARTESIAN_POINT ( 'NONE',  ( 5.619686913847246501, -1.681401280226066941, 0.3840984716911073349 ) ) ;
#114677 = CARTESIAN_POINT ( 'NONE',  ( -7.888146445052511169, 8.097259028849730811, 1.040834085586084257E-14 ) ) ;
#114678 = CARTESIAN_POINT ( 'NONE',  ( 0.6504783628028444342, 0.8526279987398683868, 1.509985294034902337 ) ) ;
#114679 = CYLINDRICAL_SURFACE ( 'NONE', #158118, 11.99999999999999112 ) ;
#114680 = COLOUR_RGB ( '', 0.08235294, 0.09019608, 0.10196078) ;
#114681 =( NAMED_UNIT ( * ) SI_UNIT ( $, .STERADIAN. ) SOLID_ANGLE_UNIT ( ) );
#114682 = CARTESIAN_POINT ( 'NONE',  ( 4.944265959323273840, -1.029449158807031361, 1.911525048081736955 ) ) ;
#114683 = CARTESIAN_POINT ( 'NONE',  ( 3.299243935302543118, 1.439784963707075649, 1.122460502641378755 ) ) ;
#114684 = CARTESIAN_POINT ( 'NONE',  ( 0.6726124357511429341, 1.356994209013298036, -1.416925378234991095 ) ) ;
#114685 = CARTESIAN_POINT ( 'NONE',  ( 5.384029865600029829, -2.117513407852515073, 0.002815966404249789501 ) ) ;
#114686 = VECTOR ( 'NONE', #31729, 999.9999999999998863 ) ;
#114688 = CARTESIAN_POINT ( 'NONE',  ( 1.364683531249988535, 4.467708333674754506, -0.7879004041258300672 ) ) ;
#114687 = CARTESIAN_POINT ( 'NONE',  ( 5.706620831843001618, 2.020032061211772589, 1.083668233456626551 ) ) ;
#114689 = CARTESIAN_POINT ( 'NONE',  ( 7.727257484784855635, 11.10255193463598111, -1.199719254218446718 ) ) ;
#114690 = CARTESIAN_POINT ( 'NONE',  ( 0.8738735914427527840, 0.4098651554323496926, -2.080331290949386513 ) ) ;
#114691 = CARTESIAN_POINT ( 'NONE',  ( -4.365362273920257330, 6.116008624372160973, 1.443375672974064550 ) ) ;
#114692 = CARTESIAN_POINT ( 'NONE',  ( -4.894130264408873110, 5.772535398974209642, -1.082531754730543971 ) ) ;
#114693 = CARTESIAN_POINT ( 'NONE',  ( 6.614155491087242211, 2.165850671381476023, -0.1511765098734293433 ) ) ;
#114695 = CARTESIAN_POINT ( 'NONE',  ( -0.7500000000000006661, 12.98958333401613352, -1.299038105676657340 ) ) ;
#114694 = CARTESIAN_POINT ( 'NONE',  ( 6.883263157960364254, 4.694764272337425659, 2.516417202187768432 ) ) ;
#114697 = ORIENTED_EDGE ( 'NONE', *, *, #93021, .T. ) ;
#114696 = CARTESIAN_POINT ( 'NONE',  ( 2.192296887966191488, 1.369148959659401754, 1.749082743080948799 ) ) ;
#114698 = CARTESIAN_POINT ( 'NONE',  ( 6.223279759862190730, 1.994869330463379331, 0.2930738960792296233 ) ) ;
#114700 = CARTESIAN_POINT ( 'NONE',  ( 5.629752743445687990, 1.989327071453067752, -0.5446528645957140480 ) ) ;
#114699 = CARTESIAN_POINT ( 'NONE',  ( 5.009901455449552010, 5.803638771901306725, -1.199719254218452047 ) ) ;
#114702 = CARTESIAN_POINT ( 'NONE',  ( -3.474999999999998312, -3.470833333333334103, 2.006292185433951047 ) ) ;
#114701 = CARTESIAN_POINT ( 'NONE',  ( 4.667750024854814050, 8.667735138964429709, -0.7998128361456381397 ) ) ;
#114703 = CARTESIAN_POINT ( 'NONE',  ( 4.213551878797002992, 8.137837301896977849, 0.000000000000000000 ) ) ;
#114704 = CARTESIAN_POINT ( 'NONE',  ( -1.642778471874998480, -3.988541666188710089, 2.845375778867863303 ) ) ;
#114705 = CARTESIAN_POINT ( 'NONE',  ( 1.244123718695680836, 2.983005466778237746, 0.7750000000000100142 ) ) ;
#114706 = CARTESIAN_POINT ( 'NONE',  ( 4.792441439910442469, 1.527937338083688923, -1.027124420945781935 ) ) ;
#114707 = EDGE_CURVE ( 'NONE', #106531, #182678, #108556, .T. ) ;
#114708 = CARTESIAN_POINT ( 'NONE',  ( 5.355634372598031767, 6.206993841907870291, -1.199719254218445830 ) ) ;
#114709 = SURFACE_STYLE_FILL_AREA ( #193747 ) ;
#114710 = CARTESIAN_POINT ( 'NONE',  ( 1.377515174558477273, 1.023066641755419282, 1.388426169202553018 ) ) ;
#114711 = CARTESIAN_POINT ( 'NONE',  ( -0.1003747550864658999, -1.976661868047492998, 0.3981153667176607902 ) ) ;
#114712 = CARTESIAN_POINT ( 'NONE',  ( 1.442429577410338615, -1.974492438002553918, -1.176823363874231587 ) ) ;
#114713 = CARTESIAN_POINT ( 'NONE',  ( -0.6823417656250212460, 3.863541667008085767, 1.181850606188767472 ) ) ;
#114714 = CARTESIAN_POINT ( 'NONE',  ( 1.353188757747030957, -1.783583821274600911, 1.391813662893444548 ) ) ;
#114715 = CARTESIAN_POINT ( 'NONE',  ( 3.932330475907989342, 1.126754335618613379, -1.779114833428483866 ) ) ;
#114716 = CARTESIAN_POINT ( 'NONE',  ( -3.311934663488232733, 7.085950550703385531, -0.7998128361456481317 ) ) ;
#114717 = CARTESIAN_POINT ( 'NONE',  ( 2.424752316626857862, -0.004995123648579914352, 1.769921776121333945 ) ) ;
#114718 = CARTESIAN_POINT ( 'NONE',  ( 7.610204295972345712, 7.772993188256215547, 0.7998128361456341429 ) ) ;
#114719 = CARTESIAN_POINT ( 'NONE',  ( 6.021229617800532452, 6.197391773621639288, 0.000000000000000000 ) ) ;
#114720 = CARTESIAN_POINT ( 'NONE',  ( -5.656776405399756236, 7.622658444431597680, -1.599625672291256295 ) ) ;
#114721 = CARTESIAN_POINT ( 'NONE',  ( -1.402160292154681736E-14, 2.087500000000021227, -1.732050807568863648 ) ) ;
#114722 = CARTESIAN_POINT ( 'NONE',  ( 5.414381242519362480, -2.221583670654456721, 0.0001252536179462138133 ) ) ;
#114723 = CARTESIAN_POINT ( 'NONE',  ( 3.591891977137162684, -2.188917585555647527, -0.1077332384093188100 ) ) ;
#114724 = CARTESIAN_POINT ( 'NONE',  ( -5.786632634934295361, 5.645492917045106473, 0.7998128361456341429 ) ) ;
#114725 = CARTESIAN_POINT ( 'NONE',  ( 0.4652101495396396280, -7.972382850425330680, 9.716492259128738596 ) ) ;
#114726 = CARTESIAN_POINT ( 'NONE',  ( -0.6823417656250212460, 3.551041667008085323, 1.181850606188767472 ) ) ;
#114727 = CARTESIAN_POINT ( 'NONE',  ( 6.890000000000010338, 4.693995042360769254, 2.562605081426703180 ) ) ;
#114728 = CARTESIAN_POINT ( 'NONE',  ( -5.273758566035884776, 5.255065869904374409, 0.000000000000000000 ) ) ;
#114729 = CARTESIAN_POINT ( 'NONE',  ( 5.642871316567687145, 2.044259226470702462, 0.5637153772257290640 ) ) ;
#114730 = CARTESIAN_POINT ( 'NONE',  ( -6.536439455564198475, 8.719208346281938304, 1.443375672974064550 ) ) ;
#114731 = VERTEX_POINT ( 'NONE', #212373 ) ;
#114733 = CARTESIAN_POINT ( 'NONE',  ( -3.904385051055635270, 6.538571078664754843, 1.082531754730560403 ) ) ;
#114732 = CARTESIAN_POINT ( 'NONE',  ( -4.014622883422322985, 7.697827440719083647, -0.7216878364870458196 ) ) ;
#114734 = CARTESIAN_POINT ( 'NONE',  ( 5.168682875307768931, 7.053215992657626110, -1.599625672291256295 ) ) ;
#114735 = CARTESIAN_POINT ( 'NONE',  ( 6.198766299729112639, 1.534709720371667308, 1.016988835930050739 ) ) ;
#114736 = FACE_OUTER_BOUND ( 'NONE', #75150, .T. ) ;
#114737 = CARTESIAN_POINT ( 'NONE',  ( -1.201851678989727383E-14, 4.009375000341416140, -1.575800808251660134 ) ) ;
#114738 = CARTESIAN_POINT ( 'NONE',  ( 1.926944929849357280, -1.137335869680399902, -1.317475996949101669 ) ) ;
#114739 = CARTESIAN_POINT ( 'NONE',  ( 2.171277156482887882, 5.684907115872006145, -0.7998128361456291469 ) ) ;
#114740 = CARTESIAN_POINT ( 'NONE',  ( 1.499999999999996891, 10.92708333401613707, -0.8660254037844378194 ) ) ;
#114741 = CARTESIAN_POINT ( 'NONE',  ( -1.364683531250000748, -0.4281249996585800854, 0.000000000000000000 ) ) ;
#114742 = CARTESIAN_POINT ( 'NONE',  ( -0.4307572970102932497, 3.041534709929986313, -0.4240169840791543354 ) ) ;
#114743 = CARTESIAN_POINT ( 'NONE',  ( 6.473507614529132148, 2.070149491355821159, -0.6224772505839873959 ) ) ;
#114744 = CARTESIAN_POINT ( 'NONE',  ( -3.436101866059630527, 6.096203712789787232, 1.199719254218462483 ) ) ;
#114745 = AXIS2_PLACEMENT_3D ( 'NONE', #175767, #172561, #158440 ) ;
#114746 = CARTESIAN_POINT ( 'NONE',  ( -5.043269954159181445, 8.827639346586952485, 1.214306433183764966E-14 ) ) ;
#114747 = CARTESIAN_POINT ( 'NONE',  ( 5.436455051933180016, 2.129025116502227810, 0.3735886874452337691 ) ) ;
#114749 = ORIENTED_EDGE ( 'NONE', *, *, #55036, .T. ) ;
#114748 = LINE ( 'NONE', #63796, #146766 ) ;
#114750 = CARTESIAN_POINT ( 'NONE',  ( 0.6823417656249882723, 2.676041667008084879, -1.181850606188749264 ) ) ;
#114751 = CARTESIAN_POINT ( 'NONE',  ( 6.327413238363588377, -1.857107522167710245, 0.6617740914907597194 ) ) ;
#114752 = CARTESIAN_POINT ( 'NONE',  ( 4.622224120573574346, 0.3796314994632241646, -1.691551752166654543 ) ) ;
#114753 = ADVANCED_FACE ( 'NONE', ( #192931 ), #128361, .T. ) ;
#114755 = CARTESIAN_POINT ( 'NONE',  ( 1.628746693258641853, 0.2190750365392846177, 2.180598679842937759 ) ) ;
#114754 = CARTESIAN_POINT ( 'NONE',  ( -1.360316468750032870, -1.088541666325267165, 0.7853790794158641564 ) ) ;
#114756 = CARTESIAN_POINT ( 'NONE',  ( 2.890017657663559891, 1.631080081281432559, 1.632583592418336282 ) ) ;
#114757 = CARTESIAN_POINT ( 'NONE',  ( 4.868464682339723737, -1.349271924330990080, 1.557713215823807174 ) ) ;
#114758 = CARTESIAN_POINT ( 'NONE',  ( 1.218581363712217591, -0.04816221259190026777, 1.941509521754792855 ) ) ;
#114759 = CARTESIAN_POINT ( 'NONE',  ( -5.707619481228814351, 9.602713794834864203, -0.7216878364870207285 ) ) ;
#114761 = EDGE_CURVE ( 'NONE', #196200, #50747, #75748, .T. ) ;
#114760 = CARTESIAN_POINT ( 'NONE',  ( -3.546339698426324460, 6.295090860542775779, -1.199719254218450271 ) ) ;
#114762 = CARTESIAN_POINT ( 'NONE',  ( -0.1108833634136767443, 0.0002062650063822807356, -1.896853557917008271 ) ) ;
#114763 = CARTESIAN_POINT ( 'NONE',  ( 4.025719079702368752, -0.3592959752154977204, 2.089770972018199835 ) ) ;
#114764 = CARTESIAN_POINT ( 'NONE',  ( 0.9146856577476671912, -1.281363086869342194, -1.556907195799726917 ) ) ;
#114765 = CARTESIAN_POINT ( 'NONE',  ( -4.839897649954225223, 7.630002444046455778, 1.082531754730560403 ) ) ;
#114766 = CARTESIAN_POINT ( 'NONE',  ( 4.401547605996741552, 1.770323140634282311, 1.317293360403009927 ) ) ;
#114767 = CARTESIAN_POINT ( 'NONE',  ( 0.000000000000000000, 1.551257596039481879, 0.000000000000000000 ) ) ;
#114768 = CARTESIAN_POINT ( 'NONE',  ( -8.043940816608023070, -6.893137084989708008, 7.503508839934920793 ) ) ;
#114769 = CARTESIAN_POINT ( 'NONE',  ( -8.072954122294394352, 8.383144328957069291, -0.7998128361456362523 ) ) ;
#114770 = CARTESIAN_POINT ( 'NONE',  ( -5.543378919943204863, 7.538303290789565736, -1.349654061105177050 ) ) ;
#114771 = CARTESIAN_POINT ( 'NONE',  ( 0.07378579499363849270, 7.051136084633868428, 3.951055989447525896 ) ) ;
#114772 = ORIENTED_EDGE ( 'NONE', *, *, #106908, .T. ) ;
#114773 = CARTESIAN_POINT ( 'NONE',  ( 4.698151523293167209, -2.060395484190484794, -0.05257267949314303745 ) ) ;
#114774 = CARTESIAN_POINT ( 'NONE',  ( 1.360316468749965590, 2.494791667008093849, 0.7853790794158861388 ) ) ;
#114775 = CARTESIAN_POINT ( 'NONE',  ( 0.3846410972798547934, -8.199730735666078019, 9.492545994384032682 ) ) ;
#114776 = CARTESIAN_POINT ( 'NONE',  ( -5.590039407536138150, 5.416134151747256986, 0.000000000000000000 ) ) ;
#114777 = CARTESIAN_POINT ( 'NONE',  ( 3.299477536675638145, 1.824990673169521793, -0.8654797531507262276 ) ) ;
#114778 = CARTESIAN_POINT ( 'NONE',  ( -1.500000000000001332, -0.3499999999999753308, 0.000000000000000000 ) ) ;
#114779 = CARTESIAN_POINT ( 'NONE',  ( 9.029367117021314115, 12.51771682229149008, -1.082531754730543083 ) ) ;
#114780 = CARTESIAN_POINT ( 'NONE',  ( 8.620286740190458374, 8.951422706510690830, 1.040834085586084257E-14 ) ) ;
#114781 = COLOUR_RGB ( '', 0.72549020, 0.75294118, 0.79215686) ;
#114782 = CARTESIAN_POINT ( 'NONE',  ( 2.940362659251498645, 2.045167860313545916, 0.2535661900368457733 ) ) ;
#114783 = DIRECTION ( 'NONE',  ( -0.000000000000000000, 1.000000000000000000, -0.000000000000000000 ) ) ;
#114784 = CARTESIAN_POINT ( 'NONE',  ( 6.342516933094585418, 6.294024598232139667, 1.040834085586084257E-14 ) ) ;
#114785 = CARTESIAN_POINT ( 'NONE',  ( -0.1411974294642202310, 0.2398548052158452348, -1.934266582396115819 ) ) ;
#114786 = CARTESIAN_POINT ( 'NONE',  ( 1.183273638618479673, -0.8294958387620559037, 1.643756842616146630 ) ) ;
#114787 = CARTESIAN_POINT ( 'NONE',  ( -0.004676085075996058368, -0.5178430341337829645, -2.257629771169813448 ) ) ;
#114788 = CARTESIAN_POINT ( 'NONE',  ( 6.496291879603339758, 7.608037276739255006, 1.199719254218452935 ) ) ;
#114789 = CARTESIAN_POINT ( 'NONE',  ( 2.565889408427945995, 2.120439650033152379, -0.4189318973958494619 ) ) ;
#114790 = CARTESIAN_POINT ( 'NONE',  ( -3.145128448690310830, 6.613140923539910787, -0.7216878364870267237 ) ) ;
#114791 = CARTESIAN_POINT ( 'NONE',  ( 1.534389036647098692, 0.6371565916030231813, 1.913260934284975345 ) ) ;
#114792 = TOROIDAL_SURFACE ( 'NONE', #183828, 3.399419719642636561, 0.1000000000000000056 ) ;
#114793 = CARTESIAN_POINT ( 'NONE',  ( 2.917634960997887994, 0.7719352619847442698, 2.165007881682521784 ) ) ;
#114794 = CARTESIAN_POINT ( 'NONE',  ( 0.3999999999999758193, 3.000000000029069636, -2.023857702507768419 ) ) ;
#114795 = CARTESIAN_POINT ( 'NONE',  ( 0.3911966820569385828, 1.383097094795827209, 1.259704262696823118 ) ) ;
#114796 = CARTESIAN_POINT ( 'NONE',  ( 4.750830034454851969, -1.584041870840187327, 1.173487520707878096 ) ) ;
#114797 = CARTESIAN_POINT ( 'NONE',  ( 4.259000112335223243, -0.004834882008357410665, -2.016708403958865414 ) ) ;
#114799 = CARTESIAN_POINT ( 'NONE',  ( 10.18181017373857067, 11.94149529319227909, 1.082531754730548412 ) ) ;
#114798 = CARTESIAN_POINT ( 'NONE',  ( 0.6823417656249899377, 2.342708333674753618, 1.181850606188767472 ) ) ;
#114801 = CARTESIAN_POINT ( 'NONE',  ( 6.410775461673044795, 1.561785836243877235, -1.413106494374539945 ) ) ;
#114800 = CARTESIAN_POINT ( 'NONE',  ( -5.377780486114890124, 9.425827667109372143, 0.000000000000000000 ) ) ;
#114802 = CARTESIAN_POINT ( 'NONE',  ( 6.830528382861658088, -1.277203763263988101, 1.630111558092485868 ) ) ;
#114803 = CARTESIAN_POINT ( 'NONE',  ( 5.147291874682557555, 9.156924287104992288, 0.7998128361456462443 ) ) ;
#114804 = CARTESIAN_POINT ( 'NONE',  ( -5.768104287610143821, 8.816873204598778102, -1.199719254218440723 ) ) ;
#114805 = CARTESIAN_POINT ( 'NONE',  ( 1.997523430356448193, 3.481192892629490832, -0.3999999999998126721 ) ) ;
#114806 = CARTESIAN_POINT ( 'NONE',  ( 4.763928514684708126, 0.6297656808758389513, -1.919195086291412888 ) ) ;
#114807 = CARTESIAN_POINT ( 'NONE',  ( -1.500000000000001332, 0.9312500006828163812, 0.000000000000000000 ) ) ;
#114808 = CARTESIAN_POINT ( 'NONE',  ( 3.510674805948321264, -0.9346715503392712954, -2.110115307156499753 ) ) ;
#114809 = CARTESIAN_POINT ( 'NONE',  ( 2.289955638094377299, -1.343889277006144356, -1.564782475634781900 ) ) ;
#114810 = CARTESIAN_POINT ( 'NONE',  ( 8.432808358020029260, 8.940623960552603222, 0.7216878364870438212 ) ) ;
#114811 = CARTESIAN_POINT ( 'NONE',  ( 7.354371980770088690, 7.544798497178720531, 0.000000000000000000 ) ) ;
#114812 = CARTESIAN_POINT ( 'NONE',  ( 5.845500506147374153, 6.848780674373954547, 1.199719254218453823 ) ) ;
#114813 = CARTESIAN_POINT ( 'NONE',  ( -1.364683531250014514, 0.3427083336747508424, 0.7879004041258379498 ) ) ;
#114814 = CARTESIAN_POINT ( 'NONE',  ( 5.578253857379852576, 5.472660686556754861, -0.7998128361456481317 ) ) ;
#114815 = CARTESIAN_POINT ( 'NONE',  ( 6.222829318548112276, 9.243422724072711816, -1.082531754730537976 ) ) ;
#114816 = CARTESIAN_POINT ( 'NONE',  ( 4.053319971960964274, 1.836175303466779374, -1.158372938815607656 ) ) ;
#114817 = CARTESIAN_POINT ( 'NONE',  ( -2.511332776996739291, -0.8887487162373162164, -2.129472066838233868 ) ) ;
#114819 = CARTESIAN_POINT ( 'NONE',  ( 2.858754248528099229, 0.2676582106064147593, -1.821554178878769470 ) ) ;
#114818 = CARTESIAN_POINT ( 'NONE',  ( -5.599154252763867134, 5.634694171087028636, 0.000000000000000000 ) ) ;
#114820 = CARTESIAN_POINT ( 'NONE',  ( -0.6823417656250212460, 4.051041667008085767, 1.181850606188767472 ) ) ;
#114821 = CARTESIAN_POINT ( 'NONE',  ( 3.878626735558046157, -0.2160506499642600997, -2.180900317982924275 ) ) ;
#114822 = DIRECTION ( 'NONE',  ( -5.578564026256490882E-16, -1.000000000000000000, -9.066213480720158442E-32 ) ) ;
#114823 = CARTESIAN_POINT ( 'NONE',  ( 5.946200445400964263, 2.259567648220105252, 0.1180026366056959042 ) ) ;
#114824 = CARTESIAN_POINT ( 'NONE',  ( -5.969600656924041182, 6.101865228085409321, -0.7346798775042752139 ) ) ;
#114825 = CARTESIAN_POINT ( 'NONE',  ( 5.559975706299111309, 7.414571502401146930, -1.245397951563255834 ) ) ;
#114826 = CARTESIAN_POINT ( 'NONE',  ( -6.305950843687521790, 7.489935751457798219, 1.082531754730548412 ) ) ;
#114827 = CARTESIAN_POINT ( 'NONE',  ( 4.502716413514295191, 6.346531463890372926, -1.443375672974068769 ) ) ;
#114828 = CARTESIAN_POINT ( 'NONE',  ( 6.749276393231373739, -1.423207027788903067, -1.051611706393209111 ) ) ;
#114829 = PRESENTATION_LAYER_ASSIGNMENT (  '', '', ( #142334 ) ) ;
#114830 = CARTESIAN_POINT ( 'NONE',  ( 3.721343298090164620, 1.727675083452884897, 1.033047338021097383 ) ) ;
#114831 = CARTESIAN_POINT ( 'NONE',  ( 5.933664784275179294, 10.07435934829639912, -0.7998128361456291469 ) ) ;
#114832 = CARTESIAN_POINT ( 'NONE',  ( 3.452270085047473458, 2.106147100029008179, 0.001788861226008006461 ) ) ;
#114833 = CARTESIAN_POINT ( 'NONE',  ( 1.792461972651203439, 1.418048008323580911, -1.288064678409290398 ) ) ;
#114834 = AXIS2_PLACEMENT_3D ( 'NONE', #134552, #197375, #148644 ) ;
#114835 = CARTESIAN_POINT ( 'NONE',  ( 3.979481780810941949, 4.601482484822914998, 1.199719254218464037 ) ) ;
#114836 = CARTESIAN_POINT ( 'NONE',  ( 3.578522297727056767, 1.251517597477384447, -1.520772613757546354 ) ) ;
#114837 = CARTESIAN_POINT ( 'NONE',  ( 0.8306673739700667358, 0.1335802410974036292, 1.865940672528036304 ) ) ;
#114838 = CARTESIAN_POINT ( 'NONE',  ( 1.363640982571033611, -0.4799814350611387725, 1.902108589862220311 ) ) ;
#114840 = VERTEX_POINT ( 'NONE', #201192 ) ;
#114839 = CARTESIAN_POINT ( 'NONE',  ( 0.6153073421325053749, 1.564839666810373231, 1.099065937236625157 ) ) ;
#114841 = CARTESIAN_POINT ( 'NONE',  ( 4.365362273920230685, 8.036747052974847705, 0.7216878364870298324 ) ) ;
#114842 = CARTESIAN_POINT ( 'NONE',  ( 1.364683531249988757, 0.9468750003414211358, 0.000000000000000000 ) ) ;
#114843 = CARTESIAN_POINT ( 'NONE',  ( 6.543822781336226413, 0.7137633992815132222, -1.729328153040734728 ) ) ;
#114844 = CARTESIAN_POINT ( 'NONE',  ( 3.728655938958122196, 4.308852335994623139, -1.199719254218446718 ) ) ;
#114845 = FACE_OUTER_BOUND ( 'NONE', #167037, .T. ) ;
#114846 = CARTESIAN_POINT ( 'NONE',  ( 6.315297747118990834, -1.772576088781053327, -1.069364167438614732 ) ) ;
#114847 = FILL_AREA_STYLE_COLOUR ( '', #197695 ) ;
#114848 = CARTESIAN_POINT ( 'NONE',  ( 0.7661813929631040576, -2.060537521029872643, 0.2012509062776293156 ) ) ;
#114849 = CARTESIAN_POINT ( 'NONE',  ( -1.500000000000013101, 2.420833333333359150, 0.8660254037844403729 ) ) ;
#114850 = CARTESIAN_POINT ( 'NONE',  ( 5.262536180398716290, 9.291375977107183104, -0.7998128361456291469 ) ) ;
#114851 = CARTESIAN_POINT ( 'NONE',  ( -9.176171038350775078, 9.599954387697719582, -0.7998128361456291469 ) ) ;
#114852 = CARTESIAN_POINT ( 'NONE',  ( 4.179656494762836516, 8.098292687190454586, -0.7998128361456362523 ) ) ;
#114853 = CARTESIAN_POINT ( 'NONE',  ( 5.197945112634200449, 1.424400718755761908, 1.570990128125760554 ) ) ;
#114854 = CARTESIAN_POINT ( 'NONE',  ( 2.925527285498711549, 6.635141943048991742, 0.7998128361456281477 ) ) ;
#114855 = CARTESIAN_POINT ( 'NONE',  ( 1.364683531249986537, 1.655208333674748955, -0.7879004041258239610 ) ) ;
#114856 = ORIENTED_EDGE ( 'NONE', *, *, #165594, .F. ) ;
#114857 = CARTESIAN_POINT ( 'NONE',  ( 1.499999999999989120, 2.775000000000020339, 1.214306433183764966E-14 ) ) ;
#114859 = CARTESIAN_POINT ( 'NONE',  ( 4.521807925357579805, 5.234196320127330715, -1.199719254218452047 ) ) ;
#114858 = CARTESIAN_POINT ( 'NONE',  ( 6.689906388054261299, -1.280585065398877731, -1.486383542710856043 ) ) ;
#114860 = CARTESIAN_POINT ( 'NONE',  ( 4.358749857130030492, -0.7741967591250037417, 1.861731939633674893 ) ) ;
#114861 = CARTESIAN_POINT ( 'NONE',  ( 3.960093407954877520, -1.098340823217320184, 1.569403885630010320 ) ) ;
#114862 = CARTESIAN_POINT ( 'NONE',  ( -1.911686719268524293, 3.274494700676914949, -0.4236673858377688062 ) ) ;
#114863 = CARTESIAN_POINT ( 'NONE',  ( 1.452940684028160234, -1.882004992133184285, -1.122693704575933316 ) ) ;
#114864 = CARTESIAN_POINT ( 'NONE',  ( 0.1333692844072559558, 0.7140749627707367875, -2.136770008611441618 ) ) ;
#114865 = CARTESIAN_POINT ( 'NONE',  ( 2.952262541859524969, 0.6266372353985818489, 1.762611677789377440 ) ) ;
#114866 = CARTESIAN_POINT ( 'NONE',  ( -1.602468905319636405E-14, -1.131249999317182064, -1.732050807568870754 ) ) ;
#114867 = CARTESIAN_POINT ( 'NONE',  ( -6.669721502918952716, 9.868759955792373972, 1.199719254218452047 ) ) ;
#114869 = CARTESIAN_POINT ( 'NONE',  ( 5.765271170472290763, 1.955999355395316996, -0.8108409051663100220 ) ) ;
#114868 = CARTESIAN_POINT ( 'NONE',  ( -4.067082894419624672, 6.728385229256075739, 1.082531754730560403 ) ) ;
#114870 = CARTESIAN_POINT ( 'NONE',  ( 0.000000000000000000, 4.400000000000001243, 0.000000000000000000 ) ) ;
#114872 = CARTESIAN_POINT ( 'NONE',  ( -7.795011973214244883, 8.058878488363559356, 0.7998128361456341429 ) ) ;
#114871 = CARTESIAN_POINT ( 'NONE',  ( 1.804351596996961238, 1.546985077243122397, -1.406606537801007972 ) ) ;
#114874 = ORIENTED_EDGE ( 'NONE', *, *, #133578, .T. ) ;
#114873 = CARTESIAN_POINT ( 'NONE',  ( 0.3051044079889728144, -0.4676614632079054701, 1.660094367756638434 ) ) ;
#114875 = CARTESIAN_POINT ( 'NONE',  ( 6.154511665599609493, 9.267681812253174556, 1.199719254218462483 ) ) ;
#114876 = ADVANCED_FACE ( 'NONE', ( #183895 ), #172560, .F. ) ;
#114877 = CARTESIAN_POINT ( 'NONE',  ( 1.579999999999985860, -1.099999999999976108, 2.579999999999999183 ) ) ;
#114879 =( GEOMETRIC_REPRESENTATION_CONTEXT ( 3 ) GLOBAL_UNCERTAINTY_ASSIGNED_CONTEXT ( ( #144821 ) ) GLOBAL_UNIT_ASSIGNED_CONTEXT ( ( #173998, #27715, #125301 ) ) REPRESENTATION_CONTEXT ( 'NONE', 'WORKASPACE' ) );
#114878 = CARTESIAN_POINT ( 'NONE',  ( 0.6124999999999776179, 0.8333333333333594606, 1.060881119635894487 ) ) ;
#114880 = CARTESIAN_POINT ( 'NONE',  ( -2.632154883592737318E-16, -9.671843677217918156, 9.585733692702627096 ) ) ;
#114882 = CARTESIAN_POINT ( 'NONE',  ( 9.531018800282605952, 11.18223869082697597, 1.082531754730548412 ) ) ;
#114881 = CARTESIAN_POINT ( 'NONE',  ( 7.169564303528210836, 7.258913197071374945, -0.7998128361456281477 ) ) ;
#114883 = DIRECTION ( 'NONE',  ( 3.706092522800016599E-15, 0.000000000000000000, 1.000000000000000000 ) ) ;
#114885 = CARTESIAN_POINT ( 'NONE',  ( 1.207327558334120754, 1.371319684050668730, 1.183719584703796679 ) ) ;
#114884 = CARTESIAN_POINT ( 'NONE',  ( 4.694866332082116678, 8.699370830729650450, 0.7998128361456341429 ) ) ;
#114886 = CARTESIAN_POINT ( 'NONE',  ( -7.019370843573183194, 9.212351955633947043, 1.599625672291283607 ) ) ;
#114887 = CARTESIAN_POINT ( 'NONE',  ( 4.704842999142070603, 5.447737239542574272, -1.199719254218452047 ) ) ;
#114888 = CARTESIAN_POINT ( 'NONE',  ( -6.470902446588409518, 6.777469385738574381, 0.2989120342885512871 ) ) ;
#114889 = CARTESIAN_POINT ( 'NONE',  ( 7.035755370848908896, 7.173079118937375931, 0.7998128361456352531 ) ) ;
#114890 = DIRECTION ( 'NONE',  ( -0.000000000000000000, 1.000000000000000000, -0.000000000000000000 ) ) ;
#114891 = CARTESIAN_POINT ( 'NONE',  ( 3.915468285211845848E-16, 4.500000000000003553, -2.149999999999999911 ) ) ;
#114892 = CARTESIAN_POINT ( 'NONE',  ( 4.016016189339381981, 7.573203028563332495, -0.3002613606930375489 ) ) ;
#114893 = CARTESIAN_POINT ( 'NONE',  ( 10.07334494527360569, 10.85458331234846696, 0.000000000000000000 ) ) ;
#114894 = ADVANCED_FACE ( 'NONE', ( #37653 ), #207318, .F. ) ;
#114895 = CARTESIAN_POINT ( 'NONE',  ( 3.033498015644376267, 1.768043114356824930, -0.5812464218588138110 ) ) ;
#114896 = EDGE_CURVE ( 'NONE', #120419, #24390, #136775, .T. ) ;
#114897 = CARTESIAN_POINT ( 'NONE',  ( 0.1928052069046156669, 1.667086954950956157, 0.9433992581227236274 ) ) ;
#114898 = CARTESIAN_POINT ( 'NONE',  ( 6.282248997152713343, -1.030047846951231971, 1.627708832905690350 ) ) ;
#114899 = CARTESIAN_POINT ( 'NONE',  ( 6.250451049865752395, -2.060019788584551481, -0.2068627631737207651 ) ) ;
#114900 =( NAMED_UNIT ( * ) SI_UNIT ( $, .STERADIAN. ) SOLID_ANGLE_UNIT ( ) );
#114901 = STYLED_ITEM ( 'NONE', ( #136384 ), #75064 ) ;
#114902 = CARTESIAN_POINT ( 'NONE',  ( 4.759808938472720463, 8.174556087920027636, -0.7576060450402433144 ) ) ;
#114903 = CARTESIAN_POINT ( 'NONE',  ( -5.097502569058225852, 5.049433873430440478, -0.7216878364870207285 ) ) ;
#114904 = CARTESIAN_POINT ( 'NONE',  ( 7.754900677336718395, 11.99120852362745460, -0.7216878364870267237 ) ) ;
#114905 = CARTESIAN_POINT ( 'NONE',  ( 5.155114233317533490, 1.639596689546858777, -1.090739528099492928 ) ) ;
#114906 = CARTESIAN_POINT ( 'NONE',  ( 1.840644454891388282, 1.218392294859267144, -1.735325642819861791 ) ) ;
#114907 = CARTESIAN_POINT ( 'NONE',  ( -5.742041750587549842, 6.657802449562273850, 1.199719254218450271 ) ) ;
#114908 = CARTESIAN_POINT ( 'NONE',  ( -11.95482906247546850, 9.001069635099803179, -0.6096848022493118746 ) ) ;
#114909 = CARTESIAN_POINT ( 'NONE',  ( 3.475000000000000533, -2.654166666666667229, 2.006292185433948827 ) ) ;
#114910 = CARTESIAN_POINT ( 'NONE',  ( 6.175747540105122724, -1.175446681380667213, 1.849350104233343783 ) ) ;
#114911 = CARTESIAN_POINT ( 'NONE',  ( 3.231779075379137556, 6.036511184309971689, -2.420000000000002149 ) ) ;
#114912 = CARTESIAN_POINT ( 'NONE',  ( 4.137660063496669594, -1.327783069688622586, -1.395926297547624984 ) ) ;
#114913 = CARTESIAN_POINT ( 'NONE',  ( -8.030507057996002729, 8.263346410617135263, 1.040834085586084257E-14 ) ) ;
#114914 = CARTESIAN_POINT ( 'NONE',  ( 0.7096328715897933792, -1.817275359149352676, 0.1739118742359047065 ) ) ;
#114915 = CARTESIAN_POINT ( 'NONE',  ( 0.6103625832605160673, -2.195865045534075133, 0.2202409711149767024 ) ) ;
#114916 = CARTESIAN_POINT ( 'NONE',  ( 1.250000000000037526, 8.500000000000000000, -11.02939254900286592 ) ) ;
#114917 = VERTEX_POINT ( 'NONE', #99998 ) ;
#114918 = FACE_OUTER_BOUND ( 'NONE', #27738, .T. ) ;
#114919 = ORIENTED_EDGE ( 'NONE', *, *, #197493, .F. ) ;
#114920 = CARTESIAN_POINT ( 'NONE',  ( 6.702011354250313246, 0.7569246535186587854, -1.818382958529676019 ) ) ;
#114921 = CARTESIAN_POINT ( 'NONE',  ( 1.030689935155226555, -1.755017395645932066, 0.8318847510124205424 ) ) ;
#114922 = CARTESIAN_POINT ( 'NONE',  ( 6.397888825007291835, 0.2158721846312293136, 2.288236095241158452 ) ) ;
#114924 = CARTESIAN_POINT ( 'NONE',  ( 5.489040303513849750, 0.1347565666095333348, 1.856089258439092893 ) ) ;
#114923 = CARTESIAN_POINT ( 'NONE',  ( -7.119966945832006289, 8.335658187339330283, 1.199719254218452047 ) ) ;
#114925 = CARTESIAN_POINT ( 'NONE',  ( 6.333594036239346359, 7.418223126147930557, 1.199719254218453823 ) ) ;
#114926 = SURFACE_SIDE_STYLE ('',( #67145 ) ) ;
#114927 = CARTESIAN_POINT ( 'NONE',  ( 6.509000000000011887, 3.696273625755361447, 2.514342382328867753 ) ) ;
#114928 = CARTESIAN_POINT ( 'NONE',  ( -4.367698041896780126, 8.247398148854895084, 0.7998128361456481317 ) ) ;
#114929 = CARTESIAN_POINT ( 'NONE',  ( 6.720655732516701342, 6.039000170257122768, 2.421169367564251385 ) ) ;
#114930 = CARTESIAN_POINT ( 'NONE',  ( 0.9080814035550346386, -0.9900877184637231210, -1.955254813705724404 ) ) ;
#114931 = CARTESIAN_POINT ( 'NONE',  ( 4.744990575102895569, 5.598539094783909320, -1.082531754730548412 ) ) ;
#114932 = CARTESIAN_POINT ( 'NONE',  ( -0.1855116875246293484, 13.36893861697142860, -1.371511898276919217 ) ) ;
#114933 = CARTESIAN_POINT ( 'NONE',  ( 2.300394833791450377, 2.756885564284757617, -2.500000000000000444 ) ) ;
#114934 = CARTESIAN_POINT ( 'NONE',  ( 1.383131112650197281, 1.687622997524572677, -0.6969523973551354779 ) ) ;
#114935 = CARTESIAN_POINT ( 'NONE',  ( -3.379006598303881059, 4.965260336153046516, -1.599625672291256295 ) ) ;
#114936 = CARTESIAN_POINT ( 'NONE',  ( -0.1010051578917390280, 3.387064998577566488, -1.997555336163420181 ) ) ;
#114937 = FACE_OUTER_BOUND ( 'NONE', #21798, .T. ) ;
#114938 = CARTESIAN_POINT ( 'NONE',  ( 10.70146331988817323, 11.37946204949139251, 0.7998128361456341429 ) ) ;
#114939 = CARTESIAN_POINT ( 'NONE',  ( 6.727182134110220701, 0.005875948494733078051, 1.810970247402940103 ) ) ;
#114940 = CARTESIAN_POINT ( 'NONE',  ( 4.961744919065852244, -0.5270168765720646409, 1.889542207339139024 ) ) ;
#114941 = CARTESIAN_POINT ( 'NONE',  ( -9.203287345578106127, 9.631590079462940324, 0.7998128361456462443 ) ) ;
#114942 = CARTESIAN_POINT ( 'NONE',  ( 7.149227073107712549, 7.235186428247455837, -0.7998128361456281477 ) ) ;
#114943 = CARTESIAN_POINT ( 'NONE',  ( 4.670628115925999246, 0.8122961462209904449, 1.958930372594757330 ) ) ;
#114944 = CARTESIAN_POINT ( 'NONE',  ( 4.177398808104064720, 1.432170664236757540, 1.658919600136643524 ) ) ;
#114945 = CARTESIAN_POINT ( 'NONE',  ( 3.635557746758808495, 7.393234471193928847, -0.7998128361456291469 ) ) ;
#114946 = CARTESIAN_POINT ( 'NONE',  ( 3.221598570378156001, 0.3083542414583049784, -2.047064864394084971 ) ) ;
#114948 = CARTESIAN_POINT ( 'NONE',  ( 1.364683531249988757, -0.5531249996585801965, 0.000000000000000000 ) ) ;
#114947 = DIRECTION ( 'NONE',  ( 0.000000000000000000, 1.000000000000000000, 0.000000000000000000 ) ) ;
#114949 = ORIENTED_EDGE ( 'NONE', *, *, #131308, .T. ) ;
#114950 = CARTESIAN_POINT ( 'NONE',  ( 2.602471654445730032, -0.2222675636014606049, 2.287907847288372043 ) ) ;
#114951 = CARTESIAN_POINT ( 'NONE',  ( 8.107412671292035355, 10.48173408797264194, 1.443375672974076540 ) ) ;
#114953 = CARTESIAN_POINT ( 'NONE',  ( 3.285556943750000070, -1.334374999522040861, 0.000000000000000000 ) ) ;
#114952 = CARTESIAN_POINT ( 'NONE',  ( 5.072158865288233898, 7.971250205261355859, 1.082531754730549078 ) ) ;
#114954 = CARTESIAN_POINT ( 'NONE',  ( 6.720655732516660485, 7.629137130509104914, 2.326260288887294969 ) ) ;
#114955 = CARTESIAN_POINT ( 'NONE',  ( -9.705102360090382518, 4.469090025550438661, -7.059677490138621891 ) ) ;
#114956 = CARTESIAN_POINT ( 'NONE',  ( 3.820204237656314561, 1.844379349147889480, 0.6080220579995837538 ) ) ;
#114957 = ORIENTED_EDGE ( 'NONE', *, *, #130852, .F. ) ;
#114958 = CARTESIAN_POINT ( 'NONE',  ( -6.735605996566196296E-15, -9.746166700180788567, 9.579665964948873125 ) ) ;
#114959 = ADVANCED_FACE ( 'NONE', ( #154088 ), #200343, .F. ) ;
#114960 = CARTESIAN_POINT ( 'NONE',  ( 3.533378866418676711, -0.1359047358975660202, 1.907598245988059826 ) ) ;
#114961 = CYLINDRICAL_SURFACE ( 'NONE', #68834, 2.250000000000000444 ) ;
#114962 = CARTESIAN_POINT ( 'NONE',  ( 5.614166379062860202, -0.7790257685919326214, -1.538869111107727505 ) ) ;
#114963 = CARTESIAN_POINT ( 'NONE',  ( 3.239470508323912146, 0.4852670486454255250, -1.957170429962351577 ) ) ;
#114964 = CARTESIAN_POINT ( 'NONE',  ( 5.520273603857641653, -2.079230528169520031, 0.9805040003046764374 ) ) ;
#114965 = CARTESIAN_POINT ( 'NONE',  ( 1.500000000000001332, 11.12499999999999645, 0.000000000000000000 ) ) ;
#114966 = CARTESIAN_POINT ( 'NONE',  ( 0.8212658843103730621, 2.040464674744349338, 0.8412164853940640175 ) ) ;
#114967 = CARTESIAN_POINT ( 'NONE',  ( -5.153507786970276783, 6.145418851954329575, -1.082531754730549967 ) ) ;
#114968 = CARTESIAN_POINT ( 'NONE',  ( 5.764868906847371299, -1.600580677892119441, -0.7553990054774415430 ) ) ;
#114970 = CARTESIAN_POINT ( 'NONE',  ( 1.711265200625663008, -0.2773638578843647950, 2.275360193931966535 ) ) ;
#114969 = CARTESIAN_POINT ( 'NONE',  ( 5.200434439293556643, 8.224868058221247225, -1.199719254218452047 ) ) ;
#114971 = CARTESIAN_POINT ( 'NONE',  ( 1.165484214331854895, -1.106714608479087092, 1.343107696387570549 ) ) ;
#114972 = CARTESIAN_POINT ( 'NONE',  ( 0.4153311931458965045, 3.850000000000006306, -0.4999999999999987232 ) ) ;
#114973 = FACE_OUTER_BOUND ( 'NONE', #195969, .T. ) ;
#114974 = CARTESIAN_POINT ( 'NONE',  ( -2.993318053567081360, 6.714231172462041819, 0.000000000000000000 ) ) ;
#114975 = CARTESIAN_POINT ( 'NONE',  ( -1.360316468750018659, 0.6927083336747492659, 0.7853790794158961308 ) ) ;
#114976 = CARTESIAN_POINT ( 'NONE',  ( -11.86685672517501899, 13.60918917859810584, -1.056525322636018727 ) ) ;
#114977 = ADVANCED_FACE ( 'NONE', ( #41426 ), #108600, .F. ) ;
#114978 = CARTESIAN_POINT ( 'NONE',  ( 1.258521197368984268, -2.171350058325251187, -0.0004004535333074903960 ) ) ;
#114979 = CARTESIAN_POINT ( 'NONE',  ( 2.009000277268524481, 0.004839059525654776373, 2.016708403978189956 ) ) ;
#114980 = VECTOR ( 'NONE', #148251, 1000.000000000000000 ) ;
#114981 = CARTESIAN_POINT ( 'NONE',  ( 0.7499999999999885647, 0.7645833340161543035, 1.299038105676657340 ) ) ;
#114982 = CARTESIAN_POINT ( 'NONE',  ( 5.830678075864223153, 1.857343136638961445, 0.5113247108688694365 ) ) ;
#114983 = CARTESIAN_POINT ( 'NONE',  ( 0.6823417656249934904, 12.44270833367473017, 1.181850606188764807 ) ) ;
#114984 = CARTESIAN_POINT ( 'NONE',  ( 2.461440635673370014, -1.844245817859784031, 1.238046099332066108 ) ) ;
#114985 = ORIENTED_EDGE ( 'NONE', *, *, #170070, .F. ) ;
#114987 = AXIS2_PLACEMENT_3D ( 'NONE', #169143, #90051, #73776 ) ;
#114986 = CARTESIAN_POINT ( 'NONE',  ( -2.796816994357229635, 2.968434822912338067, 2.452793345967703598 ) ) ;
#114988 = CARTESIAN_POINT ( 'NONE',  ( -6.102578539482539810, 6.292298848917299736, 0.000000000000000000 ) ) ;
#114989 = CARTESIAN_POINT ( 'NONE',  ( 8.809047120577066181, 11.30030761213851953, 1.599625672291281386 ) ) ;
#114990 = DIRECTION ( 'NONE',  ( -0.000000000000000000, -1.000000000000000000, 0.000000000000000000 ) ) ;
#114991 = FACE_OUTER_BOUND ( 'NONE', #66895, .T. ) ;
#114992 = CARTESIAN_POINT ( 'NONE',  ( 5.847135585344571673, 0.4968686550196474982, -1.668027988745724777 ) ) ;
#114993 = CARTESIAN_POINT ( 'NONE',  ( 3.244534624505683418, -1.932379277470747558, -0.3379807920969243873 ) ) ;
#114995 = CARTESIAN_POINT ( 'NONE',  ( -7.375272376154096143, 8.667201196010339004, -1.082531754730544860 ) ) ;
#114994 = CARTESIAN_POINT ( 'NONE',  ( 4.497554271431305040, 6.270232621468402989, -1.599625672291256295 ) ) ;
#114996 = CARTESIAN_POINT ( 'NONE',  ( -5.803933766307007858, 6.065161521460068705, 0.5445525043519475750 ) ) ;
#114997 = CARTESIAN_POINT ( 'NONE',  ( 4.956464464747484477, 0.8595337117903809609, 2.092967149517725112 ) ) ;
#114998 = CARTESIAN_POINT ( 'NONE',  ( 0.8013246507756426329, -1.769997244335961284, 1.058882903378530749 ) ) ;
#114999 = CARTESIAN_POINT ( 'NONE',  ( -6.021792782764022078, 10.17717534653336209, -0.7998128361456291469 ) ) ;
#115000 =( BOUNDED_CURVE ( )  B_SPLINE_CURVE ( 3, ( #71184, #100507, #134115, #200124 ),
 .UNSPECIFIED., .F., .T. ) 
 B_SPLINE_CURVE_WITH_KNOTS ( ( 4, 4 ),
 ( 4.082329036714103410, 4.712388980384689674 ),
 .UNSPECIFIED. ) 
 CURVE ( )  GEOMETRIC_REPRESENTATION_ITEM ( )  RATIONAL_B_SPLINE_CURVE ( ( 1.000000000000000000, 0.9671913951458349645, 0.9671913951458349645, 1.000000000000000000 ) ) 
 REPRESENTATION_ITEM ( '' )  );
#115001 = CARTESIAN_POINT ( 'NONE',  ( -3.673896439178936824, 5.309298483840612093, 1.443375672974064550 ) ) ;
#115002 = CARTESIAN_POINT ( 'NONE',  ( 2.184789616947193203, -2.218938341775698042, -0.4411300470171536370 ) ) ;
#115003 = ORIENTED_EDGE ( 'NONE', *, *, #23766, .F. ) ;
#115004 = CARTESIAN_POINT ( 'NONE',  ( -1.500000000000013101, 1.952083334016152527, 0.8660254037844403729 ) ) ;
#115005 = CARTESIAN_POINT ( 'NONE',  ( 2.547943918863291302, 1.870051909910470878, 0.05015897750767356333 ) ) ;
#115006 = CARTESIAN_POINT ( 'NONE',  ( 1.740413025836908156, 1.729532991921935325, -0.1275185469355680501 ) ) ;
#115007 = ADVANCED_FACE ( 'NONE', ( #173565 ), #57655, .F. ) ;
#115008 = CARTESIAN_POINT ( 'NONE',  ( 4.810206850810132551, 1.511280187219691928, -1.587364365194674498 ) ) ;
#115009 = CARTESIAN_POINT ( 'NONE',  ( 6.352564483950959406, 0.7153834962906236994, 2.193980215933882150 ) ) ;
#115010 = CARTESIAN_POINT ( 'NONE',  ( 1.516555680085801994, 1.384881227076775190, -1.526387457142893256 ) ) ;
#115011 = CARTESIAN_POINT ( 'NONE',  ( 4.365135538708351248, 1.883338149218495516, -0.4730343525067778332 ) ) ;
#115012 = CARTESIAN_POINT ( 'NONE',  ( -8.469039510030723861, 13.03229652834454733, 1.040834085586084257E-14 ) ) ;
#115013 = DIRECTION ( 'NONE',  ( -0.7771862570881746812, 0.6292706268317899143, 0.000000000000000000 ) ) ;
#115014 = CARTESIAN_POINT ( 'NONE',  ( 1.187500000000001110, -1.451031289061072815, 1.451031289061169183 ) ) ;
#115015 = EDGE_CURVE ( 'NONE', #209652, #164105, #82699, .T. ) ;
#115016 = CARTESIAN_POINT ( 'NONE',  ( 3.995055777641403516, 7.602996552368006533, -0.05680687033517151097 ) ) ;
#115017 = CARTESIAN_POINT ( 'NONE',  ( 6.239611212763971793, -1.913511330438378177, -0.6350998681113121380 ) ) ;
#115018 = CARTESIAN_POINT ( 'NONE',  ( 0.000000000000000000, 0.000000000000000000, 0.000000000000000000 ) ) ;
#115019 = CARTESIAN_POINT ( 'NONE',  ( -1.360316468750021768, 0.6406250003414132310, -3.469446951953614189E-14 ) ) ;
#115020 = CARTESIAN_POINT ( 'NONE',  ( 6.012342310302175363, -1.897698807000438359, 0.6819931642896917001 ) ) ;
#115021 = CARTESIAN_POINT ( 'NONE',  ( -9.022061154889962964, 12.61315621642528129, -1.199719254218446718 ) ) ;
#115022 = CARTESIAN_POINT ( 'NONE',  ( 8.121497709785879593, 9.433834401960398353, -1.199719254218445830 ) ) ;
#115023 = CARTESIAN_POINT ( 'NONE',  ( 3.553118775233146120, 6.302999783484076524, -1.199719254218453823 ) ) ;
#115025 = DIRECTION ( 'NONE',  ( 0.000000000000000000, 0.000000000000000000, 1.000000000000000000 ) ) ;
#115024 = CARTESIAN_POINT ( 'NONE',  ( 2.367563199519676420, 1.790531440309536926, -0.3556685536310541518 ) ) ;
#115026 = CARTESIAN_POINT ( 'NONE',  ( 10.97030574691034843, 11.30000000000000249, -1.695191245859933193 ) ) ;
#115027 = CARTESIAN_POINT ( 'NONE',  ( -1.225000000000032063, 1.833333334016213012, 0.7072540797572777205 ) ) ;
#115028 = ORIENTED_EDGE ( 'NONE', *, *, #144354, .T. ) ;
#115029 = CARTESIAN_POINT ( 'NONE',  ( -6.116136693096208887, 6.308116694799912771, 0.7216878364870257245 ) ) ;
#115030 = FACE_BOUND ( 'NONE', #84987, .T. ) ;
#115031 = CARTESIAN_POINT ( 'NONE',  ( -9.158696461231359720, 10.64389961198009615, 1.199719254218462483 ) ) ;
#115032 = CARTESIAN_POINT ( 'NONE',  ( 0.05299788485858129838, 0.3494575625802974206, 1.989167885679890002 ) ) ;
#115033 = CARTESIAN_POINT ( 'NONE',  ( 0.2762449081346768365, 2.096790360132039233, -0.3154013857558089495 ) ) ;
#115034 = VERTEX_POINT ( 'NONE', #189775 ) ;
#115035 = CARTESIAN_POINT ( 'NONE',  ( -6.774234028683526532, 7.932303117332766718, 1.199719254218452047 ) ) ;
#115036 = CIRCLE ( 'NONE', #49272, 0.04999999999999883010 ) ;
#115037 = CARTESIAN_POINT ( 'NONE',  ( 4.864678189204997949, 4.569879397027603929, 0.7998128361456341429 ) ) ;
#115038 = CARTESIAN_POINT ( 'NONE',  ( 6.174695665487812235, -1.956078286930991394, -0.6490473743868007128 ) ) ;
#115039 = CARTESIAN_POINT ( 'NONE',  ( 5.326796142270829648, 0.8146286751641409474, -1.844708973168760924 ) ) ;
#115040 = ORIENTED_EDGE ( 'NONE', *, *, #100912, .F. ) ;
#115041 = ORIENTED_EDGE ( 'NONE', *, *, #203953, .F. ) ;
#115042 = ORIENTED_EDGE ( 'NONE', *, *, #31289, .F. ) ;
#115043 = CARTESIAN_POINT ( 'NONE',  ( 9.946057155611644163, 2.515145635913765609, 6.189092007093160319 ) ) ;
#115044 = CARTESIAN_POINT ( 'NONE',  ( 4.067155351693835485E-15, 0.2500000006828133059, -1.225000000000014300 ) ) ;
#115046 = EDGE_LOOP ( 'NONE', ( #51163, #56902, #52783, #79562, #157094 ) ) ;
#115045 = CARTESIAN_POINT ( 'NONE',  ( -6.038177310039794854, 8.137902509836795417, -1.599625672291271394 ) ) ;
#115047 = CARTESIAN_POINT ( 'NONE',  ( 5.853046489161108035, 7.294594176516559614, 1.271900669079442325 ) ) ;
#115048 = CARTESIAN_POINT ( 'NONE',  ( 4.692732413458527319, -1.238132498367884082, -1.591073831703953445 ) ) ;
#115049 = CARTESIAN_POINT ( 'NONE',  ( 5.173706384855800700, -1.019854773079221344, 1.532662130498331887 ) ) ;
#115050 = CARTESIAN_POINT ( 'NONE',  ( -0.02319159430949970999, 0.003959926571647092407, -1.810968101872318714 ) ) ;
#115051 = CARTESIAN_POINT ( 'NONE',  ( 2.754834555525199846, 0.7783630933865728352, 2.172589714749242784 ) ) ;
#115052 = CARTESIAN_POINT ( 'NONE',  ( 7.517069824134078537, 7.734612647770044092, 0.000000000000000000 ) ) ;
#115053 = CARTESIAN_POINT ( 'NONE',  ( 6.415313282229532454, -0.2716245656670859820, 2.144420208805633887 ) ) ;
#115055 = CARTESIAN_POINT ( 'NONE',  ( 6.448874621594486989, 10.67543749183559143, 0.7998128361456462443 ) ) ;
#115054 = CARTESIAN_POINT ( 'NONE',  ( 3.450407915430803385, -1.350735839785843773, 1.497501794165828626 ) ) ;
#115056 = CARTESIAN_POINT ( 'NONE',  ( 0.9252163604592329449, -1.233020167302405490, -1.500395619358737553 ) ) ;
#115057 = CARTESIAN_POINT ( 'NONE',  ( -4.192495815123836955, 5.914331089109674089, -1.599625672291256295 ) ) ;
#115058 = VERTEX_POINT ( 'NONE', #91239 ) ;
#115059 = CARTESIAN_POINT ( 'NONE',  ( 11.86687934130374522, 9.990480503834419324, 1.056332641424306606 ) ) ;
#115060 = CARTESIAN_POINT ( 'NONE',  ( -4.950662367645459305, 5.804802846121667415, -1.199719254218453823 ) ) ;
#115061 = AXIS2_PLACEMENT_3D ( 'NONE', #202345, #150448, #19345 ) ;
#115062 = CARTESIAN_POINT ( 'NONE',  ( 3.977312496258199825, 1.761605600429091201, -0.6297503393934977822 ) ) ;
#115063 = CIRCLE ( 'NONE', #108107, 2.000000000000000000 ) ;
#115066 = CARTESIAN_POINT ( 'NONE',  ( -5.424143973919053785, 8.485862515284315677, 1.199719254218454489 ) ) ;
#115065 = CARTESIAN_POINT ( 'NONE',  ( -1.500000000000001332, 0.6812500006828161592, 0.000000000000000000 ) ) ;
#115064 = CARTESIAN_POINT ( 'NONE',  ( 1.793074957647671663, -0.09724762972821224261, -1.910064080951429100 ) ) ;
#115067 = CARTESIAN_POINT ( 'NONE',  ( 3.035963658818414235, -1.482449291622448095, -1.634993338104336891 ) ) ;
#115068 = CARTESIAN_POINT ( 'NONE',  ( 6.883263157960399781, 2.970623603138924818, 2.399364662246627589 ) ) ;
#115069 = CARTESIAN_POINT ( 'NONE',  ( 3.891353782322113375, 4.498666486585943147, -1.199719254218446718 ) ) ;
#115070 = CARTESIAN_POINT ( 'NONE',  ( 6.251718229232841928, 8.387033582228703210, -1.443375672974078761 ) ) ;
#115071 = CARTESIAN_POINT ( 'NONE',  ( -4.946027110887008860, 4.664786472323266153, -0.7998128361456221525 ) ) ;
#115072 = CARTESIAN_POINT ( 'NONE',  ( -5.424670858799220063, 9.342883411992149334, 0.000000000000000000 ) ) ;
#115073 = CARTESIAN_POINT ( 'NONE',  ( 0.8605430240068573378, -1.430899983082928761, 1.356264857227080567 ) ) ;
#115074 = CARTESIAN_POINT ( 'NONE',  ( 1.466329616580586581, 2.273096917617071888, -0.3966160293069305731 ) ) ;
#115075 = CARTESIAN_POINT ( 'NONE',  ( 1.504273306027693602, 1.959471947749168663, 0.09963418240711149898 ) ) ;
#115076 = CARTESIAN_POINT ( 'NONE',  ( 5.559457797297955750, 1.683061182826322666, 1.192002683324727252 ) ) ;
#115077 = CARTESIAN_POINT ( 'NONE',  ( 4.853455804012216213, 6.685451076146141425, 1.443375672974062551 ) ) ;
#115078 = CARTESIAN_POINT ( 'NONE',  ( 6.215487077222150880, 6.216099443039444949, 0.000000000000000000 ) ) ;
#115079 = VERTEX_POINT ( 'NONE', #8889 ) ;
#115080 = CARTESIAN_POINT ( 'NONE',  ( 0.6823417656249899377, 5.238541667008086655, -1.181850606188754593 ) ) ;
#115081 = CARTESIAN_POINT ( 'NONE',  ( -5.956409969451652131, 6.075908546082715134, -0.6293437877468227581 ) ) ;
#115082 = CARTESIAN_POINT ( 'NONE',  ( 4.975479186090860928, 4.907073259968533385, 0.7216878364870317197 ) ) ;
#115083 = CARTESIAN_POINT ( 'NONE',  ( 0.8487579731258857452, -2.154475699732544491, -0.2676485622446558299 ) ) ;
#115085 = CARTESIAN_POINT ( 'NONE',  ( 6.022987620897008121, -1.731432113864934674, 0.6267441317700100933 ) ) ;
#115084 = CARTESIAN_POINT ( 'NONE',  ( 9.499606441938663437, -9.580980486002390606, -0.08647223992350253075 ) ) ;
#115086 = CARTESIAN_POINT ( 'NONE',  ( 6.506745451169511085, -8.202869699938540649, 6.922231005658569636 ) ) ;
#115087 = CARTESIAN_POINT ( 'NONE',  ( -6.493979435825336211, -7.868711954889216820, 6.493979435825359303 ) ) ;
#115088 = CARTESIAN_POINT ( 'NONE',  ( 1.493192106177696044, 1.412881632968411516, 1.225925835885120829 ) ) ;
#115089 = CARTESIAN_POINT ( 'NONE',  ( 5.835289683280778128, -1.956920075724715602, 0.9183947573421016308 ) ) ;
#115090 = CARTESIAN_POINT ( 'NONE',  ( -6.136354103119505687, 5.996982182489118962, -0.08184359936842452998 ) ) ;
#115091 = CARTESIAN_POINT ( 'NONE',  ( 0.07755575628181145265, 6.946778278137147211, -2.783982195446454533 ) ) ;
#115092 = CARTESIAN_POINT ( 'NONE',  ( -1.364683531250014514, -0.7197916663252461600, 0.7879004041258379498 ) ) ;
#115093 = CARTESIAN_POINT ( 'NONE',  ( 1.418461073652961257, -0.6892283116659430053, -1.783923526276688154 ) ) ;
#115094 =( BOUNDED_SURFACE ( )  B_SPLINE_SURFACE ( 3, 2, ( 
 ( #132914, #18041, #164319 ),
 ( #36439, #181616, #84128 ),
 ( #102514, #100379, #214085 ),
 ( #150214, #151277, #86264 ),
 ( #33245, #168576, #135038 ),
 ( #51645, #99327, #2849 ),
 ( #201051, #20177, #117769 ),
 ( #16971, #68918, #149127 ) ),
 .UNSPECIFIED., .F., .F., .T. ) 
 B_SPLINE_SURFACE_WITH_KNOTS ( ( 4, 2, 2, 4 ),
 ( 3, 3 ),
 ( 1.016439536705160407E-16, 0.0002568729646054561692, 0.0005137459292108107487, 0.001027491858421519799 ),
 ( 0.000000000000000000, 1.000000000000000000 ),
 .UNSPECIFIED. ) 
 GEOMETRIC_REPRESENTATION_ITEM ( )  RATIONAL_B_SPLINE_SURFACE ( (
 ( 1.000000000000000000, 0.3826834323651128189, 1.000000000000000000),
 ( 1.000000000000000000, 0.3847114443836955888, 1.000000000000000000),
 ( 1.000000000000000000, 0.4039255759072543084, 1.000000000000000000),
 ( 1.000000000000000000, 0.4557194474498772463, 1.000000000000000000),
 ( 1.000000000000000000, 0.4874388927526764892, 1.000000000000000000),
 ( 1.000000000000000000, 0.5833547384511119649, 1.000000000000000000),
 ( 1.000000000000000000, 0.6470545345841089979, 1.000000000000000000),
 ( 1.000000000000000000, 0.7045118851637771629, 1.000000000000000000) ) ) 
 REPRESENTATION_ITEM ( '' )  SURFACE ( )  );
#115096 = EDGE_CURVE ( 'NONE', #151327, #36526, #172479, .T. ) ;
#115095 = CARTESIAN_POINT ( 'NONE',  ( 3.256490041505883504, -1.340903482672378466, 1.155240514129013407 ) ) ;
#115097 = CARTESIAN_POINT ( 'NONE',  ( 0.8207898099904624711, 1.447681275506585541, -1.249484660484905030 ) ) ;
#115099 = CARTESIAN_POINT ( 'NONE',  ( 5.220295459014530515, 1.888029131402849670, 0.3228437444452412763 ) ) ;
#115098 = CARTESIAN_POINT ( 'NONE',  ( 3.271045316616016940, -3.187365041801710763, -0.6525704249654357136 ) ) ;
#115100 = CARTESIAN_POINT ( 'NONE',  ( 6.144967554776202157, -0.2872888210109864060, -1.948340736549762697 ) ) ;
#115101 = CARTESIAN_POINT ( 'NONE',  ( -0.7500000000000215383, 4.941666666666684193, 1.299038105676671107 ) ) ;
#115102 = CARTESIAN_POINT ( 'NONE',  ( 1.213308285724056690, 1.730450836393576886, -1.225479750871574458 ) ) ;
#115103 = CARTESIAN_POINT ( 'NONE',  ( -1.579999999999998073, 8.674529973577531194, -2.419999999999989715 ) ) ;
#115104 = CARTESIAN_POINT ( 'NONE',  ( 4.188257260935820625, -1.850246793840780279, -0.2747695030091561463 ) ) ;
#115106 = ORIENTED_EDGE ( 'NONE', *, *, #207247, .F. ) ;
#115105 = CARTESIAN_POINT ( 'NONE',  ( 0.1350027811974127134, -1.670744041527939094, 0.7364786222084362954 ) ) ;
#115108 = CARTESIAN_POINT ( 'NONE',  ( 1.499999999999978906, 4.295833333333352044, -0.8660254037844369313 ) ) ;
#115107 = CARTESIAN_POINT ( 'NONE',  ( 4.459734715955371520, 0.4851516707722826061, -2.152740496749529608 ) ) ;
#115109 = CARTESIAN_POINT ( 'NONE',  ( -0.6823417656250212460, 4.613541667008086655, 1.181850606188767472 ) ) ;
#115110 = CARTESIAN_POINT ( 'NONE',  ( 1.908709741418318062, 0.6448079515158434694, 1.959386160279535494 ) ) ;
#115111 = CARTESIAN_POINT ( 'NONE',  ( 6.474182045725470402, 7.511966127223233869, -1.199719254218446718 ) ) ;
#115112 = CARTESIAN_POINT ( 'NONE',  ( -8.850775351622791831, 9.220326086515070685, -0.7998128361456291469 ) ) ;
#115113 = FACE_BOUND ( 'NONE', #92889, .T. ) ;
#115114 = CARTESIAN_POINT ( 'NONE',  ( 8.055515824813896941, 12.54985222892493368, 0.7998128361456462443 ) ) ;
#115115 = CARTESIAN_POINT ( 'NONE',  ( -3.423866110619523173, -0.02112260055291484417, -0.4190911324384871683 ) ) ;
#115116 = CARTESIAN_POINT ( 'NONE',  ( 0.1753634416057741618, 2.865130778691078461, -2.632309609290181651 ) ) ;
#115117 = ORIENTED_EDGE ( 'NONE', *, *, #53950, .F. ) ;
#115118 = CARTESIAN_POINT ( 'NONE',  ( 4.105968538015460467, 0.7004154448949986289, -1.948405661837959713 ) ) ;
#115119 = CARTESIAN_POINT ( 'NONE',  ( -1.402160292154681736E-14, -0.7406249996585823059, -1.575800808251665908 ) ) ;
#115120 = CARTESIAN_POINT ( 'NONE',  ( 1.019082891775088484, 1.996809913787592095, 0.8282600050937349856 ) ) ;
#115121 = CARTESIAN_POINT ( 'NONE',  ( -6.114219544286552122, 7.015314154546907766, -0.9703045268592332961 ) ) ;
#115122 = CARTESIAN_POINT ( 'NONE',  ( 2.209634141364385851, 1.562563088667227262, 1.279657157811086909 ) ) ;
#115123 = DIRECTION ( 'NONE',  ( -0.7384114592157855483, 0.000000000000000000, 0.6743504407196708739 ) ) ;
#115124 = VERTEX_POINT ( 'NONE', #127008 ) ;
#115126 = CARTESIAN_POINT ( 'NONE',  ( 7.782016984564054773, 10.10210578678999482, 1.443375672974076540 ) ) ;
#115125 = CARTESIAN_POINT ( 'NONE',  ( -3.475000000000000533, -3.529166666666667229, -2.006292185433948827 ) ) ;
#115127 = ADVANCED_FACE ( 'NONE', ( #194036 ), #46755, .T. ) ;
#115128 = CARTESIAN_POINT ( 'NONE',  ( 0.1368885365587524383, -5.294776013890285959, 10.99935770452674610 ) ) ;
#115129 = CARTESIAN_POINT ( 'NONE',  ( 0.1457207355009884908, 1.993892511249679034, -0.3006540981884687214 ) ) ;
#115130 = CARTESIAN_POINT ( 'NONE',  ( 4.441096743985088580, -1.694418930461354611, -1.389946530008886905 ) ) ;
#115131 = CARTESIAN_POINT ( 'NONE',  ( 1.499999999999990896, 3.306250000682818602, 1.214306433183764966E-14 ) ) ;
#115132 = CARTESIAN_POINT ( 'NONE',  ( 3.427896188528327226, -1.883279545317056547, 0.3315703044584616399 ) ) ;
#115133 = CARTESIAN_POINT ( 'NONE',  ( -3.928111819657352566, 5.605883094398769195, 1.599625672291267398 ) ) ;
#115134 = CARTESIAN_POINT ( 'NONE',  ( 6.778713616708431644, 7.010846762355714468, 1.040834085586084257E-14 ) ) ;
#115136 = CARTESIAN_POINT ( 'NONE',  ( 2.495720449669075247, -1.994069261235394741, 0.2986488809556055446 ) ) ;
#115135 = CARTESIAN_POINT ( 'NONE',  ( -9.531018800282611281, 12.14260790512831889, 1.443375672974076540 ) ) ;
#115137 = CARTESIAN_POINT ( 'NONE',  ( 0.6823417656249969321, 12.33854166700806765, -1.181850606188757036 ) ) ;
#115139 = CARTESIAN_POINT ( 'NONE',  ( -8.072954122294394352, 8.383144328957069291, -0.7998128361456362523 ) ) ;
#115138 = CARTESIAN_POINT ( 'NONE',  ( 0.3281778771060560040, 1.171583119817346086, -1.970250653751925762 ) ) ;
#115140 = CARTESIAN_POINT ( 'NONE',  ( 3.891373129206575410, 1.249378432800802852, 1.189308452707043884 ) ) ;
#115141 = CARTESIAN_POINT ( 'NONE',  ( 0.1405533004714617507, 0.6596865332844923380, -2.358301179948574244 ) ) ;
#115142 = CARTESIAN_POINT ( 'NONE',  ( 4.304877467538922531, 4.981110786005563007, 1.199719254218464037 ) ) ;
#115143 = DIRECTION ( 'NONE',  ( -1.000000000000000000, -3.451266460341926211E-31, -8.638326563840810896E-31 ) ) ;
#115144 = CARTESIAN_POINT ( 'NONE',  ( 5.040934186182656873, 4.775511393501539636, 1.040834085586084257E-14 ) ) ;
#115145 = CARTESIAN_POINT ( 'NONE',  ( 0.07536363704233400851, 2.864322694550157866, -2.632457840217194089 ) ) ;
#115146 = EDGE_LOOP ( 'NONE', ( #210701, #81941, #36048, #101725, #168668, #38657, #75121, #189308 ) ) ;
#115148 = VECTOR ( 'NONE', #36829, 1000.000000000000000 ) ;
#115147 = DIRECTION ( 'NONE',  ( -1.000000000000000000, 0.000000000000000000, 0.000000000000000000 ) ) ;
#115149 = EDGE_LOOP ( 'NONE', ( #76207, #145274, #186363, #169441 ) ) ;
#115150 = CARTESIAN_POINT ( 'NONE',  ( 5.461500695664097904, -1.431772717462083566, -1.109608708211702099 ) ) ;
#115151 = EDGE_LOOP ( 'NONE', ( #177846, #208584, #71769, #201906 ) ) ;
#115153 = CARTESIAN_POINT ( 'NONE',  ( 6.229045230835819069, 6.231917288922055320, -0.7998128361456481317 ) ) ;
#115152 = CIRCLE ( 'NONE', #21647, 12.00000000000000178 ) ;
#115154 = CARTESIAN_POINT ( 'NONE',  ( 7.019253602638862333, -7.126685749119995528, -7.019253602638886314 ) ) ;
#115155 = CARTESIAN_POINT ( 'NONE',  ( 5.690068458729246714, 1.084374654971603569, 1.450890516563392518 ) ) ;
#115156 = CARTESIAN_POINT ( 'NONE',  ( 5.926322542504858681, 8.007405281046052536, -1.443375672974078761 ) ) ;
#115157 = CARTESIAN_POINT ( 'NONE',  ( -11.91826848330605593, 10.09270354043010798, -1.400000080589192120 ) ) ;
#115158 = CARTESIAN_POINT ( 'NONE',  ( 2.572451567087580493, -2.097416440861415321, -0.6350555677336399141 ) ) ;
#115159 = EDGE_CURVE ( 'NONE', #85209, #184855, #76316, .T. ) ;
#115161 = CARTESIAN_POINT ( 'NONE',  ( 7.391166297744269365, 11.77477778067701664, 1.040834085586084257E-14 ) ) ;
#115160 = CARTESIAN_POINT ( 'NONE',  ( 6.566864649055507819, 1.378042638564499489, -1.251022615016267103 ) ) ;
#115162 = CARTESIAN_POINT ( 'NONE',  ( 4.235878408818731344, 1.915113449751761010, -0.05082400106456300831 ) ) ;
#115163 = DIRECTION ( 'NONE',  ( -5.421010862427537947E-16, 0.000000000000000000, 1.000000000000000000 ) ) ;
#115164 = SURFACE_STYLE_USAGE ( .BOTH. , #162798 ) ;
#115165 = CARTESIAN_POINT ( 'NONE',  ( -1.364683531250014514, 0.2802083336747505649, 0.7879004041258379498 ) ) ;
#115166 = CARTESIAN_POINT ( 'NONE',  ( 5.016153647376196290, 8.796003655340152605, 0.7216878364870438212 ) ) ;
#115168 = CARTESIAN_POINT ( 'NONE',  ( 5.419199134695255715, -1.912947687149676668, 0.9079543477103575455 ) ) ;
#115167 = CARTESIAN_POINT ( 'NONE',  ( -10.46653140006992899, 11.31330084294416771, -0.7216878364870267237 ) ) ;
#115169 = CARTESIAN_POINT ( 'NONE',  ( 1.200320640528436789, -2.161883444890321915, 0.0006282887012112879947 ) ) ;
#115170 = CARTESIAN_POINT ( 'NONE',  ( -6.784929528996132220, 6.880448970109080520, 0.000000000000000000 ) ) ;
#115171 = CARTESIAN_POINT ( 'NONE',  ( 5.564695703766185275, 5.456842840674144490, 0.000000000000000000 ) ) ;
#115172 = CARTESIAN_POINT ( 'NONE',  ( 0.4811275135914867551, 1.705355465787803393, -0.6520327999673739550 ) ) ;
#115173 = CARTESIAN_POINT ( 'NONE',  ( -3.242371291962510504, 6.934516940598226320, 1.040834085586084257E-14 ) ) ;
#115174 = CARTESIAN_POINT ( 'NONE',  ( 3.030095697178539549, 1.015519584536026976, -1.516846343748608605 ) ) ;
#115175 = ADVANCED_FACE ( 'NONE', ( #176734, #16329 ), #161564, .T. ) ;
#115176 = CARTESIAN_POINT ( 'NONE',  ( 9.235375178776246585, 13.16128858080087660, -9.014701623559966848 ) ) ;
#115177 = ORIENTED_EDGE ( 'NONE', *, *, #46152, .F. ) ;
#115178 = CARTESIAN_POINT ( 'NONE',  ( 3.121499051359075239, 0.2915335129191589103, -1.947736612120597455 ) ) ;
#115179 = ORIENTED_EDGE ( 'NONE', *, *, #160804, .T. ) ;
#115180 = CARTESIAN_POINT ( 'NONE',  ( 4.405766152992893758, -0.8336290453338083273, -1.754189941349618920 ) ) ;
#115181 = CARTESIAN_POINT ( 'NONE',  ( -5.725286006720766707, 9.901527117808042178, 0.7998128361456291469 ) ) ;
#115183 = CARTESIAN_POINT ( 'NONE',  ( 5.185831674374465905, 2.043064739972153543, -0.5678235988075125418 ) ) ;
#115182 = CARTESIAN_POINT ( 'NONE',  ( 5.397027666691686321, 8.454226823519094935, 1.199719254218451159 ) ) ;
#115184 = CARTESIAN_POINT ( 'NONE',  ( -4.596923820214036560, 8.483565078729160547, 0.2266403168418751335 ) ) ;
#115185 = CARTESIAN_POINT ( 'NONE',  ( 3.264218543254516103, 1.912461472423478970, -0.002497826895729581952 ) ) ;
#115186 = CARTESIAN_POINT ( 'NONE',  ( 5.877843389052785028, 6.166481636157870483, -0.8510708418205383818 ) ) ;
#115187 = DIRECTION ( 'NONE',  ( 0.9992060137953822085, 0.000000000000000000, -0.03984146075563027578 ) ) ;
#115188 = CARTESIAN_POINT ( 'NONE',  ( 5.727393547130178675, 5.646656991265468939, 0.000000000000000000 ) ) ;
#115189 = CARTESIAN_POINT ( 'NONE',  ( 3.985207087413062066, 6.736826471035503694, -1.199719254218452047 ) ) ;
#115190 = AXIS2_PLACEMENT_3D ( 'NONE', #185673, #182473, #37302 ) ;
#115191 = CARTESIAN_POINT ( 'NONE',  ( 4.318997845537309033, 1.554796018123940193, -1.278706705004019506 ) ) ;
#115192 = CARTESIAN_POINT ( 'NONE',  ( -0.2713731142545342534, 2.604673336870401812, 1.982545097633750197 ) ) ;
#115193 = CARTESIAN_POINT ( 'NONE',  ( 4.793472150574508817, 1.354911484294840429, 1.223852735664505698 ) ) ;
#115194 = CARTESIAN_POINT ( 'NONE',  ( 0.4497787391488928810, 1.533077660697563793, 1.391591089521776681 ) ) ;
#115195 = CARTESIAN_POINT ( 'NONE',  ( -9.517460647113315630, 10.20605163116143821, 0.7216878364870438212 ) ) ;
#115196 = CARTESIAN_POINT ( 'NONE',  ( -6.081163491871431681, 7.123212080692602477, 1.153528356629534013 ) ) ;
#115197 = CARTESIAN_POINT ( 'NONE',  ( 0.000000000000000000, 1.000000000000000888, 0.000000000000000000 ) ) ;
#115198 = CARTESIAN_POINT ( 'NONE',  ( 6.227412191919261986, -1.760757567598171480, 0.6321290105378990498 ) ) ;
#115199 = CARTESIAN_POINT ( 'NONE',  ( 5.764187864104357573, 9.876636274763768597, 1.040834085586084257E-14 ) ) ;
#115200 = CARTESIAN_POINT ( 'NONE',  ( -4.761938266897808525, 6.578680616179307883, 1.599625672291267175 ) ) ;
#115201 = CARTESIAN_POINT ( 'NONE',  ( -1.402160292154681736E-14, 10.98437500034139802, 1.575800808251682339 ) ) ;
#115202 = CARTESIAN_POINT ( 'NONE',  ( -5.331380718671772101, 7.243030143248949670, -1.599625672291256295 ) ) ;
#115203 = CARTESIAN_POINT ( 'NONE',  ( 4.207107738942202246, 3.802713871720993399, 1.214306433183764966E-14 ) ) ;
#115204 = CARTESIAN_POINT ( 'NONE',  ( -3.133342898089680695, 6.669667457830990465, 0.7216878364870338292 ) ) ;
#115205 = VECTOR ( 'NONE', #151511, 1000.000000000000114 ) ;
#115206 = CARTESIAN_POINT ( 'NONE',  ( -5.205440912643032547, 8.160432600470439723, 1.199719254218452047 ) ) ;
#115207 = CIRCLE ( 'NONE', #135869, 0.8299999999999999600 ) ;
#115208 = CARTESIAN_POINT ( 'NONE',  ( 1.094682738308445202, 2.038987083759949304, 0.3576228084290478115 ) ) ;
#115209 = CARTESIAN_POINT ( 'NONE',  ( 2.794651083563943761, 1.531546425470770245, -1.462076589042210495 ) ) ;
#115210 = CARTESIAN_POINT ( 'NONE',  ( 8.269583629331492602, 11.73526576994040482, 1.199719254218450271 ) ) ;
#115211 = DIRECTION ( 'NONE',  ( 1.000000000000000000, -2.168404344971003188E-14, 0.000000000000000000 ) ) ;
#115212 = CARTESIAN_POINT ( 'NONE',  ( 6.104363016364067640, 2.067617457866403718, 0.1074407263862015016 ) ) ;
#115213 = CARTESIAN_POINT ( 'NONE',  ( 4.981510052282690282, 6.816019998287410786, 1.424969591591069396 ) ) ;
#115214 = CARTESIAN_POINT ( 'NONE',  ( 6.019457014787495730, 6.125047393447951016, -0.7216878364870257245 ) ) ;
#115216 = CYLINDRICAL_SURFACE ( 'NONE', #1313, 0.08000000000000041800 ) ;
#115215 = CARTESIAN_POINT ( 'NONE',  ( 11.41157692552970815, 9.840896629130003959, -3.404533818002362100 ) ) ;
#115217 = CARTESIAN_POINT ( 'NONE',  ( 2.713130565535960770, -0.2235823006870632790, 2.281328536464954038 ) ) ;
#115219 = FACE_OUTER_BOUND ( 'NONE', #210344, .T. ) ;
#115218 = CARTESIAN_POINT ( 'NONE',  ( -7.015401035077363900, 6.062865449010540253, 2.437084766375293476 ) ) ;
#115220 = CARTESIAN_POINT ( 'NONE',  ( 2.759904966095374501, 0.6844231338998980618, -1.785916880244736715 ) ) ;
#115221 = ORIENTED_EDGE ( 'NONE', *, *, #19306, .T. ) ;
#115222 = CARTESIAN_POINT ( 'NONE',  ( 8.405692050348340771, 8.908988268268968724, 1.040834085586084257E-14 ) ) ;
#115223 = ADVANCED_FACE ( 'NONE', ( #94443 ), #113153, .T. ) ;
#115224 = CIRCLE ( 'NONE', #142866, 0.08000000000000020983 ) ;
#115225 = CARTESIAN_POINT ( 'NONE',  ( 0.2287712656204986261, 1.385237311202421662, -1.461098210751586857 ) ) ;
#115226 = CARTESIAN_POINT ( 'NONE',  ( 1.199968502355329703, 0.8001272530510427083, -1.791371145023381128 ) ) ;
#115227 = CARTESIAN_POINT ( 'NONE',  ( -7.974166903131914452, 12.45494515362926435, -0.7998128361456281477 ) ) ;
#115228 = CARTESIAN_POINT ( 'NONE',  ( -6.690058733339450114, 9.892486724616283311, 1.199719254218452047 ) ) ;
#115229 = DIRECTION ( 'NONE',  ( 0.000000000000000000, 0.000000000000000000, -1.000000000000000000 ) ) ;
#115231 = CARTESIAN_POINT ( 'NONE',  ( 2.324752472428833983, -0.002986221762550990942, 1.770032028303660576 ) ) ;
#115230 = CARTESIAN_POINT ( 'NONE',  ( 4.119144422497845959, -2.000575632760223765, 0.6069725389450402186 ) ) ;
#115232 = CARTESIAN_POINT ( 'NONE',  ( -10.88266508516670150, 3.691791674785632082, 3.942622913914227922 ) ) ;
#115234 = CARTESIAN_POINT ( 'NONE',  ( 4.769621702613293657, 1.317199799690757178, 1.875844486027035574 ) ) ;
#115233 = FACE_OUTER_BOUND ( 'NONE', #61360, .T. ) ;
#115235 = CARTESIAN_POINT ( 'NONE',  ( 4.171615353782907931, -0.9995084519054014960, 1.424469360818179986 ) ) ;
#115236 = VECTOR ( 'NONE', #12272, 1000.000000000000227 ) ;
#115237 = CARTESIAN_POINT ( 'NONE',  ( 9.725276259704228821, 10.24057714594344048, 0.7998128361456462443 ) ) ;
#115238 = CARTESIAN_POINT ( 'NONE',  ( 4.200348813226637112, -1.195399808894830773, -1.256130793262473455 ) ) ;
#115239 = CARTESIAN_POINT ( 'NONE',  ( 5.125502745298136098, 0.2179265861129157655, -2.160231653469760982 ) ) ;
#115240 = CARTESIAN_POINT ( 'NONE',  ( 2.333974999846879061, 5.874721266463329705, -0.7998128361456291469 ) ) ;
#115241 = CARTESIAN_POINT ( 'NONE',  ( 5.225796113160614986, 0.8128206588041908542, -1.845625551132886288 ) ) ;
#115242 = CARTESIAN_POINT ( 'NONE',  ( 6.750000000000005329, 3.748112931134527976E-13, 1.999999999999984901 ) ) ;
#115243 = CARTESIAN_POINT ( 'NONE',  ( -1.500000000000011324, 4.410416667349484676, -0.8660254037844313801 ) ) ;
#115244 = CARTESIAN_POINT ( 'NONE',  ( 2.661056112795460837, -1.675086148048400503, -0.9512456543366625272 ) ) ;
#115245 = CARTESIAN_POINT ( 'NONE',  ( -1.500000000000001110, 10.55208333401613352, 0.8660254037844419273 ) ) ;
#115246 = CARTESIAN_POINT ( 'NONE',  ( 5.203485844055394161, 1.958870149131001881, -1.047680120605886556 ) ) ;
#115247 = ORIENTED_EDGE ( 'NONE', *, *, #205822, .T. ) ;
#115248 = CARTESIAN_POINT ( 'NONE',  ( 6.883263157960335832, 6.035928496661214560, 2.641088654967935323 ) ) ;
#115249 = CARTESIAN_POINT ( 'NONE',  ( 0.7499999999999902300, 3.233333333333352044, 1.299038105676669330 ) ) ;
#115250 = CARTESIAN_POINT ( 'NONE',  ( 6.100279051144945619, 9.204410428722734849, -1.199719254218440723 ) ) ;
#115251 = CARTESIAN_POINT ( 'NONE',  ( 6.619590441841330275, 0.3365870006281460047, -1.932621868259084330 ) ) ;
#115252 = CARTESIAN_POINT ( 'NONE',  ( 7.104109303880752790, 11.23195192126214970, -0.7216878364870267237 ) ) ;
#115253 = CARTESIAN_POINT ( 'NONE',  ( 0.4019237886466778820, 10.10491455036742892, 1.500000000000001554 ) ) ;
#115254 = CARTESIAN_POINT ( 'NONE',  ( 5.225741863424510747, 5.061396693608882558, 0.7998128361456352531 ) ) ;
#115255 = CARTESIAN_POINT ( 'NONE',  ( -0.08726289061519039436, -1.242903867559573161, -1.588418431006669351 ) ) ;
#115257 = CARTESIAN_POINT ( 'NONE',  ( 4.773915743512389120, -2.023523412367009833, 0.3991901646795847913 ) ) ;
#115256 = CARTESIAN_POINT ( 'NONE',  ( 9.459838494033030898, 12.05956421450382088, 1.599625672291281386 ) ) ;
#115258 = CARTESIAN_POINT ( 'NONE',  ( -4.765854690403601879, 5.518917546014321829, 1.199719254218462483 ) ) ;
#115259 = CARTESIAN_POINT ( 'NONE',  ( 0.7499999999999920064, 5.264583334016151639, 1.299038105676669330 ) ) ;
#115260 = CARTESIAN_POINT ( 'NONE',  ( 1.364683531249986537, -0.5947916663252456049, -0.7879004041258309554 ) ) ;
#115261 = CARTESIAN_POINT ( 'NONE',  ( 5.676977070516882051, -0.04517083460114229565, -1.870152005306220611 ) ) ;
#115262 = CARTESIAN_POINT ( 'NONE',  ( 4.852092609920839905, 0.1625460678297725725, -1.726498261149024271 ) ) ;
#115263 = CARTESIAN_POINT ( 'NONE',  ( 4.388070221843799246, -0.3869516340575751001, -1.696700118790330558 ) ) ;
#115264 = CARTESIAN_POINT ( 'NONE',  ( 2.659370686574860976, 6.254349567645977714, -0.7998128361456291469 ) ) ;
#115265 = EDGE_CURVE ( 'NONE', #164527, #163622, #50606, .T. ) ;
#115266 = CARTESIAN_POINT ( 'NONE',  ( 2.138584244316643179, 0.5063124247480701445, 2.235611027800854078 ) ) ;
#115267 = CARTESIAN_POINT ( 'NONE',  ( -1.364683531250010295, 5.342708333674750953, 0.7879004041258379498 ) ) ;
#115268 = CARTESIAN_POINT ( 'NONE',  ( 5.232010533483211212, 2.060019964192044917, 0.3561100859283144460 ) ) ;
#115269 = CARTESIAN_POINT ( 'NONE',  ( 1.235996726672627943, 0.3573974351761283752, 1.805938768738392319 ) ) ;
#115270 = CARTESIAN_POINT ( 'NONE',  ( 4.068383102448127175, 7.735681852393593516, 0.5751369358401996479 ) ) ;
#115271 = CARTESIAN_POINT ( 'NONE',  ( 2.865861461037176205, -0.1511401116795624278, -2.010826411938296143 ) ) ;
#115272 = CARTESIAN_POINT ( 'NONE',  ( 1.465048628566959277, 0.1585425061045864503, -2.185770122351132994 ) ) ;
#115273 = CARTESIAN_POINT ( 'NONE',  ( 9.258966325506417405, 13.63624071251986258, -6.830021722722439570 ) ) ;
#115274 = CARTESIAN_POINT ( 'NONE',  ( -8.227100285394159940, 8.492705175914988303, 0.7998128361456602331 ) ) ;
#115275 =( BOUNDED_SURFACE ( )  B_SPLINE_SURFACE ( 1, 2, ( 
 ( #23805, #73633, #124611, #190569, #139732, #203605, #205756, #56324, #121405, #187377, #57386, #41160, #107269, #173289, #8625, #140810, #54884, #152383, #137220, #83095, #3961, #51693, #136144, #19163, #149174, #203240, #198963, #20226, #17019, #18085, #70029, #185925, #85237, #36486, #167563, #135085, #121038, #50607, #202162, #116732, #187005, #102563, #182731, #134034, #132960, #100423, #53820, #201099, #52739, #184859, #168623, #34350, #751, #119950, #86311, #101493, #66817, #37561, #151325, #103641, #166494, #35415, #169693, #5027, #21281, #118873, #1830, #87387, #67889, #84173, #150262, #2893, #200042, #117815, #183805, #153454, #68966, #38636, #71102, #104715, #139353, #106894, #189150, #206457, #207528, #124246, #171835, #88464, #55953, #22352, #204297, #57022, #155590, #123189, #73246, #72174, #90607, #191263, #26645, #122106, #190204, #175058, #92746, #188071, #172920, #23428, #154524, #138282, #6104, #24496, #39700, #7175, #105809, #140446, #158790, #41864, #10387, #126372, #107973, #208578, #75407, #40789, #109039, #156666, #76462, #9334, #142571, #174002, #205383, #58084, #25573, #8258, #91684, #74342, #89539, #157737, #141520, #59147, #125305, #60211, #42929, #192331, #43990, #170763, #46940, #197420, #45873, #164929, #130384, #81547, #62108, #14394, #115182, #198476, #82604, #114131, #195309, #49062, #113058, #79417, #29611, #146585, #210470, #161751, #95696, #258, #13342, #99936, #98876, #50121, #179064, #212602, #80485, #31748, #32802, #163886, #211532, #128267, #145534, #194229, #63167, #96766, #30683, #162817, #64240, #111995, #129333, #196374, #83666, #48014, #180123, #15461, #97821, #147630, #148689, #116242, #177997, #213648, #65274, #131420, #181177, #16521, #66329, #132474, #182231, #33855, #165998, #17583, #19734, #87949, #149757, #3467, #85813, #150832, #18664, #21841, #187572, #102067, #52249, #201666, #170256, #104209, #35986, #118376, #51185, #2394, #151892, #22921, #200602, #69536, #103136, #135643, #53313, #154023, #137783, #1334, #185433, #4524, #67395, #119445, #54389 ),
 ( #136713, #133536, #117308, #37053, #169194, #199543, #121600, #186506, #183304, #5590, #34911, #100983, #167072, #84744, #20787, #71669, #203802, #68473, #86882, #55448, #39197, #134601, #152949, #184364, #168132, #70599, #202738, #120527, #38137, #105289, #171325, #58653, #10945, #108535, #77019, #44554, #42430, #126941, #208085, #107471, #27206, #173497, #143148, #142071, #209143, #174565, #73834, #190766, #26141, #25073, #92254, #189708, #138851, #122683, #74906, #158300, #155091, #159348, #91175, #191831, #205957, #157234, #6677, #123747, #109614, #204868, #8829, #110670, #89036, #57590, #125872, #192898, #141014, #41361, #188646, #176670, #72754, #56523, #60782, #207022, #93313, #124807, #40277, #106387, #9891, #172410, #23998, #75968, #59712, #43494, #90101, #156166, #7747, #175619, #139930, #78094, #61851, #16266, #148441, #111737, #147379, #94377, #128018, #146328, #13082, #15211, #79162, #177743, #193972, #178817, #28282, #45620, #29358, #32545, #95452, #132216, #131182, #82350, #211284, #30430, #46686, #63984, #65027, #196126, #161502, #160417, #145278, #12022, #62907, #129077, #195048, #112804, #96516, #144221, #162565, #14137, #115988, #80230, #212343, #47764, #130137, #113878, #114925, #9, #210215, #179873, #97573, #31498, #163630, #213406, #81302, #98620, #197172, #48808, #180924, #164681, #66074, #198225, #49861, #35729, #51998, #183051, #50929, #54128, #5329, #134344, #84485, #19472, #202475, #136457, #68214, #87685, #118124, #117054, #70340, #55193, #100736, #186239, #150575, #184109, #21580, #120265, #71410, #102877, #153759, #33607, #168935, #2137, #86620, #101805, #99677, #137522, #149496, #185168, #181976, #34666, #20538, #37874, #167874, #201410, #85549, #151639, #203539, #1079, #152688, #67144, #165747, #53049, #133278, #200349, #83414, #166815, #4270, #3206, #69275, #135389, #119182, #199286, #17333, #103951, #18409, #169993, #36792, #75703, #41093, #206758, #187314, #139666, #25871, #109346, #207820, #154828, #57323, #121339, #72485, #6413, #125605, #138586, #10683, #9626, #175356 ) ),
 .UNSPECIFIED., .F., .F., .T. ) 
 B_SPLINE_SURFACE_WITH_KNOTS ( ( 2, 2 ),
 ( 3, 2, 2, 2, 2, 2, 2, 2, 2, 2, 2, 2, 2, 2, 2, 2, 2, 2, 2, 2, 2, 2, 2, 2, 2, 2, 2, 2, 2, 2, 2, 2, 2, 2, 2, 2, 2, 2, 2, 2, 2, 2, 2, 2, 2, 2, 2, 2, 2, 2, 2, 2, 2, 2, 2, 2, 2, 2, 2, 2, 2, 2, 2, 2, 2, 2, 2, 2, 2, 2, 2, 2, 2, 2, 2, 2, 2, 2, 2, 2, 2, 2, 2, 2, 2, 2, 2, 2, 2, 2, 2, 2, 2, 2, 2, 2, 2, 2, 2, 2, 2, 2, 2, 2, 2, 2, 2, 2, 2, 2, 2, 2, 2, 2, 2, 2, 2, 2, 2, 2, 3 ),
 ( 0.000000000000000000, 1.000000000000000000 ),
 ( 0.000000000000000000, 0.008333333333333333218, 0.01666666666666666644, 0.02500000000000000139, 0.03333333333333333287, 0.04166666666666666435, 0.05000000000000000278, 0.05833333333333333426, 0.06666666666666666574, 0.07499999999999999722, 0.08333333333333332871, 0.09166666666666666019, 0.1000000000000000056, 0.1083333333333333370, 0.1166666666666666685, 0.1250000000000000000, 0.1333333333333333315, 0.1416666666666666630, 0.1499999999999999944, 0.1583333333333333259, 0.1666666666666666574, 0.1749999999999999889, 0.1833333333333333204, 0.1916666666666666796, 0.2000000000000000111, 0.2083333333333333426, 0.2166666666666666741, 0.2250000000000000056, 0.2333333333333333370, 0.2416666666666666685, 0.2500000000000000000, 0.2583333333333333592, 0.2666666666666666630, 0.2750000000000000222, 0.2833333333333333259, 0.2916666666666666852, 0.2999999999999999889, 0.3083333333333333481, 0.3166666666666666519, 0.3250000000000000111, 0.3333333333333333148, 0.3416666666666666741, 0.3499999999999999778, 0.3583333333333333370, 0.3666666666666666408, 0.3750000000000000000, 0.3833333333333333592, 0.3916666666666666630, 0.4000000000000000222, 0.4083333333333333259, 0.4166666666666666852, 0.4249999999999999889, 0.4333333333333333481, 0.4416666666666666519, 0.4500000000000000111, 0.4583333333333333148, 0.4666666666666666741, 0.4749999999999999778, 0.4833333333333333370, 0.4916666666666666408, 0.5000000000000000000, 0.5083333333333333037, 0.5166666666666667185, 0.5250000000000000222, 0.5333333333333333259, 0.5416666666666666297, 0.5500000000000000444, 0.5583333333333333481, 0.5666666666666666519, 0.5749999999999999556, 0.5833333333333333703, 0.5916666666666666741, 0.5999999999999999778, 0.6083333333333332815, 0.6166666666666666963, 0.6250000000000000000, 0.6333333333333333037, 0.6416666666666667185, 0.6500000000000000222, 0.6583333333333333259, 0.6666666666666666297, 0.6750000000000000444, 0.6833333333333333481, 0.6916666666666666519, 0.6999999999999999556, 0.7083333333333333703, 0.7166666666666666741, 0.7249999999999999778, 0.7333333333333332815, 0.7416666666666666963, 0.7500000000000000000, 0.7583333333333333037, 0.7666666666666667185, 0.7750000000000000222, 0.7833333333333333259, 0.7916666666666666297, 0.8000000000000000444, 0.8083333333333333481, 0.8166666666666666519, 0.8249999999999999556, 0.8333333333333333703, 0.8416666666666666741, 0.8499999999999999778, 0.8583333333333332815, 0.8666666666666666963, 0.8750000000000000000, 0.8833333333333333037, 0.8916666666666667185, 0.9000000000000000222, 0.9083333333333333259, 0.9166666666666666297, 0.9250000000000000444, 0.9333333333333333481, 0.9416666666666666519, 0.9499999999999999556, 0.9583333333333333703, 0.9666666666666666741, 0.9749999999999999778, 0.9833333333333332815, 0.9916666666666666963, 1.000000000000000000 ),
 .UNSPECIFIED. ) 
 GEOMETRIC_REPRESENTATION_ITEM ( )  RATIONAL_B_SPLINE_SURFACE ( (
 ( 1.000000000000000000, 0.8660254037844387076, 1.000000000000000000, 0.8660254037844387076, 1.000000000000000000, 0.8660254037844387076, 1.000000000000000000, 0.8660254037844387076, 1.000000000000000000, 0.8660254037844387076, 1.000000000000000000, 0.8660254037844387076, 1.000000000000000000, 0.8660254037844387076, 1.000000000000000000, 0.8660254037844387076, 1.000000000000000000, 0.8660254037844387076, 1.000000000000000000, 0.8660254037844387076, 1.000000000000000000, 0.8660254037844387076, 1.000000000000000000, 0.8660254037844387076, 1.000000000000000000, 0.8660254037844387076, 1.000000000000000000, 0.8660254037844387076, 1.000000000000000000, 0.8660254037844387076, 1.000000000000000000, 0.8660254037844387076, 1.000000000000000000, 0.8660254037844387076, 1.000000000000000000, 0.8660254037844387076, 1.000000000000000000, 0.8660254037844387076, 1.000000000000000000, 0.8660254037844387076, 1.000000000000000000, 0.8660254037844387076, 1.000000000000000000, 0.8660254037844387076, 1.000000000000000000, 0.8660254037844387076, 1.000000000000000000, 0.8660254037844387076, 1.000000000000000000, 0.8660254037844387076, 1.000000000000000000, 0.8660254037844387076, 1.000000000000000000, 0.8660254037844387076, 1.000000000000000000, 0.8660254037844387076, 1.000000000000000000, 0.8660254037844387076, 1.000000000000000000, 0.8660254037844387076, 1.000000000000000000, 0.8660254037844387076, 1.000000000000000000, 0.8660254037844387076, 1.000000000000000000, 0.8660254037844387076, 1.000000000000000000, 0.8660254037844387076, 1.000000000000000000, 0.8660254037844387076, 1.000000000000000000, 0.8660254037844387076, 1.000000000000000000, 0.8660254037844387076, 1.000000000000000000, 0.8660254037844387076, 1.000000000000000000, 0.8660254037844387076, 1.000000000000000000, 0.8660254037844387076, 1.000000000000000000, 0.8660254037844387076, 1.000000000000000000, 0.8660254037844387076, 1.000000000000000000, 0.8660254037844387076, 1.000000000000000000, 0.8660254037844387076, 1.000000000000000000, 0.8660254037844387076, 1.000000000000000000, 0.8660254037844387076, 1.000000000000000000, 0.8660254037844387076, 1.000000000000000000, 0.8660254037844387076, 1.000000000000000000, 0.8660254037844387076, 1.000000000000000000, 0.8660254037844387076, 1.000000000000000000, 0.8660254037844387076, 1.000000000000000000, 0.8660254037844387076, 1.000000000000000000, 0.8660254037844387076, 1.000000000000000000, 0.8660254037844387076, 1.000000000000000000, 0.8660254037844387076, 1.000000000000000000, 0.8660254037844387076, 1.000000000000000000, 0.8660254037844387076, 1.000000000000000000, 0.8660254037844387076, 1.000000000000000000, 0.8660254037844387076, 1.000000000000000000, 0.8660254037844387076, 1.000000000000000000, 0.8660254037844387076, 1.000000000000000000, 0.8660254037844387076, 1.000000000000000000, 0.8660254037844387076, 1.000000000000000000, 0.8660254037844387076, 1.000000000000000000, 0.8660254037844387076, 1.000000000000000000, 0.8660254037844387076, 1.000000000000000000, 0.8660254037844387076, 1.000000000000000000, 0.8660254037844387076, 1.000000000000000000, 0.8660254037844387076, 1.000000000000000000, 0.8660254037844387076, 1.000000000000000000, 0.8660254037844387076, 1.000000000000000000, 0.8660254037844387076, 1.000000000000000000, 0.8660254037844387076, 1.000000000000000000, 0.8660254037844387076, 1.000000000000000000, 0.8660254037844387076, 1.000000000000000000, 0.8660254037844387076, 1.000000000000000000, 0.8660254037844387076, 1.000000000000000000, 0.8660254037844387076, 1.000000000000000000, 0.8660254037844387076, 1.000000000000000000, 0.8660254037844387076, 1.000000000000000000, 0.8660254037844387076, 1.000000000000000000, 0.8660254037844387076, 1.000000000000000000, 0.8660254037844387076, 1.000000000000000000, 0.8660254037844387076, 1.000000000000000000, 0.8660254037844387076, 1.000000000000000000, 0.8660254037844387076, 1.000000000000000000, 0.8660254037844387076, 1.000000000000000000, 0.8660254037844387076, 1.000000000000000000, 0.8660254037844387076, 1.000000000000000000, 0.8660254037844387076, 1.000000000000000000, 0.8660254037844387076, 1.000000000000000000, 0.8660254037844387076, 1.000000000000000000, 0.8660254037844387076, 1.000000000000000000, 0.8660254037844387076, 1.000000000000000000, 0.8660254037844387076, 1.000000000000000000, 0.8660254037844387076, 1.000000000000000000, 0.8660254037844387076, 1.000000000000000000, 0.8660254037844387076, 1.000000000000000000, 0.8660254037844387076, 1.000000000000000000, 0.8660254037844387076, 1.000000000000000000, 0.8660254037844387076, 1.000000000000000000, 0.8660254037844387076, 1.000000000000000000, 0.8660254037844387076, 1.000000000000000000, 0.8660254037844387076, 1.000000000000000000, 0.8660254037844387076, 1.000000000000000000, 0.8660254037844387076, 1.000000000000000000, 0.8660254037844387076, 1.000000000000000000, 0.8660254037844387076, 1.000000000000000000, 0.8660254037844387076, 1.000000000000000000, 0.8660254037844387076, 1.000000000000000000, 0.8660254037844387076, 1.000000000000000000, 0.8660254037844387076, 1.000000000000000000, 0.8660254037844387076, 1.000000000000000000, 0.8660254037844387076, 1.000000000000000000, 0.8660254037844387076, 1.000000000000000000, 0.8660254037844387076, 1.000000000000000000, 0.8660254037844387076, 1.000000000000000000, 0.8660254037844387076, 1.000000000000000000, 0.8660254037844387076, 1.000000000000000000, 0.8660254037844387076, 1.000000000000000000),
 ( 1.000000000000000000, 0.8660254037844387076, 1.000000000000000000, 0.8660254037844387076, 1.000000000000000000, 0.8660254037844387076, 1.000000000000000000, 0.8660254037844387076, 1.000000000000000000, 0.8660254037844387076, 1.000000000000000000, 0.8660254037844387076, 1.000000000000000000, 0.8660254037844387076, 1.000000000000000000, 0.8660254037844387076, 1.000000000000000000, 0.8660254037844387076, 1.000000000000000000, 0.8660254037844387076, 1.000000000000000000, 0.8660254037844387076, 1.000000000000000000, 0.8660254037844387076, 1.000000000000000000, 0.8660254037844387076, 1.000000000000000000, 0.8660254037844387076, 1.000000000000000000, 0.8660254037844387076, 1.000000000000000000, 0.8660254037844387076, 1.000000000000000000, 0.8660254037844387076, 1.000000000000000000, 0.8660254037844387076, 1.000000000000000000, 0.8660254037844387076, 1.000000000000000000, 0.8660254037844387076, 1.000000000000000000, 0.8660254037844387076, 1.000000000000000000, 0.8660254037844387076, 1.000000000000000000, 0.8660254037844387076, 1.000000000000000000, 0.8660254037844387076, 1.000000000000000000, 0.8660254037844387076, 1.000000000000000000, 0.8660254037844387076, 1.000000000000000000, 0.8660254037844387076, 1.000000000000000000, 0.8660254037844387076, 1.000000000000000000, 0.8660254037844387076, 1.000000000000000000, 0.8660254037844387076, 1.000000000000000000, 0.8660254037844387076, 1.000000000000000000, 0.8660254037844387076, 1.000000000000000000, 0.8660254037844387076, 1.000000000000000000, 0.8660254037844387076, 1.000000000000000000, 0.8660254037844387076, 1.000000000000000000, 0.8660254037844387076, 1.000000000000000000, 0.8660254037844387076, 1.000000000000000000, 0.8660254037844387076, 1.000000000000000000, 0.8660254037844387076, 1.000000000000000000, 0.8660254037844387076, 1.000000000000000000, 0.8660254037844387076, 1.000000000000000000, 0.8660254037844387076, 1.000000000000000000, 0.8660254037844387076, 1.000000000000000000, 0.8660254037844387076, 1.000000000000000000, 0.8660254037844387076, 1.000000000000000000, 0.8660254037844387076, 1.000000000000000000, 0.8660254037844387076, 1.000000000000000000, 0.8660254037844387076, 1.000000000000000000, 0.8660254037844387076, 1.000000000000000000, 0.8660254037844387076, 1.000000000000000000, 0.8660254037844387076, 1.000000000000000000, 0.8660254037844387076, 1.000000000000000000, 0.8660254037844387076, 1.000000000000000000, 0.8660254037844387076, 1.000000000000000000, 0.8660254037844387076, 1.000000000000000000, 0.8660254037844387076, 1.000000000000000000, 0.8660254037844387076, 1.000000000000000000, 0.8660254037844387076, 1.000000000000000000, 0.8660254037844387076, 1.000000000000000000, 0.8660254037844387076, 1.000000000000000000, 0.8660254037844387076, 1.000000000000000000, 0.8660254037844387076, 1.000000000000000000, 0.8660254037844387076, 1.000000000000000000, 0.8660254037844387076, 1.000000000000000000, 0.8660254037844387076, 1.000000000000000000, 0.8660254037844387076, 1.000000000000000000, 0.8660254037844387076, 1.000000000000000000, 0.8660254037844387076, 1.000000000000000000, 0.8660254037844387076, 1.000000000000000000, 0.8660254037844387076, 1.000000000000000000, 0.8660254037844387076, 1.000000000000000000, 0.8660254037844387076, 1.000000000000000000, 0.8660254037844387076, 1.000000000000000000, 0.8660254037844387076, 1.000000000000000000, 0.8660254037844387076, 1.000000000000000000, 0.8660254037844387076, 1.000000000000000000, 0.8660254037844387076, 1.000000000000000000, 0.8660254037844387076, 1.000000000000000000, 0.8660254037844387076, 1.000000000000000000, 0.8660254037844387076, 1.000000000000000000, 0.8660254037844387076, 1.000000000000000000, 0.8660254037844387076, 1.000000000000000000, 0.8660254037844387076, 1.000000000000000000, 0.8660254037844387076, 1.000000000000000000, 0.8660254037844387076, 1.000000000000000000, 0.8660254037844387076, 1.000000000000000000, 0.8660254037844387076, 1.000000000000000000, 0.8660254037844387076, 1.000000000000000000, 0.8660254037844387076, 1.000000000000000000, 0.8660254037844387076, 1.000000000000000000, 0.8660254037844387076, 1.000000000000000000, 0.8660254037844387076, 1.000000000000000000, 0.8660254037844387076, 1.000000000000000000, 0.8660254037844387076, 1.000000000000000000, 0.8660254037844387076, 1.000000000000000000, 0.8660254037844387076, 1.000000000000000000, 0.8660254037844387076, 1.000000000000000000, 0.8660254037844387076, 1.000000000000000000, 0.8660254037844387076, 1.000000000000000000, 0.8660254037844387076, 1.000000000000000000, 0.8660254037844387076, 1.000000000000000000, 0.8660254037844387076, 1.000000000000000000, 0.8660254037844387076, 1.000000000000000000, 0.8660254037844387076, 1.000000000000000000, 0.8660254037844387076, 1.000000000000000000, 0.8660254037844387076, 1.000000000000000000, 0.8660254037844387076, 1.000000000000000000, 0.8660254037844387076, 1.000000000000000000, 0.8660254037844387076, 1.000000000000000000, 0.8660254037844387076, 1.000000000000000000, 0.8660254037844387076, 1.000000000000000000, 0.8660254037844387076, 1.000000000000000000, 0.8660254037844387076, 1.000000000000000000, 0.8660254037844387076, 1.000000000000000000, 0.8660254037844387076, 1.000000000000000000, 0.8660254037844387076, 1.000000000000000000, 0.8660254037844387076, 1.000000000000000000, 0.8660254037844387076, 1.000000000000000000, 0.8660254037844387076, 1.000000000000000000, 0.8660254037844387076, 1.000000000000000000) ) ) 
 REPRESENTATION_ITEM ( '' )  SURFACE ( )  );
#115276 = CARTESIAN_POINT ( 'NONE',  ( 1.732962091629593804, -1.965256999408044436, -0.6514315320021792921 ) ) ;
#115277 = CARTESIAN_POINT ( 'NONE',  ( 5.138703914779377158, 5.953908307786102583, 1.199719254218462483 ) ) ;
#115278 = CARTESIAN_POINT ( 'NONE',  ( 1.360316468749955598, -0.9739583329918906074, 0.7853790794158580502 ) ) ;
#115279 = CARTESIAN_POINT ( 'NONE',  ( 3.967525559752110631, -1.763746451813380967, -1.176840329774282212 ) ) ;
#115280 = CARTESIAN_POINT ( 'NONE',  ( -1.364683531250014514, -0.2614583329919080157, -0.7879004041258359514 ) ) ;
#115282 = EDGE_CURVE ( 'NONE', #139590, #93819, #125512, .T. ) ;
#115281 = CARTESIAN_POINT ( 'NONE',  ( 0.08247339995742437868, -1.868340020190910833, -0.4694531300831055742 ) ) ;
#115283 = ORIENTED_EDGE ( 'NONE', *, *, #133829, .F. ) ;
#115284 = CARTESIAN_POINT ( 'NONE',  ( -5.818384198920079520, 6.817144982608731141, 1.199719254218452935 ) ) ;
#115285 = CARTESIAN_POINT ( 'NONE',  ( 8.062294901620731480, 12.55776115186623620, 1.040834085586084257E-14 ) ) ;
#115286 = CARTESIAN_POINT ( 'NONE',  ( 5.844973620822830895, 8.872867420051733234, 1.082531754730549967 ) ) ;
#115287 = CARTESIAN_POINT ( 'NONE',  ( -3.474999999999998312, -2.027083332377417779, 2.006292185433951047 ) ) ;
#115288 = CARTESIAN_POINT ( 'NONE',  ( -6.392833124043511894, 7.417059051927569868, 1.199719254218450271 ) ) ;
#115289 = CARTESIAN_POINT ( 'NONE',  ( 3.058857861556500968, 0.4949273143410140574, 1.958058250343613693 ) ) ;
#115290 = CARTESIAN_POINT ( 'NONE',  ( 1.483573828499670899, 1.945989852495342065, -0.8055925053903155719 ) ) ;
#115291 = CARTESIAN_POINT ( 'NONE',  ( -6.903036488013351679, 8.082572653217566128, -1.199719254218452047 ) ) ;
#115292 = CARTESIAN_POINT ( 'NONE',  ( 8.215351014876830504, 11.67199438640995801, -1.199719254218446718 ) ) ;
#115293 = CARTESIAN_POINT ( 'NONE',  ( 4.803460451949028709, -1.436610920757129817, -1.182842806638328526 ) ) ;
#115294 = CARTESIAN_POINT ( 'NONE',  ( 8.589254009457354400, 9.979550084910457031, -1.199719254218446718 ) ) ;
#115295 = DIRECTION ( 'NONE',  ( -5.551115123125766062E-17, 0.000000000000000000, 1.000000000000000000 ) ) ;
#115296 = CARTESIAN_POINT ( 'NONE',  ( -4.600294193738529103, 4.261431402316699035, -0.7998128361456221525 ) ) ;
#115297 = AXIS2_PLACEMENT_3D ( 'NONE', #149445, #33557, #183001 ) ;
#115298 = CARTESIAN_POINT ( 'NONE',  ( -6.344325816190970357, 9.489131654609717970, 1.199719254218452047 ) ) ;
#115299 = CARTESIAN_POINT ( 'NONE',  ( 6.819229409281153842, -0.1590044787766713985, 2.026160355490718601 ) ) ;
#115300 = AXIS2_PLACEMENT_3D ( 'NONE', #25042, #125840, #206990 ) ;
#115302 = CARTESIAN_POINT ( 'NONE',  ( -4.974982779204009553, 6.815313220028144769, 1.450550931683711298 ) ) ;
#115301 = CARTESIAN_POINT ( 'NONE',  ( -6.936931872047518155, 8.122117267924091166, 1.199719254218452047 ) ) ;
#115303 = CARTESIAN_POINT ( 'NONE',  ( -0.6823417656250003738, -0.03229166632524871350, -1.181850606188749264 ) ) ;
#115304 = CARTESIAN_POINT ( 'NONE',  ( 1.827078023146003760, -1.230200505038709036, 1.222094307470813934 ) ) ;
#115305 = CARTESIAN_POINT ( 'NONE',  ( 1.569815774166925859, -1.651746245857487638, -0.5483857920917082351 ) ) ;
#115307 = CARTESIAN_POINT ( 'NONE',  ( 5.666945020832160118, 9.555260257705446847, 0.7216878364870438212 ) ) ;
#115306 = CARTESIAN_POINT ( 'NONE',  ( 6.235062949421072531, 0.2195253172713066969, 2.297251706954360095 ) ) ;
#115308 = CARTESIAN_POINT ( 'NONE',  ( -11.78041000490145862, 4.728159582424554586, -4.968671142906706528 ) ) ;
#115309 = CARTESIAN_POINT ( 'NONE',  ( 2.143891142268034677, 0.7916089892260335104, -1.902880034897576733 ) ) ;
#115310 = EDGE_CURVE ( 'NONE', #206340, #78493, #195070, .T. ) ;
#115311 = CARTESIAN_POINT ( 'NONE',  ( 1.106795812180675798, 0.8196504822069600182, -1.842164015508622521 ) ) ;
#115312 = CARTESIAN_POINT ( 'NONE',  ( 8.857846419285928974, 14.66713266182295250, -8.029988375369475406 ) ) ;
#115313 = CARTESIAN_POINT ( 'NONE',  ( -5.204350862799341115, 7.165104988056252289, -1.599625672291271394 ) ) ;
#115314 = EDGE_CURVE ( 'NONE', #95577, #69400, #120111, .T. ) ;
#115315 = CARTESIAN_POINT ( 'NONE',  ( 6.684453402082996654, -1.835023323784425564, -0.3624468955198830722 ) ) ;
#115316 = B_SPLINE_CURVE_WITH_KNOTS ( 'NONE', 3,
 ( #107574, #77131, #193005, #190871, #42536, #108639 ),
 .UNSPECIFIED., .F., .F.,
 ( 4, 2, 4 ),
 ( 0.000000000000000000, 0.0003778774010236168619, 0.0007557548020472337237 ),
 .UNSPECIFIED. ) ;
#115318 = CARTESIAN_POINT ( 'NONE',  ( -5.302647476720585118, 9.200522799567075083, 0.000000000000000000 ) ) ;
#115317 = CARTESIAN_POINT ( 'NONE',  ( 4.746305163667582150, 0.9781546018433548983, -1.643150005489722787 ) ) ;
#115319 = CARTESIAN_POINT ( 'NONE',  ( 5.813141826352885566, 1.944573597739504889, 1.043518232037063287 ) ) ;
#115320 = CARTESIAN_POINT ( 'NONE',  ( -7.743115126736118015, 8.206258200713163475, 0.7216878364870317197 ) ) ;
#115321 = CARTESIAN_POINT ( 'NONE',  ( 7.014364370223726830, 9.276787413384745662, -1.599625672291269396 ) ) ;
#115322 = CARTESIAN_POINT ( 'NONE',  ( -4.136646265500970365, 5.919449624541475607, -1.443375672974066548 ) ) ;
#115323 = CARTESIAN_POINT ( 'NONE',  ( 0.02995210924121824436, -1.980234168275105455, 0.3962368897427023806 ) ) ;
#115324 = ORIENTED_EDGE ( 'NONE', *, *, #145607, .T. ) ;
#115325 = CARTESIAN_POINT ( 'NONE',  ( 4.507023749723728656, 1.786828103088284658, -1.460221407940938798 ) ) ;
#115326 = CARTESIAN_POINT ( 'NONE',  ( 5.055110333045015558, 1.632132345252810035, -1.088295032039228172 ) ) ;
#115327 = CARTESIAN_POINT ( 'NONE',  ( 2.360140415366944744, -1.961439503465340239, 0.04308618615556784187 ) ) ;
#115328 = CARTESIAN_POINT ( 'NONE',  ( 8.561083932025322696, 12.07534945641652158, -1.199719254218446718 ) ) ;
#115329 = CARTESIAN_POINT ( 'NONE',  ( -9.523390464710169923, 14.62238631451544713, 7.301111590532052276 ) ) ;
#115330 = VERTEX_POINT ( 'NONE', #37942 ) ;
#115331 = CARTESIAN_POINT ( 'NONE',  ( 0.04044418650436896329, 0.8167838292495681607, 1.953657075893009853 ) ) ;
#115333 = CARTESIAN_POINT ( 'NONE',  ( -9.345647958521597687, 9.797677461230342999, 0.7998128361456462443 ) ) ;
#115332 = CARTESIAN_POINT ( 'NONE',  ( -5.436983294280064882, 6.301900917203534291, 1.199719254218450271 ) ) ;
#115334 = CARTESIAN_POINT ( 'NONE',  ( 0.8492453639068753279, 1.839163117542693904, -0.08803940487626948919 ) ) ;
#115335 = VERTEX_POINT ( 'NONE', #166881 ) ;
#115336 = CARTESIAN_POINT ( 'NONE',  ( 4.698188964201695406, 0.9341788774818636787, -1.959971951513925781 ) ) ;
#115337 = CARTESIAN_POINT ( 'NONE',  ( -0.4592128676388293473, 2.866047475813795486, 1.947548603248408616 ) ) ;
#115338 = CARTESIAN_POINT ( 'NONE',  ( 2.215225606797793567, 1.700350911433265555, -1.266953333846132512 ) ) ;
#115339 = CARTESIAN_POINT ( 'NONE',  ( 1.499999999999990896, 3.306250000682818602, 1.214306433183764966E-14 ) ) ;
#115340 = CARTESIAN_POINT ( 'NONE',  ( 9.088043039861931405, 9.497138389460751284, 1.040834085586084257E-14 ) ) ;
#115341 = CARTESIAN_POINT ( 'NONE',  ( 6.270956187569860063, 6.991113019333711875, 0.9580997929081371822 ) ) ;
#115342 = CARTESIAN_POINT ( 'NONE',  ( 1.581398767000765426, 1.905217558097069386, -0.7859657096468860571 ) ) ;
#115343 = AXIS2_PLACEMENT_3D ( 'NONE', #168336, #154221, #68672 ) ;
#115345 = CARTESIAN_POINT ( 'NONE',  ( 8.744138462177931004, 13.53963283848627697, -8.151542665958993794 ) ) ;
#115344 = CARTESIAN_POINT ( 'NONE',  ( -9.664264568442742842, 10.16939683947169115, -0.7998128361456291469 ) ) ;
#115346 = CARTESIAN_POINT ( 'NONE',  ( -1.364683531249997417, 3.509375000341423245, 1.214306433183764966E-14 ) ) ;
#115347 = CARTESIAN_POINT ( 'NONE',  ( 0.07775346131142636674, 2.855377671833533970, -2.776861204146412021 ) ) ;
#115348 = CARTESIAN_POINT ( 'NONE',  ( 5.574911853349990842, 7.504993371562844295, -1.384166627116256709 ) ) ;
#115349 = CARTESIAN_POINT ( 'NONE',  ( 5.408822929737922003, -0.4686924282312036061, -1.853821656156897868 ) ) ;
#115350 = CARTESIAN_POINT ( 'NONE',  ( 11.88156762547253997, 12.22000008454031672, -1.686557021358706443 ) ) ;
#115351 = CARTESIAN_POINT ( 'NONE',  ( 1.968429645022830465, 1.162096202078844120, 1.940986467279571359 ) ) ;
#115352 = CARTESIAN_POINT ( 'NONE',  ( -9.408995418203979000, 12.00024729270324286, 1.443375672974076540 ) ) ;
#115353 = CARTESIAN_POINT ( 'NONE',  ( 1.617148605665112537, 1.507408818846365017, 1.004416837792695194 ) ) ;
#115354 = CARTESIAN_POINT ( 'NONE',  ( 1.938566325679047297, -1.478098309594473525, 1.218629399928832013 ) ) ;
#115355 = CARTESIAN_POINT ( 'NONE',  ( 2.559107912120599071, 1.664280205102614429, -1.231313097332722872 ) ) ;
#115356 = CARTESIAN_POINT ( 'NONE',  ( -1.364683531250000748, 2.071875000341422357, 1.214306433183764966E-14 ) ) ;
#115357 = CARTESIAN_POINT ( 'NONE',  ( 1.094530253197498526, -0.4767503703589200392, -1.912843428949811075 ) ) ;
#115358 = CARTESIAN_POINT ( 'NONE',  ( 5.602155610709171896, -1.926676517935271171, 0.002254597750208849581 ) ) ;
#115360 = CARTESIAN_POINT ( 'NONE',  ( 6.403672513108120690, 6.804938187689173468, -0.5019199613840990004 ) ) ;
#115359 = CARTESIAN_POINT ( 'NONE',  ( 1.208152727780729130, -0.5562822606778123902, 2.239534654701015981 ) ) ;
#115361 = CARTESIAN_POINT ( 'NONE',  ( -1.364683531250000748, 1.509375000341421691, 0.000000000000000000 ) ) ;
#115362 = CARTESIAN_POINT ( 'NONE',  ( 5.758276963478038191, -2.062851381910678850, -0.003602753815758196875 ) ) ;
#115363 = CIRCLE ( 'NONE', #143013, 11.09999999999999964 ) ;
#115364 =( BOUNDED_SURFACE ( )  B_SPLINE_SURFACE ( 3, 2, ( 
 ( #57316, #207812, #108267 ),
 ( #191557, #174288, #11743 ),
 ( #160146, #23733, #155887 ),
 ( #26928, #25863, #61573 ),
 ( #24797, #59440, #141809 ),
 ( #58381, #123480, #205679 ),
 ( #159078, #107193, #156962 ),
 ( #192624, #109338, #125597 ) ),
 .UNSPECIFIED., .F., .F., .T. ) 
 B_SPLINE_SURFACE_WITH_KNOTS ( ( 4, 2, 2, 4 ),
 ( 3, 3 ),
 ( 0.000000000000000000, 0.0002575597274893397974, 0.0005151194549786795949, 0.001030238909957359190 ),
 ( 0.000000000000000000, 1.000000000000000000 ),
 .UNSPECIFIED. ) 
 GEOMETRIC_REPRESENTATION_ITEM ( )  RATIONAL_B_SPLINE_SURFACE ( (
 ( 1.000000000000000000, 0.9238795325112786339, 1.000000000000000000),
 ( 1.000000000000000000, 0.9228594682463818755, 1.000000000000000000),
 ( 1.000000000000000000, 0.9150875845227504080, 1.000000000000000000),
 ( 1.000000000000000000, 0.8905471774192377232, 1.000000000000000000),
 ( 1.000000000000000000, 0.8740340839248615934, 1.000000000000000000),
 ( 1.000000000000000000, 0.8160099319846065846, 1.000000000000000000),
 ( 1.000000000000000000, 0.7673743911479209423, 1.000000000000000000),
 ( 1.000000000000000000, 0.7100530722070742540, 1.000000000000000000) ) ) 
 REPRESENTATION_ITEM ( '' )  SURFACE ( )  );
#115366 = CARTESIAN_POINT ( 'NONE',  ( -5.494078562035765501, 7.432844293840273231, -1.599625672291256295 ) ) ;
#115365 = AXIS2_PLACEMENT_3D ( 'NONE', #168513, #114512, #180508 ) ;
#115367 = CARTESIAN_POINT ( 'NONE',  ( 3.571683402196252910, 6.254382171615883834, 1.199719254218462483 ) ) ;
#115369 = CARTESIAN_POINT ( 'NONE',  ( 1.499999999999989120, 5.295833333333356485, -0.8660254037844323793 ) ) ;
#115368 = CARTESIAN_POINT ( 'NONE',  ( 0.04767123857605212733, -1.629476508726154016, -1.334019646271035198 ) ) ;
#115370 = CARTESIAN_POINT ( 'NONE',  ( -1.364683531249997417, 3.071875000341423245, 1.214306433183764966E-14 ) ) ;
#115371 = CARTESIAN_POINT ( 'NONE',  ( 4.973979902034267653, 1.240098594129716458, 1.770319513135506062 ) ) ;
#115372 = CARTESIAN_POINT ( 'NONE',  ( 5.444012513273879250, -1.283034597847107161, -1.559753263307301463 ) ) ;
#115373 = CARTESIAN_POINT ( 'NONE',  ( -0.6823417656250246877, -1.198958332991911790, 1.181850606188755259 ) ) ;
#115374 = CARTESIAN_POINT ( 'NONE',  ( -5.938108093105513241, 6.030140318152288792, 0.7216878364870317197 ) ) ;
#115377 = CARTESIAN_POINT ( 'NONE',  ( 3.375617060122621194, 6.882044303544283537, 1.040834085586084257E-14 ) ) ;
#115376 = CARTESIAN_POINT ( 'NONE',  ( 1.642778471875001811, -1.042708332855375009, 2.845375778867859751 ) ) ;
#115375 = CARTESIAN_POINT ( 'NONE',  ( 6.851666526859736983, 9.086973262793417661, -1.599625672291269396 ) ) ;
#115378 = CARTESIAN_POINT ( 'NONE',  ( -4.145761110728687804, 8.058748072483927771, -0.7998128361456481317 ) ) ;
#115379 = CARTESIAN_POINT ( 'NONE',  ( 3.696500153570709379, 1.422608671726926177, -1.429447704489300364 ) ) ;
#115380 = CARTESIAN_POINT ( 'NONE',  ( -8.552495972122143186, 8.872333477097637200, 0.7998128361456462443 ) ) ;
#115382 = SURFACE_SIDE_STYLE ('',( #98026 ) ) ;
#115381 = CARTESIAN_POINT ( 'NONE',  ( -4.776550190716183586, 4.467063398790632966, 1.214306433183764966E-14 ) ) ;
#115383 = CARTESIAN_POINT ( 'NONE',  ( -1.364683531250012516, 4.738541667008091096, -0.7879004041258300672 ) ) ;
#115385 = CARTESIAN_POINT ( 'NONE',  ( -1.402160292154681736E-14, 9.171875000341398021, 1.575800808251682339 ) ) ;
#115384 = CARTESIAN_POINT ( 'NONE',  ( 5.243122039519461097, -1.856066598825537373, 1.107904190987746063 ) ) ;
#115386 = FACE_OUTER_BOUND ( 'NONE', #123666, .T. ) ;
#115387 = CARTESIAN_POINT ( 'NONE',  ( -11.57172163803348575, 7.019044685052739929, -3.185222216268118522 ) ) ;
#115389 = CARTESIAN_POINT ( 'NONE',  ( 5.466422796518627614, -1.967893101392578448, -0.4390109167287381542 ) ) ;
#115388 = CARTESIAN_POINT ( 'NONE',  ( -7.226132685959434809, 8.493204890783200511, 1.082531754730549967 ) ) ;
#115390 = CARTESIAN_POINT ( 'NONE',  ( -1.402160292154681736E-14, 0.009375000341421267647, -1.575800808251665908 ) ) ;
#115391 = AXIS2_PLACEMENT_3D ( 'NONE', #140242, #206263, #9140 ) ;
#115392 = CARTESIAN_POINT ( 'NONE',  ( 0.4512176508754310866, 0.5462255407458499468, -1.636193974722987221 ) ) ;
#115393 = CARTESIAN_POINT ( 'NONE',  ( 5.086243903782109221, 5.962981304947771122, -1.199719254218452047 ) ) ;
#115395 = CARTESIAN_POINT ( 'NONE',  ( 7.693325821111733021, 7.940244644243982464, -0.7998128361456341429 ) ) ;
#115394 = CARTESIAN_POINT ( 'NONE',  ( 7.375272376154084597, 9.627570410311676596, -1.443375672974057666 ) ) ;
#115396 = CARTESIAN_POINT ( 'NONE',  ( -12.00000795471044945, 9.073126563016209900, 0.3090979129135709158 ) ) ;
#115397 = CARTESIAN_POINT ( 'NONE',  ( 6.608674649642057197, 1.385883050205028333, -1.256505298338560062 ) ) ;
#115398 = CARTESIAN_POINT ( 'NONE',  ( 0.4166524477783914437, -0.6801522605285510448, -1.894826352922045487 ) ) ;
#115399 = DIRECTION ( 'NONE',  ( 0.000000000000000000, 0.000000000000000000, 1.000000000000000000 ) ) ;
#115400 = CARTESIAN_POINT ( 'NONE',  ( 3.329339556154627289, 0.05228039400686017302, 2.206313527657398854 ) ) ;
#115401 = CARTESIAN_POINT ( 'NONE',  ( -7.092323753280154186, 7.447001598347859463, 0.7216878364870317197 ) ) ;
#115402 = ORIENTED_EDGE ( 'NONE', *, *, #177464, .F. ) ;
#115403 = CARTESIAN_POINT ( 'NONE',  ( 8.229436053370667636, 11.58446391469906267, 1.082531754730558626 ) ) ;
#115405 = CARTESIAN_POINT ( 'NONE',  ( 1.581657880887325174, -0.6766953518495041342, 1.899626397962331126 ) ) ;
#115404 = CARTESIAN_POINT ( 'NONE',  ( 1.928540351845555056, -1.002238520345886785, -1.868699319572619366 ) ) ;
#115406 = CARTESIAN_POINT ( 'NONE',  ( 2.513665319321151337, -0.5648568745635518251, 1.721363734954905356 ) ) ;
#115407 = CARTESIAN_POINT ( 'NONE',  ( 5.989670002187236442, 10.20997511251894529, -0.7998128361456481317 ) ) ;
#115408 = EDGE_CURVE ( 'NONE', #63111, #93339, #143497, .T. ) ;
#115409 = CARTESIAN_POINT ( 'NONE',  ( 5.113396490648394632, 9.117379672398465473, 1.040834085586084257E-14 ) ) ;
#115411 = CARTESIAN_POINT ( 'NONE',  ( 0.4443725376216747236, -1.385435448976629180, 1.323305594895395343 ) ) ;
#115410 = CARTESIAN_POINT ( 'NONE',  ( -6.078132937628113908, 5.985576603521232109, 1.040834085586084257E-14 ) ) ;
#115412 = CARTESIAN_POINT ( 'NONE',  ( 1.848071122224584251, 8.944961669792201420, 0.7750000000000004663 ) ) ;
#115413 = CARTESIAN_POINT ( 'NONE',  ( -0.4000000000000322742, 4.000000000000017764, 0.9782388782688753448 ) ) ;
#115414 = CARTESIAN_POINT ( 'NONE',  ( 6.168596704093459060, 7.259412911939593371, -1.082531754730543083 ) ) ;
#115415 = CARTESIAN_POINT ( 'NONE',  ( 1.364683531249986537, 0.2177083336747502595, -0.7879004041258309554 ) ) ;
#115416 = DIRECTION ( 'NONE',  ( 0.000000000000000000, -1.000000000000000000, 0.000000000000000000 ) ) ;
#115417 = CARTESIAN_POINT ( 'NONE',  ( -9.972185678051314284, 11.59297036493672017, 1.199719254218462483 ) ) ;
#115418 = CARTESIAN_POINT ( 'NONE',  ( 4.223607183596161718, -2.069420184152844566, 0.6248923283326962563 ) ) ;
#115419 = CARTESIAN_POINT ( 'NONE',  ( -7.295696057929500711, 7.684269287105433222, 0.7216878364870317197 ) ) ;
#115420 = CARTESIAN_POINT ( 'NONE',  ( 4.258669648468278446, 7.022179452304728287, 1.082531754730549078 ) ) ;
#115421 = CARTESIAN_POINT ( 'NONE',  ( 2.232824136269210502, 1.381628265877183903, -1.608862310199298928 ) ) ;
#115422 = CYLINDRICAL_SURFACE ( 'NONE', #117581, 2.025000000000006573 ) ;
#115423 = CARTESIAN_POINT ( 'NONE',  ( 2.899638734157696796, -0.6216841358992927224, 1.870808799549168233 ) ) ;
#115424 = ORIENTED_EDGE ( 'NONE', *, *, #197258, .T. ) ;
#115425 = DIRECTION ( 'NONE',  ( 1.276756478318932585E-15, -1.000000000000000000, 1.665334536937738262E-16 ) ) ;
#115426 = CARTESIAN_POINT ( 'NONE',  ( 5.652785005015395825, -0.4769087673412530370, -1.910818445241519559 ) ) ;
#115427 = CARTESIAN_POINT ( 'NONE',  ( 1.482261173788253394, -0.2847754331270537231, -1.920845095517382362 ) ) ;
#115428 = ORIENTED_EDGE ( 'NONE', *, *, #101605, .T. ) ;
#115429 = CARTESIAN_POINT ( 'NONE',  ( -4.821859908315634158, 5.654533310236863564, 1.199719254218452935 ) ) ;
#115431 = CARTESIAN_POINT ( 'NONE',  ( -2.331034670843834533E-15, -6.705807707623487879, 10.34804402329814010 ) ) ;
#115430 = CARTESIAN_POINT ( 'NONE',  ( -7.132998214565509087, 7.494455136514109661, 0.7216878364870317197 ) ) ;
#115433 = CARTESIAN_POINT ( 'NONE',  ( 5.472687561410540802, 9.536552588287639409, 0.7998128361456462443 ) ) ;
#115432 = CARTESIAN_POINT ( 'NONE',  ( 2.941443032221033427, 0.7519493320215028254, -1.950910760374990671 ) ) ;
#115435 = CARTESIAN_POINT ( 'NONE',  ( 3.729901657090938460, 7.365652676665848553, 0.7216878364870257245 ) ) ;
#115434 = CARTESIAN_POINT ( 'NONE',  ( 6.109920781252839994, 10.27999134477033216, 1.040834085586084257E-14 ) ) ;
#115437 = EDGE_LOOP ( 'NONE', ( #204579, #138954, #202443, #165392 ) ) ;
#115436 = CARTESIAN_POINT ( 'NONE',  ( 6.129550632656369125, -0.2293275368827427663, 1.898405681093485953 ) ) ;
#115438 = CARTESIAN_POINT ( 'NONE',  ( 4.530015419921377351, -1.356323209173672106, -1.740806116466916187 ) ) ;
#115439 = CARTESIAN_POINT ( 'NONE',  ( 1.905583573826599597, 1.834846665736546756, 1.225745012653912891 ) ) ;
#115440 = FACE_OUTER_BOUND ( 'NONE', #47603, .T. ) ;
#115441 = CARTESIAN_POINT ( 'NONE',  ( 1.154776974461441341, 0.3738248154092556064, 1.875208037630435864 ) ) ;
#115442 = AXIS2_PLACEMENT_3D ( 'NONE', #103451, #20045, #22155 ) ;
#115443 = CARTESIAN_POINT ( 'NONE',  ( -4.848826244296223109, 5.027555131033083491, -0.8732430475888957044 ) ) ;
#115444 = CARTESIAN_POINT ( 'NONE',  ( 11.49978884755361008, 13.74270821162803990, -3.429452816445331731 ) ) ;
#115445 = CARTESIAN_POINT ( 'NONE',  ( 4.264170421968140445, -2.065031762457261610, 0.1491743435546449281 ) ) ;
#115446 = CARTESIAN_POINT ( 'NONE',  ( -5.250031796989778066, 7.148123067953287446, 1.599625672291267398 ) ) ;
#115447 = COLOUR_RGB ( '', 0.72549020, 0.75294118, 0.79215686) ;
#115449 = CARTESIAN_POINT ( 'NONE',  ( 2.202237438260604030, -2.161223104231101644, 0.05255616829508147347 ) ) ;
#115448 = CARTESIAN_POINT ( 'NONE',  ( -4.600294193738529103, 4.261431402316699035, -0.7998128361456221525 ) ) ;
#115450 = CARTESIAN_POINT ( 'NONE',  ( 3.157961424266928052, 0.9873743524775533409, 1.956624655947765357 ) ) ;
#115451 = CARTESIAN_POINT ( 'NONE',  ( -4.685165750215470659, 7.704147214923535714, 1.047329974316240753 ) ) ;
#115452 = CARTESIAN_POINT ( 'NONE',  ( 3.469446951953614189E-15, -6.938893903907228378E-15, -5.500000000000003553 ) ) ;
#115453 = CARTESIAN_POINT ( 'NONE',  ( 0.3525790917594442964, -6.713792789267425398, 9.484899655072640101 ) ) ;
#115454 = CARTESIAN_POINT ( 'NONE',  ( 1.364683531249996529, 15.02604166700806587, 0.7879004041258405033 ) ) ;
#115455 = CARTESIAN_POINT ( 'NONE',  ( -4.034433228518296666, 6.864533312316751790, -1.199719254218450271 ) ) ;
#115456 = PRODUCT_DEFINITION_CONTEXT ( 'detailed design', #60163, 'design' ) ;
#115457 = CARTESIAN_POINT ( 'NONE',  ( 0.1060925565549031974, -0.09613213100253051313, 2.014232862735332308 ) ) ;
#115458 = CARTESIAN_POINT ( 'NONE',  ( -8.663296969452339624, 13.05100419776235299, 1.040834085586084257E-14 ) ) ;
#115459 = CARTESIAN_POINT ( 'NONE',  ( 4.223533608758993196, 0.2584441732129874603, -2.054024224480345939 ) ) ;
#115460 = CARTESIAN_POINT ( 'NONE',  ( 5.800440434243619769, 1.421441630026821112, -1.569310636533404635 ) ) ;
#115461 = CARTESIAN_POINT ( 'NONE',  ( 4.638861114170084399, 8.563755066507100722, 0.7998128361456462443 ) ) ;
#115462 = CARTESIAN_POINT ( 'NONE',  ( 1.364683531249992088, 5.634375000341417916, 1.214306433183764966E-14 ) ) ;
#115463 = CARTESIAN_POINT ( 'NONE',  ( 4.487129304207951641, 0.09229547738082846675, 1.967383831439367903 ) ) ;
#115464 = CARTESIAN_POINT ( 'NONE',  ( 6.070342170859510667, -2.174803699615239783, -0.7246130948556377405 ) ) ;
#115465 = CARTESIAN_POINT ( 'NONE',  ( 2.701551412915685457, -0.5726843992823158480, 1.733614832724015731 ) ) ;
#115466 = CARTESIAN_POINT ( 'NONE',  ( 2.878073747850912412, 6.579779482459851003, -0.7998128361456362523 ) ) ;
#115467 = CARTESIAN_POINT ( 'NONE',  ( 4.433153041544209749, 7.155467067568137551, -1.082531754730548412 ) ) ;
#115468 = CARTESIAN_POINT ( 'NONE',  ( -5.859094939400033120, 9.987361195942037639, -0.7998128361456231517 ) ) ;
#115469 = CARTESIAN_POINT ( 'NONE',  ( 5.879395890181562834, 6.888325289080478697, -1.199719254218452047 ) ) ;
#115470 = ORIENTED_EDGE ( 'NONE', *, *, #51769, .F. ) ;
#115471 = CARTESIAN_POINT ( 'NONE',  ( 4.482685760555058074, -1.311686992106766203, 1.527362355471563182 ) ) ;
#115472 = CARTESIAN_POINT ( 'NONE',  ( 4.522284091987982535, 0.9210895807079204634, 1.732038000912524689 ) ) ;
#115473 = CARTESIAN_POINT ( 'NONE',  ( -6.287230548435221777, 8.358188277972981695, -1.599625672291263179 ) ) ;
#115474 = CARTESIAN_POINT ( 'NONE',  ( -5.111587607552082524, 5.922272616020886282, 1.199719254218450271 ) ) ;
#115475 = CARTESIAN_POINT ( 'NONE',  ( -10.00198841339046041, 1.970899860167807605, -6.221464951633984164 ) ) ;
#115476 = CARTESIAN_POINT ( 'NONE',  ( -5.906512197408906317, 6.919960980845699439, -1.199719254218453823 ) ) ;
#115478 = CARTESIAN_POINT ( 'NONE',  ( 6.034039731144309471, 0.8686908000094315518, -1.541921269980907949 ) ) ;
#115477 = CARTESIAN_POINT ( 'NONE',  ( 0.2047783418026409563, 1.821168281471240435, 1.026754182986739927 ) ) ;
#115479 = CARTESIAN_POINT ( 'NONE',  ( 10.99970480906932657, -5.741816521215535651, 0.08058606168009173343 ) ) ;
#115480 = CARTESIAN_POINT ( 'NONE',  ( 1.781448188194576066, 1.512826363221421833, 1.585725795389548942 ) ) ;
#115481 = CARTESIAN_POINT ( 'NONE',  ( 1.135833342500572440, 0.3383711564543417927, 1.707032442944929729 ) ) ;
#115482 = CARTESIAN_POINT ( 'NONE',  ( 6.823831386379729302, 6.855558127064808716, -0.7998128361456281477 ) ) ;
#115483 = CARTESIAN_POINT ( 'NONE',  ( 1.136830759877343722, -1.561040526032995590, 0.7340551814495520633 ) ) ;
#115484 = CARTESIAN_POINT ( 'NONE',  ( 1.101424459656743071, -0.5276332240332289869, 2.126988402630063835 ) ) ;
#115485 = CARTESIAN_POINT ( 'NONE',  ( 2.666872310945223923, -1.521158656661812714, 1.599105504226288499 ) ) ;
#115486 = CARTESIAN_POINT ( 'NONE',  ( 0.9718041211803396529, -0.3205511010368928271, 2.147183668106082521 ) ) ;
#115487 = DIRECTION ( 'NONE',  ( 1.000000000000000000, 0.000000000000000000, 0.000000000000000000 ) ) ;
#115488 = CARTESIAN_POINT ( 'NONE',  ( 1.991562931776114542, -0.4585136385713373675, 2.066967827372573563 ) ) ;
#115489 = CARTESIAN_POINT ( 'NONE',  ( 6.827182134110157286, 6.032625672350935275, 2.883942191975923830 ) ) ;
#115490 = ORIENTED_EDGE ( 'NONE', *, *, #212409, .F. ) ;
#115492 = CARTESIAN_POINT ( 'NONE',  ( -1.364683531250000748, -0.1781249996585798634, 0.000000000000000000 ) ) ;
#115491 = CARTESIAN_POINT ( 'NONE',  ( 2.419810632640221115, -1.322813552229468614, -1.872022261021451639 ) ) ;
#115493 = CARTESIAN_POINT ( 'NONE',  ( 2.737856954955798727, 5.281584649835344258, 1.199719254218452047 ) ) ;
#115494 = CARTESIAN_POINT ( 'NONE',  ( 5.464099601507359516, 6.333536608968757697, 1.199719254218462483 ) ) ;
#115495 = CARTESIAN_POINT ( 'NONE',  ( 4.969482899335432968, -1.875980303166164376, -1.189202907730102732 ) ) ;
#115496 = CARTESIAN_POINT ( 'NONE',  ( -7.049876689426103127, 10.20831132343037062, -1.082531754730537976 ) ) ;
#115497 = CARTESIAN_POINT ( 'NONE',  ( -4.951116456853996262, 6.538279688806403200, -2.442614223628299719 ) ) ;
#115498 = CARTESIAN_POINT ( 'NONE',  ( 4.012850279964918165, 7.625483060026979842, -0.7216878364870197293 ) ) ;
#115499 = CARTESIAN_POINT ( 'NONE',  ( -6.019457014343129408, 9.966524250134902729, 0.000000000000000000 ) ) ;
#115500 =( GEOMETRIC_REPRESENTATION_CONTEXT ( 3 ) GLOBAL_UNCERTAINTY_ASSIGNED_CONTEXT ( ( #66174 ) ) GLOBAL_UNIT_ASSIGNED_CONTEXT ( ( #132509, #120562, #70633 ) ) REPRESENTATION_CONTEXT ( 'NONE', 'WORKASPACE' ) );
#115501 = CARTESIAN_POINT ( 'NONE',  ( 3.879041347285658414, 6.579279767591636130, -1.082531754730548412 ) ) ;
#115502 = VERTEX_POINT ( 'NONE', #3274 ) ;
#115503 = CARTESIAN_POINT ( 'NONE',  ( 3.340470361411255418, 0.4872029778183216697, -1.956561305313428978 ) ) ;
#115505 = CARTESIAN_POINT ( 'NONE',  ( 1.516546868092843781, 0.8322427235708649285, 1.887369835301610621 ) ) ;
#115504 = CARTESIAN_POINT ( 'NONE',  ( 7.263417608619159083, 9.497073181520933716, -1.599625672291262513 ) ) ;
#115506 = CARTESIAN_POINT ( 'NONE',  ( 11.89942855770814312, 11.37999999999999901, 0.6999999999999992895 ) ) ;
#115507 = CARTESIAN_POINT ( 'NONE',  ( 5.356880090730863131, 7.343055753976412525, 1.443375672974064550 ) ) ;
#115508 = AXIS2_PLACEMENT_3D ( 'NONE', #109507, #192794, #77994 ) ;
#115509 = CARTESIAN_POINT ( 'NONE',  ( 0.7500000000000006661, 8.614583334016129967, 1.299038105676657340 ) ) ;
#115510 = CARTESIAN_POINT ( 'NONE',  ( 0.6823417656249899377, 4.176041667008085767, -1.181850606188754593 ) ) ;
#115511 = CARTESIAN_POINT ( 'NONE',  ( 3.961010909407122860, 0.2689195440248594027, -2.174814543647784593 ) ) ;
#115512 = CARTESIAN_POINT ( 'NONE',  ( 1.195935645703485539, 1.779627574718087635, 0.9480385367472210500 ) ) ;
#115513 = CARTESIAN_POINT ( 'NONE',  ( 0.8371598888798935656, 0.7463826720714299423, -1.683355135116317847 ) ) ;
#115514 = CARTESIAN_POINT ( 'NONE',  ( 8.457588896826466751, 8.761608555919362828, 1.040834085586084257E-14 ) ) ;
#115515 = CARTESIAN_POINT ( 'NONE',  ( 5.596661130663158623, -0.4455768995972574364, -1.770251349769519367 ) ) ;
#115516 = CARTESIAN_POINT ( 'NONE',  ( 5.643203987388664800, 0.8197706014990979728, 1.842448445624145226 ) ) ;
#115517 = CARTESIAN_POINT ( 'NONE',  ( -7.641992139597101108, 12.06740792950531649, 0.7998128361456481317 ) ) ;
#115519 = CARTESIAN_POINT ( 'NONE',  ( -4.633854640820660009, 8.628190524257904670, -0.7998128361456362523 ) ) ;
#115518 = CARTESIAN_POINT ( 'NONE',  ( 4.821284755203490313, -0.1158696699916968720, 2.259674544810440278 ) ) ;
#115520 = CARTESIAN_POINT ( 'NONE',  ( 0.7156196601619690956, -0.3068708111382661974, 2.083463767009658962 ) ) ;
#115521 = CARTESIAN_POINT ( 'NONE',  ( -5.749539660647037032, 8.865490816466966351, 1.199719254218454489 ) ) ;
#115522 = CARTESIAN_POINT ( 'NONE',  ( 4.316890830952234914, -1.536253448065309613, 1.388129241271539138 ) ) ;
#115523 = CARTESIAN_POINT ( 'NONE',  ( 8.378048858240820351, 11.86180853700128601, -1.199719254218446718 ) ) ;
#115524 = CARTESIAN_POINT ( 'NONE',  ( -3.755786496842897795E-14, 2.609375000341406459, -1.570758158831778273 ) ) ;
#115525 = SHAPE_DEFINITION_REPRESENTATION ( #126764, #47273 ) ;
#115527 = EDGE_CURVE ( 'NONE', #91287, #85555, #86670, .T. ) ;
#115526 = CARTESIAN_POINT ( 'NONE',  ( -7.395082721250053837, 10.71501471051202614, -1.199719254218446718 ) ) ;
#115528 =( NAMED_UNIT ( * ) PLANE_ANGLE_UNIT ( ) SI_UNIT ( $, .RADIAN. ) );
#115529 = CARTESIAN_POINT ( 'NONE',  ( 7.550965208168244125, 7.774157262476569130, -0.7998128361456341429 ) ) ;
#115530 = CARTESIAN_POINT ( 'NONE',  ( 4.433499500630886381, 7.080826916883525612, -1.109343814354251112 ) ) ;
#115531 = CARTESIAN_POINT ( 'NONE',  ( -2.578021764892882040, 6.159442492350315490, 0.7998128361456341429 ) ) ;
#115533 = CARTESIAN_POINT ( 'NONE',  ( 1.441950287000768771, -2.089521377041357653, 0.7543469697938051111 ) ) ;
#115532 = CARTESIAN_POINT ( 'NONE',  ( 0.2465380642357860586, 1.084720387836759725, -1.822023332652397354 ) ) ;
#115534 = CARTESIAN_POINT ( 'NONE',  ( -3.410126044457033156, -0.03745499569612897872, 0.000000000000000000 ) ) ;
#115535 = CARTESIAN_POINT ( 'NONE',  ( -6.343235766347277149, 8.493804042195527870, -1.599625672291271394 ) ) ;
#115536 = CARTESIAN_POINT ( 'NONE',  ( 4.788000803920411386, 8.737751371215816576, 1.040834085586084257E-14 ) ) ;
#115537 = CARTESIAN_POINT ( 'NONE',  ( 3.402741375674179114, 0.4741672551989496998, 1.903589013717405853 ) ) ;
#115538 = CARTESIAN_POINT ( 'NONE',  ( 6.634017235788401301, 6.634108284708264414, 0.7998128361456341429 ) ) ;
#115539 = CARTESIAN_POINT ( 'NONE',  ( -4.014242769884851292, 7.626870978312306981, -0.02218799730280621163 ) ) ;
#115540 = CARTESIAN_POINT ( 'NONE',  ( 3.225950485047770933, 5.851027101609320269, 1.199719254218450271 ) ) ;
#115541 = CARTESIAN_POINT ( 'NONE',  ( -5.858531774880906262, 6.967946837850073294, 1.082531754730549078 ) ) ;
#115542 = CARTESIAN_POINT ( 'NONE',  ( -6.995644074971465010, 10.14503993989993091, 1.082531754730549967 ) ) ;
#115543 = CARTESIAN_POINT ( 'NONE',  ( 2.303126745213024851, -0.3670769733005623814, -2.088442229865586697 ) ) ;
#115544 = CARTESIAN_POINT ( 'NONE',  ( -5.101610940492132151, 9.173906207207963348, -0.7998128361456362523 ) ) ;
#115545 = CARTESIAN_POINT ( 'NONE',  ( 3.947668504265917644, 1.419370528949075005, 1.354593381527373186 ) ) ;
#115546 = CARTESIAN_POINT ( 'NONE',  ( 3.696290335837215668, -2.159122111672501454, -0.1082323872379290647 ) ) ;
#115547 = CARTESIAN_POINT ( 'NONE',  ( 3.157574601152390414, 0.8305207305269333151, 1.643389852989694200 ) ) ;
#115548 = CARTESIAN_POINT ( 'NONE',  ( -4.015022313999534909, 7.625723350685065682, -0.07359193599470841007 ) ) ;
#115549 = CARTESIAN_POINT ( 'NONE',  ( 1.364683531249986537, -0.7822916663252464931, -0.7879004041258309554 ) ) ;
#115550 = CARTESIAN_POINT ( 'NONE',  ( 5.120954501598782294, -1.650910780824323298, 0.5508982476954398244 ) ) ;
#115551 = CARTESIAN_POINT ( 'NONE',  ( 1.050790385994986975, 15.00000000000000711, -12.64745918785790835 ) ) ;
#115552 = CARTESIAN_POINT ( 'NONE',  ( 3.551873057100274789, 7.087676300018221021, 0.7216878364870298324 ) ) ;
#115553 = CARTESIAN_POINT ( 'NONE',  ( 6.620655732516647518, 0.007553340620044743381, 1.826407896915738238 ) ) ;
#115554 = CARTESIAN_POINT ( 'NONE',  ( 1.745224485312408813, -1.826185749030174499, 1.156423465944363294 ) ) ;
#115555 = CARTESIAN_POINT ( 'NONE',  ( 4.323592178502837058, -1.495822217463145476, 1.351947993609707632 ) ) ;
#115556 = CARTESIAN_POINT ( 'NONE',  ( -8.636180661780660017, 11.09863007687603087, -1.443375672974058777 ) ) ;
#115557 = CARTESIAN_POINT ( 'NONE',  ( 1.516726440323381331, 1.451591637995581996, -1.601975981646540426 ) ) ;
#115558 = EDGE_CURVE ( 'NONE', #186548, #95626, #1459, .T. ) ;
#115559 = CARTESIAN_POINT ( 'NONE',  ( 2.249238725404782091, -1.581088017263340806, -1.177247449022495118 ) ) ;
#115560 = CARTESIAN_POINT ( 'NONE',  ( 6.509000000000010111, 6.037005099786168394, 2.594901386363585694 ) ) ;
#115561 = CARTESIAN_POINT ( 'NONE',  ( 3.561997098397641448, -1.302002156301942604, 1.441148521680717387 ) ) ;
#115564 = ORIENTED_EDGE ( 'NONE', *, *, #180702, .F. ) ;
#115563 = CARTESIAN_POINT ( 'NONE',  ( -4.841670253855968831, 4.821239182352949904, 0.000000000000000000 ) ) ;
#115562 = DIRECTION ( 'NONE',  ( 8.638326563840814399E-31, -0.000000000000000000, 1.000000000000000000 ) ) ;
#115565 = CARTESIAN_POINT ( 'NONE',  ( -6.688968683495758683, 8.897159112202094988, -1.599625672291271394 ) ) ;
#115566 = CARTESIAN_POINT ( 'NONE',  ( 5.032011289327418702, 5.899709921417326974, 1.199719254218452935 ) ) ;
#115567 = CARTESIAN_POINT ( 'NONE',  ( -6.317173229324657413, 6.334733287159020954, 0.000000000000000000 ) ) ;
#115568 = CARTESIAN_POINT ( 'NONE',  ( -9.775065565328612038, 10.50659070241261794, -0.7216878364870267237 ) ) ;
#115569 = CARTESIAN_POINT ( 'NONE',  ( 1.149787729276055437, -1.740433383357189223, -1.356609624190791008 ) ) ;
#115570 = CARTESIAN_POINT ( 'NONE',  ( -1.642778471875000035, -4.017708332855376874, -2.845375778867859751 ) ) ;
#115571 = CARTESIAN_POINT ( 'NONE',  ( 5.190269257085567745, 1.011813749630154691, -1.680575076195559792 ) ) ;
#115572 = ORIENTED_EDGE ( 'NONE', *, *, #183072, .T. ) ;
#115573 = CARTESIAN_POINT ( 'NONE',  ( 3.362624215892480173, -2.041811681064845896, -0.5603701389207839112 ) ) ;
#115574 = CARTESIAN_POINT ( 'NONE',  ( -1.500000000000013101, 2.410416667349482456, -0.8660254037844313801 ) ) ;
#115575 = CARTESIAN_POINT ( 'NONE',  ( 0.1747926744264452492, 5.725295659261265158, -2.449351454080525681 ) ) ;
#115576 = CARTESIAN_POINT ( 'NONE',  ( 4.136529068399773301, -1.600833271991594309, 0.9093273525555560788 ) ) ;
#115577 = ORIENTED_EDGE ( 'NONE', *, *, #124727, .T. ) ;
#115578 = APPLICATION_CONTEXT ( 'automotive_design' ) ;
#115579 = UNCERTAINTY_MEASURE_WITH_UNIT (LENGTH_MEASURE( 1.000000000000000082E-05 ), #162627, 'distance_accuracy_value', 'NONE');
#115580 = CARTESIAN_POINT ( 'NONE',  ( -8.995998617867369873, 10.45408546138876993, 1.199719254218462483 ) ) ;
#115581 = CARTESIAN_POINT ( 'NONE',  ( 2.020417662918754687, 3.956598013261175772, -11.36521191596581737 ) ) ;
#115582 = CARTESIAN_POINT ( 'NONE',  ( 5.220985865760717992, 1.604251394084664550, -1.386888226476624242 ) ) ;
#115583 = CARTESIAN_POINT ( 'NONE',  ( -0.1104750535120025967, -0.004616138082884357029, -2.103378236956429337 ) ) ;
#115584 = CARTESIAN_POINT ( 'NONE',  ( 4.449046963578762615, 8.342305224150557308, -0.7998128361456231517 ) ) ;
#115585 = CARTESIAN_POINT ( 'NONE',  ( 5.413377607122367152, -0.3064755606005803434, 2.037752308911133348 ) ) ;
#115588 = CARTESIAN_POINT ( 'NONE',  ( 4.106863108761789505, -0.3106082297497716471, 1.814695527881895476 ) ) ;
#115587 = CARTESIAN_POINT ( 'NONE',  ( 1.187708300173949461, -1.176858333569561932, -1.441725857702576219 ) ) ;
#115586 = DIRECTION ( 'NONE',  ( -1.000000000000000000, 0.000000000000000000, 0.000000000000000000 ) ) ;
#115589 = CARTESIAN_POINT ( 'NONE',  ( 8.229962938695207342, 9.560377169021284871, 1.199719254218462483 ) ) ;
#115590 = CARTESIAN_POINT ( 'NONE',  ( 8.966186108929086629, 2.441452740530747345, 7.552575952455595321 ) ) ;
#115591 = CARTESIAN_POINT ( 'NONE',  ( 0.4735722981416969346, 7.464727232010901048, 4.424040350390570531 ) ) ;
#115593 = ORIENTED_EDGE ( 'NONE', *, *, #167712, .F. ) ;
#115592 = FACE_OUTER_BOUND ( 'NONE', #143215, .T. ) ;
#115594 = CARTESIAN_POINT ( 'NONE',  ( 3.686314334879085663, -1.088174899301070253, 1.919869060924610293 ) ) ;
#115595 = CARTESIAN_POINT ( 'NONE',  ( 4.394006599171666139, -0.8711832027283890056, 2.088141772348524050 ) ) ;
#115596 = CARTESIAN_POINT ( 'NONE',  ( -6.724481002698126098, 8.868313807946373473, -1.443375672974059665 ) ) ;
#115597 = CARTESIAN_POINT ( 'NONE',  ( 4.464998409566146798, -1.450835031669978292, 1.084616504919968305 ) ) ;
#115598 = CARTESIAN_POINT ( 'NONE',  ( 5.366386423658583205, -1.870495304593930097, -0.4130858509987145877 ) ) ;
#115599 = CARTESIAN_POINT ( 'NONE',  ( 6.727182134110222478, 0.005875948494733079785, 1.810970247402940547 ) ) ;
#115600 = CARTESIAN_POINT ( 'NONE',  ( 5.190257414508706368, -1.856628772771324210, -0.2281712211116558864 ) ) ;
#115601 = CARTESIAN_POINT ( 'NONE',  ( 5.934019871859393724, 1.109147300373466871, 1.494279092885692606 ) ) ;
#115602 = CARTESIAN_POINT ( 'NONE',  ( -1.500000000000008216, 12.99999999999999822, 3.469446951953614189E-15 ) ) ;
#115604 = AXIS2_PLACEMENT_3D ( 'NONE', #156031, #38016, #169072 ) ;
#115603 = CARTESIAN_POINT ( 'NONE',  ( 6.051566426668148146, 0.5099629880620482059, -1.694758430261036564 ) ) ;
#115605 = CARTESIAN_POINT ( 'NONE',  ( 0.2863426850727782136, -0.6839425765656822476, -1.897108587135355684 ) ) ;
#115607 = CARTESIAN_POINT ( 'NONE',  ( 2.737057789242686390, 0.2582918889518608374, 2.090101187703028884 ) ) ;
#115606 = CARTESIAN_POINT ( 'NONE',  ( -3.267151830768952880, 5.795132321663641228, -1.082531754730549078 ) ) ;
#115608 = CARTESIAN_POINT ( 'NONE',  ( 8.615316546479974136, 12.13862083994696839, 1.199719254218450271 ) ) ;
#115610 = CARTESIAN_POINT ( 'NONE',  ( -9.775592450653132204, 11.36361159963886891, -1.199719254218441611 ) ) ;
#115609 = CARTESIAN_POINT ( 'NONE',  ( -8.673617379884035472E-15, 3.975067388631681187, -1.561251128379126385E-14 ) ) ;
#115611 = CYLINDRICAL_SURFACE ( 'NONE', #23650, 0.08000000000000041800 ) ;
#115612 = CARTESIAN_POINT ( 'NONE',  ( 1.775654988352931563, 0.3410282263864356511, -1.990609417402624537 ) ) ;
#115613 = CARTESIAN_POINT ( 'NONE',  ( -1.364683531250012516, 2.738541667008090208, -0.7879004041258289570 ) ) ;
#115614 = CARTESIAN_POINT ( 'NONE',  ( 3.310162060030825248, 7.013606170011280838, -0.7998128361456291469 ) ) ;
#115615 = CARTESIAN_POINT ( 'NONE',  ( 3.356853517036356038, -1.639235867460669072, 1.409173823127254366 ) ) ;
#115616 = CARTESIAN_POINT ( 'NONE',  ( 6.889999999999965041, 7.051532193125384040, 2.878152852197481071 ) ) ;
#115618 = CYLINDRICAL_SURFACE ( 'NONE', #145333, 0.08000000000000012657 ) ;
#115617 = CARTESIAN_POINT ( 'NONE',  ( 3.386504508363381571, 7.172948703057747011, -0.7998128361456362523 ) ) ;
#115619 = CARTESIAN_POINT ( 'NONE',  ( 10.37162432432990755, 11.20257592124748136, -0.7216878364870257245 ) ) ;
#115620 = CARTESIAN_POINT ( 'NONE',  ( 0.000000000000000000, 3.900000000000000799, 0.000000000000000000 ) ) ;
#115621 = CARTESIAN_POINT ( 'NONE',  ( -5.883875478650828050, 9.808345791827219884, 0.7216878364870458196 ) ) ;
#115622 = CARTESIAN_POINT ( 'NONE',  ( -0.6823417656250212460, 1.301041667008083547, 1.181850606188755259 ) ) ;
#115623 = CARTESIAN_POINT ( 'NONE',  ( 0.9080814035550346386, -0.9900877184637231210, -1.955254813705724404 ) ) ;
#115624 = CARTESIAN_POINT ( 'NONE',  ( -1.975475456537005874E-15, 2.812500000000000888, 1.224999999999953904 ) ) ;
#115625 = CARTESIAN_POINT ( 'NONE',  ( 1.798126127191189472, -0.7612548243747189192, 2.130717213291497547 ) ) ;
#115626 = CARTESIAN_POINT ( 'NONE',  ( -6.832419346282942563, 10.05857410638369487, 1.199719254218453823 ) ) ;
#115627 = CARTESIAN_POINT ( 'NONE',  ( -5.558479791478509568, 5.587240632920778438, 0.000000000000000000 ) ) ;
#115628 = CARTESIAN_POINT ( 'NONE',  ( 1.364683531249988535, 3.217708333674748289, -0.7879004041258239610 ) ) ;
#115629 = CARTESIAN_POINT ( 'NONE',  ( 4.784634885068531851, 8.146353749921887655, 0.8039021629790907841 ) ) ;
#115630 = CARTESIAN_POINT ( 'NONE',  ( 0.7500000000000006661, 11.16666666666666430, -1.299038105676657340 ) ) ;
#115631 = CARTESIAN_POINT ( 'NONE',  ( 4.913904330310220558, 4.697586238308844919, 0.000000000000000000 ) ) ;
#115632 = CARTESIAN_POINT ( 'NONE',  ( 3.215802288110910290, -0.8691132097216300867, -1.541513200001721540 ) ) ;
#115633 = CARTESIAN_POINT ( 'NONE',  ( 6.071336392737415544, 0.1682094380959769098, -2.200428349287026908 ) ) ;
#115634 = CARTESIAN_POINT ( 'NONE',  ( -1.402160292154681736E-14, 8.421875000341403350, 1.575800808251682339 ) ) ;
#115635 = ORIENTED_EDGE ( 'NONE', *, *, #169884, .T. ) ;
#115636 = CARTESIAN_POINT ( 'NONE',  ( -5.098748287191073203, 8.106234214101666780, 1.199719254218452935 ) ) ;
#115637 = CARTESIAN_POINT ( 'NONE',  ( 4.763296089436113157, 1.880429982106451181, -0.7283946704290320540 ) ) ;
#115638 = ORIENTED_EDGE ( 'NONE', *, *, #6898, .F. ) ;
#115639 = ADVANCED_FACE ( 'NONE', ( #202541 ), #139744, .T. ) ;
#115640 = CARTESIAN_POINT ( 'NONE',  ( 2.289737743334671283, -0.8020533187339596859, 1.690132462187944107 ) ) ;
#115641 = CARTESIAN_POINT ( 'NONE',  ( 3.485274717979901293, 0.04603381543630095940, 2.069897711131869933 ) ) ;
#115642 = AXIS2_PLACEMENT_3D ( 'NONE', #19540, #133343, #118187 ) ;
#115643 = CARTESIAN_POINT ( 'NONE',  ( -7.146556367734805626, 9.431011410480991231, 1.443375672974064550 ) ) ;
#115644 = CARTESIAN_POINT ( 'NONE',  ( 1.880979024232478425, -1.749874716401520036, -0.7718601483891265325 ) ) ;
#115645 = CARTESIAN_POINT ( 'NONE',  ( 11.97929049433705373, 11.37999999999999901, 0.7046979865771783036 ) ) ;
#115646 = CARTESIAN_POINT ( 'NONE',  ( -10.82993273518205690, 5.589502548902120616, -6.507125152095314391 ) ) ;
#115647 = CARTESIAN_POINT ( 'NONE',  ( -4.916039773278787273, 4.881957280557857715, 0.5603013081572870702 ) ) ;
#115648 = AXIS2_PLACEMENT_3D ( 'NONE', #87339, #154480, #105761 ) ;
#115649 = CARTESIAN_POINT ( 'NONE',  ( -0.6823417656249969321, 4.280208333674755394, -1.181850606188749264 ) ) ;
#115650 = CARTESIAN_POINT ( 'NONE',  ( 0.8086807686161383568, -0.4671638426185490967, -1.854305266343849956 ) ) ;
#115651 = EDGE_CURVE ( 'NONE', #162782, #96449, #150081, .T. ) ;
#115652 = CARTESIAN_POINT ( 'NONE',  ( 5.777182853198898904, 6.873039762554409293, -1.082531754730548412 ) ) ;
#115653 = CARTESIAN_POINT ( 'NONE',  ( 2.717183929654675811, -1.705535211757349456, -0.9694657131227711888 ) ) ;
#115654 = CARTESIAN_POINT ( 'NONE',  ( 1.850000000000000089, 4.013456704145457099E-20, 0.5999999999999969802 ) ) ;
#115655 = CARTESIAN_POINT ( 'NONE',  ( -3.772911886352873445, 7.623757310712140800, 0.7998128361456352531 ) ) ;
#115657 = CARTESIAN_POINT ( 'NONE',  ( -1.264911064067355984, 3.815615028976178102, -0.5000000000000005551 ) ) ;
#115656 = CARTESIAN_POINT ( 'NONE',  ( 7.587759525142423911, 12.00413654597487501, 0.7998128361456462443 ) ) ;
#115658 = B_SPLINE_CURVE_WITH_KNOTS ( 'NONE', 3,
 ( #150918, #2480, #52337, #213219, #126744, #62712 ),
 .UNSPECIFIED., .F., .F.,
 ( 4, 2, 4 ),
 ( 2.168404344970997553E-19, 0.001225895755212360813, 0.002451791510424720759 ),
 .UNSPECIFIED. ) ;
#115659 = CARTESIAN_POINT ( 'NONE',  ( 0.3857445262360514882, -0.8876765639535091346, 1.646530163845527195 ) ) ;
#115660 = CARTESIAN_POINT ( 'NONE',  ( 0.6823417656249882723, 2.426041667008084435, -1.181850606188749264 ) ) ;
#115661 = CARTESIAN_POINT ( 'NONE',  ( 1.705339411233731672, 1.749488060808137790, -0.9960635233151514667 ) ) ;
#115663 = CARTESIAN_POINT ( 'NONE',  ( 0.9314518356654817310, -1.671823418590481447, -1.299033474062233351 ) ) ;
#115662 = CARTESIAN_POINT ( 'NONE',  ( -6.724481002698120768, 9.828683022247721723, -1.082531754730538864 ) ) ;
#115664 = CARTESIAN_POINT ( 'NONE',  ( 8.991265305961727350, 12.32808046726238516, -7.950307984862021726 ) ) ;
#115665 = CARTESIAN_POINT ( 'NONE',  ( 3.227070907399377298, -1.911900318415656441, -0.7948586591664741352 ) ) ;
#115666 = CARTESIAN_POINT ( 'NONE',  ( 4.167152111353856547, 5.955039778036558040, 1.599625672291262513 ) ) ;
#115668 = CARTESIAN_POINT ( 'NONE',  ( 3.520313441042647540, 7.258782781191745137, 0.7998128361456321445 ) ) ;
#115667 = CARTESIAN_POINT ( 'NONE',  ( 5.771452434752829319, 1.244600244801373767, 1.679635579212119145 ) ) ;
#115670 = ORIENTED_EDGE ( 'NONE', *, *, #205691, .T. ) ;
#115669 = CARTESIAN_POINT ( 'NONE',  ( 4.278209411971904075, -1.050932907216840295, 1.492538610026641122 ) ) ;
#115671 = CARTESIAN_POINT ( 'NONE',  ( 7.879259827836241570, 12.34422023245099176, 1.040834085586084257E-14 ) ) ;
#115672 = CARTESIAN_POINT ( 'NONE',  ( 9.281908132336914363, 13.38402037623112939, -6.770111635749896273 ) ) ;
#115673 = CARTESIAN_POINT ( 'NONE',  ( 5.245248717291847385, -1.895131572898335115, 1.130396782059706950 ) ) ;
#115675 =( BOUNDED_CURVE ( )  B_SPLINE_CURVE ( 2, ( #70577, #20768, #202719, #54370, #38118, #11997, #174540 ),
 .UNSPECIFIED., .F., .T. ) 
 B_SPLINE_CURVE_WITH_KNOTS ( ( 3, 2, 2, 3 ),
 ( 0.2624999999999999001, 0.2666666666666666075, 0.2708333333333333148, 0.2750000000000000777 ),
 .UNSPECIFIED. ) 
 CURVE ( )  GEOMETRIC_REPRESENTATION_ITEM ( )  RATIONAL_B_SPLINE_CURVE ( ( 1.000000000000003553, 0.8660254037844351549, 1.000000000000000000, 0.8660254037844387076, 1.000000000000000000, 0.8660254037844369313, 1.000000000000001776 ) ) 
 REPRESENTATION_ITEM ( '' )  );
#115674 = CARTESIAN_POINT ( 'NONE',  ( 1.364683531249996529, 10.02604166700806587, 0.7879004041258403923 ) ) ;
#115676 = ORIENTED_EDGE ( 'NONE', *, *, #127848, .F. ) ;
#115677 = CARTESIAN_POINT ( 'NONE',  ( 3.949791169003769475, -1.320912084567291034, -1.382976300589415342 ) ) ;
#115678 = CARTESIAN_POINT ( 'NONE',  ( -10.13488352141530768, 11.78278451552804817, 1.199719254218462483 ) ) ;
#115679 = CARTESIAN_POINT ( 'NONE',  ( 6.795661308947685164, 8.951357498570873261, -1.599625672291262513 ) ) ;
#115680 = CARTESIAN_POINT ( 'NONE',  ( 1.360316468750007779, 1.296875000341410455, -2.602085213965210642E-14 ) ) ;
#115681 = CARTESIAN_POINT ( 'NONE',  ( 5.802526556524483681, 5.871961858807763335, 1.040834085586084257E-14 ) ) ;
#115682 = EDGE_CURVE ( 'NONE', #28251, #18174, #91353, .T. ) ;
#115683 = CARTESIAN_POINT ( 'NONE',  ( -5.599738924909661186, 5.745725798494749625, 0.2540040342395213369 ) ) ;
#115684 = CARTESIAN_POINT ( 'NONE',  ( 7.127625674359589603, 14.48154076733629303, -9.656946008600062470 ) ) ;
#115685 = CARTESIAN_POINT ( 'NONE',  ( 0.06366010765614799061, -1.203631707120488947, 1.393476991864414760 ) ) ;
#115686 = ORIENTED_EDGE ( 'NONE', *, *, #3792, .T. ) ;
#115687 = CARTESIAN_POINT ( 'NONE',  ( 6.051950339013592028, 7.082009231019537943, 1.085686599464001478 ) ) ;
#115688 = CARTESIAN_POINT ( 'NONE',  ( 5.272658424858247095, -1.760895560629770262, -0.6313210838888929644 ) ) ;
#115689 = DIRECTION ( 'NONE',  ( -0.000000000000000000, 1.000000000000000000, -0.000000000000000000 ) ) ;
#115690 = CYLINDRICAL_SURFACE ( 'NONE', #15430, 1.224999999999996980 ) ;
#115692 = CARTESIAN_POINT ( 'NONE',  ( -5.856759171423528088, 8.816340885760650892, 1.082531754730548412 ) ) ;
#115691 = CIRCLE ( 'NONE', #56747, 11.69999999999999041 ) ;
#115693 = CARTESIAN_POINT ( 'NONE',  ( 4.904298879841284098, 6.744767997946721216, 1.599625672291267398 ) ) ;
#115694 = CARTESIAN_POINT ( 'NONE',  ( 1.217558188649459527, 0.3894938459214473125, -1.930362121600463610 ) ) ;
#115695 = EDGE_CURVE ( 'NONE', #172181, #78601, #143322, .T. ) ;
#115696 = CARTESIAN_POINT ( 'NONE',  ( 1.862907868837269998, -0.1017702599966328891, -2.013986063733465226 ) ) ;
#115697 = CARTESIAN_POINT ( 'NONE',  ( -7.147119532698295252, 11.49005655479003174, 0.000000000000000000 ) ) ;
#115698 = CARTESIAN_POINT ( 'NONE',  ( 7.530627977747744062, 7.750430493652658015, -0.7998128361456341429 ) ) ;
#115699 = CARTESIAN_POINT ( 'NONE',  ( 1.419999999999822515, 7.240846818246208905, 4.154462424328221104 ) ) ;
#115700 = CARTESIAN_POINT ( 'NONE',  ( 2.589988673929614738, -2.185656584452956075, -0.1600571409424780822 ) ) ;
#115701 = CARTESIAN_POINT ( 'NONE',  ( 6.340460056601358474, 1.806591233369018834, 0.2625940548972791611 ) ) ;
#115702 = CARTESIAN_POINT ( 'NONE',  ( -9.541187415715041809, 12.15447128979948310, -1.599625672291263179 ) ) ;
#115703 = CARTESIAN_POINT ( 'NONE',  ( 6.825078400183573812, 7.629137130509070275, 2.455651831298297338 ) ) ;
#115704 = CARTESIAN_POINT ( 'NONE',  ( 10.48884024596648601, 1.000000000000000888, -5.608780650328974104 ) ) ;
#115705 = CIRCLE ( 'NONE', #98500, 2.000000000000000000 ) ;
#115706 = CARTESIAN_POINT ( 'NONE',  ( 4.421367491832270957, 6.251624388594711590, 1.443375672974058777 ) ) ;
#115707 = CARTESIAN_POINT ( 'NONE',  ( 8.609591239877852686, 10.00327685373437347, -1.199719254218445830 ) ) ;
#115708 = CARTESIAN_POINT ( 'NONE',  ( 3.837121167867449945, 4.435395103055503441, 1.199719254218464037 ) ) ;
#115709 = CARTESIAN_POINT ( 'NONE',  ( 5.533136088152891929, 9.469426179571447832, -0.7216878364870458196 ) ) ;
#115710 = VERTEX_POINT ( 'NONE', #33664 ) ;
#115712 = CARTESIAN_POINT ( 'NONE',  ( 2.262359935378143394, 2.012689932058016495, 0.04726890441942610543 ) ) ;
#115711 = CARTESIAN_POINT ( 'NONE',  ( 5.372543328820884589, -0.05112055865702340440, -1.840719716649619198 ) ) ;
#115713 = CARTESIAN_POINT ( 'NONE',  ( 3.146212962842390937, -0.1666923573656608759, -2.292372948102610053 ) ) ;
#115715 = CARTESIAN_POINT ( 'NONE',  ( 1.358004595412452664, -1.861131634099476573, -0.006961619045023344915 ) ) ;
#115714 = CARTESIAN_POINT ( 'NONE',  ( 3.094265954482833703, 2.800000000000017586, -2.490342512183683965 ) ) ;
#115716 = CARTESIAN_POINT ( 'NONE',  ( -3.475000000000000533, 0.000000000000000000, 0.000000000000000000 ) ) ;
#115717 = CARTESIAN_POINT ( 'NONE',  ( -3.253066792275140173, 5.882662793374543675, 1.199719254218462483 ) ) ;
#115718 = CARTESIAN_POINT ( 'NONE',  ( -9.497986836791788789, 15.41982400883598459, -7.334206419346871009 ) ) ;
#115719 = CARTESIAN_POINT ( 'NONE',  ( 4.060738401289211374, 0.5150538496448524572, 1.841637258418599155 ) ) ;
#115720 = CARTESIAN_POINT ( 'NONE',  ( -7.995557903757128493, 10.35123685918189729, 1.599625672291295375 ) ) ;
#115721 = CARTESIAN_POINT ( 'NONE',  ( -6.943184063974178422, 8.233374508458908281, -1.082531754730549967 ) ) ;
#115723 = CARTESIAN_POINT ( 'NONE',  ( 1.797508989346347619, -0.6330400025267440833, 1.760413054629046625 ) ) ;
#115722 = CARTESIAN_POINT ( 'NONE',  ( 3.983990651536262195, -2.068283627568163308, -0.3046923749255076586 ) ) ;
#115724 = CARTESIAN_POINT ( 'NONE',  ( 6.887178846062110615, 9.058127958537705027, -1.443375672974057666 ) ) ;
#115725 = CARTESIAN_POINT ( 'NONE',  ( -0.6823417656250212460, 4.863541667008086655, 1.181850606188767472 ) ) ;
#115726 = CARTESIAN_POINT ( 'NONE',  ( 6.058133912487986272, -1.297239342979487509, 1.306937132449899508 ) ) ;
#115727 = CARTESIAN_POINT ( 'NONE',  ( 2.835626683552519012, 6.459981564119914310, 0.000000000000000000 ) ) ;
#115728 = CYLINDRICAL_SURFACE ( 'NONE', #134307, 0.07999999999999998779 ) ;
#115729 = CARTESIAN_POINT ( 'NONE',  ( 4.775862138867135620, 0.9967549737653296216, 1.407514542897546850 ) ) ;
#115730 = CARTESIAN_POINT ( 'NONE',  ( -7.009729113465285266, 8.136771039586342624, -1.199719254218446718 ) ) ;
#115731 = SURFACE_STYLE_USAGE ( .BOTH. , #65821 ) ;
#115732 = FILL_AREA_STYLE_COLOUR ( '', #3487 ) ;
#115733 =( BOUNDED_SURFACE ( )  B_SPLINE_SURFACE ( 3, 2, ( 
 ( #162753, #80417, #146515 ),
 ( #212534, #64174, #108717 ),
 ( #158470, #81485, #83603 ),
 ( #197354, #150764, #198408 ),
 ( #50052, #183239, #85742 ),
 ( #3399, #16455, #67325 ) ),
 .UNSPECIFIED., .F., .F., .T. ) 
 B_SPLINE_SURFACE_WITH_KNOTS ( ( 4, 2, 4 ),
 ( 3, 3 ),
 ( 0.000000000000000000, 0.0003754689591423961527, 0.0007509379182847923054 ),
 ( 0.000000000000000000, 1.000000000000000000 ),
 .UNSPECIFIED. ) 
 GEOMETRIC_REPRESENTATION_ITEM ( )  RATIONAL_B_SPLINE_SURFACE ( (
 ( 1.000000000000000000, 0.7071067811865551223, 1.000000000000000000),
 ( 1.000000000000000000, 0.7018599272026838642, 1.000000000000000000),
 ( 1.000000000000000000, 0.6927733177256477637, 1.000000000000000000),
 ( 1.000000000000000000, 0.6772007068877506919, 1.000000000000000000),
 ( 1.000000000000000000, 0.6709974581634180479, 1.000000000000000000),
 ( 1.000000000000000000, 0.6711954675835484219, 1.000000000000000000) ) ) 
 REPRESENTATION_ITEM ( '' )  SURFACE ( )  );
#115734 = CARTESIAN_POINT ( 'NONE',  ( 0.000000000000000000, 14.00000000000000533, -0.6500000000000000222 ) ) ;
#115735 = CARTESIAN_POINT ( 'NONE',  ( 5.207971749312423348, 0.6875717650507988665, -2.059362367386765591 ) ) ;
#115736 = CARTESIAN_POINT ( 'NONE',  ( 3.650846181029033133, -1.491723252493650564, 1.052289205326197852 ) ) ;
#115737 = CARTESIAN_POINT ( 'NONE',  ( 0.9714493606215730548, -0.2934177832072166758, 1.939591667560663035 ) ) ;
#115738 = CARTESIAN_POINT ( 'NONE',  ( 5.313701412219064224, -1.345319185855331279, -1.634962184252206630 ) ) ;
#115740 = CARTESIAN_POINT ( 'NONE',  ( 0.6823417656249899377, 3.738541667008085767, -1.181850606188754593 ) ) ;
#115739 = CARTESIAN_POINT ( 'NONE',  ( 6.216396969532355321, 2.137338928125806614, 0.8291867496624371059 ) ) ;
#115741 = CARTESIAN_POINT ( 'NONE',  ( 3.741371894207620397, 7.428709027653095376, 2.448389769268505933 ) ) ;
#115742 = CARTESIAN_POINT ( 'NONE',  ( 7.716561984472250835, 12.15440608185967086, 1.040834085586084257E-14 ) ) ;
#115743 = CARTESIAN_POINT ( 'NONE',  ( 1.225412164737609055, 1.871785320780447792, 0.9964087003688710809 ) ) ;
#115744 = CARTESIAN_POINT ( 'NONE',  ( -4.121315508874255684, 7.752025827087861920, -0.7216878364870267237 ) ) ;
#115745 = CARTESIAN_POINT ( 'NONE',  ( 6.000769315822030740E-16, -3.600000000000005862, 4.899999999999999467 ) ) ;
#115746 = CARTESIAN_POINT ( 'NONE',  ( -3.741687207247254676, 7.309126141856352454, 1.040834085586084257E-14 ) ) ;
#115747 = CARTESIAN_POINT ( 'NONE',  ( 6.491115304390381979, 0.2044268322529273207, 2.161409909153473752 ) ) ;
#115749 = CARTESIAN_POINT ( 'NONE',  ( 1.500000000000001332, 12.40625000068279427, 0.000000000000000000 ) ) ;
#115748 = CARTESIAN_POINT ( 'NONE',  ( 6.883263157960391787, 1.253787318140922480, 2.167784446185747171 ) ) ;
#115751 = ORIENTED_EDGE ( 'NONE', *, *, #62042, .T. ) ;
#115750 = CARTESIAN_POINT ( 'NONE',  ( 2.842673000788879634, 1.232056068812878991, -1.848115600964394867 ) ) ;
#115752 = CARTESIAN_POINT ( 'NONE',  ( 6.486953984781112403, -2.015912550161761629, 0.05229459904129707404 ) ) ;
#115754 = CARTESIAN_POINT ( 'NONE',  ( 4.803617054199708747, -1.591134784341166508, -1.312391874486463550 ) ) ;
#115753 = CARTESIAN_POINT ( 'NONE',  ( 5.657830175604453338, 5.495223381160312393, 0.7998128361456341429 ) ) ;
#115756 = CARTESIAN_POINT ( 'NONE',  ( -0.2408018239684096284, -0.007136184528808932684, -2.100252307185761058 ) ) ;
#115755 = CARTESIAN_POINT ( 'NONE',  ( 4.854701522145073334, 7.821512988214679218, -1.199719254218450271 ) ) ;
#115757 = CARTESIAN_POINT ( 'NONE',  ( 6.737475991348287785, 6.825086509519945999, -0.7998128361456481317 ) ) ;
#115758 = CARTESIAN_POINT ( 'NONE',  ( 1.642778471875001811, -3.930208332855376074, 2.845375778867859751 ) ) ;
#115759 = CARTESIAN_POINT ( 'NONE',  ( 1.203907071533389272, 2.962770253743141069, 0.7750000000000100142 ) ) ;
#115760 = CARTESIAN_POINT ( 'NONE',  ( 0.6739141125756157313, -1.159797070128726793, 1.739218980263528946 ) ) ;
#115761 = CARTESIAN_POINT ( 'NONE',  ( 4.317794123949899365, 1.129187743159822288, -1.454283868005897151 ) ) ;
#115763 = EDGE_LOOP ( 'NONE', ( #203388, #148552, #28417, #98045 ) ) ;
#115762 = CARTESIAN_POINT ( 'NONE',  ( 4.517891501851804215, 6.293959390292322986, -1.599625672291255185 ) ) ;
#115764 = CARTESIAN_POINT ( 'NONE',  ( 2.221339967433374252, -1.673790515994465711, 0.4157018595009522310 ) ) ;
#115765 = CARTESIAN_POINT ( 'NONE',  ( -2.836231403021655773, 6.427000396871998866, 0.000000000000000000 ) ) ;
#115766 = CARTESIAN_POINT ( 'NONE',  ( 1.776460590643181625, 1.997282851074515975, -1.137850514363091481 ) ) ;
#115767 = CARTESIAN_POINT ( 'NONE',  ( -1.364683531249997417, 4.321875000341417028, 1.214306433183764966E-14 ) ) ;
#115768 = CARTESIAN_POINT ( 'NONE',  ( 0.8258823708265795593, -2.148021843699068789, 0.7105549608077809109 ) ) ;
#115769 = CARTESIAN_POINT ( 'NONE',  ( 4.319037722229518650, 1.925386421186209507, 0.8538897750212376403 ) ) ;
#115770 = CARTESIAN_POINT ( 'NONE',  ( -3.902768115887413014, 5.646591783325653147, -1.599625672291283607 ) ) ;
#115771 = CARTESIAN_POINT ( 'NONE',  ( 2.723612921674794407, -1.015349471937683656, -1.449289906420585305 ) ) ;
#115772 = CARTESIAN_POINT ( 'NONE',  ( 5.452350330990040739, 9.512825819463730070, 0.7998128361456462443 ) ) ;
#115773 = CARTESIAN_POINT ( 'NONE',  ( 3.865483193227626124, 7.523831135491951372, -0.7216878364870338292 ) ) ;
#115776 = EDGE_CURVE ( 'NONE', #31452, #121557, #15232, .T. ) ;
#115775 = AXIS2_PLACEMENT_3D ( 'NONE', #148442, #111739, #131185 ) ;
#115774 = CARTESIAN_POINT ( 'NONE',  ( -5.117312914154178216, 8.057616602233474978, -1.199719254218452047 ) ) ;
#115777 = CARTESIAN_POINT ( 'NONE',  ( -0.7500000000000215383, 1.941666666666688634, 1.299038105676659116 ) ) ;
#115778 = CARTESIAN_POINT ( 'NONE',  ( -3.100010679019018500, 6.768429558830820980, 1.040834085586084257E-14 ) ) ;
#115779 = CARTESIAN_POINT ( 'NONE',  ( 5.133148801814766848, 2.052693810517117079, 0.8496366593433544168 ) ) ;
#115780 = CARTESIAN_POINT ( 'NONE',  ( 3.363397379774799134, 2.138023915923603635, -0.4802275100637617977 ) ) ;
#115781 = CARTESIAN_POINT ( 'NONE',  ( -5.436983294280064882, 6.301900917203534291, 1.199719254218450271 ) ) ;
#115782 = CARTESIAN_POINT ( 'NONE',  ( -4.309512724297390740, 6.121127159803966933, 1.599625672291270506 ) ) ;
#115783 = CARTESIAN_POINT ( 'NONE',  ( 5.795592431653455279, 1.959276243578732091, -0.8114611383256833399 ) ) ;
#115784 = B_SPLINE_CURVE_WITH_KNOTS ( 'NONE', 3,
 ( #73243, #126368, #155588, #206453, #109035, #26641, #207524, #72171, #105807, #175054 ),
 .UNSPECIFIED., .F., .F.,
 ( 4, 2, 2, 2, 4 ),
 ( 0.001944662270655115070, 0.002404849405959078121, 0.002865036541263041824, 0.003325223676567005959, 0.003785410811870969661 ),
 .UNSPECIFIED. ) ;
#115785 = CARTESIAN_POINT ( 'NONE',  ( -1.201851678989727383E-14, 3.821875000341423689, 1.575800808251672791 ) ) ;
#115786 = CARTESIAN_POINT ( 'NONE',  ( 6.890000000000001457, 2.439643239904603966, 2.382311923195524095 ) ) ;
#115787 = CARTESIAN_POINT ( 'NONE',  ( -4.826339496784927796, 5.693446170079573321, 1.082531754730560403 ) ) ;
#115788 = CARTESIAN_POINT ( 'NONE',  ( 5.361630242575341931, -1.673063676233761621, -1.302930760576012092 ) ) ;
#115789 = CARTESIAN_POINT ( 'NONE',  ( -7.919371124158132602, 8.411890197705517380, -0.7216878364870338292 ) ) ;
#115790 = ORIENTED_EDGE ( 'NONE', *, *, #126439, .F. ) ;
#115792 = FACE_OUTER_BOUND ( 'NONE', #89876, .T. ) ;
#115791 = CARTESIAN_POINT ( 'NONE',  ( -6.143253000767895600, 6.339752387083549934, 0.000000000000000000 ) ) ;
#115793 = CARTESIAN_POINT ( 'NONE',  ( 5.518332215962025167, 6.396807992499198292, -1.199719254218445830 ) ) ;
#115794 = CARTESIAN_POINT ( 'NONE',  ( 6.427308110136687347, -1.208249125052461181, -1.389453836245766016 ) ) ;
#115795 = UNCERTAINTY_MEASURE_WITH_UNIT (LENGTH_MEASURE( 1.000000000000000082E-05 ), #164460, 'distance_accuracy_value', 'NONE');
#115796 = CARTESIAN_POINT ( 'NONE',  ( 0.3282377607281172782, 0.9888354509981792662, -1.225000000000007860 ) ) ;
#115797 = CARTESIAN_POINT ( 'NONE',  ( 0.6823417656249882723, 2.988541667008084879, -1.181850606188754593 ) ) ;
#115798 = CARTESIAN_POINT ( 'NONE',  ( 1.504977638028012432, -1.727349551440153119, 0.2125612633746311042 ) ) ;
#115799 = CARTESIAN_POINT ( 'NONE',  ( 3.816783937446950770, 4.411668334231586996, 1.199719254218464037 ) ) ;
#115800 = CARTESIAN_POINT ( 'NONE',  ( 0.2913577194270203785, -1.795273245208812485, 0.7915465721433642132 ) ) ;
#115801 = CARTESIAN_POINT ( 'NONE',  ( -1.364683531250014514, 0.5510416670080878765, -0.7879004041258289570 ) ) ;
#115802 = FACE_OUTER_BOUND ( 'NONE', #190322, .T. ) ;
#115803 = CARTESIAN_POINT ( 'NONE',  ( 4.733375416736937069, -1.977748744329570263, 0.8730265686548792647 ) ) ;
#115804 = EDGE_CURVE ( 'NONE', #178259, #193812, #199347, .T. ) ;
#115805 = TOROIDAL_SURFACE ( 'NONE', #205567, 3.599999999999999201, 0.4999999999999998890 ) ;
#115806 = CARTESIAN_POINT ( 'NONE',  ( -4.135400547368138113, 4.783387712472935149, 1.199719254218462483 ) ) ;
#115807 = CARTESIAN_POINT ( 'NONE',  ( -6.033015167956800262, 9.021972881716168402, -1.082531754730537976 ) ) ;
#115808 = CARTESIAN_POINT ( 'NONE',  ( 4.750933126423753095, -1.738186171353903742, 1.284983810367075208 ) ) ;
#115810 = ORIENTED_EDGE ( 'NONE', *, *, #107334, .F. ) ;
#115809 = CARTESIAN_POINT ( 'NONE',  ( -5.307090785106547415, 5.156303768904543894, -0.7998128361456362523 ) ) ;
#115811 = CARTESIAN_POINT ( 'NONE',  ( -1.364683531249997417, 3.009375000341422801, 1.214306433183764966E-14 ) ) ;
#115812 = CARTESIAN_POINT ( 'NONE',  ( 5.518811311470022574, 1.820418058502238035, 0.7569790930031635723 ) ) ;
#115813 = CARTESIAN_POINT ( 'NONE',  ( 5.272643526055802887, -1.725312034932389382, 0.1713184177872198732 ) ) ;
#115814 = CIRCLE ( 'NONE', #91503, 0.07999999999999984901 ) ;
#115816 = CARTESIAN_POINT ( 'NONE',  ( 1.699035084177059174, 1.824418957995146195, 1.213967346723361596 ) ) ;
#115815 = CARTESIAN_POINT ( 'NONE',  ( 1.360316468749964480, -0.2343749996585806072, -5.204170427930421283E-15 ) ) ;
#115817 = CARTESIAN_POINT ( 'NONE',  ( 3.751255533806226339, -1.888273344036644819, 1.326175916821286105 ) ) ;
#115818 = CARTESIAN_POINT ( 'NONE',  ( 4.692684478349196553, -0.4476203070050369104, -2.011419953914685088 ) ) ;
#115819 = CARTESIAN_POINT ( 'NONE',  ( 0.2341854262303414147, 0.3310631332954366290, 1.913375037591731775 ) ) ;
#115820 = CARTESIAN_POINT ( 'NONE',  ( -5.517805330637490790, 9.381263952478319013, 0.7216878364870458196 ) ) ;
#115821 = CARTESIAN_POINT ( 'NONE',  ( -5.503684012504701961, 5.385662534202396934, 0.000000000000000000 ) ) ;
#115822 = CARTESIAN_POINT ( 'NONE',  ( 0.4153311931458965045, 3.850000000000006306, -0.4999999999999987232 ) ) ;
#115823 = CARTESIAN_POINT ( 'NONE',  ( 4.342108446431157454, -1.306982937058022820, -1.669832246961988176 ) ) ;
#115824 = PRESENTATION_STYLE_ASSIGNMENT (( #49696 ) ) ;
#115825 = CARTESIAN_POINT ( 'NONE',  ( 1.248672897702383988, 1.986100274556975354, -0.3474695496914689818 ) ) ;
#115826 = CARTESIAN_POINT ( 'NONE',  ( -6.439759776366783761, 8.536139043893143707, 1.443375672974078761 ) ) ;
#115827 = CARTESIAN_POINT ( 'NONE',  ( 4.823365732668142947, -0.1123398232194070118, 2.204042774474362254 ) ) ;
#115828 = CARTESIAN_POINT ( 'NONE',  ( 1.001543065824772753E-15, -1.159374999522043481, 3.793834371823811669 ) ) ;
#115829 = AXIS2_PLACEMENT_3D ( 'NONE', #209952, #127760, #174304 ) ;
#115830 = CARTESIAN_POINT ( 'NONE',  ( 0.1399997263885795484, 5.723012109828673921, -2.593777676649943409 ) ) ;
#115831 = DIRECTION ( 'NONE',  ( 2.526156499269438135E-14, 0.6299249119529302110, -0.7766560405360234398 ) ) ;
#115832 = CARTESIAN_POINT ( 'NONE',  ( -9.566809970446467304, -7.630846356335648117, 9.989423754102837008E-15 ) ) ;
#115834 = CARTESIAN_POINT ( 'NONE',  ( -9.242574560015905050, -9.438200158419387975, 0.5964493340168121049 ) ) ;
#115833 = CARTESIAN_POINT ( 'NONE',  ( -4.684263184503158151, 8.377143357790286515, -0.6327197186303500365 ) ) ;
#115835 = SURFACE_STYLE_FILL_AREA ( #15049 ) ;
#115836 = ORIENTED_EDGE ( 'NONE', *, *, #99758, .F. ) ;
#115837 = CARTESIAN_POINT ( 'NONE',  ( 3.010674446437047624, 1.493694004556917365, -1.420165857245965668 ) ) ;
#115838 = CARTESIAN_POINT ( 'NONE',  ( -1.360316468750072838, 1.661458333674769694, 0.7853790794158601596 ) ) ;
#115839 = CARTESIAN_POINT ( 'NONE',  ( -6.417086777969760902, 6.381022750586497594, 0.7998128361456341429 ) ) ;
#115840 = CARTESIAN_POINT ( 'NONE',  ( 3.264323853713008816, 2.019862492602925386, -0.002211735406987268802 ) ) ;
#115841 = CARTESIAN_POINT ( 'NONE',  ( -1.500000000000015099, -0.5791666666666476226, 0.8660254037844403729 ) ) ;
#115842 = CARTESIAN_POINT ( 'NONE',  ( 10.38518247838791986, 11.21839376764850726, 0.7216878364870438212 ) ) ;
#115843 = CARTESIAN_POINT ( 'NONE',  ( 3.256764320543267921, -1.561506546599530143, 1.345091337369247242 ) ) ;
#115844 = DIRECTION ( 'NONE',  ( 0.000000000000000000, 0.000000000000000000, 1.000000000000000000 ) ) ;
#115845 = CARTESIAN_POINT ( 'NONE',  ( 6.505214776458575265, 6.483838748823460563, 1.040834085586084257E-14 ) ) ;
#115846 = CARTESIAN_POINT ( 'NONE',  ( -0.1409997244346087863, -0.002808977843308038246, -2.000147647483837776 ) ) ;
#115848 = AXIS2_PLACEMENT_3D ( 'NONE', #208294, #177961, #175834 ) ;
#115847 = CARTESIAN_POINT ( 'NONE',  ( 1.569984571489828173, -1.747861548559765721, -0.5788160320587890650 ) ) ;
#115849 = CARTESIAN_POINT ( 'NONE',  ( 6.691986956589398794, -0.9478133180038283978, 1.990996264204819122 ) ) ;
#115850 = CARTESIAN_POINT ( 'NONE',  ( 5.631432701629774051, 7.663367133358481631, 1.599625672291269396 ) ) ;
#115851 = CARTESIAN_POINT ( 'NONE',  ( 1.142116303652768172, 0.8771353898661786719, -1.975824051420910221 ) ) ;
#115852 = CARTESIAN_POINT ( 'NONE',  ( -2.806174608348664723, 6.217694776474651519, 1.040834085586084257E-14 ) ) ;
#115853 = CARTESIAN_POINT ( 'NONE',  ( 2.202361591730035428, 1.313542931311746598, -1.530159205979222170 ) ) ;
#115854 = EDGE_CURVE ( 'NONE', #175466, #169074, #153639, .T. ) ;
#115855 = CARTESIAN_POINT ( 'NONE',  ( -0.1054627972275519465, 3.385846599571567417, -2.076146368081344118 ) ) ;
#115856 = CARTESIAN_POINT ( 'NONE',  ( 0.1626889888870358680, -1.668787113083155305, -0.8454427722031019332 ) ) ;
#115857 = CARTESIAN_POINT ( 'NONE',  ( 11.43195036480943116, 11.15524496285256006, 3.649565797774380727 ) ) ;
#115858 = CARTESIAN_POINT ( 'NONE',  ( 4.434422825387909661, 1.933224968735423266, 0.3856102937377944295 ) ) ;
#115859 = CARTESIAN_POINT ( 'NONE',  ( 4.979703994296570180, -0.7212954316567052881, 1.883311551353183511 ) ) ;
#115861 = CARTESIAN_POINT ( 'NONE',  ( 9.124274191872634887, 11.66807252865000244, -1.443375672974058777 ) ) ;
#115860 = CARTESIAN_POINT ( 'NONE',  ( -1.402160292154681736E-14, 2.446875000341416584, -1.575800808251660134 ) ) ;
#115863 = CARTESIAN_POINT ( 'NONE',  ( 6.568975480045090798, -1.924755568788787397, -0.8553139683228675461 ) ) ;
#115862 = CARTESIAN_POINT ( 'NONE',  ( -8.213542131780492639, 8.476887330032372603, 1.040834085586084257E-14 ) ) ;
#115864 = CARTESIAN_POINT ( 'NONE',  ( 4.844224204019831781, -0.9789346907586125024, 1.824324395707350943 ) ) ;
#115865 = CARTESIAN_POINT ( 'NONE',  ( 6.632963465583686435, 8.761543347979550589, -1.599625672291262513 ) ) ;
#115866 = CARTESIAN_POINT ( 'NONE',  ( -6.738566041191992539, 7.820414121934134322, 1.199719254218450271 ) ) ;
#115867 = CARTESIAN_POINT ( 'NONE',  ( 6.639320575229283428, 0.5834889568891787892, 2.056715522164854981 ) ) ;
#115868 = CARTESIAN_POINT ( 'NONE',  ( 5.097918204798724595, 1.359643563815411405, 1.493766824747685185 ) ) ;
#115869 = CARTESIAN_POINT ( 'NONE',  ( -0.7500000000000249800, -0.5270833326505158789, 1.299038105676659116 ) ) ;
#115870 = CARTESIAN_POINT ( 'NONE',  ( 3.879734811474966794, 2.173438607767137043, -0.7759833549572618949 ) ) ;
#115871 = CIRCLE ( 'NONE', #102202, 0.09999999999999982514 ) ;
#115872 = CARTESIAN_POINT ( 'NONE',  ( 1.235300832636996970, -0.04672723545543105983, -2.062185333280424526 ) ) ;
#115873 = CARTESIAN_POINT ( 'NONE',  ( 7.104109303880752790, 11.23195192126214970, -0.7216878364870267237 ) ) ;
#115874 = CARTESIAN_POINT ( 'NONE',  ( 6.180537922983273091, 8.303989891604203422, -1.599625672291281386 ) ) ;
#115875 = CARTESIAN_POINT ( 'NONE',  ( 4.389807875774629942, 8.343469298370917997, 0.7998128361456271485 ) ) ;
#115876 = CARTESIAN_POINT ( 'NONE',  ( 0.6823417656249882723, 0.1552083336747514530, 1.181850606188755259 ) ) ;
#115877 = CARTESIAN_POINT ( 'NONE',  ( 3.705121118284530279, 7.544668081299086282, -1.734723475976807094E-15 ) ) ;
#115878 = CARTESIAN_POINT ( 'NONE',  ( 6.927853306458749749, 8.145212281365775908, 1.082531754730558626 ) ) ;
#115880 = CARTESIAN_POINT ( 'NONE',  ( -4.475070042639309520, 5.445751865460756846, 1.284222742053057642 ) ) ;
#115879 = CARTESIAN_POINT ( 'NONE',  ( 3.789651875377809898, -2.007375656734013969, 0.8277776116962390907 ) ) ;
#115881 = CARTESIAN_POINT ( 'NONE',  ( -4.448483798615272100, 8.203998508444197313, 0.000000000000000000 ) ) ;
#115883 = CARTESIAN_POINT ( 'NONE',  ( 3.227900028218867234, 1.797025815167479390, 0.4004103908350764573 ) ) ;
#115882 = CARTESIAN_POINT ( 'NONE',  ( -4.528060117284246289, 6.305822774963486310, 1.443375672974064550 ) ) ;
#115884 = CARTESIAN_POINT ( 'NONE',  ( 1.364683531249990311, 4.634375000341417916, 1.214306433183764966E-14 ) ) ;
#115885 = CARTESIAN_POINT ( 'NONE',  ( 4.792620198997869174, 1.822056328612733145, -1.217503271791681163 ) ) ;
#115886 = CARTESIAN_POINT ( 'NONE',  ( 8.809690371089210714, 13.28836970969089748, 8.148114100277194183 ) ) ;
#115887 = CARTESIAN_POINT ( 'NONE',  ( 5.190393989392352303, -2.244764952986468831, -0.2824595779603657486 ) ) ;
#115888 = CARTESIAN_POINT ( 'NONE',  ( -5.768665591941109838, 6.232869020846472097, -1.039980349891131972 ) ) ;
#115889 = CARTESIAN_POINT ( 'NONE',  ( 5.488371254093075358, 7.473176909139983337, -1.250075884424824757 ) ) ;
#115890 = CARTESIAN_POINT ( 'NONE',  ( -4.434925645001610128, 8.188180662561590495, 0.7216878364870338292 ) ) ;
#115891 = CARTESIAN_POINT ( 'NONE',  ( 5.397554552016228691, 5.469770863539975991, 0.7216878364870328300 ) ) ;
#115892 = CARTESIAN_POINT ( 'NONE',  ( 6.274623264596165484, -1.681128386917314366, -0.5530667918781423387 ) ) ;
#115893 = CARTESIAN_POINT ( 'NONE',  ( 3.791655721365494891, 1.894798488814054327, -0.6802303536831488806 ) ) ;
#115894 = CARTESIAN_POINT ( 'NONE',  ( 8.132193210098487057, 8.381980254736715708, 1.040834085586084257E-14 ) ) ;
#115895 = CARTESIAN_POINT ( 'NONE',  ( 3.118299990072324057, -1.036503014707575332, -1.833135815837197535 ) ) ;
#115896 = CARTESIAN_POINT ( 'NONE',  ( 0.5619445578959707532, -1.063298924184744587, 1.593181094007071863 ) ) ;
#115897 = CARTESIAN_POINT ( 'NONE',  ( 2.822068529938852155, 6.444163718237301275, -0.7998128361456291469 ) ) ;
#115899 = EDGE_CURVE ( 'NONE', #71638, #101997, #120531, .T. ) ;
#115898 = CARTESIAN_POINT ( 'NONE',  ( 1.697640821309716497, -1.424308401971938975, -1.360563176039381261 ) ) ;
#115900 = CARTESIAN_POINT ( 'NONE',  ( 1.006479672118578916, 1.419055151971573059, -1.218976214888117804 ) ) ;
#115901 = CARTESIAN_POINT ( 'NONE',  ( 1.381223342121252085, -0.05156877537583307025, 1.961363007973878858 ) ) ;
#115903 = ORIENTED_EDGE ( 'NONE', *, *, #87595, .T. ) ;
#115902 = CARTESIAN_POINT ( 'NONE',  ( 0.07037084582631887575, 0.7337836260858082715, 1.766209603411242668 ) ) ;
#115904 = CARTESIAN_POINT ( 'NONE',  ( 5.883875478650832491, 6.927238148923188454, -1.082531754730543083 ) ) ;
#115905 = CARTESIAN_POINT ( 'NONE',  ( 0.6823417656249882723, 0.9885416670080832136, -1.181850606188749264 ) ) ;
#115906 = CARTESIAN_POINT ( 'NONE',  ( 5.682452175617663137, -1.825344843996518529, -0.4084625512627630406 ) ) ;
#115907 = CARTESIAN_POINT ( 'NONE',  ( 6.949925879317214950, -6.532648833121268872, -6.447267651612722084 ) ) ;
#115908 = ORIENTED_EDGE ( 'NONE', *, *, #831, .T. ) ;
#115909 = CARTESIAN_POINT ( 'NONE',  ( 2.482948226198860464, 5.072301959192136778, 2.420000000000000373 ) ) ;
#115910 = DIRECTION ( 'NONE',  ( 0.000000000000000000, 0.000000000000000000, -1.000000000000000000 ) ) ;
#115911 = CARTESIAN_POINT ( 'NONE',  ( 0.9771079587245214970, 1.912259438035465386, 0.7939916666956441382 ) ) ;
#115912 = CARTESIAN_POINT ( 'NONE',  ( 0.7499999999999902300, 1.733333333333357595, 1.299038105676657340 ) ) ;
#115913 = CARTESIAN_POINT ( 'NONE',  ( 5.991813822235618758, 9.077867661661846554, 1.199719254218462483 ) ) ;
#115914 = CARTESIAN_POINT ( 'NONE',  ( -8.701635661872465732, 9.046329781806354831, 1.040834085586084257E-14 ) ) ;
#115915 = CARTESIAN_POINT ( 'NONE',  ( 6.378184920586140727, 6.405913593630768510, 0.000000000000000000 ) ) ;
#115916 = CARTESIAN_POINT ( 'NONE',  ( 5.848313825214911610, 1.045240856298999432, -1.844880668361434939 ) ) ;
#115917 = CARTESIAN_POINT ( 'NONE',  ( 4.085803189671889157, 5.860132702740892263, -1.599625672291273171 ) ) ;
#115918 = CARTESIAN_POINT ( 'NONE',  ( -1.364683531250012516, 1.030208333674754062, 0.7879004041258379498 ) ) ;
#115920 = EDGE_CURVE ( 'NONE', #103686, #212524, #8283, .T. ) ;
#115919 = CARTESIAN_POINT ( 'NONE',  ( 0.7499999999999902300, 2.483333333333351156, 1.299038105676669330 ) ) ;
#115922 = CARTESIAN_POINT ( 'NONE',  ( 4.578903193113299963, 6.365139696764064325, 1.599625672291267398 ) ) ;
#115921 = CARTESIAN_POINT ( 'NONE',  ( 5.846142468697441252, -0.8834969228576605715, 1.751761657833034613 ) ) ;
#115923 = CARTESIAN_POINT ( 'NONE',  ( 2.776720060080526853, -1.994564479802892087, 0.2930246351905210211 ) ) ;
#115924 = CARTESIAN_POINT ( 'NONE',  ( 4.171028900271775974, 1.708651049203385286, -0.8665242481073615055 ) ) ;
#115925 = CARTESIAN_POINT ( 'NONE',  ( 11.92050416151432835, 9.947946247203756087, -1.381922468431410866 ) ) ;
#115926 = CARTESIAN_POINT ( 'NONE',  ( 1.558417602779540889, -1.546676288433556756, 1.552911753681482487 ) ) ;
#115927 = DIRECTION ( 'NONE',  ( -1.000000000000000000, -3.451266460341926649E-31, -8.638326563840809144E-31 ) ) ;
#115928 = CARTESIAN_POINT ( 'NONE',  ( 3.426877311086639288, 0.04264493303338459662, 1.870215716092846314 ) ) ;
#115929 = CARTESIAN_POINT ( 'NONE',  ( -0.7500000000000006661, -1.110416665983847473, -1.299038105676652011 ) ) ;
#115930 = CARTESIAN_POINT ( 'NONE',  ( -7.182068686937172153, 9.402166106225269715, 1.599625672291283607 ) ) ;
#115932 = CARTESIAN_POINT ( 'NONE',  ( 5.062167955004798436, -1.175237403299607797, 1.760913580352542862 ) ) ;
#115931 = CARTESIAN_POINT ( 'NONE',  ( -4.528060117284246289, 6.305822774963486310, 1.443375672974064550 ) ) ;
#115933 = DIRECTION ( 'NONE',  ( -5.551115123125765446E-17, 0.000000000000000000, 1.000000000000000000 ) ) ;
#115934 = CARTESIAN_POINT ( 'NONE',  ( -11.55950211276791428, 12.21999999999998288, 3.221476510067114329 ) ) ;
#115935 = B_SPLINE_CURVE_WITH_KNOTS ( 'NONE', 3,
 ( #143001, #208999, #111594, #94237 ),
 .UNSPECIFIED., .F., .F.,
 ( 4, 4 ),
 ( 0.000000000000000000, 0.0001936595853974351948 ),
 .UNSPECIFIED. ) ;
#115937 = CARTESIAN_POINT ( 'NONE',  ( 6.620655732516668834, 6.034240673559561507, 2.768629221164942145 ) ) ;
#115936 = CARTESIAN_POINT ( 'NONE',  ( 2.419574211619343274, -1.206166186839405352, -1.707533215648052050 ) ) ;
#115939 = ORIENTED_EDGE ( 'NONE', *, *, #60516, .T. ) ;
#115938 = CARTESIAN_POINT ( 'NONE',  ( 1.307153468561640164, -0.4245502288011630543, 1.671566548543522268 ) ) ;
#115940 = CARTESIAN_POINT ( 'NONE',  ( 5.289652487626049115, 9.323011668872403845, 0.7998128361456462443 ) ) ;
#115941 = CARTESIAN_POINT ( 'NONE',  ( -0.7500000000000006661, 11.98958333401613174, -1.299038105676657340 ) ) ;
#115942 = CARTESIAN_POINT ( 'NONE',  ( 0.000000000000000000, 2.099999999999997868, 0.000000000000000000 ) ) ;
#115943 = SURFACE_SIDE_STYLE ('',( #63933 ) ) ;
#115944 = CARTESIAN_POINT ( 'NONE',  ( 5.273758565591489145, 9.096542726591325234, -0.7216878364870267237 ) ) ;
#115945 = DIRECTION ( 'NONE',  ( 0.000000000000000000, 0.000000000000000000, -1.000000000000000000 ) ) ;
#115947 = CARTESIAN_POINT ( 'NONE',  ( 0.7854713186128524649, 1.746033005210102962, -0.4821264535347525859 ) ) ;
#115946 = CARTESIAN_POINT ( 'NONE',  ( 4.844006021832467646, 8.873367135438366304, 0.000000000000000000 ) ) ;
#115948 = CARTESIAN_POINT ( 'NONE',  ( -8.179646747746328828, 8.437342715325849341, -0.7998128361456291469 ) ) ;
#115949 = CARTESIAN_POINT ( 'NONE',  ( 3.734381245560244089, 6.444196322207211836, 1.199719254218462483 ) ) ;
#115950 = CARTESIAN_POINT ( 'NONE',  ( -6.197060558222979409, 6.958367536249086882, 0.8797177744420351386 ) ) ;
#115951 = CARTESIAN_POINT ( 'NONE',  ( 5.525830126021535449, 8.604496359403894346, -1.199719254218452047 ) ) ;
#115952 = CARTESIAN_POINT ( 'NONE',  ( 1.499999999999990896, 4.025000000000021672, 1.214306433183764966E-14 ) ) ;
#115953 = FILL_AREA_STYLE_COLOUR ( '', #55822 ) ;
#115954 = CARTESIAN_POINT ( 'NONE',  ( 3.996677956334552029, 7.600660605679141035, 0.1064861495668877750 ) ) ;
#115955 = CARTESIAN_POINT ( 'NONE',  ( 9.029367117021314115, 12.51771682229149008, -1.082531754730543083 ) ) ;
#115956 = ORIENTED_EDGE ( 'NONE', *, *, #37732, .F. ) ;
#115957 = CARTESIAN_POINT ( 'NONE',  ( 2.734617598447198539, -1.779929554887052401, -0.5434082684390993956 ) ) ;
#115958 = CARTESIAN_POINT ( 'NONE',  ( 0.3510145263703016716, 0.1867627727243931779, -1.906451055755745250 ) ) ;
#115959 = CARTESIAN_POINT ( 'NONE',  ( 6.264670948233396430, -1.361836867979081545, 1.362739274238314868 ) ) ;
#115960 = COLOUR_RGB ( '', 0.09019608, 0.27058824, 0.51372549) ;
#115961 = LINE ( 'NONE', #1053, #53799 ) ;
#115962 = CARTESIAN_POINT ( 'NONE',  ( 4.871809496981259535, 8.050285353323946680, -0.9368363805376724862 ) ) ;
#115963 = CARTESIAN_POINT ( 'NONE',  ( -1.534404370307023369, 8.695807324171010322, -2.514078760162028470 ) ) ;
#115964 = CARTESIAN_POINT ( 'NONE',  ( -4.934804725694236893, 4.859619722839116918, -0.7216878364870207285 ) ) ;
#115965 = AXIS2_PLACEMENT_3D ( 'NONE', #70330, #6401, #72473 ) ;
#115966 = CARTESIAN_POINT ( 'NONE',  ( 8.432808358020016826, 10.86136238915529084, 1.443375672974076540 ) ) ;
#115967 = CARTESIAN_POINT ( 'NONE',  ( 5.032068834786890044, 1.130672129898707245, 1.612349476345806831 ) ) ;
#115968 = EDGE_CURVE ( 'NONE', #192662, #212849, #32593, .T. ) ;
#115969 = CARTESIAN_POINT ( 'NONE',  ( 1.330900338397854155, 1.421537331630345014, -1.573617108223644312 ) ) ;
#115970 = CARTESIAN_POINT ( 'NONE',  ( -6.227272627378437342, 6.159572908229946187, -0.7998128361456291469 ) ) ;
#115971 = CARTESIAN_POINT ( 'NONE',  ( 3.475000000000000533, -2.624999999999998668, 0.000000000000000000 ) ) ;
#115972 = CARTESIAN_POINT ( 'NONE',  ( 6.351546390744762682, 2.185874319550953793, -0.1572705277706408500 ) ) ;
#115973 = LINE ( 'NONE', #49846, #140060 ) ;
#115974 = CARTESIAN_POINT ( 'NONE',  ( 3.891558735110557610, 1.394649387769153259, 1.329109640543422399 ) ) ;
#115975 = CARTESIAN_POINT ( 'NONE',  ( -6.612626235163205024, 8.737816579155630592, -1.599625672291263179 ) ) ;
#115976 = ADVANCED_FACE ( 'NONE', ( #73636 ), #170942, .T. ) ;
#115977 = CARTESIAN_POINT ( 'NONE',  ( 0.2701547006425785713, -1.196777392914155635, 1.378664180083796875 ) ) ;
#115978 = CARTESIAN_POINT ( 'NONE',  ( 1.260703874955213744, 0.8971468365699288849, 2.016480257658866737 ) ) ;
#115979 = CARTESIAN_POINT ( 'NONE',  ( 5.551071401176296938, 6.352922844458268159, -1.167898382037794613 ) ) ;
#115980 = ORIENTED_EDGE ( 'NONE', *, *, #204649, .T. ) ;
#115981 = PRESENTATION_STYLE_ASSIGNMENT (( #143399 ) ) ;
#115982 = VERTEX_POINT ( 'NONE', #57389 ) ;
#115983 = CARTESIAN_POINT ( 'NONE',  ( 6.737161338948785883, -0.09310609838950174855, -1.967343120315911298 ) ) ;
#115984 = CARTESIAN_POINT ( 'NONE',  ( 1.909617033088998328, -0.9174269660217245770, -1.711723090954318405 ) ) ;
#115985 = CARTESIAN_POINT ( 'NONE',  ( 6.186922437512073714, -1.269050685324083050, -1.916131536371464383 ) ) ;
#115987 = CARTESIAN_POINT ( 'NONE',  ( 4.223391696059366929, 0.2311737859471388323, -1.846484453672825321 ) ) ;
#115986 = CARTESIAN_POINT ( 'NONE',  ( -7.117104292530948229, 7.267986194233038155, -0.7998128361456362523 ) ) ;
#115988 = CARTESIAN_POINT ( 'NONE',  ( 5.200434439293556643, 8.224868058221247225, -1.199719254218452047 ) ) ;
#115989 = CARTESIAN_POINT ( 'NONE',  ( -5.303674958368855386, 4.754885796981216828, 2.500000000000000444 ) ) ;
#115990 = CARTESIAN_POINT ( 'NONE',  ( -6.891622154448065807, 6.934647356477856128, 1.040834085586084257E-14 ) ) ;
#115991 = CARTESIAN_POINT ( 'NONE',  ( -4.556949027968976829, 5.449433633119473264, 1.082531754730549078 ) ) ;
#115992 = CARTESIAN_POINT ( 'NONE',  ( -0.02351032182101517320, -2.127384168920816165, -0.5261613093957145937 ) ) ;
#115993 = CARTESIAN_POINT ( 'NONE',  ( 4.284013352238246419, 6.021101549076499637, -1.443375672974051449 ) ) ;
#115994 = ORIENTED_EDGE ( 'NONE', *, *, #17058, .T. ) ;
#115995 = LINE ( 'NONE', #130143, #119227 ) ;
#115996 = CARTESIAN_POINT ( 'NONE',  ( -7.065207446497166366, 9.336104335703744539, 0.000000000000000000 ) ) ;
#115997 = CARTESIAN_POINT ( 'NONE',  ( 1.699542765152612711, -0.6164703606487754728, 1.718597393154073671 ) ) ;
#115998 = CARTESIAN_POINT ( 'NONE',  ( -5.447678794592645701, 5.250046769979851646, 0.000000000000000000 ) ) ;
#115999 = CARTESIAN_POINT ( 'NONE',  ( 3.797271647414564910, 1.222981480435406443, -1.229749918556479304 ) ) ;
#116000 = CARTESIAN_POINT ( 'NONE',  ( -6.335246490290919574, 6.944623119882351148, -0.8941629942194727620 ) ) ;
#116001 = CARTESIAN_POINT ( 'NONE',  ( -1.876272499184424847, 0.7121508056591905333, 0.8723429728170274400 ) ) ;
#116002 = COLOUR_RGB ( '', 0.72549020, 0.75294118, 0.79215686) ;
#116003 = CARTESIAN_POINT ( 'NONE',  ( 1.386567914617388375, 8.090296256147718523, -10.72428812184712932 ) ) ;
#116004 = CARTESIAN_POINT ( 'NONE',  ( 0.3109947909220554529, 1.675391530434092280, 0.9509023542121838313 ) ) ;
#116005 = CARTESIAN_POINT ( 'NONE',  ( 4.750807836863311095, -0.4258335417525476729, -1.914832529679215023 ) ) ;
#116006 = CARTESIAN_POINT ( 'NONE',  ( -8.690940161559884913, 10.09818392903003748, 1.199719254218462483 ) ) ;
#116007 = CARTESIAN_POINT ( 'NONE',  ( 7.122110765880372618, 7.203550736482235095, 0.7998128361456341429 ) ) ;
#116008 = CARTESIAN_POINT ( 'NONE',  ( 5.110073233524446756, -0.7627883623938614965, 1.978724553277847464 ) ) ;
#116009 = CARTESIAN_POINT ( 'NONE',  ( -6.997979842947967377, 11.31606025008131233, -0.7998128361456291469 ) ) ;
#116010 = CIRCLE ( 'NONE', #188624, 0.05000000000000009298 ) ;
#116011 = CARTESIAN_POINT ( 'NONE',  ( 0.000000000000000000, -9.999999999999994671, 0.000000000000000000 ) ) ;
#116012 = CARTESIAN_POINT ( 'NONE',  ( 2.659107809384615884, 1.665393510391148801, -1.229642267604726058 ) ) ;
#116014 = CARTESIAN_POINT ( 'NONE',  ( -0.6823417656250246877, -0.6364583329919113464, 1.181850606188755259 ) ) ;
#116013 = FILL_AREA_STYLE_COLOUR ( '', #117030 ) ;
#116015 = ORIENTED_EDGE ( 'NONE', *, *, #108010, .T. ) ;
#116016 = CARTESIAN_POINT ( 'NONE',  ( 2.584987504963653038, -0.7174396784795608051, 2.183947998982360250 ) ) ;
#116017 = CARTESIAN_POINT ( 'NONE',  ( 7.619319141200057821, 10.87266085050000974, 1.082531754730557072 ) ) ;
#116019 = CARTESIAN_POINT ( 'NONE',  ( 3.285556943749998737, -2.005208332855377140, -1.896917185911906500 ) ) ;
#116018 = CARTESIAN_POINT ( 'NONE',  ( 5.180624094197585627, 8.097792972322238825, -1.082531754730548412 ) ) ;
#116020 = FILL_AREA_STYLE_COLOUR ( '', #151464 ) ;
#116021 = ORIENTED_EDGE ( 'NONE', *, *, #212155, .F. ) ;
#116023 = DIRECTION ( 'NONE',  ( 0.000000000000000000, -1.000000000000000000, 0.000000000000000000 ) ) ;
#116022 = AXIS2_PLACEMENT_3D ( 'NONE', #21332, #87438, #71151 ) ;
#116024 = CARTESIAN_POINT ( 'NONE',  ( 4.517770118113122457, -0.5046507728132009207, 1.844564425022446885 ) ) ;
#116025 = CARTESIAN_POINT ( 'NONE',  ( 1.773601632590606955E-15, -3.437048488108780906E-15, -0.2598076211376265099 ) ) ;
#116026 = CARTESIAN_POINT ( 'NONE',  ( 4.735197965344590365, -1.576124854778211626, 0.7008788178320748408 ) ) ;
#116027 = CARTESIAN_POINT ( 'NONE',  ( 3.977750132953357998, -0.7672935630990398437, 1.865046046545227654 ) ) ;
#116028 = CARTESIAN_POINT ( 'NONE',  ( 5.080843078579284189, -0.8290085517158821693, 2.144167039965215071 ) ) ;
#116029 = CARTESIAN_POINT ( 'NONE',  ( 1.120068590173186163, -2.152398693614396397, 0.4866647226241942459 ) ) ;
#116030 = CARTESIAN_POINT ( 'NONE',  ( -5.655159470675923394, 5.770309935309573923, 0.000000000000000000 ) ) ;
#116031 = CARTESIAN_POINT ( 'NONE',  ( 6.292257686217937795, -1.761477974832075244, -0.1709902323579186867 ) ) ;
#116033 = CARTESIAN_POINT ( 'NONE',  ( 2.361634033267061561, 2.247686861432355077, -0.4490786020208848983 ) ) ;
#116032 = CARTESIAN_POINT ( 'NONE',  ( 6.737475991348287785, 6.825086509519945999, -0.7998128361456481317 ) ) ;
#116034 = CARTESIAN_POINT ( 'NONE',  ( 0.07555271646370392835, -1.686692104669092807, -0.4283695578703243245 ) ) ;
#116035 = CARTESIAN_POINT ( 'NONE',  ( -4.322352044658376968, 3.937165561723182883, 0.7998128361456341429 ) ) ;
#116036 = CARTESIAN_POINT ( 'NONE',  ( 6.474583112218436298, -0.1034247314782872212, -2.189140632845664403 ) ) ;
#116037 = CARTESIAN_POINT ( 'NONE',  ( -6.064239847062411926, 10.29697326487330500, 0.000000000000000000 ) ) ;
#116038 = CARTESIAN_POINT ( 'NONE',  ( -1.360316468750028651, -1.078124999658591765, -4.510281037539698445E-14 ) ) ;
#116039 = CARTESIAN_POINT ( 'NONE',  ( 1.394453263437886604E-15, -2.362500000000000266, 3.474999999999999645 ) ) ;
#116040 = CARTESIAN_POINT ( 'NONE',  ( 0.3093308919281665959, -1.743438469055924145, 1.293836907758689758 ) ) ;
#116041 = CARTESIAN_POINT ( 'NONE',  ( 1.798064920797682653, -0.9548589541341389042, -1.776165177175797583 ) ) ;
#116042 = CARTESIAN_POINT ( 'NONE',  ( 1.499999999999987121, 0.7854166673494828999, 0.8660254037844524744 ) ) ;
#116043 = CARTESIAN_POINT ( 'NONE',  ( 5.268162717194916134, 0.9514403766726580169, 1.675093392909310142 ) ) ;
#116044 = CARTESIAN_POINT ( 'NONE',  ( -8.012344526598182026E-15, 12.29687500034140513, -1.575800808251669460 ) ) ;
#116045 = CARTESIAN_POINT ( 'NONE',  ( 2.531719857061366152, -0.2131849592692437734, 2.211133432850121761 ) ) ;
#116046 = VERTEX_POINT ( 'NONE', #155965 ) ;
#116047 = CARTESIAN_POINT ( 'NONE',  ( 0.4545465019492176406, 7.933486811681471629, -1.993247486878108266 ) ) ;
#116048 = CARTESIAN_POINT ( 'NONE',  ( 3.023105066167310895, 5.702484939155337607, 2.500000000000000444 ) ) ;
#116049 = CARTESIAN_POINT ( 'NONE',  ( 7.892817981449907982, 12.36003807833360391, 0.7998128361456462443 ) ) ;
#116050 = CARTESIAN_POINT ( 'NONE',  ( 1.299038105676669330, 7.500000000000000000, 0.7500000000000006661 ) ) ;
#116051 = CARTESIAN_POINT ( 'NONE',  ( 4.300191697305631777, 1.341742100086223743, -1.108517911846224502 ) ) ;
#116052 = CARTESIAN_POINT ( 'NONE',  ( 3.613678190204441254, 0.4790664972640528707, -1.902336835828049244 ) ) ;
#116054 = CARTESIAN_POINT ( 'NONE',  ( -6.209271165378811297, 10.18797409300986878, 0.7216878364870458196 ) ) ;
#116053 = CARTESIAN_POINT ( 'NONE',  ( 3.486418057008484617, 7.219238166485217434, 1.040834085586084257E-14 ) ) ;
#116055 = CARTESIAN_POINT ( 'NONE',  ( 0.000000000000000000, -0.02379966007286238305, 0.000000000000000000 ) ) ;
#116056 = AXIS2_PLACEMENT_3D ( 'NONE', #15306, #33702, #115025 ) ;
#116057 = CARTESIAN_POINT ( 'NONE',  ( 1.293506021254931193, -1.865543137965872678, 0.8802379953135958113 ) ) ;
#116058 = CARTESIAN_POINT ( 'NONE',  ( -6.184490626128011925, 10.36698949712469364, -0.7998128361456291469 ) ) ;
#116059 = CARTESIAN_POINT ( 'NONE',  ( -3.755245360860931303, 5.404205559136275205, -1.443375672974051449 ) ) ;
#116060 = CARTESIAN_POINT ( 'NONE',  ( 1.552057811931725428, 0.6552935188219483065, -2.165526471026494537 ) ) ;
#116061 = EDGE_LOOP ( 'NONE', ( #189875, #103643, #137646, #58615 ) ) ;
#116062 = CARTESIAN_POINT ( 'NONE',  ( 1.499999999999987121, 0.5770833340161539704, -0.8660254037844253849 ) ) ;
#116063 = CARTESIAN_POINT ( 'NONE',  ( 3.057714436724996876, 1.861869414292870006, -0.1796979844640861634 ) ) ;
#116064 = CARTESIAN_POINT ( 'NONE',  ( 1.424001084297383146, -1.255706242181073851, -1.196294345734474129 ) ) ;
#116065 = CARTESIAN_POINT ( 'NONE',  ( 5.232042516939362287, 2.159042084939459816, 0.3751777721049884273 ) ) ;
#116066 = CARTESIAN_POINT ( 'NONE',  ( 6.212023164884419302, -2.291203086667678690, 0.2740844210103609568 ) ) ;
#116067 = CARTESIAN_POINT ( 'NONE',  ( 1.604443549136617575, -0.7409017435648653782, -1.923293390451373819 ) ) ;
#116068 = CARTESIAN_POINT ( 'NONE',  ( 3.855361883123554989, 1.927135149742021047, -0.2389370807101970084 ) ) ;
#116069 = CARTESIAN_POINT ( 'NONE',  ( -4.243338890952904841, 5.973648010910253880, -1.443375672974051449 ) ) ;
#116070 = CARTESIAN_POINT ( 'NONE',  ( 6.116445839754358182, 1.256427234498383561, -1.385894902050835542 ) ) ;
#116071 = CARTESIAN_POINT ( 'NONE',  ( 1.781250000000001332, 0.7852924748300815772, 1.895863743164048154 ) ) ;
#116072 = DIRECTION ( 'NONE',  ( -0.000000000000000000, -1.000000000000000000, -0.000000000000000000 ) ) ;
#116073 = CARTESIAN_POINT ( 'NONE',  ( 0.2273701076888709205, -1.544753302685021534, -0.7874640570253422789 ) ) ;
#116074 = CARTESIAN_POINT ( 'NONE',  ( -1.360316468750013108, 1.390625000341414008, -3.469446951953614189E-15 ) ) ;
#116075 = CARTESIAN_POINT ( 'NONE',  ( 4.166638809851969327, 1.319227567334404494, 1.525044649537968589 ) ) ;
#116076 = CARTESIAN_POINT ( 'NONE',  ( -9.561524646135538319, 12.17819805862340310, -1.599625672291263179 ) ) ;
#116077 = CARTESIAN_POINT ( 'NONE',  ( 8.289920859751990889, 11.75899253876431416, 1.199719254218450271 ) ) ;
#116078 = CARTESIAN_POINT ( 'NONE',  ( 5.401997860402196316, 5.267028690082820930, 0.000000000000000000 ) ) ;
#116079 = CARTESIAN_POINT ( 'NONE',  ( 2.086296903703276140, -1.790263230197926436, -0.3570169370194844483 ) ) ;
#116080 = CARTESIAN_POINT ( 'NONE',  ( 1.500000000000013545, 5.254166666666685970, 0.8660254037844385966 ) ) ;
#116081 = CARTESIAN_POINT ( 'NONE',  ( -9.587704862635016312, 4.026159954882873926, 6.671158199369250141 ) ) ;
#116082 = VERTEX_POINT ( 'NONE', #203608 ) ;
#116083 = CARTESIAN_POINT ( 'NONE',  ( -5.058600711230246461, 7.955432358860325515, 1.082531754730549967 ) ) ;
#116084 = UNCERTAINTY_MEASURE_WITH_UNIT (LENGTH_MEASURE( 1.000000000000000082E-05 ), #11767, 'distance_accuracy_value', 'NONE');
#116085 = LINE ( 'NONE', #111844, #21497 ) ;
#116086 = CARTESIAN_POINT ( 'NONE',  ( -8.459397779922852578, 11.95671561229694824, 1.199719254218453823 ) ) ;
#116087 = CARTESIAN_POINT ( 'NONE',  ( -0.1755239516839811886, -0.8679694584908944632, -1.822324207963136988 ) ) ;
#116088 = CARTESIAN_POINT ( 'NONE',  ( 6.305373609846285810, 1.934184411435871498, -1.092212275460135773 ) ) ;
#116089 = EDGE_LOOP ( 'NONE', ( #199034, #149488, #69936, #196119 ) ) ;
#116090 = CARTESIAN_POINT ( 'NONE',  ( -7.099629715411508890, 8.311931418515415615, 1.199719254218452047 ) ) ;
#116091 = CARTESIAN_POINT ( 'NONE',  ( 3.655894977179307226, 7.416961240017848844, -0.7998128361456291469 ) ) ;
#116092 = CARTESIAN_POINT ( 'NONE',  ( 6.016494556629995216, 1.386029456380773572, -1.525348796181945854 ) ) ;
#116093 = CARTESIAN_POINT ( 'NONE',  ( 5.133435478496918947, 0.5880181904946504279, 1.928752423557971829 ) ) ;
#116094 = ORIENTED_EDGE ( 'NONE', *, *, #212871, .F. ) ;
#116095 = ORIENTED_EDGE ( 'NONE', *, *, #188915, .F. ) ;
#116096 = CARTESIAN_POINT ( 'NONE',  ( 4.779848517908583894, 4.883929213520019630, -0.7538207499340529028 ) ) ;
#116097 = CARTESIAN_POINT ( 'NONE',  ( 0.9311234436981525864, -1.253119629485603070, 3.474999999999998757 ) ) ;
#116100 = VERTEX_POINT ( 'NONE', #8628 ) ;
#116099 = CARTESIAN_POINT ( 'NONE',  ( -6.966220764712148572, 6.002124920821316323, 2.500000000000000444 ) ) ;
#116098 = CARTESIAN_POINT ( 'NONE',  ( -6.791708605802965870, 6.888357893050385705, -0.7998128361456362523 ) ) ;
#116101 = CARTESIAN_POINT ( 'NONE',  ( 4.941988244637107286, 8.095350367992509177, 1.064974588601754757 ) ) ;
#116102 = CARTESIAN_POINT ( 'NONE',  ( 5.061874962716293780, 1.677747168027879709, -1.117663061872615771 ) ) ;
#116103 = CARTESIAN_POINT ( 'NONE',  ( 4.417794048288587128, 1.130693009273657124, -1.452954439256304520 ) ) ;
#116104 = CARTESIAN_POINT ( 'NONE',  ( 0.07680821025391955381, 7.629137130509078268, -2.410791881123967251 ) ) ;
#116105 = CARTESIAN_POINT ( 'NONE',  ( 2.930630293717914725, 1.281480123180640529, -1.919000982882083095 ) ) ;
#116106 = CARTESIAN_POINT ( 'NONE',  ( 6.587282531393223728, 8.778525268082516320, 1.599625672291268286 ) ) ;
#116107 = CARTESIAN_POINT ( 'NONE',  ( 4.692742333269261934, -0.4685372120167423660, -2.110058259655919422 ) ) ;
#116109 = CARTESIAN_POINT ( 'NONE',  ( 6.958359152311676787, 9.141171649162195934, -1.599625672291262513 ) ) ;
#116108 = CARTESIAN_POINT ( 'NONE',  ( 3.485564796978508184, -0.5807542032013839339, 1.931124776463407189 ) ) ;
#116110 = CARTESIAN_POINT ( 'NONE',  ( 1.610778572542032050, -0.2360344744354908597, 1.927585326284560585 ) ) ;
#116111 = EDGE_CURVE ( 'NONE', #133306, #104840, #157049, .T. ) ;
#116112 = CARTESIAN_POINT ( 'NONE',  ( -4.406563619641430840, 5.099744630125142564, -1.199719254218446718 ) ) ;
#116113 = EDGE_CURVE ( 'NONE', #84148, #213513, #67165, .T. ) ;
#116114 = CARTESIAN_POINT ( 'NONE',  ( 4.095287530520356434, 1.233756528997317137, -1.939045446859017030 ) ) ;
#116115 = DIRECTION ( 'NONE',  ( 0.7384114592165702540, -8.251132798224216436E-15, -0.6743504407188115612 ) ) ;
#116117 = AXIS2_PLACEMENT_3D ( 'NONE', #130113, #164659, #144199 ) ;
#116116 = CARTESIAN_POINT ( 'NONE',  ( -5.978219388983010418, 5.939287140093762574, -0.7998128361456362523 ) ) ;
#116118 = CARTESIAN_POINT ( 'NONE',  ( 2.940157781200231746, 1.856316385841882965, 0.2306766016651334850 ) ) ;
#116119 = VECTOR ( 'NONE', #72470, 1000.000000000000000 ) ;
#116122 = CARTESIAN_POINT ( 'NONE',  ( -6.286140498591554326, 7.362860665558790707, 1.199719254218452047 ) ) ;
#116121 = CARTESIAN_POINT ( 'NONE',  ( -1.364683531250010295, 5.530208333674751842, 0.7879004041258379498 ) ) ;
#116120 = CARTESIAN_POINT ( 'NONE',  ( 1.125099709691119276, 1.687896996356451629, 0.8989547360247207575 ) ) ;
#116123 = B_SPLINE_CURVE_WITH_KNOTS ( 'NONE', 3,
 ( #88844, #174367, #141884, #72561, #40084, #138659 ),
 .UNSPECIFIED., .F., .F.,
 ( 4, 2, 4 ),
 ( 0.000000000000000000, 0.0003778774010236168076, 0.0007557548020472336153 ),
 .UNSPECIFIED. ) ;
#116124 = CARTESIAN_POINT ( 'NONE',  ( 3.264504910713565078, 0.9923201075644829672, 1.971275125648555449 ) ) ;
#116125 = CARTESIAN_POINT ( 'NONE',  ( 1.273556527089495960, 3.289757214169906074, 0.7750000000000135669 ) ) ;
#116126 = CARTESIAN_POINT ( 'NONE',  ( 4.162516854595432747, 4.815023404238158555, 1.199719254218464037 ) ) ;
#116127 = CARTESIAN_POINT ( 'NONE',  ( 5.655159470231527763, 9.611786791996525636, -0.7216878364870458196 ) ) ;
#116128 = CARTESIAN_POINT ( 'NONE',  ( -4.620631424159025613, 4.285158171140619032, -0.7998128361456221525 ) ) ;
#116129 = CARTESIAN_POINT ( 'NONE',  ( -6.360183458142173230, 9.473945563590925545, 1.082531754730549967 ) ) ;
#116130 = CARTESIAN_POINT ( 'NONE',  ( 0.8781228960479293688, -1.098726114091676198, 1.636593336376483743 ) ) ;
#116131 = CARTESIAN_POINT ( 'NONE',  ( 0.6226543773679366067, -1.237902357568532841, -1.947274881911696953 ) ) ;
#116132 = CARTESIAN_POINT ( 'NONE',  ( 1.943732651021431224, 1.350599318427040840, 1.423195245143428433 ) ) ;
#116133 = CARTESIAN_POINT ( 'NONE',  ( 4.961816841544592904, -0.5550570666568316325, 1.986392505239948036 ) ) ;
#116134 = CARTESIAN_POINT ( 'NONE',  ( 5.178851490740193242, 8.025448591630130579, 1.082531754730558626 ) ) ;
#116135 = CARTESIAN_POINT ( 'NONE',  ( 4.993145711582793744, 9.047363440147082159, -0.7998128361456481317 ) ) ;
#116136 = ORIENTED_EDGE ( 'NONE', *, *, #33908, .T. ) ;
#116137 = CARTESIAN_POINT ( 'NONE',  ( 7.063434842595398777, 11.18449838309590483, -0.7216878364870267237 ) ) ;
#116138 = CARTESIAN_POINT ( 'NONE',  ( 1.364683531249988535, 4.967708333674756283, -0.7879004041258300672 ) ) ;
#116139 = CARTESIAN_POINT ( 'NONE',  ( -10.79323443277434791, 4.699918835924045801, -5.141973237006214781 ) ) ;
#116140 = CARTESIAN_POINT ( 'NONE',  ( 4.650083499362880346, 4.527444958785877382, 0.7216878364870317197 ) ) ;
#116141 = CARTESIAN_POINT ( 'NONE',  ( 0.9542540200799983774, -0.7831509020928304476, 2.025049046554725063 ) ) ;
#116143 = CARTESIAN_POINT ( 'NONE',  ( 6.233933901472759942, 1.822226914158030286, 0.2631550708301691466 ) ) ;
#116142 = DIRECTION ( 'NONE',  ( 1.000000000000000000, -0.000000000000000000, 1.224646799147353207E-16 ) ) ;
#116144 = CARTESIAN_POINT ( 'NONE',  ( 11.81911962874431055, 12.34289426515882759, 1.591749704452489533 ) ) ;
#116145 = CARTESIAN_POINT ( 'NONE',  ( -8.673617379884035472E-15, 3.975067388631681187, -1.561251128379126385E-14 ) ) ;
#116146 = CARTESIAN_POINT ( 'NONE',  ( 1.106479506788549116, 1.420293003395491693, -1.217391549091076275 ) ) ;
#116147 = CARTESIAN_POINT ( 'NONE',  ( 5.325516461952285674, -2.054413220456321909, 0.6725034809518318779 ) ) ;
#116148 = CARTESIAN_POINT ( 'NONE',  ( -5.958637689794747949, 6.108898536480521280, 0.7553493914738591553 ) ) ;
#116149 = CARTESIAN_POINT ( 'NONE',  ( -0.02244404828160087226, 6.946777552644228138, -2.784171975256703124 ) ) ;
#116150 = EDGE_CURVE ( 'NONE', #40935, #16236, #87928, .T. ) ;
#116151 = CARTESIAN_POINT ( 'NONE',  ( 6.272253174914359519, 6.990222103910356921, -0.9563742486745248073 ) ) ;
#116152 = CARTESIAN_POINT ( 'NONE',  ( -1.201851678989727383E-14, 5.509375000341415252, -1.575800808251660134 ) ) ;
#116153 = CARTESIAN_POINT ( 'NONE',  ( 1.541514448083292965, -1.800223203088219481, 0.6453159242577054533 ) ) ;
#116154 = CARTESIAN_POINT ( 'NONE',  ( 2.869705036365962858, 0.9450794480442193946, 1.496173807068044148 ) ) ;
#116155 = AXIS2_PLACEMENT_3D ( 'NONE', #57548, #123706, #8785 ) ;
#116156 = CARTESIAN_POINT ( 'NONE',  ( 1.014147342612067737, -1.912461472154961539, 0.0006945104691555297090 ) ) ;
#116158 = CARTESIAN_POINT ( 'NONE',  ( 5.888286034446420736, -0.6943482264498787027, -1.785519067699488982 ) ) ;
#116157 = CARTESIAN_POINT ( 'NONE',  ( 7.047919420689662040, -8.186910006423167019, -6.389500220311202128 ) ) ;
#116159 = CARTESIAN_POINT ( 'NONE',  ( -0.7500000000000006661, -0.8916666666666448471, -1.299038105676652011 ) ) ;
#116160 = CARTESIAN_POINT ( 'NONE',  ( 5.986760398725940568, 1.897641426698594813, 0.5270043353632068994 ) ) ;
#116161 = CARTESIAN_POINT ( 'NONE',  ( 0.9848172835694012361, -1.340914915981223476, 1.642866500755429948 ) ) ;
#116162 = DIRECTION ( 'NONE',  ( -0.000000000000000000, 1.000000000000000000, -0.000000000000000000 ) ) ;
#116163 = CARTESIAN_POINT ( 'NONE',  ( 4.135518821028766112, -1.289757458839156934, -1.355179912160727085 ) ) ;
#116165 = VERTEX_POINT ( 'NONE', #187380 ) ;
#116164 = CARTESIAN_POINT ( 'NONE',  ( 0.2580658466875830337, 0.6954254843183353962, 1.688255465954719536 ) ) ;
#116167 = CARTESIAN_POINT ( 'NONE',  ( 4.644395130292630292, 8.311692339142366492, -0.4369040224408097250 ) ) ;
#116166 = CARTESIAN_POINT ( 'NONE',  ( 2.965657822035951963, 0.3232568108629539361, -2.182957019552448141 ) ) ;
#116168 = CARTESIAN_POINT ( 'NONE',  ( -0.6823417656250212460, 4.863541667008086655, 1.181850606188767472 ) ) ;
#116169 = CARTESIAN_POINT ( 'NONE',  ( 1.979039114045421988, 1.923815945824264073, 0.7444423131674202665 ) ) ;
#116170 = CARTESIAN_POINT ( 'NONE',  ( 6.257251587906815793, 7.258880593101466161, 1.199719254218462483 ) ) ;
#116171 = CARTESIAN_POINT ( 'NONE',  ( -9.989660255170729641, 10.54902514065433827, -0.7998128361456291469 ) ) ;
#116172 = CARTESIAN_POINT ( 'NONE',  ( -4.778319401024116786, 15.44696626029461939, -10.96850100116969351 ) ) ;
#116173 = CARTESIAN_POINT ( 'NONE',  ( -3.451466477441916147, -0.01064274562824485404, -0.2975466414532820791 ) ) ;
#116174 = MECHANICAL_DESIGN_GEOMETRIC_PRESENTATION_REPRESENTATION (  '', ( #50392 ), #136840 ) ;
#116175 = CARTESIAN_POINT ( 'NONE',  ( -3.945059511896602089, 7.546393830613923548, 1.040834085586084257E-14 ) ) ;
#116176 = VERTEX_POINT ( 'NONE', #122487 ) ;
#116177 = CARTESIAN_POINT ( 'NONE',  ( 4.316890830952234914, -1.536253448065309613, 1.388129241271539138 ) ) ;
#116178 = CARTESIAN_POINT ( 'NONE',  ( 0.7499999999999902300, 5.566666666666685082, -1.299038105676658228 ) ) ;
#116179 = CARTESIAN_POINT ( 'NONE',  ( 1.634274655659254005, 1.066924998833935989, -1.879885089102695250 ) ) ;
#116180 = CARTESIAN_POINT ( 'NONE',  ( -5.717536675473545493, 7.305230138711669596, -1.214019596050613492 ) ) ;
#116181 = CARTESIAN_POINT ( 'NONE',  ( 2.543622981932230243, -1.883669348803659549, 0.7290701893776069253 ) ) ;
#116182 = CARTESIAN_POINT ( 'NONE',  ( 3.469446951953614189E-15, 0.2401923788623722134, 6.938893903907228378E-15 ) ) ;
#116183 = ORIENTED_EDGE ( 'NONE', *, *, #181109, .F. ) ;
#116184 = AXIS2_PLACEMENT_3D ( 'NONE', #76333, #62225, #42798 ) ;
#116185 = ADVANCED_FACE ( 'NONE', ( #25943 ), #42957, .T. ) ;
#116187 = CARTESIAN_POINT ( 'NONE',  ( 8.324343129110697959, 9.774450407793066731, -1.082531754730543083 ) ) ;
#116186 = CARTESIAN_POINT ( 'NONE',  ( -1.737499999999997824, -3.091666666666666341, 3.009438278150925683 ) ) ;
#116188 = DIRECTION ( 'NONE',  ( 0.000000000000000000, 1.000000000000000000, 0.000000000000000000 ) ) ;
#116189 = CARTESIAN_POINT ( 'NONE',  ( 6.509000000000050967, 0.007656933339270000430, 1.900274884395843022 ) ) ;
#116190 = CARTESIAN_POINT ( 'NONE',  ( 6.639320575229294086, 2.013432609116216021, 2.506292271646192393 ) ) ;
#116191 = CARTESIAN_POINT ( 'NONE',  ( 4.827760788416924242, 1.126602223531171898, -1.879657820484957664 ) ) ;
#116192 = CARTESIAN_POINT ( 'NONE',  ( -1.201851678989727383E-14, 3.618750000682816381, -1.732050807568863648 ) ) ;
#116193 = CARTESIAN_POINT ( 'NONE',  ( 3.252119977711815491, 0.8557668478980616777, -1.710280963351323846 ) ) ;
#116194 = CARTESIAN_POINT ( 'NONE',  ( -4.069418662396130593, 7.899405539437467816, -0.7998128361456281477 ) ) ;
#116195 = CARTESIAN_POINT ( 'NONE',  ( 3.185802909086945967, 5.700225246367978116, 1.082531754730546636 ) ) ;
#116197 = CARTESIAN_POINT ( 'NONE',  ( 1.827750133516142128, 0.7691037069590834774, -1.864176919362303675 ) ) ;
#116196 = DIRECTION ( 'NONE',  ( 1.000000000000000000, 0.000000000000000000, 0.000000000000000000 ) ) ;
#116198 = CARTESIAN_POINT ( 'NONE',  ( -1.402160292154681736E-14, 12.48437500034139624, 1.575800808251682339 ) ) ;
#116200 = CARTESIAN_POINT ( 'NONE',  ( -6.330731382938325602, 6.350551133041632212, 0.7998128361456281477 ) ) ;
#116199 = CARTESIAN_POINT ( 'NONE',  ( 0.6973257247198815234, 1.878305535369644064, 1.313909787900492843 ) ) ;
#116201 = CARTESIAN_POINT ( 'NONE',  ( 3.908989539853875428, 1.479446464633243474, 0.8863536201247077528 ) ) ;
#116202 = CARTESIAN_POINT ( 'NONE',  ( 8.025500584646550806, 8.327781868367935658, 0.000000000000000000 ) ) ;
#116203 = CARTESIAN_POINT ( 'NONE',  ( 3.009020027229115879, 5.597941567487558778, -1.199719254218446718 ) ) ;
#116204 = CARTESIAN_POINT ( 'NONE',  ( 0.000000000000000000, 5.499999999999998224, -2.000000000000000000 ) ) ;
#116205 = CARTESIAN_POINT ( 'NONE',  ( 1.275752070009423367, -1.914805681740685106, 0.4264308320794732432 ) ) ;
#116206 = EDGE_CURVE ( 'NONE', #180856, #209493, #59513, .T. ) ;
#116207 = CARTESIAN_POINT ( 'NONE',  ( -1.500000000000021982, 7.809273069926255140, 3.635729725621167141 ) ) ;
#116208 = CARTESIAN_POINT ( 'NONE',  ( 5.854423403002611437, 5.724582146458163656, 1.040834085586084257E-14 ) ) ;
#116209 = CARTESIAN_POINT ( 'NONE',  ( 0.07516593201273635838, 0.7223771927552320449, -2.128525933252373381 ) ) ;
#116210 = ORIENTED_EDGE ( 'NONE', *, *, #52332, .F. ) ;
#116211 = CARTESIAN_POINT ( 'NONE',  ( 0.3915760470782835290, -1.894197279051227589, 0.8358220917567968922 ) ) ;
#116212 = ORIENTED_EDGE ( 'NONE', *, *, #189930, .T. ) ;
#116213 = CARTESIAN_POINT ( 'NONE',  ( 4.758376837038695406, 1.806999933331495445, 0.1280191873242030876 ) ) ;
#116214 = VERTEX_POINT ( 'NONE', #175421 ) ;
#116215 = CARTESIAN_POINT ( 'NONE',  ( 6.638652492546827766, 7.774124658506663010, 1.199719254218452047 ) ) ;
#116216 = CARTESIAN_POINT ( 'NONE',  ( 5.619718922174004483, -0.4339147374951453084, 1.758609293272636487 ) ) ;
#116217 = CARTESIAN_POINT ( 'NONE',  ( 5.492461626867537916, 9.421972641405202964, -0.7216878364870458196 ) ) ;
#116218 = DIRECTION ( 'NONE',  ( 0.000000000000000000, -0.7999999999999973799, 0.6000000000000034195 ) ) ;
#116219 = CARTESIAN_POINT ( 'NONE',  ( 5.863316726098953602, 5.994608360591326068, -0.2888550730815123702 ) ) ;
#116221 = CARTESIAN_POINT ( 'NONE',  ( 9.622536337397022521, 12.24937836509514710, 1.599625672291281386 ) ) ;
#116220 = CARTESIAN_POINT ( 'NONE',  ( 6.461375281700972195, 1.547960615844719667, 1.032782510450443114 ) ) ;
#116222 = CARTESIAN_POINT ( 'NONE',  ( 4.060093344861609665, -1.099912525845229583, 1.568156085375242093 ) ) ;
#116223 = CARTESIAN_POINT ( 'NONE',  ( -6.598949805828081772, -8.057948861126607909, -6.880414557363810246 ) ) ;
#116224 = CARTESIAN_POINT ( 'NONE',  ( 11.35610322553117513, 13.61421628929173266, 3.553412924323500643 ) ) ;
#116225 = CARTESIAN_POINT ( 'NONE',  ( 6.480434237652132445, 7.623223367758051872, 1.082531754730558626 ) ) ;
#116226 = EDGE_CURVE ( 'NONE', #59934, #2638, #49884, .T. ) ;
#116228 = CARTESIAN_POINT ( 'NONE',  ( 5.682842148387160286, 1.729519065878544426, -1.221158300678204300 ) ) ;
#116227 = CARTESIAN_POINT ( 'NONE',  ( -9.991996023591624976, 10.75967623705280296, 1.040834085586084257E-14 ) ) ;
#116229 = CARTESIAN_POINT ( 'NONE',  ( 0.9542513359644848592, 2.159166806557303531, -0.1069676271590186134 ) ) ;
#116230 = CARTESIAN_POINT ( 'NONE',  ( -6.283277845290492714, 6.295188672452495915, -0.7998128361456362523 ) ) ;
#116231 = CARTESIAN_POINT ( 'NONE',  ( 5.890091390494168522, 5.836471141856793388, 0.000000000000000000 ) ) ;
#116232 = CARTESIAN_POINT ( 'NONE',  ( 0.5514207423844892375, 0.5776932562693118944, -1.731835939664846613 ) ) ;
#116233 = CARTESIAN_POINT ( 'NONE',  ( -3.253066792275140173, 5.882662793374543675, 1.199719254218462483 ) ) ;
#116234 = EDGE_CURVE ( 'NONE', #63041, #197916, #198602, .T. ) ;
#116235 = CARTESIAN_POINT ( 'NONE',  ( 3.786012796616508247, -0.9002957760516903107, 1.588078298607284111 ) ) ;
#116236 = CARTESIAN_POINT ( 'NONE',  ( 9.710969956560674632, 13.29837910982962690, -8.127984515541683663 ) ) ;
#116237 = ORIENTED_EDGE ( 'NONE', *, *, #66344, .F. ) ;
#116238 = CARTESIAN_POINT ( 'NONE',  ( 2.717198260794476017, -1.712298780928861008, -0.9731099088599747260 ) ) ;
#116239 = ORIENTED_EDGE ( 'NONE', *, *, #46969, .T. ) ;
#116240 = CARTESIAN_POINT ( 'NONE',  ( 4.388185931656235717, -0.4287674410733510744, -1.893983405979382306 ) ) ;
#116241 = CARTESIAN_POINT ( 'NONE',  ( -3.006876207180748217, 6.730049018344652190, -0.7998128361456481317 ) ) ;
#116243 = CARTESIAN_POINT ( 'NONE',  ( 4.869442314738527067, -1.792836814666173062, -1.132239877606910472 ) ) ;
#116242 = CARTESIAN_POINT ( 'NONE',  ( 6.505933609711257226, 8.683618192786854095, -1.599625672291281386 ) ) ;
#116244 = CARTESIAN_POINT ( 'NONE',  ( -3.659182332138577465E-15, -7.246166700193014343, 9.579665964947889023 ) ) ;
#116245 = CARTESIAN_POINT ( 'NONE',  ( 2.807167725247063483, 1.639017566557477990, -0.9848878580655600068 ) ) ;
#116246 = CARTESIAN_POINT ( 'NONE',  ( 6.075519867480115188, 6.040327746143013599, 0.3625371965378897388 ) ) ;
#116247 = DIRECTION ( 'NONE',  ( -0.000000000000000000, 1.000000000000000000, 9.023263958591317418E-17 ) ) ;
#116248 = VERTEX_POINT ( 'NONE', #95247 ) ;
#116249 = CARTESIAN_POINT ( 'NONE',  ( -1.364683531250014514, 12.83854166700806410, -0.7879004041258335089 ) ) ;
#116250 = CARTESIAN_POINT ( 'NONE',  ( 3.217027588192558074, 6.975225629525113824, -1.734723475976807094E-15 ) ) ;
#116251 = CARTESIAN_POINT ( 'NONE',  ( 3.472859903394816872, 7.203420320602605287, -0.7998128361456291469 ) ) ;
#116252 = CARTESIAN_POINT ( 'NONE',  ( -0.4525991836887841013, 2.827044806229560336, 1.949989785391225361 ) ) ;
#116253 = CARTESIAN_POINT ( 'NONE',  ( 4.846238042176662653, 1.821038859956089606, 0.1311717439725426648 ) ) ;
#116254 = CARTESIAN_POINT ( 'NONE',  ( 0.000000000000000000, 18.91999999999999815, 11.09999999999999964 ) ) ;
#116255 = CARTESIAN_POINT ( 'NONE',  ( -9.503902493499651882, 10.19023378527882784, 1.040834085586084257E-14 ) ) ;
#116256 = CARTESIAN_POINT ( 'NONE',  ( -6.279577920751266973, 6.982973266031838655, 0.9645283542769074181 ) ) ;
#116257 = PLANE ( 'NONE',  #191803 ) ;
#116258 = CARTESIAN_POINT ( 'NONE',  ( 5.155093292349416600, -1.580716073637401076, -1.000049079914612449 ) ) ;
#116259 = CARTESIAN_POINT ( 'NONE',  ( 6.588372581236919601, 9.773852880496709972, -1.199719254218440723 ) ) ;
#116260 = CARTESIAN_POINT ( 'NONE',  ( -5.596818484342970912, 5.424043074688561283, -0.7998128361456221525 ) ) ;
#116261 = CARTESIAN_POINT ( 'NONE',  ( -1.402160292154681736E-14, 10.48437500034139447, 1.575800808251682339 ) ) ;
#116262 = CARTESIAN_POINT ( 'NONE',  ( -6.098470168048611306, 6.009303372345148553, 1.040834085586084257E-14 ) ) ;
#116263 = CARTESIAN_POINT ( 'NONE',  ( 4.369805582306193870, 3.992528022312320957, 1.214306433183764966E-14 ) ) ;
#116264 = CARTESIAN_POINT ( 'NONE',  ( -3.472296738431328134, 7.065113604896248845, 0.000000000000000000 ) ) ;
#116265 = CARTESIAN_POINT ( 'NONE',  ( -6.240830780992103755, 6.175390754112560110, 1.040834085586084257E-14 ) ) ;
#116266 = CARTESIAN_POINT ( 'NONE',  ( 0.3388458784313007066, -2.007247006727829852, -0.5063607812752639603 ) ) ;
#116267 =( BOUNDED_SURFACE ( )  B_SPLINE_SURFACE ( 3, 3, ( 
 ( #2113, #183027, #201386, #200325, #153737, #133253, #187289, #101782, #166790, #199259 ),
 ( #119157, #21558, #167849, #19448, #85524, #5304, #20512, #55169, #137498, #121314 ),
 ( #185141, #4247, #151613, #53024, #3180, #86597, #69251, #36767, #102853, #168909 ),
 ( #152663, #39991, #106100, #191541, #126641, #26912, #76730, #172122, #205663, #155870 ),
 ( #204583, #159062, #122394, #175329, #60483, #9603, #207795, #188351, #75681, #140721 ),
 ( #89823, #192606, #24782, #154802, #141791, #59423, #57300, #10658, #189427, #23716 ),
 ( #104999, #7460, #109320, #171039, #74616, #6389, #73539, #139640, #90885, #8535 ) ),
 .UNSPECIFIED., .T., .F., .T. ) 
 B_SPLINE_SURFACE_WITH_KNOTS ( ( 4, 3, 4 ),
 ( 4, 1, 1, 1, 1, 1, 1, 4 ),
 ( 0.000000000000000000, 0.5000000000000000000, 1.000000000000000000 ),
 ( 0.000000000000000000, 0.09487947018404768729, 0.1878442364269655440, 0.2584026419818104547, 0.3617053504666527530, 0.5211417612611924932, 0.7337075935910832847, 1.000000000000000000 ),
 .UNSPECIFIED. ) 
 GEOMETRIC_REPRESENTATION_ITEM ( )  RATIONAL_B_SPLINE_SURFACE ( (
 ( 1.000000000000000000, 1.000000000000000000, 1.000000000000000000, 0.9999999999999996669, 1.000000000000000222, 1.000000000000000000, 1.000000000000000222, 0.9999999999999997780, 1.000000000000000000, 1.000000000000000000),
 ( 0.3333333333333333703, 0.3333333333333333703, 0.3333333333333334259, 0.3333333333333332593, 0.3333333333333334814, 0.3333333333333333148, 0.3333333333333334259, 0.3333333333333333148, 0.3333333333333333703, 0.3333333333333333703),
 ( 0.3333333333333333703, 0.3333333333333333703, 0.3333333333333334259, 0.3333333333333332593, 0.3333333333333334814, 0.3333333333333333148, 0.3333333333333334259, 0.3333333333333333148, 0.3333333333333333703, 0.3333333333333333703),
 ( 1.000000000000000000, 1.000000000000000000, 1.000000000000000000, 0.9999999999999996669, 1.000000000000000222, 1.000000000000000000, 1.000000000000000222, 0.9999999999999997780, 1.000000000000000000, 1.000000000000000000),
 ( 0.3333333333333333703, 0.3333333333333333703, 0.3333333333333334259, 0.3333333333333332593, 0.3333333333333334814, 0.3333333333333333148, 0.3333333333333334259, 0.3333333333333333148, 0.3333333333333333703, 0.3333333333333333703),
 ( 0.3333333333333333703, 0.3333333333333333703, 0.3333333333333334259, 0.3333333333333332593, 0.3333333333333334814, 0.3333333333333333148, 0.3333333333333334259, 0.3333333333333333148, 0.3333333333333333703, 0.3333333333333333703),
 ( 1.000000000000000000, 1.000000000000000000, 1.000000000000000000, 0.9999999999999996669, 1.000000000000000222, 1.000000000000000000, 1.000000000000000222, 0.9999999999999997780, 1.000000000000000000, 1.000000000000000000) ) ) 
 REPRESENTATION_ITEM ( '' )  SURFACE ( )  );
#116268 = CARTESIAN_POINT ( 'NONE',  ( 2.777094422528699535, 1.814377389300044330, -1.091000554854235638 ) ) ;
#116269 = AXIS2_PLACEMENT_3D ( 'NONE', #53411, #116342, #119548 ) ;
#116270 = CARTESIAN_POINT ( 'NONE',  ( 8.860417081730671995, 10.29590700256267155, 1.199719254218453823 ) ) ;
#116271 = CARTESIAN_POINT ( 'NONE',  ( -3.614985261929179128, 3.508924507031892848, 2.500000000000000000 ) ) ;
#116272 = CARTESIAN_POINT ( 'NONE',  ( 6.350451050988413115, -2.059726887988411637, -0.2088473404622398499 ) ) ;
#116273 = CARTESIAN_POINT ( 'NONE',  ( 4.626207451132414938, 6.895778996938287442, -1.211788453915439989 ) ) ;
#116274 = CARTESIAN_POINT ( 'NONE',  ( 4.690757960648213931, 8.416375354157496602, 0.7216878364870438212 ) ) ;
#116275 = CARTESIAN_POINT ( 'NONE',  ( -3.475000000000000533, -2.829166666666666607, -2.006292185433948827 ) ) ;
#116276 = CARTESIAN_POINT ( 'NONE',  ( 2.098001248608129199, -2.291667096838309270, 0.05881920129262825647 ) ) ;
#116278 = DIRECTION ( 'NONE',  ( 5.176899690512889973E-31, -0.5999999999999999778, 0.8000000000000000444 ) ) ;
#116277 = CARTESIAN_POINT ( 'NONE',  ( 0.09986456629675066754, -1.825204794925545881, -0.04862044751281074939 ) ) ;
#116279 = CARTESIAN_POINT ( 'NONE',  ( 2.179812656587180264, 1.874749209517186710, -0.3766967574026017229 ) ) ;
#116280 = EDGE_LOOP ( 'NONE', ( #161293, #196342, #157722, #154065 ) ) ;
#116281 = CARTESIAN_POINT ( 'NONE',  ( 7.578644679914713578, 8.904468883731073703, 1.082531754730558626 ) ) ;
#116282 = CARTESIAN_POINT ( 'NONE',  ( 0.1057268774627964369, 1.494660468187744229, 1.348908602934977496 ) ) ;
#116283 = CARTESIAN_POINT ( 'NONE',  ( 1.094497266827038962, 1.931770780797737341, 0.3408682529649207926 ) ) ;
#116284 = CARTESIAN_POINT ( 'NONE',  ( -0.6124999999999984901, 2.770833334016134408, -1.060881119635941339 ) ) ;
#116285 = CARTESIAN_POINT ( 'NONE',  ( -7.853197290813634268, 10.18514947741448573, 1.599625672291295375 ) ) ;
#116286 = CARTESIAN_POINT ( 'NONE',  ( -6.337068562759858636, 6.936200024879327408, -0.9492287992594623525 ) ) ;
#116288 = CARTESIAN_POINT ( 'NONE',  ( 2.641160111863867233, -1.309778345111691999, -1.190485388269453049 ) ) ;
#116287 = CARTESIAN_POINT ( 'NONE',  ( 3.785173937466048244, 1.514314676582936947, 1.441642292586094110 ) ) ;
#116289 = FACE_OUTER_BOUND ( 'NONE', #71826, .T. ) ;
#116291 = CARTESIAN_POINT ( 'NONE',  ( 5.103627735775233987, -2.281604237428825233, 0.2209099425345140144 ) ) ;
#116290 = CARTESIAN_POINT ( 'NONE',  ( 0.007772928215642942867, 8.279395425053875712, 2.079985476292312008 ) ) ;
#116292 = CARTESIAN_POINT ( 'NONE',  ( 2.782837888936703585, 1.230821076073612463, 1.230640916823136255 ) ) ;
#116293 = CARTESIAN_POINT ( 'NONE',  ( 2.218730694130720771, 5.740269576461138890, 0.7998128361456462443 ) ) ;
#116294 = CARTESIAN_POINT ( 'NONE',  ( 3.888156192069020634, 7.758209000714329839, 1.040834085586084257E-14 ) ) ;
#116295 = CARTESIAN_POINT ( 'NONE',  ( 2.881899232214884865, -0.1729783253755692307, 1.725191050717300945 ) ) ;
#116296 = CARTESIAN_POINT ( 'NONE',  ( 3.807220332926362083, -1.777014928589750076, 1.247251757893479640 ) ) ;
#116297 = CARTESIAN_POINT ( 'NONE',  ( 3.337278367258157630, 7.045241861776501580, 0.7998128361456341429 ) ) ;
#116298 = CARTESIAN_POINT ( 'NONE',  ( 5.173064673083394460, 1.776168143800487043, -0.9548534231369476544 ) ) ;
#116300 = AXIS2_PLACEMENT_3D ( 'NONE', #144894, #81973, #210902 ) ;
#116299 = CARTESIAN_POINT ( 'NONE',  ( 0.1562501595635738816, -1.895867669153105339, 0.7852924748299968671 ) ) ;
#116301 = CARTESIAN_POINT ( 'NONE',  ( 0.7499999999999920064, 4.764583334016150751, 1.299038105676669330 ) ) ;
#116302 = CARTESIAN_POINT ( 'NONE',  ( 2.485270279442112429, 1.762041721199611333, -0.7789696210150058864 ) ) ;
#116303 = CARTESIAN_POINT ( 'NONE',  ( -1.500000000000001110, 8.302083334016129967, 0.8660254037844419273 ) ) ;
#116304 = CARTESIAN_POINT ( 'NONE',  ( 5.607756438734910809, 1.682095628590657643, 1.451081198120441229 ) ) ;
#116305 = ORIENTED_EDGE ( 'NONE', *, *, #196046, .F. ) ;
#116306 = CARTESIAN_POINT ( 'NONE',  ( 6.983263157960398537, 3.691045885609476773, 2.560325512483021981 ) ) ;
#116307 = CARTESIAN_POINT ( 'NONE',  ( 0.7499999999999902300, 1.483333333333357373, 1.299038105676657340 ) ) ;
#116308 = CARTESIAN_POINT ( 'NONE',  ( 5.777746017718023097, 9.892454120646377191, 0.7998128361456462443 ) ) ;
#116309 = CARTESIAN_POINT ( 'NONE',  ( 4.080641047588898118, 5.783833860318930320, -1.443375672974051449 ) ) ;
#116310 = CARTESIAN_POINT ( 'NONE',  ( 6.654749070045313353, -0.5220710138904552933, -1.891073168474053823 ) ) ;
#116311 = CARTESIAN_POINT ( 'NONE',  ( 9.246297574839983824, 9.889694713509232571, 0.7216878364870438212 ) ) ;
#116312 = CARTESIAN_POINT ( 'NONE',  ( 0.2032326336602353622, 3.360045134790890842, 2.069225858299823084 ) ) ;
#116313 = VECTOR ( 'NONE', #163621, 1000.000000000000000 ) ;
#116314 = CARTESIAN_POINT ( 'NONE',  ( 4.420840606507738357, 7.315341919971147355, 1.199719254218451159 ) ) ;
#116315 = CARTESIAN_POINT ( 'NONE',  ( -5.167065940583949413, 5.200867483535597913, 0.000000000000000000 ) ) ;
#116316 = CARTESIAN_POINT ( 'NONE',  ( 4.264169596968480747, -2.057349986699669397, 0.1488187104187361498 ) ) ;
#116317 = CARTESIAN_POINT ( 'NONE',  ( -4.229253852459088137, 7.021547696922494808, 1.199719254218464037 ) ) ;
#116318 = CARTESIAN_POINT ( 'NONE',  ( -1.500000000000013101, 3.410416667349487785, -0.8660254037844313801 ) ) ;
#116319 = CARTESIAN_POINT ( 'NONE',  ( -1.402160292154681736E-14, -0.6781249996585819728, 1.575800808251672791 ) ) ;
#116320 = CARTESIAN_POINT ( 'NONE',  ( 6.098880659294531270, 1.529360415809786433, -1.076766019972655197 ) ) ;
#116321 = CARTESIAN_POINT ( 'NONE',  ( 4.377415392590312315, -0.3859441149459389431, -1.690453949067998840 ) ) ;
#116322 = CARTESIAN_POINT ( 'NONE',  ( 3.948569229637605815, -1.449640539659799776, -0.9628182713226125511 ) ) ;
#116323 = CARTESIAN_POINT ( 'NONE',  ( 4.416205349749311004, 6.175325546172740765, 1.599625672291267398 ) ) ;
#116324 = CARTESIAN_POINT ( 'NONE',  ( 1.541004877621090507, -1.933652123512133114, 1.230999918854805975 ) ) ;
#116325 = CARTESIAN_POINT ( 'NONE',  ( 1.364683531249990311, 5.176041667008085767, 0.7879004041258500513 ) ) ;
#116326 = CARTESIAN_POINT ( 'NONE',  ( 5.618719695961268634, -0.05021595884377753893, 2.090305304898040006 ) ) ;
#116327 = CARTESIAN_POINT ( 'NONE',  ( 0.6031360380127914755, -1.832534659106283659, 0.1778487281504093076 ) ) ;
#116328 = VECTOR ( 'NONE', #15713, 1000.000000000000000 ) ;
#116329 = DIRECTION ( 'NONE',  ( 0.6095094443605824086, -2.582722057095079198E-12, -0.7927788072566358535 ) ) ;
#116330 =( LENGTH_UNIT ( ) NAMED_UNIT ( * ) SI_UNIT ( .MILLI., .METRE. ) );
#116331 = CARTESIAN_POINT ( 'NONE',  ( 1.494767762416524093, -2.000856930885573259, 0.2496086726550551249 ) ) ;
#116332 = CARTESIAN_POINT ( 'NONE',  ( 0.5334774086375413393, -1.552487152004313087, -1.546944964277228607 ) ) ;
#116333 = CARTESIAN_POINT ( 'NONE',  ( 8.305220197644215929, 14.86737089724833893, -9.585679967850639471 ) ) ;
#116334 = CARTESIAN_POINT ( 'NONE',  ( -8.376239975144482486, 8.666701480623698828, 1.040834085586084257E-14 ) ) ;
#116335 = CARTESIAN_POINT ( 'NONE',  ( 5.789495288235341874, 6.713164910151406595, 1.199719254218462483 ) ) ;
#116336 = CARTESIAN_POINT ( 'NONE',  ( 1.360316468749949825, 1.994791667008131597, 0.7853790794158701516 ) ) ;
#116337 = CARTESIAN_POINT ( 'NONE',  ( 3.000754678503589012, -2.089479603458433754, -0.3603616953608209661 ) ) ;
#116338 = CARTESIAN_POINT ( 'NONE',  ( 1.364683531249986537, -0.09479166632524321789, -0.7879004041258309554 ) ) ;
#116339 = CARTESIAN_POINT ( 'NONE',  ( 5.619710272201024814, -1.780234218580947436, 0.4041525643716862848 ) ) ;
#116340 = EDGE_LOOP ( 'NONE', ( #183171, #158142, #109566, #61805 ) ) ;
#116341 = CARTESIAN_POINT ( 'NONE',  ( -4.959250327548641479, 9.007818825440551791, -0.7998128361456362523 ) ) ;
#116342 = DIRECTION ( 'NONE',  ( 0.000000000000000000, 1.000000000000000000, 0.000000000000000000 ) ) ;
#116343 = CARTESIAN_POINT ( 'NONE',  ( 1.001543065824772753E-15, -3.718749999044085097, 4.012584370867899430 ) ) ;
#116344 = CARTESIAN_POINT ( 'NONE',  ( -5.856232286098998152, 8.919689202835742847, 1.199719254218452047 ) ) ;
#116345 = CARTESIAN_POINT ( 'NONE',  ( 3.814717077619066643, -0.6377016420256261808, -1.916516432535425363 ) ) ;
#116346 = CARTESIAN_POINT ( 'NONE',  ( 6.440462174652990868, 2.181831651002089423, 0.3301269925025315799 ) ) ;
#116347 = EDGE_CURVE ( 'NONE', #30182, #62722, #150237, .T. ) ;
#116348 = CARTESIAN_POINT ( 'NONE',  ( 10.37606763316019531, 10.99983374830873650, 0.7998128361456462443 ) ) ;
#116349 = CARTESIAN_POINT ( 'NONE',  ( 4.363987150452108388, -1.856190122274929077, 0.1334137851533196695 ) ) ;
#116350 = CARTESIAN_POINT ( 'NONE',  ( 9.673906298550626559, 11.24497775551929557, 1.199719254218452047 ) ) ;
#116351 = CARTESIAN_POINT ( 'NONE',  ( 11.96217875511318063, 13.82854366578976624, -0.9561995067075083066 ) ) ;
#116352 = CARTESIAN_POINT ( 'NONE',  ( -3.358669367883384105, 4.941533567329135401, -1.599625672291262513 ) ) ;
#116353 =( BOUNDED_CURVE ( )  B_SPLINE_CURVE ( 2, ( #124191, #103586, #87332, #186952, #72123 ),
 .UNSPECIFIED., .F., .T. ) 
 B_SPLINE_CURVE_WITH_KNOTS ( ( 3, 2, 3 ),
 ( 0.5000000000000000000, 0.5083333333333333037, 0.5121012724118086945 ),
 .UNSPECIFIED. ) 
 CURVE ( )  GEOMETRIC_REPRESENTATION_ITEM ( )  RATIONAL_B_SPLINE_CURVE ( ( 1.000000000000000000, 0.8660254037844387076, 1.000000000000000000, 0.9394230260075716599, 0.9336261354299888460 ) ) 
 REPRESENTATION_ITEM ( '' )  );
#116354 = CARTESIAN_POINT ( 'NONE',  ( -6.808165692356648258, 11.09461040772476714, 0.7998128361456481317 ) ) ;
#116355 = CARTESIAN_POINT ( 'NONE',  ( 6.245006310359877411, -1.742422335079217843, 1.100243706638550423 ) ) ;
#116357 = CARTESIAN_POINT ( 'NONE',  ( -4.232483270035822365, 7.525443216328503659, 1.020073867034466675 ) ) ;
#116356 = CARTESIAN_POINT ( 'NONE',  ( -7.259464905474441565, 7.434073576000447048, -0.7998128361456362523 ) ) ;
#116358 = CARTESIAN_POINT ( 'NONE',  ( 1.364683531249986537, -0.09479166632524321789, -0.7879004041258309554 ) ) ;
#116359 = CARTESIAN_POINT ( 'NONE',  ( 1.194254265631944367, -1.094737682603286189, -1.344534739289292569 ) ) ;
#116360 = CARTESIAN_POINT ( 'NONE',  ( 1.657743431332364681, -1.232332549506355290, 1.229129442381997395 ) ) ;
#116362 = CARTESIAN_POINT ( 'NONE',  ( 9.259855728453651125, 9.905512559391842942, 1.040834085586084257E-14 ) ) ;
#116361 = CARTESIAN_POINT ( 'NONE',  ( 6.287736656369789401, 1.586309881779718323, 1.676255113901073512 ) ) ;
#116363 = CARTESIAN_POINT ( 'NONE',  ( 4.686278372178935392, 5.496354851410763409, 1.199719254218452047 ) ) ;
#116364 = CARTESIAN_POINT ( 'NONE',  ( 1.511086176359067501, 1.816151333767004772, 0.9739060079534812564 ) ) ;
#116365 = CARTESIAN_POINT ( 'NONE',  ( 4.008406971134620633, 7.828225232965717595, 0.7998128361456321445 ) ) ;
#116366 = EDGE_CURVE ( 'NONE', #179068, #45871, #202889, .T. ) ;
#116367 = ADVANCED_FACE ( 'NONE', ( #110475 ), #192699, .T. ) ;
#116368 = CARTESIAN_POINT ( 'NONE',  ( 6.397888825007291835, 0.2158721846312293136, 2.288236095241158452 ) ) ;
#116369 = CARTESIAN_POINT ( 'NONE',  ( -10.17567228521070710, -0.02076350362892331880, 2.419999999999999485 ) ) ;
#116370 = CARTESIAN_POINT ( 'NONE',  ( -5.529746549527323474, 7.544733289238903851, -1.599625672291271394 ) ) ;
#116371 = CARTESIAN_POINT ( 'NONE',  ( 6.368025811218641863, 0.9635043244729593059, 1.603280169136585220 ) ) ;
#116373 = CARTESIAN_POINT ( 'NONE',  ( -7.132998214565509087, 7.494455136514109661, 0.7216878364870317197 ) ) ;
#116372 = CARTESIAN_POINT ( 'NONE',  ( 4.166199421025416960, 1.911861072351704882, -0.05224187775455800542 ) ) ;
#116374 = CARTESIAN_POINT ( 'NONE',  ( 6.621690180768193379, -2.141820631849135292, 0.5315211216728524812 ) ) ;
#116375 = CARTESIAN_POINT ( 'NONE',  ( -6.197485614778184271, 9.284131412999601096, 1.082531754730549967 ) ) ;
#116376 = CARTESIAN_POINT ( 'NONE',  ( 6.688968683495743583, 8.897159112202094988, -1.599625672291283607 ) ) ;
#116377 = CARTESIAN_POINT ( 'NONE',  ( -6.474900878978163021, 9.711745571186627402, -1.199719254218452047 ) ) ;
#116378 = CARTESIAN_POINT ( 'NONE',  ( 6.498696114369957755, -2.079444522786470184, -0.4142970760486197612 ) ) ;
#116379 = VERTEX_POINT ( 'NONE', #45422 ) ;
#116380 = CARTESIAN_POINT ( 'NONE',  ( 3.013035845080668906, 1.672340031372629321, -1.590277441748239040 ) ) ;
#116381 = CARTESIAN_POINT ( 'NONE',  ( 4.984793487045196869, 1.876812866478014596, 0.5713181500588762063 ) ) ;
#116382 = CARTESIAN_POINT ( 'NONE',  ( 1.358172466202983042, -1.961936380284023063, -0.005482119489134959674 ) ) ;
#116383 = DIRECTION ( 'NONE',  ( -0.7592566023652990159, -0.6507913734559659380, 0.000000000000000000 ) ) ;
#116384 = CARTESIAN_POINT ( 'NONE',  ( -9.393996029772727852, 15.45879393270864099, 7.466831081026168881 ) ) ;
#116385 = VERTEX_POINT ( 'NONE', #142945 ) ;
#116386 = CARTESIAN_POINT ( 'NONE',  ( 0.2162074652159052257, 1.082675745310441862, -1.819457589102360551 ) ) ;
#116387 = CARTESIAN_POINT ( 'NONE',  ( -3.750802052474980108, 7.527686161196117887, 1.040834085586084257E-14 ) ) ;
#116388 = CARTESIAN_POINT ( 'NONE',  ( 0.3746297210940018885, 1.718982886236510854, -0.6599183738737608440 ) ) ;
#116390 = MECHANICAL_DESIGN_GEOMETRIC_PRESENTATION_REPRESENTATION (  '', ( #154368 ), #60985 ) ;
#116389 = CARTESIAN_POINT ( 'NONE',  ( 4.083024739667787451, 2.059781850948108506, 0.6862965400120830672 ) ) ;
#116391 = CARTESIAN_POINT ( 'NONE',  ( 9.978696604288037619, 11.55417434068213822, -6.670641654589029912 ) ) ;
#116392 = CARTESIAN_POINT ( 'NONE',  ( 2.197662576721173266, 1.936918166296027977, -0.8637449004969055544 ) ) ;
#116393 = CARTESIAN_POINT ( 'NONE',  ( 0.7499999999999885647, 2.847916667349487341, -1.299038105676658228 ) ) ;
#116394 = CARTESIAN_POINT ( 'NONE',  ( 7.214910300766615769, 11.56914578420308715, -0.7998128361456291469 ) ) ;
#116395 = CARTESIAN_POINT ( 'NONE',  ( -1.833030277982346634, 2.531131934864056632, -2.499999999999998668 ) ) ;
#116396 = CARTESIAN_POINT ( 'NONE',  ( 6.582202237817778467, 6.781708767774706104, 0.2773405359152263383 ) ) ;
#116397 = VERTEX_POINT ( 'NONE', #180731 ) ;
#116398 = CARTESIAN_POINT ( 'NONE',  ( 2.196623993872096392, -0.5467073567838857118, -1.986887711889900432 ) ) ;
#116400 = CARTESIAN_POINT ( 'NONE',  ( -10.62873463776380234, 12.29999999999998295, 3.199999999999997957 ) ) ;
#116399 = CARTESIAN_POINT ( 'NONE',  ( -8.829384350997580455, 11.32403438096243775, 1.599625672291269396 ) ) ;
#116401 = CARTESIAN_POINT ( 'NONE',  ( 1.364683531249986537, 2.655208333674754062, -0.7879004041258239610 ) ) ;
#116402 = CARTESIAN_POINT ( 'NONE',  ( 0.07735805125225460321, 4.085280796943619563, -2.643583850410589964 ) ) ;
#116403 = CARTESIAN_POINT ( 'NONE',  ( 5.900277318768097246, 7.249539301847896411, -1.301905728482563251 ) ) ;
#116404 = VERTEX_POINT ( 'NONE', #177546 ) ;
#116405 = CARTESIAN_POINT ( 'NONE',  ( 4.318947422894989785, 1.476084237994702786, -1.215703867470045774 ) ) ;
#116406 = CARTESIAN_POINT ( 'NONE',  ( -1.288108131580338211, -0.9841229182759280159, 3.227445187970915619 ) ) ;
#116407 = CARTESIAN_POINT ( 'NONE',  ( 1.370828697373091432, -1.435183881573602216, 1.748884408748638597 ) ) ;
#116408 = CARTESIAN_POINT ( 'NONE',  ( -2.819205876637805641, 5.376491725131008259, -1.199719254218446718 ) ) ;
#116409 = CARTESIAN_POINT ( 'NONE',  ( 0.9667389835759466754, -1.427192611269219924, 1.115597691851821116 ) ) ;
#116410 = CARTESIAN_POINT ( 'NONE',  ( 1.481495926510235206, -0.6419399793253840469, 1.805124470068826037 ) ) ;
#116411 = CARTESIAN_POINT ( 'NONE',  ( 3.262232429473245432, -2.068111870375147987, 0.09887451149894616043 ) ) ;
#116412 = CARTESIAN_POINT ( 'NONE',  ( -1.364683531250000748, 1.821875000341421913, 0.000000000000000000 ) ) ;
#116413 = CARTESIAN_POINT ( 'NONE',  ( 0.7781230576423033840, -1.097119503657293382, 1.637799472441689996 ) ) ;
#116414 = CARTESIAN_POINT ( 'NONE',  ( 5.514262516685338511, -0.8683059565382322820, -1.719797162412556535 ) ) ;
#116416 = CARTESIAN_POINT ( 'NONE',  ( 6.151318917739748038, 6.974181327834800825, -0.9227930848511676221 ) ) ;
#116415 = CARTESIAN_POINT ( 'NONE',  ( 0.6105616303546910206, -2.295997848557976617, 0.2320981213338509652 ) ) ;
#116417 = CARTESIAN_POINT ( 'NONE',  ( 0.6823417656249882723, 2.176041667008084435, -1.181850606188749264 ) ) ;
#116418 = CARTESIAN_POINT ( 'NONE',  ( 4.967260703730732807, 1.792967015482237469, 1.019669102033170516 ) ) ;
#116419 = CARTESIAN_POINT ( 'NONE',  ( -6.063521013809733518, 8.097193820909906137, 1.599625672291283607 ) ) ;
#116420 = CARTESIAN_POINT ( 'NONE',  ( 8.426556166093362776, 9.789735934319136135, -1.199719254218446718 ) ) ;
#116421 = CARTESIAN_POINT ( 'NONE',  ( 0.000000000000000000, 8.600000000000017408, 0.4000000000000045186 ) ) ;
#116423 = CARTESIAN_POINT ( 'NONE',  ( 1.499999999999987121, 4.295833333333352044, -0.8660254037844323793 ) ) ;
#116422 = CARTESIAN_POINT ( 'NONE',  ( 5.684633084330723563, -2.053880889230023321, -0.4646916863456708735 ) ) ;
#116424 = CARTESIAN_POINT ( 'NONE',  ( -0.6823417656250212460, 2.863541667008084879, 1.181850606188767472 ) ) ;
#116425 = CARTESIAN_POINT ( 'NONE',  ( 4.341216920475977403, -1.883070171734081200, 1.061215411333437109 ) ) ;
#116426 = CARTESIAN_POINT ( 'NONE',  ( 5.514321518048907578, -2.019862493962302441, 0.002152582845403941403 ) ) ;
#116427 = CARTESIAN_POINT ( 'NONE',  ( -2.428612866367529932E-14, 2.999999999999999112, 7.500000000000000000 ) ) ;
#116428 = ADVANCED_FACE ( 'NONE', ( #194848 ), #39516, .T. ) ;
#116431 = CARTESIAN_POINT ( 'NONE',  ( 6.317736394288140822, 7.433409217166723870, 1.082531754730558626 ) ) ;
#116430 = CARTESIAN_POINT ( 'NONE',  ( 1.001543065824772753E-15, -1.071874999522043792, 3.793834371823811669 ) ) ;
#116429 = CARTESIAN_POINT ( 'NONE',  ( 5.989670002187236442, 10.20997511251894529, -0.7998128361456481317 ) ) ;
#116432 = CARTESIAN_POINT ( 'NONE',  ( -5.004894982100124068, 5.868074229652107121, 1.199719254218452935 ) ) ;
#116433 = CARTESIAN_POINT ( 'NONE',  ( 3.151577601795185757, 1.966304690962265234, -0.4465026806126579095 ) ) ;
#116434 = CARTESIAN_POINT ( 'NONE',  ( -9.677822722056413696, 10.18521468535430685, 1.040834085586084257E-14 ) ) ;
#116435 = CARTESIAN_POINT ( 'NONE',  ( -3.952365473583647315, 4.569846793057691592, 1.199719254218462483 ) ) ;
#116436 = CARTESIAN_POINT ( 'NONE',  ( -1.001543065824772872E-14, 5.321875000341422357, 1.575800808251672791 ) ) ;
#116438 = CARTESIAN_POINT ( 'NONE',  ( -1.364683531250010740, 8.630208333674730170, 0.7879004041258445001 ) ) ;
#116437 = CARTESIAN_POINT ( 'NONE',  ( 5.383715653711652394, 1.448795075966866852, 1.604530791579752202 ) ) ;
#116439 = DIRECTION ( 'NONE',  ( 0.000000000000000000, -1.000000000000000000, 0.000000000000000000 ) ) ;
#116440 = CARTESIAN_POINT ( 'NONE',  ( -1.297568150123634245, 13.22354355972565898, -0.9828994868031125653 ) ) ;
#116442 = CARTESIAN_POINT ( 'NONE',  ( 5.290638740200859225, 1.525033539048275877, -1.319242139327673424 ) ) ;
#116441 = CARTESIAN_POINT ( 'NONE',  ( -7.171900071504745178, 9.390302721554109056, -1.443375672974058777 ) ) ;
#116443 = CARTESIAN_POINT ( 'NONE',  ( -1.499999999999997780, 4.650000000000022560, 1.214306433183764966E-14 ) ) ;
#116444 = CARTESIAN_POINT ( 'NONE',  ( 0.7852881911578631913, 1.155166132482473351, 1.281103752909551030 ) ) ;
#116445 = CARTESIAN_POINT ( 'NONE',  ( 3.400062661977048428, 7.188766548940353829, -1.734723475976807094E-15 ) ) ;
#116447 = CARTESIAN_POINT ( 'NONE',  ( 6.261886844665240481, 8.398896966899865646, 1.599625672291268286 ) ) ;
#116446 = CARTESIAN_POINT ( 'NONE',  ( 7.863365906246055914, 10.19701286208565705, -1.443375672974057666 ) ) ;
#116448 = LINE ( 'NONE', #34069, #1949 ) ;
#116449 = CARTESIAN_POINT ( 'NONE',  ( 6.239502018287079288, -1.354773164471131164, -1.289998633004642237 ) ) ;
#116450 = CARTESIAN_POINT ( 'NONE',  ( 0.5396978354115729015, -1.910900059352708125, 0.6334021227705748380 ) ) ;
#116451 = LINE ( 'NONE', #34072, #113008 ) ;
#116452 = CARTESIAN_POINT ( 'NONE',  ( 2.521453382017309952, 5.885520012421409319, 0.000000000000000000 ) ) ;
#116453 = CIRCLE ( 'NONE', #192453, 0.08000000000000020983 ) ;
#116454 = CARTESIAN_POINT ( 'NONE',  ( -6.739811759324831897, 7.996106819701333634, -1.082531754730549967 ) ) ;
#116455 = VERTEX_POINT ( 'NONE', #94182 ) ;
#116456 = CARTESIAN_POINT ( 'NONE',  ( 7.714226216051361718, 11.94375498546120795, -0.7216878364870267237 ) ) ;
#116458 = CARTESIAN_POINT ( 'NONE',  ( 2.056267757160272325, -1.238304521155994209, 1.591332585091954854 ) ) ;
#116457 = CARTESIAN_POINT ( 'NONE',  ( 1.875790325896836919, 0.3594715711359474652, -2.089634487563592824 ) ) ;
#116459 = CARTESIAN_POINT ( 'NONE',  ( 2.003910543607852812, -0.7718314612508870853, 1.639047433122240660 ) ) ;
#116460 = CARTESIAN_POINT ( 'NONE',  ( 7.472478939787284169, 8.746922180287201698, 1.199719254218452935 ) ) ;
#116461 = CARTESIAN_POINT ( 'NONE',  ( 6.455963997168007396, 2.156291961557708525, -0.1537611777119098633 ) ) ;
#116462 = EDGE_LOOP ( 'NONE', ( #5986, #48939, #101506, #127467 ) ) ;
#116463 = CIRCLE ( 'NONE', #16183, 0.7499999999999997780 ) ;
#116464 = CARTESIAN_POINT ( 'NONE',  ( 5.438792177376376991, 9.497007973581119700, 1.040834085586084257E-14 ) ) ;
#116466 = CARTESIAN_POINT ( 'NONE',  ( 0.2685667436414033160, -0.2372314691254543417, -1.900927335933370488 ) ) ;
#116465 = CARTESIAN_POINT ( 'NONE',  ( -5.901876940650454095, 5.779944607047298177, -0.7998128361456291469 ) ) ;
#116467 = CARTESIAN_POINT ( 'NONE',  ( -11.97181042169641962, 9.720000000000002416, -0.8318531151397202672 ) ) ;
#116468 = DIRECTION ( 'NONE',  ( 1.000000000000000000, -0.000000000000000000, -0.000000000000000000 ) ) ;
#116469 = CARTESIAN_POINT ( 'NONE',  ( 5.707619481228810798, 7.681975366232176583, -1.443375672974057666 ) ) ;
#116470 = CARTESIAN_POINT ( 'NONE',  ( -1.364683531250000748, 0.07187500034142035865, 0.000000000000000000 ) ) ;
#116471 = CARTESIAN_POINT ( 'NONE',  ( 2.412988153552339643, 5.758977245878946327, 0.7216878364870438212 ) ) ;
#116472 = CARTESIAN_POINT ( 'NONE',  ( -8.299562589859897699, 12.83457345481192036, -0.7998128361456281477 ) ) ;
#116473 = EDGE_CURVE ( 'NONE', #111396, #183890, #92089, .T. ) ;
#116474 = VECTOR ( 'NONE', #194562, 1000.000000000000000 ) ;
#116475 = CARTESIAN_POINT ( 'NONE',  ( 4.452137864729129646, 2.161286467946467837, -0.05003489268536746859 ) ) ;
#116476 = CARTESIAN_POINT ( 'NONE',  ( -5.804299160426237059, 7.865044668620976509, -1.443375672974066548 ) ) ;
#116477 = CARTESIAN_POINT ( 'NONE',  ( 5.451787166470912993, 6.493411461371761284, -1.082531754730548412 ) ) ;
#116478 = CARTESIAN_POINT ( 'NONE',  ( 1.529697670087664108, -0.2543295609688834835, 2.105205558366497698 ) ) ;
#116479 = CARTESIAN_POINT ( 'NONE',  ( 6.774438514930277933, -1.120217847261167243, 1.442041797927499980 ) ) ;
#116480 = CARTESIAN_POINT ( 'NONE',  ( 2.969950176076568749, 1.051608646734447650, 1.667261953242512140 ) ) ;
#116481 = CARTESIAN_POINT ( 'NONE',  ( 5.502191098127390489, -0.8541586074963626318, 1.711093258865265643 ) ) ;
#116482 = ORIENTED_EDGE ( 'NONE', *, *, #5366, .T. ) ;
#116484 = EDGE_CURVE ( 'NONE', #184579, #58494, #31491, .T. ) ;
#116483 = DIRECTION ( 'NONE',  ( 0.000000000000000000, 0.000000000000000000, -1.000000000000000000 ) ) ;
#116485 = CARTESIAN_POINT ( 'NONE',  ( 5.617622257330707747, 0.3859593044726419286, -1.931177630036359005 ) ) ;
#116486 = CARTESIAN_POINT ( 'NONE',  ( 1.622886899410342254, -1.828648197406743670, 0.6539591521299585875 ) ) ;
#116487 = ORIENTED_EDGE ( 'NONE', *, *, #60399, .F. ) ;
#116488 = CARTESIAN_POINT ( 'NONE',  ( -4.390861645979385663, 6.216034235099629157, -1.599625672291271394 ) ) ;
#116490 = CARTESIAN_POINT ( 'NONE',  ( 7.876360894896227371, 8.153785563659219804, -0.7998128361456341429 ) ) ;
#116489 = CARTESIAN_POINT ( 'NONE',  ( -6.048345925472225382, 8.149765894507963182, 1.443375672974058777 ) ) ;
#116491 = CARTESIAN_POINT ( 'NONE',  ( 5.784525094524856748, 9.900363043587685041, 1.040834085586084257E-14 ) ) ;
#116493 = CARTESIAN_POINT ( 'NONE',  ( 5.085717018457579286, 6.066329622022862189, -1.082531754730548412 ) ) ;
#116492 = CARTESIAN_POINT ( 'NONE',  ( 5.784525094524856748, 9.900363043587685041, 1.040834085586084257E-14 ) ) ;
#116495 = ORIENTED_EDGE ( 'NONE', *, *, #5165, .F. ) ;
#116494 = CARTESIAN_POINT ( 'NONE',  ( 5.813130153884224605, 1.560705751063670377, -1.104717755519408984 ) ) ;
#116496 = CARTESIAN_POINT ( 'NONE',  ( 4.512475528931441104, -0.9420208833846724916, -1.995868093903986118 ) ) ;
#116497 = CARTESIAN_POINT ( 'NONE',  ( 1.712255133470397261, -2.190042126362458319, 0.2705847154940849153 ) ) ;
#116498 = CARTESIAN_POINT ( 'NONE',  ( 0.3868389748197207378, 3.100956225802571797, -0.4583768147623590861 ) ) ;
#116499 = CARTESIAN_POINT ( 'NONE',  ( 0.5922591856823838929, -1.062013159134197693, 1.590055880637729402 ) ) ;
#116500 = CARTESIAN_POINT ( 'NONE',  ( -2.474587689922123523, 5.184834355512716542, 0.9403128211546022408 ) ) ;
#116501 = CARTESIAN_POINT ( 'NONE',  ( 3.631357695093720306, 0.05367941694835526301, -2.069842578854002468 ) ) ;
#116502 = CARTESIAN_POINT ( 'NONE',  ( -4.564291269294938225, 8.476756914152748124, 1.040834085586084257E-14 ) ) ;
#116504 = CARTESIAN_POINT ( 'NONE',  ( 1.463986924769441478, 2.129665692569195024, -0.3698555562515608020 ) ) ;
#116503 = CARTESIAN_POINT ( 'NONE',  ( -3.928111819657352566, 5.605883094398769195, 1.599625672291267398 ) ) ;
#116505 = CARTESIAN_POINT ( 'NONE',  ( 3.931328349035985603, -1.512150646884598215, -1.586510368271301541 ) ) ;
#116506 = CARTESIAN_POINT ( 'NONE',  ( -1.225000000000014300, 0.7500000000000145439, -2.602085213965210642E-14 ) ) ;
#116507 = CARTESIAN_POINT ( 'NONE',  ( 2.957086901556340575, 6.464035461875470290, 0.7216878364870257245 ) ) ;
#116508 = CARTESIAN_POINT ( 'NONE',  ( 1.500000000000001332, 12.87499999999999822, 0.000000000000000000 ) ) ;
#116509 = CARTESIAN_POINT ( 'NONE',  ( 0.6823417656249969321, 14.83854166700806410, -1.181850606188757036 ) ) ;
#116510 = CARTESIAN_POINT ( 'NONE',  ( -3.630551273409382329, 7.457669928944732796, 0.7998128361456352531 ) ) ;
#116511 = CARTESIAN_POINT ( 'NONE',  ( 6.082590270738484683, -0.5753628732939282120, 1.636087478734444600 ) ) ;
#116512 = ADVANCED_FACE ( 'NONE', ( #60581 ), #188254, .T. ) ;
#116513 = CARTESIAN_POINT ( 'NONE',  ( -4.274898507010545856, 3.881803101134051470, -0.7998128361456221525 ) ) ;
#116514 = CARTESIAN_POINT ( 'NONE',  ( 3.186448005867897670, 1.153939711166888982, -1.718631068965512210 ) ) ;
#116515 = CARTESIAN_POINT ( 'NONE',  ( 5.167619242541076297, 1.422618751053092101, 1.568198848534626100 ) ) ;
#116516 = CARTESIAN_POINT ( 'NONE',  ( 5.286789834324991055, 8.255339675766103724, -1.199719254218452935 ) ) ;
#116517 = CARTESIAN_POINT ( 'NONE',  ( -1.364683531249997417, 4.009375000341424133, 1.214306433183764966E-14 ) ) ;
#116518 = CARTESIAN_POINT ( 'NONE',  ( 3.151173496672290852, 1.691593242058259783, -1.008282029756089493 ) ) ;
#116519 = CARTESIAN_POINT ( 'NONE',  ( 5.666080500323320557, -1.458056995643598475, 1.768786637700834108 ) ) ;
#116520 = CARTESIAN_POINT ( 'NONE',  ( 3.457459740917231628, 0.4424662778084071935, -1.771134634090239190 ) ) ;
#116521 = CARTESIAN_POINT ( 'NONE',  ( 3.230585741806197841, 6.991043475407723307, 0.7998128361456271485 ) ) ;
#116522 = CARTESIAN_POINT ( 'NONE',  ( 3.348500752450929596, 6.850408611260650815, 0.7216878364870317197 ) ) ;
#116523 = CARTESIAN_POINT ( 'NONE',  ( -7.379715684540041565, 7.504089808251839244, 1.040834085586084257E-14 ) ) ;
#116525 = VERTEX_POINT ( 'NONE', #20356 ) ;
#116524 =( BOUNDED_CURVE ( )  B_SPLINE_CURVE ( 2, ( #113599, #213140, #214176, #146056, #114662, #195848, #180656, #66866, #100469 ),
 .UNSPECIFIED., .F., .T. ) 
 B_SPLINE_CURVE_WITH_KNOTS ( ( 3, 2, 2, 2, 3 ),
 ( 0.7767857142857143016, 0.7797619047619047672, 0.7857142857142856984, 0.7916666666666666297, 0.7946428571428572063 ),
 .UNSPECIFIED. ) 
 CURVE ( )  GEOMETRIC_REPRESENTATION_ITEM ( )  RATIONAL_B_SPLINE_CURVE ( ( 0.9330127018922194093, 0.9330127018922194093, 1.000000000000000000, 0.8660254037844387076, 1.000000000000000000, 0.8660254037844387076, 1.000000000000000000, 0.9330127018922180770, 0.9330127018922194093 ) ) 
 REPRESENTATION_ITEM ( '' )  );
#116526 = ORIENTED_EDGE ( 'NONE', *, *, #89254, .T. ) ;
#116527 = CARTESIAN_POINT ( 'NONE',  ( 4.359639327901571271, -1.559048523801108477, -1.273764430229076483 ) ) ;
#116528 = CARTESIAN_POINT ( 'NONE',  ( 3.889464431383614862, -1.814284039448841979, 0.7467176931179178023 ) ) ;
#116529 = CARTESIAN_POINT ( 'NONE',  ( -8.532158741701643123, 8.848606708273724308, 0.7998128361456462443 ) ) ;
#116530 = CIRCLE ( 'NONE', #168420, 2.011244508837062295 ) ;
#116531 = CARTESIAN_POINT ( 'NONE',  ( -5.759516327706961647, 5.613857225279885732, -0.7998128361456221525 ) ) ;
#116532 = CARTESIAN_POINT ( 'NONE',  ( 0.1755611466353447780, 0.6788741266964171128, -2.325051092042058620 ) ) ;
#116534 = CARTESIAN_POINT ( 'NONE',  ( 5.928513199909208886, 1.706640645603505257, 0.4684080695957025253 ) ) ;
#116533 = CARTESIAN_POINT ( 'NONE',  ( 0.4508687890585044711, -1.768401812538191287, -1.115020903081758608 ) ) ;
#116535 = CARTESIAN_POINT ( 'NONE',  ( 10.99896775280371131, -5.324706741106397523, -0.1653080603930866532 ) ) ;
#116536 = CARTESIAN_POINT ( 'NONE',  ( 2.185716925580234449, -0.9354795820612994417, 1.981881815340847730 ) ) ;
#116537 = CARTESIAN_POINT ( 'NONE',  ( 0.9424304438642245874, -1.370989592614113795, -1.072060877835380621 ) ) ;
#116538 = CARTESIAN_POINT ( 'NONE',  ( 6.745345117998789775, 7.828323044875442172, 1.199719254218462483 ) ) ;
#116539 = CARTESIAN_POINT ( 'NONE',  ( 0.2331713839410576583, 0.005725554726919174046, -1.953566683266183102 ) ) ;
#116540 = CARTESIAN_POINT ( 'NONE',  ( 0.6622201036875573488, -1.252624510564132931, 1.186060005986578014 ) ) ;
#116541 = CARTESIAN_POINT ( 'NONE',  ( 0.9490539546192258147, 1.544862702020805223, 1.701928257493188434 ) ) ;
#116542 = CARTESIAN_POINT ( 'NONE',  ( 0.7498831369015904746, 2.188782640433343474, -0.1130235578899463078 ) ) ;
#116543 = CARTESIAN_POINT ( 'NONE',  ( 3.211752199052122503, -0.4303563718574507369, 2.164345902561148005 ) ) ;
#116544 = CARTESIAN_POINT ( 'NONE',  ( 1.340952317110634118, -2.117647682651255803, -0.4779334406839957916 ) ) ;
#116545 = CARTESIAN_POINT ( 'NONE',  ( 0.01192831195480706721, -0.7772932952810689411, -1.650495136788888040 ) ) ;
#116546 = CARTESIAN_POINT ( 'NONE',  ( 2.606785607150950757, 1.995414689559615207, 0.7085744572869844271 ) ) ;
#116547 = CARTESIAN_POINT ( 'NONE',  ( 6.727182134110202938, 2.016807574165893513, 2.492494991173601182 ) ) ;
#116548 = CARTESIAN_POINT ( 'NONE',  ( 5.561526637868618117, 0.3756393653304244129, -1.889249976882242610 ) ) ;
#116549 = VERTEX_POINT ( 'NONE', #164486 ) ;
#116551 = CARTESIAN_POINT ( 'NONE',  ( 1.499999999999989120, 5.795833333333350268, -0.8660254037844323793 ) ) ;
#116550 = CARTESIAN_POINT ( 'NONE',  ( 2.103457651957148844, -0.4980181218575702173, 2.237485198869753944 ) ) ;
#116552 = CARTESIAN_POINT ( 'NONE',  ( 4.546061579283848353, 4.198160018786257552, -0.7998128361456211532 ) ) ;
#116553 = CARTESIAN_POINT ( 'NONE',  ( 4.547870462380197765, 7.393267075163835855, 1.199719254218462483 ) ) ;
#116554 = CARTESIAN_POINT ( 'NONE',  ( 5.373765183877965868, 0.4349513647441177744, -2.178143251680577208 ) ) ;
#116555 = CARTESIAN_POINT ( 'NONE',  ( -8.215877900201387973, 8.687538426430837291, 0.7216878364870578100 ) ) ;
#116556 =( NAMED_UNIT ( * ) SI_UNIT ( $, .STERADIAN. ) SOLID_ANGLE_UNIT ( ) );
#116557 = AXIS2_PLACEMENT_3D ( 'NONE', #171475, #149905, #186650 ) ;
#116558 = CARTESIAN_POINT ( 'NONE',  ( 5.721177635286841756, 6.737423998331861341, -1.082531754730543083 ) ) ;
#116559 = CARTESIAN_POINT ( 'NONE',  ( -8.798878505144658746, 10.32807501316600884, -1.082531754730543083 ) ) ;
#116560 = CARTESIAN_POINT ( 'NONE',  ( 4.407809338218622308, 8.156544971314787063, 0.000000000000000000 ) ) ;
#116561 = VERTEX_POINT ( 'NONE', #65881 ) ;
#116562 = CARTESIAN_POINT ( 'NONE',  ( 2.760388869050140137, 1.913803604375517109, -0.6351994527180188088 ) ) ;
#116564 = CARTESIAN_POINT ( 'NONE',  ( 0.9364711893796459075, -1.149011738537804250, 1.712694122252313100 ) ) ;
#116563 = CARTESIAN_POINT ( 'NONE',  ( 8.260995669428309540, 8.532249790621511565, 0.7998128361456481317 ) ) ;
#116565 = CARTESIAN_POINT ( 'NONE',  ( 5.600926855776875435, 7.627776979863398310, -1.443375672974078761 ) ) ;
#116566 = CARTESIAN_POINT ( 'NONE',  ( 2.520460663003311730, -4.091624451297095177, -2.338645729556988240 ) ) ;
#116567 = CARTESIAN_POINT ( 'NONE',  ( -0.6823417656250212460, 3.301041667008085323, 1.181850606188767472 ) ) ;
#116568 = CARTESIAN_POINT ( 'NONE',  ( 3.820431320580887302, 2.080737768064028437, 0.6879518193209921417 ) ) ;
#116569 = CARTESIAN_POINT ( 'NONE',  ( 0.8795299900376440938, -0.4926441280813895762, -1.955172062459666904 ) ) ;
#116570 = CARTESIAN_POINT ( 'NONE',  ( 1.557894219809667247, -1.301531972126177772, 1.302644501960325885 ) ) ;
#116571 = CARTESIAN_POINT ( 'NONE',  ( 5.478174288590652807, -2.235914823156583964, -0.5050262530511948622 ) ) ;
#116572 = CARTESIAN_POINT ( 'NONE',  ( 4.312339554033173705, 1.684294245562456993, 0.7440144950455057637 ) ) ;
#116573 = CARTESIAN_POINT ( 'NONE',  ( 8.444030743212801227, 8.745790710036752458, 0.7998128361456462443 ) ) ;
#116574 = SURFACE_STYLE_FILL_AREA ( #85079 ) ;
#116575 = CARTESIAN_POINT ( 'NONE',  ( 4.225493254642153751, -1.746956894163293361, 0.5300125199643389573 ) ) ;
#116576 = CARTESIAN_POINT ( 'NONE',  ( 4.500625067706437221, -1.976956227568788638, 0.3961002554062897918 ) ) ;
#116577 = CARTESIAN_POINT ( 'NONE',  ( -9.203287345578106127, 9.631590079462940324, 0.7998128361456462443 ) ) ;
#116579 = CARTESIAN_POINT ( 'NONE',  ( -5.271087860662956537, 9.371629280740593870, 0.000000000000000000 ) ) ;
#116578 = CARTESIAN_POINT ( 'NONE',  ( 4.557670991828286056, 0.4998169670675355336, -2.206472437794388952 ) ) ;
#116580 = CARTESIAN_POINT ( 'NONE',  ( 6.704139028598911310, -2.105588161048920437, 0.04759252156865538541 ) ) ;
#116581 = CARTESIAN_POINT ( 'NONE',  ( -1.772826578342764359, 3.950000000000574385, -0.4000000000000286660 ) ) ;
#116582 = CARTESIAN_POINT ( 'NONE',  ( 5.002425025097493538, 2.064580399062130311, 0.1557331365308264881 ) ) ;
#116583 = CARTESIAN_POINT ( 'NONE',  ( 8.052653171512838881, 11.48218023581863001, -1.199719254218446718 ) ) ;
#116584 =( NAMED_UNIT ( * ) PLANE_ANGLE_UNIT ( ) SI_UNIT ( $, .RADIAN. ) );
#116585 = APPLICATION_PROTOCOL_DEFINITION ( 'draft international standard', 'automotive_design', 1998, #144661 ) ;
#116587 = CARTESIAN_POINT ( 'NONE',  ( 2.438006290551326671, 0.9082397578730906362, -1.698968261161729831 ) ) ;
#116586 = CARTESIAN_POINT ( 'NONE',  ( -8.097244055859620815, 10.46987070330147063, -1.599625672291263179 ) ) ;
#116588 = UNCERTAINTY_MEASURE_WITH_UNIT (LENGTH_MEASURE( 1.000000000000000082E-05 ), #15813, 'distance_accuracy_value', 'NONE');
#116589 = CARTESIAN_POINT ( 'NONE',  ( 0.5988051026822670542, 6.720402535194986982, 3.593870046926598061 ) ) ;
#116590 = CARTESIAN_POINT ( 'NONE',  ( 6.789911431267126041, -1.283970416288570116, -1.493486111907322389 ) ) ;
#116591 = CARTESIAN_POINT ( 'NONE',  ( 7.472478939787284169, 8.746922180287201698, 1.199719254218452935 ) ) ;
#116592 = CARTESIAN_POINT ( 'NONE',  ( 4.952123820727618586, 6.619828698506379006, -1.244621138126526194 ) ) ;
#116593 = CARTESIAN_POINT ( 'NONE',  ( -2.605138072120212200, 6.191078184115536232, -0.7998128361456281477 ) ) ;
#116595 = CARTESIAN_POINT ( 'NONE',  ( 1.178328164221422503, 2.187401300010451077, -0.3865082640040794493 ) ) ;
#116594 = CARTESIAN_POINT ( 'NONE',  ( 1.283610819548046011, 0.1505422781087061845, -2.115291873224629082 ) ) ;
#116596 = CARTESIAN_POINT ( 'NONE',  ( 2.819468948711697287, -0.2076110458819386551, 2.095707187103168945 ) ) ;
#116597 = CARTESIAN_POINT ( 'NONE',  ( -7.747558435566414659, 8.003516027774422170, -0.7998128361456362523 ) ) ;
#116598 = CARTESIAN_POINT ( 'NONE',  ( 6.089583550832340819, 10.25626457594641749, 1.040834085586084257E-14 ) ) ;
#116599 = CARTESIAN_POINT ( 'NONE',  ( 2.734756269166933151, -1.876540383875524576, -0.5722209215143353456 ) ) ;
#116600 = CARTESIAN_POINT ( 'NONE',  ( 4.625302960556422427, 8.547937220624488575, 1.040834085586084257E-14 ) ) ;
#116601 = CARTESIAN_POINT ( 'NONE',  ( -4.061901113999940804, 7.558576442610514867, -0.4421990992426305112 ) ) ;
#116602 = CARTESIAN_POINT ( 'NONE',  ( 3.174580523894166006, 6.855427711185178019, 0.7998128361456341429 ) ) ;
#116603 = CARTESIAN_POINT ( 'NONE',  ( -6.346625304972878467, 7.537389289624049304, 1.082531754730548412 ) ) ;
#116605 = CARTESIAN_POINT ( 'NONE',  ( -7.375272376154093479, 9.627570410311676596, -1.443375672974059665 ) ) ;
#116604 = CIRCLE ( 'NONE', #40495, 2.725000000000000089 ) ;
#116606 = CARTESIAN_POINT ( 'NONE',  ( 2.004293344102888508, -0.9022931611136343344, 1.919180038594799687 ) ) ;
#116607 = CARTESIAN_POINT ( 'NONE',  ( -5.611095471209320174, 7.639640364534566075, 1.599625672291263179 ) ) ;
#116609 = CARTESIAN_POINT ( 'NONE',  ( 4.598074495912658044, 0.8407358649686399454, -1.772743347989129692 ) ) ;
#116608 = CARTESIAN_POINT ( 'NONE',  ( -0.6125000000000262457, 0.4583333333333244886, -1.060881119635996850 ) ) ;
#116610 = CARTESIAN_POINT ( 'NONE',  ( 3.186554565756247737, -2.129457467500107004, -0.3711038070777841202 ) ) ;
#116611 = CARTESIAN_POINT ( 'NONE',  ( 2.630204301513817455, 0.2276190002089127917, 1.827071974840013491 ) ) ;
#116612 = CARTESIAN_POINT ( 'NONE',  ( -4.014242769884851292, 7.626870978312306981, -0.02218799730280621163 ) ) ;
#116613 = CARTESIAN_POINT ( 'NONE',  ( -1.364683531250014514, -0.9072916663252470482, 0.7879004041258379498 ) ) ;
#116614 = CARTESIAN_POINT ( 'NONE',  ( 4.224340698251967119, 0.08847545473529906668, 1.738206131172301161 ) ) ;
#116615 = CARTESIAN_POINT ( 'NONE',  ( 4.033180945112804672, 7.763139070050654844, 0.4071004073024475090 ) ) ;
#116616 = CARTESIAN_POINT ( 'NONE',  ( 5.883875478650832491, 6.927238148923188454, -1.082531754730543083 ) ) ;
#116617 = CARTESIAN_POINT ( 'NONE',  ( -10.88586298614011660, 5.812970821470938354, 6.395187734525825896 ) ) ;
#116619 = EDGE_CURVE ( 'NONE', #135381, #116549, #81704, .T. ) ;
#116618 = CIRCLE ( 'NONE', #182250, 0.07999999999999993228 ) ;
#116620 = CARTESIAN_POINT ( 'NONE',  ( 2.272554088390315030, -1.330374092946192688, 1.703740541667747133 ) ) ;
#116621 = CARTESIAN_POINT ( 'NONE',  ( 4.587267430073429963, 1.242536178122002344, -1.587594670648798445 ) ) ;
#116622 = DIRECTION ( 'NONE',  ( -0.000000000000000000, -1.000000000000000000, -0.000000000000000000 ) ) ;
#116623 = CARTESIAN_POINT ( 'NONE',  ( 1.393688021309073433, 1.637156065531343740, 1.411701162175371893 ) ) ;
#116624 = CARTESIAN_POINT ( 'NONE',  ( 2.887526864075397715, 1.393042391738574137, 1.395278474455765805 ) ) ;
#116625 = CARTESIAN_POINT ( 'NONE',  ( 6.509000000000053632, 2.033894086284238956, 2.405029747421689290 ) ) ;
#116626 = CARTESIAN_POINT ( 'NONE',  ( 3.386211154777326815, -0.3816624740031882568, -1.904027918096486527 ) ) ;
#116629 = ORIENTED_EDGE ( 'NONE', *, *, #186483, .F. ) ;
#116628 = CARTESIAN_POINT ( 'NONE',  ( -4.855228407469635243, 4.837057028235559386, 0.7216878364870257245 ) ) ;
#116627 = CARTESIAN_POINT ( 'NONE',  ( -8.459924664802993988, 12.81373650900478189, 1.040834085586084257E-14 ) ) ;
#116630 = CARTESIAN_POINT ( 'NONE',  ( -4.462041952228957165, 5.338708711422782471, -1.082531754730549967 ) ) ;
#116631 = CARTESIAN_POINT ( 'NONE',  ( 3.562760505341037831, 7.378580699531681830, -1.734723475976807094E-15 ) ) ;
#116632 = CARTESIAN_POINT ( 'NONE',  ( -5.306037014901836990, 7.283738832175834510, 1.599625672291263179 ) ) ;
#116633 = CARTESIAN_POINT ( 'NONE',  ( -9.341204649691320583, 10.96078884847042545, 1.082531754730558626 ) ) ;
#116634 = CARTESIAN_POINT ( 'NONE',  ( 0.6576010401811819284, -1.865379905010958517, -1.178792301215730642 ) ) ;
#116635 = CARTESIAN_POINT ( 'NONE',  ( 1.642778471875000035, -3.026041666188708401, -2.845375778867859751 ) ) ;
#116636 = EDGE_CURVE ( 'NONE', #55414, #170100, #108857, .T. ) ;
#116637 = CARTESIAN_POINT ( 'NONE',  ( 4.944172655442597986, -0.9282843415348587257, 1.728263438747809078 ) ) ;
#116638 = CARTESIAN_POINT ( 'NONE',  ( 1.863907939170056149, -0.1017519224979606118, -2.013985838549677609 ) ) ;
#116639 = EDGE_LOOP ( 'NONE', ( #159214, #190978, #63895, #158155 ) ) ;
#116640 = CARTESIAN_POINT ( 'NONE',  ( 3.591103737854687061, 1.818103999434977025, 1.084929287856269742 ) ) ;
#116641 = CARTESIAN_POINT ( 'NONE',  ( 1.499999999999989120, 2.556250000682817713, 1.214306433183764966E-14 ) ) ;
#116643 = CARTESIAN_POINT ( 'NONE',  ( -5.045605722580076780, 9.038290442985410067, -0.7998128361456231517 ) ) ;
#116642 = CARTESIAN_POINT ( 'NONE',  ( 9.499679971350916574, -7.185026885903947225, 0.07802162204196347317 ) ) ;
#116644 = CARTESIAN_POINT ( 'NONE',  ( 4.224425198852012286, 0.09258891237720962009, 1.838934309869838968 ) ) ;
#116645 = ORIENTED_EDGE ( 'NONE', *, *, #149694, .F. ) ;
#116646 = CARTESIAN_POINT ( 'NONE',  ( -8.025536864285518490, 11.45054454405341282, -1.199719254218446718 ) ) ;
#116647 = LINE ( 'NONE', #202063, #158903 ) ;
#116648 = CARTESIAN_POINT ( 'NONE',  ( 4.816704082729271086, -0.7169179515637627009, -1.995842421597990413 ) ) ;
#116649 = CARTESIAN_POINT ( 'NONE',  ( 6.474182045725470402, 7.511966127223233869, -1.199719254218446718 ) ) ;
#116650 = CARTESIAN_POINT ( 'NONE',  ( 5.009085904467641015, 1.791045569760267631, 1.019200576588958240 ) ) ;
#116653 = CARTESIAN_POINT ( 'NONE',  ( 2.823586671956069605, 1.020774559177588081, -1.532180179759069283 ) ) ;
#116652 = CARTESIAN_POINT ( 'NONE',  ( 0.5372768211588532239, 1.738583335619352077, -0.6644854061606010331 ) ) ;
#116651 = CARTESIAN_POINT ( 'NONE',  ( 4.529832720741620022, 7.338536369956936589, -1.082531754730548412 ) ) ;
#116654 = CARTESIAN_POINT ( 'NONE',  ( 8.585337585951586803, 11.03931315507545108, -1.599625672291255185 ) ) ;
#116655 = DIRECTION ( 'NONE',  ( 3.330669073875479482E-16, -3.330669073875479482E-16, -1.000000000000000000 ) ) ;
#116656 = CARTESIAN_POINT ( 'NONE',  ( 1.403499169902377552, 7.376709478543040710, 4.304123474984470121 ) ) ;
#116657 = DIRECTION ( 'NONE',  ( 0.7592566023653005702, 0.6507913734559639396, 0.000000000000000000 ) ) ;
#116658 = CARTESIAN_POINT ( 'NONE',  ( 2.666872310945223923, -1.521158656661812714, 1.599105504226288499 ) ) ;
#116659 = CARTESIAN_POINT ( 'NONE',  ( 4.587383588223284292, 2.023586100481920447, -1.011833202457941283 ) ) ;
#116660 = CARTESIAN_POINT ( 'NONE',  ( -7.863365906246068349, 9.236643647784308797, -1.082531754730543971 ) ) ;
#116661 = CARTESIAN_POINT ( 'NONE',  ( 4.324329094900294379, -0.7804802743817635946, -1.635003121989448971 ) ) ;
#116662 = CARTESIAN_POINT ( 'NONE',  ( 5.858580540861003882, -1.821332666672281553, -0.5942308157336049224 ) ) ;
#116663 = CARTESIAN_POINT ( 'NONE',  ( -0.6823417656249969321, 5.280208333674756283, -1.181850606188749264 ) ) ;
#116664 = CARTESIAN_POINT ( 'NONE',  ( 4.610133579271312954, -0.8000244862099057386, -1.691074300901610261 ) ) ;
#116665 = CARTESIAN_POINT ( 'NONE',  ( 4.598021663640887269, 0.7965279161250311546, -1.682138884369558607 ) ) ;
#116666 = CARTESIAN_POINT ( 'NONE',  ( 0.08832626591284459261, -9.919998018383680005, 9.499595568239961096 ) ) ;
#116667 = CARTESIAN_POINT ( 'NONE',  ( 5.928513199909208886, 1.706640645603505257, 0.4684080695957025253 ) ) ;
#116668 = CARTESIAN_POINT ( 'NONE',  ( 0.6906390985809904848, 1.523792322931913468, -1.320830384837400118 ) ) ;
#116670 = CARTESIAN_POINT ( 'NONE',  ( 1.401149585966605882, 1.720815086091964652, -1.213930111015694369 ) ) ;
#116669 = CARTESIAN_POINT ( 'NONE',  ( -8.482597663644387609, 13.04811437422715414, -0.7998128361456281477 ) ) ;
#116671 = CARTESIAN_POINT ( 'NONE',  ( 9.531545685607134999, 11.07889037375188401, 1.199719254218450271 ) ) ;
#116673 = DIRECTION ( 'NONE',  ( -0.6507913734559640506, -0.7592566023653004592, 0.000000000000000000 ) ) ;
#116672 = DIRECTION ( 'NONE',  ( 0.000000000000000000, 0.000000000000000000, 1.000000000000000000 ) ) ;
#116674 = CARTESIAN_POINT ( 'NONE',  ( -10.32992389895503393, 1.000000000000000888, -6.106772653521458594 ) ) ;
#116675 = CARTESIAN_POINT ( 'NONE',  ( 2.144791408438687430, 1.960151896008819117, 0.4867283015469162644 ) ) ;
#116676 = CARTESIAN_POINT ( 'NONE',  ( 0.6823417656249899377, 1.592708333674752730, 1.181850606188755259 ) ) ;
#116677 = CARTESIAN_POINT ( 'NONE',  ( 6.620655732516649294, 2.985444497229528427, 2.280274006979409407 ) ) ;
#116678 = CARTESIAN_POINT ( 'NONE',  ( 4.416205349749311004, 6.175325546172740765, 1.599625672291267398 ) ) ;
#116679 = ORIENTED_EDGE ( 'NONE', *, *, #52153, .T. ) ;
#116680 = CARTESIAN_POINT ( 'NONE',  ( 2.196749789412206333, -0.5742421066207163971, -2.083876772215712325 ) ) ;
#116681 = CARTESIAN_POINT ( 'NONE',  ( 6.610000000000006537, 0.002781820520842553934, 2.000159646111852929 ) ) ;
#116684 = DIRECTION ( 'NONE',  ( -5.578564026256490882E-16, -1.000000000000000000, -9.066213480720158442E-32 ) ) ;
#116683 = CARTESIAN_POINT ( 'NONE',  ( 1.500000000000001332, 13.15625000068279604, 0.000000000000000000 ) ) ;
#116682 = CARTESIAN_POINT ( 'NONE',  ( 3.576318658954677598, 7.394398545414291313, 0.7998128361456281477 ) ) ;
#116685 = CARTESIAN_POINT ( 'NONE',  ( 9.720832950873944611, 10.44331931888218001, -0.7216878364870257245 ) ) ;
#116686 = CARTESIAN_POINT ( 'NONE',  ( 6.473846665049121540, -0.8576149079453172508, 1.823233050095712349 ) ) ;
#116687 = CARTESIAN_POINT ( 'NONE',  ( -7.863365906246074566, 8.276274433482971205, -0.7216878364870278340 ) ) ;
#116688 = MECHANICAL_DESIGN_GEOMETRIC_PRESENTATION_REPRESENTATION (  '', ( #19829 ), #64679 ) ;
#116689 = CARTESIAN_POINT ( 'NONE',  ( 0.6971427418834205136, 1.794861059153027627, 1.257291590721874686 ) ) ;
#116690 = CARTESIAN_POINT ( 'NONE',  ( 0.007473969438115558167, 8.279395425053873936, 1.999986034896453324 ) ) ;
#116691 = CARTESIAN_POINT ( 'NONE',  ( 1.956323303678444425, 2.256377666735286169, -0.1672192238599319314 ) ) ;
#116692 = CARTESIAN_POINT ( 'NONE',  ( -6.320072162264675164, 10.52516795595079557, 0.7998128361456481317 ) ) ;
#116693 = CARTESIAN_POINT ( 'NONE',  ( -5.070386261386537363, 5.017798181146802428, 1.214306433183764966E-14 ) ) ;
#116694 = CARTESIAN_POINT ( 'NONE',  ( 1.364683531249990311, 3.196875000341416140, 1.214306433183764966E-14 ) ) ;
#116695 = CARTESIAN_POINT ( 'NONE',  ( 4.649081266440608928, 8.305916344280937835, -0.4560373724170601606 ) ) ;
#116696 = CARTESIAN_POINT ( 'NONE',  ( 1.500000000000001332, 10.62499999999999645, 0.000000000000000000 ) ) ;
#116697 = CARTESIAN_POINT ( 'NONE',  ( 7.865138509703455405, 8.348618814175074121, -0.7216878364870317197 ) ) ;
#116698 = CARTESIAN_POINT ( 'NONE',  ( 2.670886861492921316, 0.09125233944726543478, -1.767527270347787116 ) ) ;
#116699 = CARTESIAN_POINT ( 'NONE',  ( 9.856941372335116469, 11.45851867493453291, 1.199719254218450271 ) ) ;
#116700 = CARTESIAN_POINT ( 'NONE',  ( 6.651417122894856426, -1.768357563224710605, -1.319949637914811458 ) ) ;
#116701 = CARTESIAN_POINT ( 'NONE',  ( -1.364683531250000748, 8.609375000341396245, 0.000000000000000000 ) ) ;
#116702 = ORIENTED_EDGE ( 'NONE', *, *, #24366, .F. ) ;
#116703 = CARTESIAN_POINT ( 'NONE',  ( -5.088052786878465739, 9.158088361325352977, 0.000000000000000000 ) ) ;
#116704 = CARTESIAN_POINT ( 'NONE',  ( 5.167592292328679449, 1.356312711205298172, 1.492245250866150785 ) ) ;
#116706 = ORIENTED_EDGE ( 'NONE', *, *, #105660, .T. ) ;
#116705 = CARTESIAN_POINT ( 'NONE',  ( 4.816585706611137496, -0.6173935602037239345, -1.703258737839604242 ) ) ;
#116707 = CARTESIAN_POINT ( 'NONE',  ( 2.641296366799699147, -1.384790685969448099, -1.257831364775918503 ) ) ;
#116708 = CARTESIAN_POINT ( 'NONE',  ( 2.219664259111033378, 0.3580842396277704176, -2.038906786875307020 ) ) ;
#116709 = CARTESIAN_POINT ( 'NONE',  ( -7.417719440008134768, 7.826629899530511025, 0.7216878364870317197 ) ) ;
#116710 = CARTESIAN_POINT ( 'NONE',  ( 2.302860652515530848, -0.3306829512400177862, -1.883434002855538081 ) ) ;
#116711 = CARTESIAN_POINT ( 'NONE',  ( -4.933139366528609848, 7.815959757607085834, 1.092252181328734473 ) ) ;
#116712 = AXIS2_PLACEMENT_3D ( 'NONE', #141476, #116188, #131371 ) ;
#116713 = CARTESIAN_POINT ( 'NONE',  ( -9.409940793360268785, 3.999985931113709814, -6.919963696468023784 ) ) ;
#116714 = CARTESIAN_POINT ( 'NONE',  ( 0.4365953560983709680, -5.836144560139977955, 10.35465518852992339 ) ) ;
#116715 = CARTESIAN_POINT ( 'NONE',  ( 1.364683531249988535, 4.176041667008081326, 0.7879004041258500513 ) ) ;
#116716 = DIRECTION ( 'NONE',  ( 0.000000000000000000, -1.000000000000000000, 0.000000000000000000 ) ) ;
#116717 = CARTESIAN_POINT ( 'NONE',  ( 5.397554552016212703, 8.350878506444006533, 1.082531754730547524 ) ) ;
#116718 = CARTESIAN_POINT ( 'NONE',  ( 1.609737659951641309, 0.5726723138891121057, -1.876404140693301414 ) ) ;
#116719 = CARTESIAN_POINT ( 'NONE',  ( 0.1575669172422279607, -0.4392406603518673736, -1.974865693180789750 ) ) ;
#116720 = CARTESIAN_POINT ( 'NONE',  ( -5.957882158562513908, 5.915560371269843465, -0.7998128361456362523 ) ) ;
#116721 = CARTESIAN_POINT ( 'NONE',  ( 5.748313822965784858, 1.043546352714582071, -1.845953426139717246 ) ) ;
#116723 = CARTESIAN_POINT ( 'NONE',  ( -10.45911050446410506, 5.175404930453152197, 5.201426885097844455 ) ) ;
#116722 = CARTESIAN_POINT ( 'NONE',  ( 7.899597058256738968, 12.36794700127490820, 1.040834085586084257E-14 ) ) ;
#116724 = CARTESIAN_POINT ( 'NONE',  ( 6.731714608790520415, -1.285842040959904287, -1.494388255172361513 ) ) ;
#116725 = CARTESIAN_POINT ( 'NONE',  ( -0.6823417656250212460, 3.051041667008084879, 1.181850606188767472 ) ) ;
#116726 = CARTESIAN_POINT ( 'NONE',  ( 1.687745526430058263, 1.925312447093192825, -0.5882657090081342410 ) ) ;
#116728 = CARTESIAN_POINT ( 'NONE',  ( 1.019337291899083064, -1.912195925978699140, 0.9092529662874779817 ) ) ;
#116727 = CARTESIAN_POINT ( 'NONE',  ( -6.222829318992474157, 10.20379193889247382, 0.000000000000000000 ) ) ;
#116730 = EDGE_CURVE ( 'NONE', #6715, #17249, #150817, .T. ) ;
#116729 = CARTESIAN_POINT ( 'NONE',  ( 10.91919020434494136, 8.223964437691744678, -4.993264204099808090 ) ) ;
#116731 = CARTESIAN_POINT ( 'NONE',  ( 2.488806849732328796, 2.007603858877416769, 0.5053560088097220904 ) ) ;
#116732 = CARTESIAN_POINT ( 'NONE',  ( 4.390861645979372341, 6.216034235099629157, -1.599625672291269396 ) ) ;
#116733 = CARTESIAN_POINT ( 'NONE',  ( 3.953084306836263995, 6.769626237021087789, 1.199719254218452047 ) ) ;
#116734 = EDGE_LOOP ( 'NONE', ( #14927, #176490, #124387, #193006 ) ) ;
#116736 = CARTESIAN_POINT ( 'NONE',  ( 5.203632029546647608, 4.965325544092860532, 1.040834085586084257E-14 ) ) ;
#116735 = CARTESIAN_POINT ( 'NONE',  ( 5.824191892830967276, 2.014527380540787505, 0.5587128073646082660 ) ) ;
#116739 = EDGE_LOOP ( 'NONE', ( #183521, #143227, #198080, #172941, #112911 ) ) ;
#116738 = CARTESIAN_POINT ( 'NONE',  ( 2.982852160962686128, -1.674641624487639424, -0.6911452858660637188 ) ) ;
#116737 = CARTESIAN_POINT ( 'NONE',  ( 4.453998568579462969, 1.825179399820752169, -0.04523609120457571658 ) ) ;
#116740 = CARTESIAN_POINT ( 'NONE',  ( 7.865701674222579598, 12.32840238656838139, -0.7998128361456352531 ) ) ;
#116741 = DIRECTION ( 'NONE',  ( -0.000000000000000000, -1.000000000000000000, -0.000000000000000000 ) ) ;
#116742 = CARTESIAN_POINT ( 'NONE',  ( 11.05419992680906027, 7.768390597564347466, 1.622890935638873655 ) ) ;
#116743 = CARTESIAN_POINT ( 'NONE',  ( 5.737410212107617369, -1.997324651315038002, 0.9386623957203034108 ) ) ;
#116744 = CARTESIAN_POINT ( 'NONE',  ( -0.6823417656250003738, 10.46354166700806587, 1.181850606188754593 ) ) ;
#116745 = VERTEX_POINT ( 'NONE', #135214 ) ;
#116746 = CARTESIAN_POINT ( 'NONE',  ( 4.072844535355981677, -1.414876986328793329, 1.286614418101794444 ) ) ;
#116748 = CARTESIAN_POINT ( 'NONE',  ( -2.625475302540713152, 6.214804952939456228, -0.7998128361456281477 ) ) ;
#116747 = AXIS2_PLACEMENT_3D ( 'NONE', #39046, #5437, #188486 ) ;
#116749 = CARTESIAN_POINT ( 'NONE',  ( 5.933664784275179294, 10.07435934829639912, -0.7998128361456291469 ) ) ;
#116750 = CARTESIAN_POINT ( 'NONE',  ( 1.360316468749957597, 1.276041667008120051, 0.7853790794158581612 ) ) ;
#116751 = CARTESIAN_POINT ( 'NONE',  ( 5.029711800545521250, 5.930713857800314237, -1.082531754730549078 ) ) ;
#116752 = DIRECTION ( 'NONE',  ( 0.000000000000000000, 0.000000000000000000, 1.000000000000000000 ) ) ;
#116753 = CARTESIAN_POINT ( 'NONE',  ( 7.695155468110882246, 14.38165973575666179, -9.208594225262938693 ) ) ;
#116754 = CARTESIAN_POINT ( 'NONE',  ( -0.006632162239710717895, -1.840811702136424088, -0.04651623371411393176 ) ) ;
#116755 = ORIENTED_EDGE ( 'NONE', *, *, #125943, .F. ) ;
#116756 = VECTOR ( 'NONE', #207174, 1000.000000000000000 ) ;
#116757 = CARTESIAN_POINT ( 'NONE',  ( 3.901501827272614964, -0.5455803081039903857, 1.789184164884791706 ) ) ;
#116758 = CARTESIAN_POINT ( 'NONE',  ( 6.749980374757213575, 8.968339418673846097, 1.599625672291268286 ) ) ;
#116759 = CARTESIAN_POINT ( 'NONE',  ( -1.499999999999995781, 8.627523663848661428, -2.579999999999989413 ) ) ;
#116760 = B_SPLINE_CURVE_WITH_KNOTS ( 'NONE', 3,
 ( #178738, #177670, #140934, #79082, #145201, #141999, #211207, #128992, #43413, #99600 ),
 .UNSPECIFIED., .F., .F.,
 ( 4, 3, 3, 4 ),
 ( 4.570397642887432356E-18, 3.125189670681054644E-05, 5.835922535859565738E-05, 8.547800541132622365E-05 ),
 .UNSPECIFIED. ) ;
#116761 = ADVANCED_FACE ( 'NONE', ( #115792 ), #104871, .T. ) ;
#116762 = CARTESIAN_POINT ( 'NONE',  ( -7.402388683381436074, 7.738467673474211495, 0.7216878364870317197 ) ) ;
#116763 = CARTESIAN_POINT ( 'NONE',  ( 5.996784015946103885, 5.890669528225568996, 1.040834085586084257E-14 ) ) ;
#116764 = CARTESIAN_POINT ( 'NONE',  ( 6.649288540346695697, 1.804226486660088558, -1.015068834323729297 ) ) ;
#116765 = CARTESIAN_POINT ( 'NONE',  ( 2.249625261780491936, 1.976952429928409805, -0.3961248688731587309 ) ) ;
#116766 = CARTESIAN_POINT ( 'NONE',  ( -8.993135964566285168, 9.386413468282476913, -0.7998128361456291469 ) ) ;
#116767 = CARTESIAN_POINT ( 'NONE',  ( 5.830888582329017744, 8.960397891762626799, -1.199719254218452047 ) ) ;
#116768 = CARTESIAN_POINT ( 'NONE',  ( -11.86239285000045918, 11.37999999999999901, -1.812080536912752837 ) ) ;
#116769 = CIRCLE ( 'NONE', #120199, 2.000000000000000000 ) ;
#116770 = CARTESIAN_POINT ( 'NONE',  ( 2.449409141518565480, 0.5832169002529237201, -2.112351429719904861 ) ) ;
#116771 = CARTESIAN_POINT ( 'NONE',  ( 6.041596546049881944, -1.325759876995153075, -1.255439798616593716 ) ) ;
#116772 = CARTESIAN_POINT ( 'NONE',  ( -4.406563619641430840, 5.099744630125142564, -1.199719254218446718 ) ) ;
#116773 = DIRECTION ( 'NONE',  ( 1.000000000000000000, -8.673617379884035472E-16, 0.000000000000000000 ) ) ;
#116774 = CARTESIAN_POINT ( 'NONE',  ( 5.289089323106923146, 6.303597310780433283, -1.082531754730548412 ) ) ;
#116775 = CARTESIAN_POINT ( 'NONE',  ( 9.043452155515161905, 10.50944792197790889, 1.199719254218453823 ) ) ;
#116776 = CARTESIAN_POINT ( 'NONE',  ( 2.367870383881045981, 5.914265881169853856, 0.000000000000000000 ) ) ;
#116777 = CARTESIAN_POINT ( 'NONE',  ( 5.722950238744187956, 9.690876021928001904, 0.7216878364870317197 ) ) ;
#116778 = VERTEX_POINT ( 'NONE', #174827 ) ;
#116780 = CARTESIAN_POINT ( 'NONE',  ( 0.4166524477783914437, -0.6801522605285510448, -1.894826352922045487 ) ) ;
#116779 = CARTESIAN_POINT ( 'NONE',  ( 4.229911503591711863, 1.806553461410321582, 0.3548724298726435022 ) ) ;
#116781 = CARTESIAN_POINT ( 'NONE',  ( 2.882471369727876542, -0.2278316040762885242, 2.287086785078895179 ) ) ;
#116783 = CARTESIAN_POINT ( 'NONE',  ( 1.463465096324652714, -0.4588509492367858766, 1.803342318195770178 ) ) ;
#116782 = CARTESIAN_POINT ( 'NONE',  ( 4.202664430556261266, 4.005456045178151570, 0.7216878364870317197 ) ) ;
#116784 = CARTESIAN_POINT ( 'NONE',  ( -1.737499999999997824, -0.2916666666666657415, 3.009438278150925683 ) ) ;
#116785 = CARTESIAN_POINT ( 'NONE',  ( -2.981903720001798597, 5.566305875722335372, -1.199719254218446718 ) ) ;
#116786 = DIRECTION ( 'NONE',  ( -5.578564026256490882E-16, -1.000000000000000000, -9.066213480720158442E-32 ) ) ;
#116787 = CARTESIAN_POINT ( 'NONE',  ( 4.957238921819991262, -1.637161358497842389, 0.9882132959125531357 ) ) ;
#116788 = CARTESIAN_POINT ( 'NONE',  ( -9.833741488613570780, 10.36711991300432345, 0.7998128361456462443 ) ) ;
#116789 = CARTESIAN_POINT ( 'NONE',  ( 6.176125489850557315, 6.957122458884915872, -0.8945188991977878201 ) ) ;
#116790 = CARTESIAN_POINT ( 'NONE',  ( -5.912764389335557702, 8.951956649983198844, 1.082531754730550855 ) ) ;
#116792 = CARTESIAN_POINT ( 'NONE',  ( 2.078771448894382701, -0.08914341469279044028, -1.868647664167771616 ) ) ;
#116791 = CARTESIAN_POINT ( 'NONE',  ( 3.825792374969799514, 1.116656699807290432, -1.767364921024146218 ) ) ;
#116793 = CARTESIAN_POINT ( 'NONE',  ( 8.283668668269706714, 8.766627655843892697, 1.040834085586084257E-14 ) ) ;
#116794 = CARTESIAN_POINT ( 'NONE',  ( -1.201851678989727383E-14, 5.509375000341415252, -1.575800808251660134 ) ) ;
#116795 = CARTESIAN_POINT ( 'NONE',  ( 6.075717905342373548, -0.9791751913862613010, 1.559117742379905858 ) ) ;
#116796 = CARTESIAN_POINT ( 'NONE',  ( 2.849184837166184536, 6.475799410002530898, 0.7998128361456362523 ) ) ;
#116797 = CARTESIAN_POINT ( 'NONE',  ( 5.605114358992040913, 6.317488171369740613, -1.123711807521186490 ) ) ;
#116798 = CARTESIAN_POINT ( 'NONE',  ( 4.107791765966132047, -1.720061694268668395, 0.1296855704675456133 ) ) ;
#116799 = CARTESIAN_POINT ( 'NONE',  ( -7.725448601688521322, 7.907444878258402809, 1.040834085586084257E-14 ) ) ;
#116800 = CARTESIAN_POINT ( 'NONE',  ( 0.6681306116654138760, 1.163384174638517177, 1.286150249643343901 ) ) ;
#116801 = CARTESIAN_POINT ( 'NONE',  ( 1.436716030283395895, 7.421837552815621741, 4.237608343040937697 ) ) ;
#116802 = CARTESIAN_POINT ( 'NONE',  ( 9.578539647746881158, -9.962495449538966596, -0.1460552299441071622 ) ) ;
#116803 = CARTESIAN_POINT ( 'NONE',  ( 4.575155497752975364, 1.982410897724752319, 0.8856408146403412784 ) ) ;
#116804 = CARTESIAN_POINT ( 'NONE',  ( 3.844227010333609584, 1.817057058749595777, 0.1772887374331885701 ) ) ;
#116805 = CARTESIAN_POINT ( 'NONE',  ( 1.446067858876250112, -0.8869304882095051523, 1.749921244195346004 ) ) ;
#116806 = CARTESIAN_POINT ( 'NONE',  ( 5.208266738515407113, 1.258803676730145371, -1.702402541353124077 ) ) ;
#116807 = ORIENTED_EDGE ( 'NONE', *, *, #10571, .F. ) ;
#116809 = CARTESIAN_POINT ( 'NONE',  ( -0.6823417656249969321, 4.530208333674755394, -1.181850606188749264 ) ) ;
#116808 = CARTESIAN_POINT ( 'NONE',  ( 5.812145867431055102, 1.542159960141289199, -1.696276722712148688 ) ) ;
#116810 = CARTESIAN_POINT ( 'NONE',  ( 9.565441069641300587, 11.11843498845840905, -1.199719254218440723 ) ) ;
#116811 = CARTESIAN_POINT ( 'NONE',  ( 1.471502243059899850, -1.820439715282649251, -1.087164402369590555 ) ) ;
#116812 = CARTESIAN_POINT ( 'NONE',  ( -4.853455804012230423, 6.685451076146141425, 1.443375672974064550 ) ) ;
#116813 = CARTESIAN_POINT ( 'NONE',  ( 2.684151225825664788, 5.114964949229812596, -1.082531754730543083 ) ) ;
#116814 = CARTESIAN_POINT ( 'NONE',  ( -4.406036734316890247, 7.123831375802920363, -1.082531754730548412 ) ) ;
#116815 = CARTESIAN_POINT ( 'NONE',  ( 6.086835205273840366, 2.090220906010348045, 0.5866831100012849243 ) ) ;
#116817 = CARTESIAN_POINT ( 'NONE',  ( -1.402160292154681736E-14, 12.59375000068279959, 1.732050807568881190 ) ) ;
#116816 = CARTESIAN_POINT ( 'NONE',  ( 6.983263157960365675, 2.037486384657179350, 2.358487060789053569 ) ) ;
#116819 = EDGE_LOOP ( 'NONE', ( #52365, #65335, #98281 ) ) ;
#116818 = CARTESIAN_POINT ( 'NONE',  ( 0.8564553275840697255, 0.8952667643853294832, -2.033071718549640305 ) ) ;
#116820 = CARTESIAN_POINT ( 'NONE',  ( 6.047500043413473136, -1.423963828944514010, 1.427935028000301809 ) ) ;
#116822 = CARTESIAN_POINT ( 'NONE',  ( 4.434473652564925317, -1.191674006009019404, 1.683292407194038054 ) ) ;
#116821 = CARTESIAN_POINT ( 'NONE',  ( 4.090809663021327758, 5.795697244990093644, 1.599625672291267398 ) ) ;
#116824 = CARTESIAN_POINT ( 'NONE',  ( 3.475000000000000533, -3.675000000000001155, 0.000000000000000000 ) ) ;
#116823 = CARTESIAN_POINT ( 'NONE',  ( 7.126746022638799971, 8.343567110280638133, 1.199719254218452047 ) ) ;
#116825 = CARTESIAN_POINT ( 'NONE',  ( 4.199993725183334803, 8.122019456014369254, -0.7998128361456362523 ) ) ;
#116826 = CARTESIAN_POINT ( 'NONE',  ( -3.285556943750000514, -3.026041666188709733, -1.896917185911906500 ) ) ;
#116827 = CARTESIAN_POINT ( 'NONE',  ( 1.284279953904125193, 3.003360285806104368, 0.7750000000000065725 ) ) ;
#116828 = CARTESIAN_POINT ( 'NONE',  ( 0.05869050280414740001, -1.868530317513932504, -0.9378765995749788198 ) ) ;
#116829 = CARTESIAN_POINT ( 'NONE',  ( 4.201796189063250253, 1.844709454618495670, 0.8146275914719460776 ) ) ;
#116830 = CARTESIAN_POINT ( 'NONE',  ( 3.966218424140379728, -1.719484690100345325, -0.6589542199007536460 ) ) ;
#116832 = ORIENTED_EDGE ( 'NONE', *, *, #19052, .F. ) ;
#116831 = CARTESIAN_POINT ( 'NONE',  ( 5.529027716274630855, 5.344953845275508542, 1.040834085586084257E-14 ) ) ;
#116833 =( LENGTH_UNIT ( ) NAMED_UNIT ( * ) SI_UNIT ( .MILLI., .METRE. ) );
#116834 = CARTESIAN_POINT ( 'NONE',  ( 2.027930484333416050, 0.9963118489298377067, -1.407687550210996230 ) ) ;
#116835 = CARTESIAN_POINT ( 'NONE',  ( 0.1984543448181053105, 1.387095780679182377, -1.463931301963219855 ) ) ;
#116836 = CARTESIAN_POINT ( 'NONE',  ( 1.723655420059172050, 2.274453554295458702, 0.3322429970207661509 ) ) ;
#116837 = CARTESIAN_POINT ( 'NONE',  ( -6.358937740009323214, 7.377514437221045718, -1.199719254218446718 ) ) ;
#116838 = CARTESIAN_POINT ( 'NONE',  ( 1.476233607035297490, 1.347422320225545089, 1.817282701917295240 ) ) ;
#116839 = CARTESIAN_POINT ( 'NONE',  ( 3.703829026103040434, -0.6115302605771840705, 2.015330080423376913 ) ) ;
#116840 = CARTESIAN_POINT ( 'NONE',  ( -4.984557751679625781, 5.844347460828191565, 1.199719254218452935 ) ) ;
#116841 = CARTESIAN_POINT ( 'NONE',  ( 7.786460292950004636, 7.978625184730144149, 1.040834085586084257E-14 ) ) ;
#116842 = CARTESIAN_POINT ( 'NONE',  ( 4.529832720297257254, 8.298905583739861314, 0.000000000000000000 ) ) ;
#116843 = CARTESIAN_POINT ( 'NONE',  ( 6.156250000000002665, -1.895863743163982207, 0.7852924748303072855 ) ) ;
#116844 = CARTESIAN_POINT ( 'NONE',  ( -5.280010757518168063, 8.247430752824802980, -1.199719254218446718 ) ) ;
#116845 = CARTESIAN_POINT ( 'NONE',  ( -1.402160292154681736E-14, 1.587500000000018785, -1.732050807568863648 ) ) ;
#116846 = CARTESIAN_POINT ( 'NONE',  ( -3.704402285031864306, 5.344888637335695414, -1.599625672291256295 ) ) ;
#116847 = CARTESIAN_POINT ( 'NONE',  ( 4.887093103977882436, -2.092044318328468488, -0.7474293538695072625 ) ) ;
#116848 = CARTESIAN_POINT ( 'NONE',  ( 3.310656966840678894, 1.981231107410564851, 0.9368519390955745152 ) ) ;
#116849 = CARTESIAN_POINT ( 'NONE',  ( -5.762378981008047241, 6.681529218386182301, 1.199719254218450271 ) ) ;
#116850 = CARTESIAN_POINT ( 'NONE',  ( -5.320648938720212051, 5.172121614787156929, 0.000000000000000000 ) ) ;
#116851 = CARTESIAN_POINT ( 'NONE',  ( 0.6823417656249882723, 2.926041667008084879, -1.181850606188754593 ) ) ;
#116852 = CARTESIAN_POINT ( 'NONE',  ( 6.610000000000010090, 4.687934210475516394, 2.842562027763709587 ) ) ;
#116853 = CARTESIAN_POINT ( 'NONE',  ( -5.639828713604883248, 6.642516923036197340, 1.082531754730548412 ) ) ;
#116855 = CARTESIAN_POINT ( 'NONE',  ( 5.203433420164765622, 1.869144303625443371, -1.001675624404389620 ) ) ;
#116854 = CIRCLE ( 'NONE', #144525, 0.07999999999999946043 ) ;
#116856 = CARTESIAN_POINT ( 'NONE',  ( -6.943184063974178422, 8.233374508458908281, -1.082531754730549967 ) ) ;
#116857 = VERTEX_POINT ( 'NONE', #8011 ) ;
#116859 = CARTESIAN_POINT ( 'NONE',  ( 6.403215362905616992, 1.794359850238020693, 1.205212418099836480 ) ) ;
#116858 = CARTESIAN_POINT ( 'NONE',  ( -5.397554552016258889, 7.390509292142662723, 1.443375672974058777 ) ) ;
#116860 = CARTESIAN_POINT ( 'NONE',  ( 4.873266149108180123, 7.772895376346490970, 1.199719254218462483 ) ) ;
#116861 = CARTESIAN_POINT ( 'NONE',  ( 5.812015183962491172, 1.231757822100377320, -1.368757117762291253 ) ) ;
#116862 =( NAMED_UNIT ( * ) PLANE_ANGLE_UNIT ( ) SI_UNIT ( $, .RADIAN. ) );
#116863 = CARTESIAN_POINT ( 'NONE',  ( -1.201851678989727383E-14, 3.259375000341420581, -1.575800808251660134 ) ) ;
#116864 = CARTESIAN_POINT ( 'NONE',  ( 0.6787880507331369717, 1.167388449615349044, 1.291009837513588998 ) ) ;
#116865 = CARTESIAN_POINT ( 'NONE',  ( 3.009020027229115879, 5.597941567487558778, -1.199719254218446718 ) ) ;
#116866 = CARTESIAN_POINT ( 'NONE',  ( 11.41126283316774348, 12.34125393091539280, 3.405403429622879230 ) ) ;
#116867 = CARTESIAN_POINT ( 'NONE',  ( -1.364683531250000748, 0.3218750003414205807, 0.000000000000000000 ) ) ;
#116868 = DIRECTION ( 'NONE',  ( 0.000000000000000000, -1.000000000000000000, 0.000000000000000000 ) ) ;
#116869 = EDGE_CURVE ( 'NONE', #94313, #213798, #43758, .T. ) ;
#116870 = CARTESIAN_POINT ( 'NONE',  ( 5.331013795412237855, 0.1550192300789655642, 2.156197635354038411 ) ) ;
#116871 = CARTESIAN_POINT ( 'NONE',  ( -4.796887421136680985, 4.490790167614548523, 1.214306433183764966E-14 ) ) ;
#116872 = CARTESIAN_POINT ( 'NONE',  ( -6.005898860729463884, 9.950706404252290582, 0.7216878364870458196 ) ) ;
#116874 = AXIS2_PLACEMENT_3D ( 'NONE', #206222, #158559, #207294 ) ;
#116873 = CONICAL_SURFACE ( 'NONE', #179134, 10.99999999999999112, 0.7853981633974479459 ) ;
#116875 = CARTESIAN_POINT ( 'NONE',  ( 4.838837662799537753, 0.3661284547709364734, 2.130314178654398205 ) ) ;
#116876 = ORIENTED_EDGE ( 'NONE', *, *, #168793, .T. ) ;
#116877 = CARTESIAN_POINT ( 'NONE',  ( 1.364683531249988535, 2.613541667008089764, 0.7879004041258500513 ) ) ;
#116878 = CARTESIAN_POINT ( 'NONE',  ( 6.046159394557358624, 1.968988722785993462, 0.09938198387684710200 ) ) ;
#116879 = CARTESIAN_POINT ( 'NONE',  ( 5.589090328658773643, 1.030979737101325400, -1.393799353210682046 ) ) ;
#116881 = CARTESIAN_POINT ( 'NONE',  ( 2.050558489324630251, -1.691691439650149897, 1.393213601605561180 ) ) ;
#116880 = CARTESIAN_POINT ( 'NONE',  ( -3.355169270512988773E-14, -0.7968749996585455797, 1.570758158831762286 ) ) ;
#116882 = CARTESIAN_POINT ( 'NONE',  ( 2.714277975868684578, -2.282582259777651501, 0.3379699517906120110 ) ) ;
#116883 = CARTESIAN_POINT ( 'NONE',  ( 5.290332094886032621, -2.044729594613464041, -0.2563108835951214970 ) ) ;
#116884 = CARTESIAN_POINT ( 'NONE',  ( 0.4978614556471228081, -0.6533520819593687801, -1.828864621591755002 ) ) ;
#116885 = CARTESIAN_POINT ( 'NONE',  ( -6.195713011320783892, 10.17215624660883577, -0.7216878364870267237 ) ) ;
#116886 = CARTESIAN_POINT ( 'NONE',  ( -4.167152111353897403, 5.955039778036558040, 1.599625672291270506 ) ) ;
#116887 = CARTESIAN_POINT ( 'NONE',  ( -11.33772463945037146, 10.89999999999998259, 3.679999999999999272 ) ) ;
#116888 = CARTESIAN_POINT ( 'NONE',  ( 3.410498715577559015, -2.118327196165440185, -0.1003008382433126094 ) ) ;
#116889 =( NAMED_UNIT ( * ) SI_UNIT ( $, .STERADIAN. ) SOLID_ANGLE_UNIT ( ) );
#116890 = CARTESIAN_POINT ( 'NONE',  ( 1.301407962653992501, 1.352153127569672098, -1.496052916918483522 ) ) ;
#116891 = CARTESIAN_POINT ( 'NONE',  ( -6.846504384776765484, 8.050305206070113684, -1.082531754730543083 ) ) ;
#116892 = CARTESIAN_POINT ( 'NONE',  ( 4.366400497975233996, 1.037236317483503312, 1.947806255051434121 ) ) ;
#116893 = CARTESIAN_POINT ( 'NONE',  ( 1.642778471875001811, -2.530208332855374387, 2.845375778867859751 ) ) ;
#116894 = CARTESIAN_POINT ( 'NONE',  ( 2.254548712976621516, -0.4907705908011159579, -1.795021142807408543 ) ) ;
#116895 = CARTESIAN_POINT ( 'NONE',  ( 1.737500000000001155, -1.939583332377418978, 3.009438278150922130 ) ) ;
#116896 = CARTESIAN_POINT ( 'NONE',  ( -0.5773502691960585853, -4.295408888567775918, 1.000000000000000888 ) ) ;
#116897 = CARTESIAN_POINT ( 'NONE',  ( 0.000000000000000000, -4.500000000000003553, -1.359291649810836722 ) ) ;
#116899 = DIRECTION ( 'NONE',  ( -0.9999980456341537316, 0.000000000000000000, -0.001977050295958555567 ) ) ;
#116898 = CARTESIAN_POINT ( 'NONE',  ( -4.728114892278019177, 8.325812319508695936, -0.7463954279460782715 ) ) ;
#116900 = CARTESIAN_POINT ( 'NONE',  ( 1.224999999999955014, 2.145833333333346360, -0.7072540797573136917 ) ) ;
#116901 = ORIENTED_EDGE ( 'NONE', *, *, #113228, .F. ) ;
#116902 = CARTESIAN_POINT ( 'NONE',  ( 3.801680928091007772, -0.6000553829732765410, 1.971583879547859963 ) ) ;
#116903 = CARTESIAN_POINT ( 'NONE',  ( -0.6801582343750403048, 1.598958333674738164, -1.178068619123869398 ) ) ;
#116904 = CARTESIAN_POINT ( 'NONE',  ( -6.905180308061733996, 6.950465202360470052, 0.7998128361456341429 ) ) ;
#116905 = CARTESIAN_POINT ( 'NONE',  ( 3.844402842710480162, 1.078523329768014349, -1.707388236230653611 ) ) ;
#116906 = CARTESIAN_POINT ( 'NONE',  ( 1.499999999999987566, -0.4749999999999823808, 0.000000000000000000 ) ) ;
#116907 = CARTESIAN_POINT ( 'NONE',  ( 3.871016551901614200, 4.474939717762034697, -1.199719254218446718 ) ) ;
#116908 = CARTESIAN_POINT ( 'NONE',  ( 1.885689728351304995, 1.420446345011391553, 1.493427266136108322 ) ) ;
#116910 = CARTESIAN_POINT ( 'NONE',  ( 1.364683531249997417, 13.23437500034139980, 2.602085213965210642E-15 ) ) ;
#116909 = CARTESIAN_POINT ( 'NONE',  ( -9.495441445486415333, 15.17076627066290229, -7.231220947886418671 ) ) ;
#116911 = CARTESIAN_POINT ( 'NONE',  ( 4.496500501226593727, 8.397667684739696270, 0.7998128361456462443 ) ) ;
#116913 = EDGE_LOOP ( 'NONE', ( #86852, #158912, #34659, #206099 ) ) ;
#116912 = CARTESIAN_POINT ( 'NONE',  ( -0.1408020194050510487, 6.947782644136224484, -2.695327183700791274 ) ) ;
#116914 = CARTESIAN_POINT ( 'NONE',  ( 1.112948326906910035, -1.796673262952220629, 0.4014371099074555693 ) ) ;
#116915 = CARTESIAN_POINT ( 'NONE',  ( 5.321004863918796346, 2.037934703285459115, 0.8473243778325880715 ) ) ;
#116916 = CARTESIAN_POINT ( 'NONE',  ( 6.200875153403774043, 8.327716660428123419, -1.599625672291283607 ) ) ;
#116917 = CARTESIAN_POINT ( 'NONE',  ( 1.915512222264357467, -0.2666219456287990952, 2.145042957367573777 ) ) ;
#116918 = CARTESIAN_POINT ( 'NONE',  ( -4.446711195602255806, 5.250546485366484717, -1.082531754730544860 ) ) ;
#116919 = CARTESIAN_POINT ( 'NONE',  ( 2.342982756445275427, -1.756855002775299379, -0.9896843009072553432 ) ) ;
#116920 = VECTOR ( 'NONE', #144180, 1000.000000000000227 ) ;
#116921 = CARTESIAN_POINT ( 'NONE',  ( -1.734723475976807094E-15, -6.054403199333757257, -10.91970695577494332 ) ) ;
#116922 = CARTESIAN_POINT ( 'NONE',  ( 0.4439547499465161251, 1.865322535695708606, 0.1421067652795371117 ) ) ;
#116923 = DIRECTION ( 'NONE',  ( -1.000000000000000000, 1.016547956922408957E-15, 1.479114432388267300E-31 ) ) ;
#116924 = CARTESIAN_POINT ( 'NONE',  ( 4.030118584743531684, 1.055711351780568741, -1.664808796107832389 ) ) ;
#116925 = CARTESIAN_POINT ( 'NONE',  ( 2.975796278104340331, -0.8128168404246680634, 1.845627246706407210 ) ) ;
#116928 = ADVANCED_FACE ( 'NONE', ( #206216, #76225, #59977, #160685 ), #144479, .T. ) ;
#116927 = CARTESIAN_POINT ( 'NONE',  ( 8.988692655735958326, 12.47026328412523988, -1.082531754730543083 ) ) ;
#116926 = CARTESIAN_POINT ( 'NONE',  ( -1.364683531250012516, 2.280208333674751842, 0.7879004041258379498 ) ) ;
#116930 = CARTESIAN_POINT ( 'NONE',  ( 6.235009869002534622, 0.2045095422857303724, 2.096118580758222549 ) ) ;
#116929 = CARTESIAN_POINT ( 'NONE',  ( -8.525379664894808585, 8.840697785332414682, -0.7998128361456291469 ) ) ;
#116931 = CARTESIAN_POINT ( 'NONE',  ( 5.863751307568212390, -0.5067217619753560109, 2.007263066363853987 ) ) ;
#116932 = CARTESIAN_POINT ( 'NONE',  ( 5.296431564432884542, 9.330920591813708143, 1.040834085586084257E-14 ) ) ;
#116933 = CARTESIAN_POINT ( 'NONE',  ( -6.795661308947694934, 8.951357498570873261, -1.599625672291263179 ) ) ;
#116934 = CARTESIAN_POINT ( 'NONE',  ( 5.220965578766386450, 1.526617224004393369, -1.322549803791906786 ) ) ;
#116935 = CARTESIAN_POINT ( 'NONE',  ( -1.402160292154681736E-14, -0.7562499993171803991, 1.732050807568877637 ) ) ;
#116936 = CARTESIAN_POINT ( 'NONE',  ( 0.5673240888519160974, 1.792687530798135143, 1.019967006830464706 ) ) ;
#116937 = CARTESIAN_POINT ( 'NONE',  ( 8.975134502566660899, 10.53370701015836275, -1.082531754730543083 ) ) ;
#116938 = CARTESIAN_POINT ( 'NONE',  ( 7.367930134383754215, 7.560616343061329125, -0.7998128361456341429 ) ) ;
#116939 = CARTESIAN_POINT ( 'NONE',  ( 4.064412189046650248, 7.963840997188264659, 0.7998128361456271485 ) ) ;
#116940 = CARTESIAN_POINT ( 'NONE',  ( 0.6823417656249899377, 0.9052083336747520637, 1.181850606188755259 ) ) ;
#116942 = CARTESIAN_POINT ( 'NONE',  ( 6.727182134110195832, 0.008744176509076214548, 1.710970312420513784 ) ) ;
#116941 = CARTESIAN_POINT ( 'NONE',  ( 3.854260808034858155, 7.718664386007802136, -0.7998128361456362523 ) ) ;
#116943 = CARTESIAN_POINT ( 'NONE',  ( 5.626270559546804328, 9.507806719539201978, 0.7216878364870438212 ) ) ;
#116945 = FACE_OUTER_BOUND ( 'NONE', #103606, .T. ) ;
#116944 = CARTESIAN_POINT ( 'NONE',  ( 2.981114689849233113, 2.043561189653697152, 0.7337040362941152916 ) ) ;
#116946 = CARTESIAN_POINT ( 'NONE',  ( -0.8870621307506136866, -0.8887487162373149951, -3.171027839057565689 ) ) ;
#116948 = CARTESIAN_POINT ( 'NONE',  ( 2.981803241483144351, -1.814435276338403735, -0.3121031562058202424 ) ) ;
#116947 = CARTESIAN_POINT ( 'NONE',  ( -5.612712406377534435, 5.650512016969639895, 0.7216878364870317197 ) ) ;
#116949 = B_SPLINE_CURVE_WITH_KNOTS ( 'NONE', 3,
 ( #191280, #175072, #26659, #90624, #110123, #158807, #192346, #44004 ),
 .UNSPECIFIED., .F., .F.,
 ( 4, 2, 2, 4 ),
 ( 1.068270986634163351E-15, 0.0004443203323512407137, 0.0006664804985263248242, 0.0008886406647014088262 ),
 .UNSPECIFIED. ) ;
#116950 = CARTESIAN_POINT ( 'NONE',  ( -1.364683531250012516, 4.488541667008090208, -0.7879004041258300672 ) ) ;
#116951 = CARTESIAN_POINT ( 'NONE',  ( 4.616832073239669043, -0.1072513232249286408, 2.189039617437993357 ) ) ;
#116952 = LINE ( 'NONE', #102780, #195408 ) ;
#116953 = CARTESIAN_POINT ( 'NONE',  ( 5.401357799220028788, 1.846321421614788516, 1.307461012187713933 ) ) ;
#116954 = CARTESIAN_POINT ( 'NONE',  ( -6.254388934605767503, 6.191208599995166040, 0.7998128361456341429 ) ) ;
#116955 = CARTESIAN_POINT ( 'NONE',  ( -5.989290089449875509, 6.089315518664643712, -0.6934025848366349720 ) ) ;
#116956 = CARTESIAN_POINT ( 'NONE',  ( 4.616554244727909762, 8.463227371007752353, -0.2998622348379786362 ) ) ;
#116957 = CARTESIAN_POINT ( 'NONE',  ( -5.926322542504872892, 8.007405281046052536, -1.443375672974066548 ) ) ;
#116958 = CARTESIAN_POINT ( 'NONE',  ( 5.289089323106923146, 6.303597310780433283, -1.082531754730548412 ) ) ;
#116959 =( BOUNDED_SURFACE ( )  B_SPLINE_SURFACE ( 3, 2, ( 
 ( #202956, #56733, #25290 ),
 ( #71885, #157451, #9045 ),
 ( #40497, #120745, #37277 ),
 ( #104423, #170471, #5809 ) ),
 .UNSPECIFIED., .F., .F., .T. ) 
 B_SPLINE_SURFACE_WITH_KNOTS ( ( 4, 4 ),
 ( 3, 3 ),
 ( 0.06089844177390838637, 0.06334004522945697879 ),
 ( 0.000000000000000000, 1.000000000000000000 ),
 .UNSPECIFIED. ) 
 GEOMETRIC_REPRESENTATION_ITEM ( )  RATIONAL_B_SPLINE_SURFACE ( (
 ( 1.000000000000000000, 0.7169884966214686850, 1.000000000000000000),
 ( 1.000000000000000000, 0.7174883642159506358, 1.000000000000000000),
 ( 1.000000000000000000, 0.7180610417775397103, 1.000000000000000000),
 ( 1.000000000000000000, 0.7187540717311186045, 1.000000000000000000) ) ) 
 REPRESENTATION_ITEM ( '' )  SURFACE ( )  );
#116960 = CARTESIAN_POINT ( 'NONE',  ( 6.450471989241519211, 0.5578098333037047052, 1.679625245746432016 ) ) ;
#116961 = CARTESIAN_POINT ( 'NONE',  ( 4.037747573665031453, -1.925786081212683465, 0.5863696817766034242 ) ) ;
#116962 = CARTESIAN_POINT ( 'NONE',  ( 7.253775878511261155, 8.421492265473332850, 1.199719254218462483 ) ) ;
#116963 = CARTESIAN_POINT ( 'NONE',  ( 3.434694453818935678, 2.054221006159732354, 0.4631738978765443382 ) ) ;
#116964 = CARTESIAN_POINT ( 'NONE',  ( 0.9838322988516207124, -1.915793139027978542, 0.001352086710114385869 ) ) ;
#116966 = CARTESIAN_POINT ( 'NONE',  ( -1.500000000000013101, 2.420833333333359150, 0.8660254037844403729 ) ) ;
#116965 = CARTESIAN_POINT ( 'NONE',  ( 0.6823417656249969321, 11.52604166700806765, -1.181850606188757036 ) ) ;
#116967 = CARTESIAN_POINT ( 'NONE',  ( 2.172252323668334206, -0.9256296301539097549, -1.738465135635240522 ) ) ;
#116968 = CIRCLE ( 'NONE', #137802, 0.07999999999999940492 ) ;
#116969 = CARTESIAN_POINT ( 'NONE',  ( 0.2681426532152464959, -1.225442487749365483, 1.413462724991432218 ) ) ;
#116970 = CARTESIAN_POINT ( 'NONE',  ( 0.9944974185457016169, 1.932217576897478528, 0.3389098420027157332 ) ) ;
#116972 = VERTEX_POINT ( 'NONE', #209403 ) ;
#116971 = CARTESIAN_POINT ( 'NONE',  ( 0.6504702201592416078, 1.884490048413577368, 0.3244712162126031085 ) ) ;
#116973 = CARTESIAN_POINT ( 'NONE',  ( 4.338245966692901412, 8.005111361209628740, -0.7216878364870197293 ) ) ;
#116974 = CARTESIAN_POINT ( 'NONE',  ( -1.402160292154681736E-14, 0.1343750003414218575, 1.575800808251672791 ) ) ;
#116975 = CARTESIAN_POINT ( 'NONE',  ( 5.594569530875261876, -0.4557361262383099465, -1.814172972432124498 ) ) ;
#116976 = CARTESIAN_POINT ( 'NONE',  ( 8.866142388332804103, 12.43125098877526113, -1.199719254218446718 ) ) ;
#116977 = DIRECTION ( 'NONE',  ( 0.000000000000000000, 0.000000000000000000, -1.000000000000000000 ) ) ;
#116978 = CARTESIAN_POINT ( 'NONE',  ( 6.139524545372063713, 1.915082402702467101, -0.7868883245659707981 ) ) ;
#116979 = CARTESIAN_POINT ( 'NONE',  ( 0.2212536527127808295, -1.848710500310095872, -0.9322282823912150240 ) ) ;
#116980 = CARTESIAN_POINT ( 'NONE',  ( 0.7499999999999885647, 1.066666666666687968, -1.299038105676652899 ) ) ;
#116981 = CARTESIAN_POINT ( 'NONE',  ( 7.613066949273408213, 8.840665181362512115, -1.199719254218441611 ) ) ;
#116982 = CARTESIAN_POINT ( 'NONE',  ( -8.690940161559884913, 10.09818392903003748, 1.199719254218462483 ) ) ;
#116983 = CARTESIAN_POINT ( 'NONE',  ( 4.694866332082116678, 8.699370830729650450, 0.7998128361456341429 ) ) ;
#116984 = CARTESIAN_POINT ( 'NONE',  ( 1.364683531249986537, 0.8635416670080893198, 0.7879004041258500513 ) ) ;
#116985 = CARTESIAN_POINT ( 'NONE',  ( -0.7500000000000215383, 2.691666666666689522, 1.299038105676671107 ) ) ;
#116987 = CARTESIAN_POINT ( 'NONE',  ( 5.169736645512481132, 4.925780929386339935, 0.7998128361456341429 ) ) ;
#116986 = CARTESIAN_POINT ( 'NONE',  ( 5.740667459973674447, -1.913685094937540132, -0.4313615418530327150 ) ) ;
#116988 = CARTESIAN_POINT ( 'NONE',  ( 3.057970071934034362, 1.730601471501746147, -1.034006501934421784 ) ) ;
#116989 = CARTESIAN_POINT ( 'NONE',  ( 4.206187189226945122, 1.174002167177927713, -1.513781418528682643 ) ) ;
#116990 = CARTESIAN_POINT ( 'NONE',  ( 11.84103413958613160, 9.989955215268565780, -1.443924719788771682 ) ) ;
#116991 = CARTESIAN_POINT ( 'NONE',  ( 1.400213348495438437, -0.7931047570679079506, -2.043190674350242819 ) ) ;
#116992 = CARTESIAN_POINT ( 'NONE',  ( 0.1333692844072559003, 2.872395615372814515, -2.542035612928101873 ) ) ;
#116993 = CARTESIAN_POINT ( 'NONE',  ( 3.672993792711932048, 0.04889617625786558258, -1.870083761627352015 ) ) ;
#116994 = CARTESIAN_POINT ( 'NONE',  ( 0.7499999999999867883, -0.4020833326505157679, -1.299038105676652899 ) ) ;
#116995 = CARTESIAN_POINT ( 'NONE',  ( -8.369460898337653276, 8.658792557682392754, 0.7998128361456462443 ) ) ;
#116997 = CARTESIAN_POINT ( 'NONE',  ( 4.288735948182021751, 1.635604132441673020, -1.344385869115312770 ) ) ;
#116996 = CARTESIAN_POINT ( 'NONE',  ( -4.446711195602255806, 5.250546485366484717, -1.082531754730544860 ) ) ;
#116999 = EDGE_CURVE ( 'NONE', #109538, #107567, #149128, .T. ) ;
#116998 = CARTESIAN_POINT ( 'NONE',  ( 0.6823417656249934904, 8.755208333674733723, 1.181850606188764807 ) ) ;
#117000 = CARTESIAN_POINT ( 'NONE',  ( 6.250451049865752395, -2.060019788584551481, -0.2068627631737207651 ) ) ;
#117002 = CARTESIAN_POINT ( 'NONE',  ( 6.620655732516648406, 3.679503859435423241, 2.787618683092321969 ) ) ;
#117001 = CARTESIAN_POINT ( 'NONE',  ( 2.050439074220523406, -1.614099552242785895, 1.328842424969446823 ) ) ;
#117004 = EDGE_LOOP ( 'NONE', ( #145416, #201101, #72759, #186813 ) ) ;
#117003 = CARTESIAN_POINT ( 'NONE',  ( 0.9028307623185973796, 1.406233313734496448, 0.9983791803314099322 ) ) ;
#117005 = CARTESIAN_POINT ( 'NONE',  ( 5.612185521052973414, 8.634967976948757951, -1.199719254218440723 ) ) ;
#117006 = CARTESIAN_POINT ( 'NONE',  ( 7.637366960813559480, 15.45595454679949832, 9.257485277755282738 ) ) ;
#117007 = CARTESIAN_POINT ( 'NONE',  ( 1.499999999999985789, -1.099999999999982991, 0.000000000000000000 ) ) ;
#117008 = CARTESIAN_POINT ( 'NONE',  ( -10.33392256004288079, 4.765625372279607141, 5.445010993851796322 ) ) ;
#117010 = CARTESIAN_POINT ( 'NONE',  ( 7.415946836550722843, 8.714654733139752807, 1.082531754730558626 ) ) ;
#117009 = CARTESIAN_POINT ( 'NONE',  ( 7.955937213120826357, 8.176348258262782664, 0.7998128361456481317 ) ) ;
#117011 = CARTESIAN_POINT ( 'NONE',  ( -2.837146587356454752, 6.532031128549641075, -0.3849993420583495141 ) ) ;
#117013 = CARTESIAN_POINT ( 'NONE',  ( 0.5042037957796470238, -1.797571035118279870, -0.2231917716723781087 ) ) ;
#117012 = CARTESIAN_POINT ( 'NONE',  ( 5.993586425693011144, 9.150212042353954800, -1.199719254218452047 ) ) ;
#117014 = CARTESIAN_POINT ( 'NONE',  ( -7.867809214632013770, 8.073532260025807261, 1.040834085586084257E-14 ) ) ;
#117015 =( BOUNDED_SURFACE ( )  B_SPLINE_SURFACE ( 3, 2, ( 
 ( #162663, #14232, #146428 ),
 ( #212442, #136556, #21682 ),
 ( #125447, #169035, #201509 ),
 ( #141657, #185272, #207669 ),
 ( #3309, #167974, #36895 ),
 ( #69379, #37977, #175200 ),
 ( #184208, #121444, #104050 ),
 ( #135487, #134446, #118222 ) ),
 .UNSPECIFIED., .F., .F., .T. ) 
 B_SPLINE_SURFACE_WITH_KNOTS ( ( 4, 2, 2, 4 ),
 ( 3, 3 ),
 ( -5.421010862427522170E-20, 0.0004401918256853618126, 0.0006602877385280428273, 0.0008803836513707237335 ),
 ( 0.000000000000000000, 1.000000000000000000 ),
 .UNSPECIFIED. ) 
 GEOMETRIC_REPRESENTATION_ITEM ( )  RATIONAL_B_SPLINE_SURFACE ( (
 ( 1.000000000000000000, 0.6787756258918289376, 1.000000000000000000),
 ( 1.000000000000000000, 0.6284487096095630054, 1.000000000000000000),
 ( 1.000000000000000000, 0.5704014816688967038, 1.000000000000000000),
 ( 1.000000000000000000, 0.4882303283126627758, 1.000000000000000000),
 ( 1.000000000000000000, 0.4617370933882599671, 1.000000000000000000),
 ( 1.000000000000000000, 0.4222438920368223325, 1.000000000000000000),
 ( 1.000000000000000000, 0.4105126989449003894, 1.000000000000000000),
 ( 1.000000000000000000, 0.4127341956165074266, 1.000000000000000000) ) ) 
 REPRESENTATION_ITEM ( '' )  SURFACE ( )  );
#117016 = AXIS2_PLACEMENT_3D ( 'NONE', #59971, #126125, #96776 ) ;
#117017 = CARTESIAN_POINT ( 'NONE',  ( 5.203632029546647608, 4.965325544092860532, 1.040834085586084257E-14 ) ) ;
#117018 = CARTESIAN_POINT ( 'NONE',  ( -6.370507937826336509, 6.842553425211714391, 0.6026486057824770315 ) ) ;
#117019 = CARTESIAN_POINT ( 'NONE',  ( 7.537407054554579489, 7.758339416593960536, 0.000000000000000000 ) ) ;
#117020 = B_SPLINE_CURVE_WITH_KNOTS ( 'NONE', 3,
 ( #140625, #189328, #107079, #109229, #40969, #92928, #124427, #42042, #108155, #25752 ),
 .UNSPECIFIED., .F., .F.,
 ( 4, 1, 1, 1, 1, 1, 1, 4 ),
 ( 0.000000000000000000, 0.09183773654504942541, 0.1838067853904964410, 0.2558923657893393822, 0.3606054339151033017, 0.5206678126786191685, 0.7335446035554463728, 1.000000000000000000 ),
 .UNSPECIFIED. ) ;
#117021 = CARTESIAN_POINT ( 'NONE',  ( 6.539320575229287336, 0.6031692783194403384, 1.851139666870088130 ) ) ;
#117022 = DIRECTION ( 'NONE',  ( 0.000000000000000000, -1.000000000000000000, 0.000000000000000000 ) ) ;
#117023 = CARTESIAN_POINT ( 'NONE',  ( -11.52483635780546578, 11.37999991357544438, 3.345866325258016083 ) ) ;
#117024 = CARTESIAN_POINT ( 'NONE',  ( 10.39874063200158893, 11.23421161353111586, 0.000000000000000000 ) ) ;
#117025 = EDGE_LOOP ( 'NONE', ( #108784, #194334, #81257, #25201 ) ) ;
#117026 = CARTESIAN_POINT ( 'NONE',  ( 2.910441987356562787, 0.6243205138760847817, 1.753359951907756065 ) ) ;
#117027 = CARTESIAN_POINT ( 'NONE',  ( 0.6498251619827577485, 0.9450094616851455465, 1.666218678892321226 ) ) ;
#117028 = CARTESIAN_POINT ( 'NONE',  ( 0.06529689308308950224, -1.700389599856198863, 1.266735544122286283 ) ) ;
#117029 = SURFACE_STYLE_USAGE ( .BOTH. , #97545 ) ;
#117031 = MECHANICAL_DESIGN_GEOMETRIC_PRESENTATION_REPRESENTATION (  '', ( #23569 ), #134319 ) ;
#117030 = COLOUR_RGB ( '', 0.08235294, 0.09019608, 0.10196078) ;
#117032 = DIRECTION ( 'NONE',  ( 0.000000000000000000, 0.000000000000000000, -1.000000000000000000 ) ) ;
#117033 = CARTESIAN_POINT ( 'NONE',  ( -1.522028533774275383, 8.691231065131706401, -2.524624912498922846 ) ) ;
#117034 = CARTESIAN_POINT ( 'NONE',  ( -4.772106882330247046, 4.669805572247793357, -0.7216878364870207285 ) ) ;
#117035 = CARTESIAN_POINT ( 'NONE',  ( 9.571693261567965294, 10.26932301469188857, 0.7216878364870438212 ) ) ;
#117036 = CARTESIAN_POINT ( 'NONE',  ( 4.469560827962531846, -0.3407972494764506810, 1.939574385640041809 ) ) ;
#117037 = CARTESIAN_POINT ( 'NONE',  ( 1.172698094321134477, 0.8626872041959358084, 1.937259058979395432 ) ) ;
#117038 = CARTESIAN_POINT ( 'NONE',  ( -6.552668314106420588, 6.539201209412602189, -0.7998128361456291469 ) ) ;
#117039 = FACE_OUTER_BOUND ( 'NONE', #152989, .T. ) ;
#117040 = CARTESIAN_POINT ( 'NONE',  ( -3.110417573979663342, 6.447385285496729956, -0.7441446434824240397 ) ) ;
#117041 = CARTESIAN_POINT ( 'NONE',  ( 5.964808794498537736, 0.1646014364122504459, -2.185315939793014639 ) ) ;
#117042 = CARTESIAN_POINT ( 'NONE',  ( 4.612281621929555264, -0.8233390244782293754, -1.741700550419862825 ) ) ;
#117043 = CARTESIAN_POINT ( 'NONE',  ( -7.100719765255177229, 9.307259030929609267, -1.599625672291263179 ) ) ;
#117044 = CARTESIAN_POINT ( 'NONE',  ( 0.07680821025393690105, 0.005952109439256307241, -1.810863387344714193 ) ) ;
#117045 = CARTESIAN_POINT ( 'NONE',  ( 1.331021600797330118, 2.127646391749141941, 0.5858054460900484761 ) ) ;
#117046 = ORIENTED_EDGE ( 'NONE', *, *, #190633, .F. ) ;
#117047 =( NAMED_UNIT ( * ) SI_UNIT ( $, .STERADIAN. ) SOLID_ANGLE_UNIT ( ) );
#117048 = ORIENTED_EDGE ( 'NONE', *, *, #101175, .F. ) ;
#117049 = CARTESIAN_POINT ( 'NONE',  ( 5.770349169015823954, -0.8820018971720828826, -1.760941755123719421 ) ) ;
#117050 = CARTESIAN_POINT ( 'NONE',  ( 1.329522225144257774, 0.9558622346672830394, -1.690450677827403103 ) ) ;
#117051 = CARTESIAN_POINT ( 'NONE',  ( 0.1458495181914116201, -0.1430550213798176262, -1.983920851313693223 ) ) ;
#117053 = CARTESIAN_POINT ( 'NONE',  ( 4.715577910371310466, 0.4106090485030155501, -1.814890118206938574 ) ) ;
#117052 = CARTESIAN_POINT ( 'NONE',  ( -6.444921918449773024, 8.612437886315108315, 1.599625672291269396 ) ) ;
#117054 = CARTESIAN_POINT ( 'NONE',  ( 5.176180785367283654, 9.260904359562321275, -0.7998128361456481317 ) ) ;
#117055 = DIRECTION ( 'NONE',  ( 0.000000000000000000, 0.000000000000000000, -1.000000000000000000 ) ) ;
#117056 = CARTESIAN_POINT ( 'NONE',  ( 1.523611765266693174, 0.5000000000000001110, -1.789163823896770200 ) ) ;
#117057 = CARTESIAN_POINT ( 'NONE',  ( -7.067878151425722955, 7.140279352951794500, 0.7998128361456341429 ) ) ;
#117058 = CARTESIAN_POINT ( 'NONE',  ( -3.327716440918550234, -0.9205823139102755626, 0.1123605076546999176 ) ) ;
#117059 = CARTESIAN_POINT ( 'NONE',  ( 0.5565083568685527116, -1.583368386835169783, 1.515454571103365344 ) ) ;
#117060 = CARTESIAN_POINT ( 'NONE',  ( 5.856759171423504107, 5.935233242856626568, -0.7216878364870257245 ) ) ;
#117061 = CARTESIAN_POINT ( 'NONE',  ( 0.4499999999999922395, 3.999999999999974243, -0.8338124244296039045 ) ) ;
#117062 = FACE_OUTER_BOUND ( 'NONE', #70118, .T. ) ;
#117063 = CARTESIAN_POINT ( 'NONE',  ( 1.769861954154128725, 0.9373860217288846330, 1.566528536362868707 ) ) ;
#117064 = CARTESIAN_POINT ( 'NONE',  ( -5.135841261478327979, 4.886236314679810455, 0.7998128361456341429 ) ) ;
#117065 = AXIS2_PLACEMENT_3D ( 'NONE', #109310, #111436, #110373 ) ;
#117066 = CARTESIAN_POINT ( 'NONE',  ( 3.146783715800211212, 0.7824046571166408670, 1.547702628640304168 ) ) ;
#117067 = CARTESIAN_POINT ( 'NONE',  ( 6.509000000000010111, 3.701365531483376881, 2.414445852726577080 ) ) ;
#117068 = CARTESIAN_POINT ( 'NONE',  ( 1.499999999999961364, 7.750000000000000000, -10.64483442802188762 ) ) ;
#117069 = CARTESIAN_POINT ( 'NONE',  ( -0.005450286198350333053, -0.4226363183827580583, -1.886779976948229853 ) ) ;
#117070 = CARTESIAN_POINT ( 'NONE',  ( 5.032062496497622384, 1.126290172248314514, 1.606047186625796819 ) ) ;
#117071 =( GEOMETRIC_REPRESENTATION_CONTEXT ( 3 ) GLOBAL_UNCERTAINTY_ASSIGNED_CONTEXT ( ( #213258 ) ) GLOBAL_UNIT_ASSIGNED_CONTEXT ( ( #16782, #82866, #195571 ) ) REPRESENTATION_CONTEXT ( 'NONE', 'WORKASPACE' ) );
#117072 = CARTESIAN_POINT ( 'NONE',  ( -7.232384877886063990, 10.52520055992070525, -1.199719254218446718 ) ) ;
#117073 = CARTESIAN_POINT ( 'NONE',  ( 6.962275575817444384, 8.081408578997208991, -1.199719254218446718 ) ) ;
#117074 = CARTESIAN_POINT ( 'NONE',  ( 4.336665864168765872, 1.303721989063952424, -1.672289659653345639 ) ) ;
#117075 = CARTESIAN_POINT ( 'NONE',  ( 6.424584688029230328, 8.588711117491191871, 1.599625672291268286 ) ) ;
#117076 = CARTESIAN_POINT ( 'NONE',  ( -9.671043645249580933, 10.17730576241299900, 0.7998128361456462443 ) ) ;
#117077 = CARTESIAN_POINT ( 'NONE',  ( 1.299038105676669330, 7.500000000000000000, -0.7500000000000006661 ) ) ;
#117078 = CARTESIAN_POINT ( 'NONE',  ( 2.500909639826456754, 0.4493149015136475022, 2.020762751476639529 ) ) ;
#117080 = CARTESIAN_POINT ( 'NONE',  ( 0.6823417656249882723, 0.2385416670080825474, -1.181850606188749264 ) ) ;
#117079 = CARTESIAN_POINT ( 'NONE',  ( 1.772826578343048798, 4.000000000000045297, -0.4500000000000284883 ) ) ;
#117081 = VERTEX_POINT ( 'NONE', #44825 ) ;
#117082 = CARTESIAN_POINT ( 'NONE',  ( 2.690384307321362467, 1.943607183752774636, 1.227106530010623864 ) ) ;
#117083 = CARTESIAN_POINT ( 'NONE',  ( 8.934460041725669655, 9.525884258209195821, 1.040834085586084257E-14 ) ) ;
#117085 = CARTESIAN_POINT ( 'NONE',  ( 3.285556943750000514, -2.413541666188708579, 1.896917185911906500 ) ) ;
#117084 = CARTESIAN_POINT ( 'NONE',  ( 4.913904330310220558, 4.697586238308844919, 0.000000000000000000 ) ) ;
#117086 = DIRECTION ( 'NONE',  ( 1.276756478318932585E-15, -1.000000000000000000, 1.665334536937738262E-16 ) ) ;
#117087 = EDGE_LOOP ( 'NONE', ( #53197, #157230, #20530, #95479 ) ) ;
#117088 = CARTESIAN_POINT ( 'NONE',  ( 0.07536363704235826688, -0.001874865094115066300, -2.144269471569634877 ) ) ;
#117089 = CARTESIAN_POINT ( 'NONE',  ( 3.603681638446740720, 1.388520161702249567, 1.315275747533505069 ) ) ;
#117090 = CARTESIAN_POINT ( 'NONE',  ( 0.000000000000000000, 0.4000000000000010214, 0.000000000000000000 ) ) ;
#117091 = CARTESIAN_POINT ( 'NONE',  ( 5.104412161113025093, -0.5839786719442441321, -1.623048794067801781 ) ) ;
#117092 = CARTESIAN_POINT ( 'NONE',  ( 3.063685658700274761, 1.282989771343697294, 1.555699169480361022 ) ) ;
#117093 = CARTESIAN_POINT ( 'NONE',  ( 4.746898448635796797, 2.273877242543398403, -0.3363112362181965853 ) ) ;
#117094 = CARTESIAN_POINT ( 'NONE',  ( -11.55950211276791073, 12.30000000000000071, -3.221476510067115662 ) ) ;
#117095 = CARTESIAN_POINT ( 'NONE',  ( 0.2763675079364875664, 1.274320874971252460, 1.801605125401319007 ) ) ;
#117096 = CARTESIAN_POINT ( 'NONE',  ( -4.014622883422329203, 6.737458226417744278, -1.082531754730546636 ) ) ;
#117097 = CARTESIAN_POINT ( 'NONE',  ( 5.553870903591159092, 1.767663364219349553, -0.08767779694792036949 ) ) ;
#117099 = CARTESIAN_POINT ( 'NONE',  ( 1.605870876717029549, -2.274517881136278508, 0.2841979012723067077 ) ) ;
#117098 = CARTESIAN_POINT ( 'NONE',  ( 5.525830126021535449, 8.604496359403894346, -1.199719254218452047 ) ) ;
#117100 = CARTESIAN_POINT ( 'NONE',  ( 0.1107398820658512667, -1.707777377628461046, 0.3340355821882161069 ) ) ;
#117101 = CARTESIAN_POINT ( 'NONE',  ( 0.4340280775911202760, 3.986815581052859603, 0.4851569899464819868 ) ) ;
#117102 = COLOUR_RGB ( '', 0.72549020, 0.75294118, 0.79215686) ;
#117103 = CARTESIAN_POINT ( 'NONE',  ( 6.527279143455773536, -1.428284688129980440, -1.662137905815167294 ) ) ;
#117104 = CARTESIAN_POINT ( 'NONE',  ( -5.029148636026397945, 4.832037928311032182, 0.7998128361456281477 ) ) ;
#117105 = CARTESIAN_POINT ( 'NONE',  ( -1.360316468750000674, -0.3489583329919356824, -0.7853790794158941324 ) ) ;
#117106 = CARTESIAN_POINT ( 'NONE',  ( 9.499771308870721853, -7.644320505141724453, 0.06917019444585296994 ) ) ;
#117107 = CARTESIAN_POINT ( 'NONE',  ( 6.795378861676105053, -1.851214886592133846, 0.9271815693319698237 ) ) ;
#117108 = CARTESIAN_POINT ( 'NONE',  ( 0.6730650033222317363, 1.776164188848127878, -0.9548607967814757291 ) ) ;
#117109 = CARTESIAN_POINT ( 'NONE',  ( 1.499999999999987121, 0.03541666734948738238, 0.8660254037844524744 ) ) ;
#117110 = CARTESIAN_POINT ( 'NONE',  ( 5.092375307706883625, -1.912163826771107855, -0.2340926620403842862 ) ) ;
#117111 = CARTESIAN_POINT ( 'NONE',  ( -1.364683531250000748, 11.10937500034139802, 0.000000000000000000 ) ) ;
#117112 = CARTESIAN_POINT ( 'NONE',  ( 1.793536179914383188, -0.1149406603053771958, -2.218580859979270681 ) ) ;
#117113 = EDGE_LOOP ( 'NONE', ( #83070, #67391, #115980, #3272, #23697, #117599 ) ) ;
#117114 = CARTESIAN_POINT ( 'NONE',  ( 0.000000000000000000, -0.02379966007286238305, 0.000000000000000000 ) ) ;
#117115 = DIRECTION ( 'NONE',  ( -0.6762880771785059197, 1.295290445962756284E-12, -0.7366372490352354196 ) ) ;
#117116 = CARTESIAN_POINT ( 'NONE',  ( 7.716561984472250835, 12.15440608185967086, 1.040834085586084257E-14 ) ) ;
#117117 = CARTESIAN_POINT ( 'NONE',  ( -5.204170427930421283E-15, 3.447199233515649386, -11.99999999999998224 ) ) ;
#117118 = ADVANCED_FACE ( 'NONE', ( #91438 ), #127208, .T. ) ;
#117119 = FACE_OUTER_BOUND ( 'NONE', #67896, .T. ) ;
#117120 = CARTESIAN_POINT ( 'NONE',  ( 4.247407853763897734, 1.739958666061100390, -0.04810691789801542495 ) ) ;
#117121 = CARTESIAN_POINT ( 'NONE',  ( 2.260140581184489239, -1.961506502764579052, 0.04509734162668613960 ) ) ;
#117123 = CARTESIAN_POINT ( 'NONE',  ( -8.039621903223732602, 8.481906429956900695, 1.040834085586084257E-14 ) ) ;
#117122 = CARTESIAN_POINT ( 'NONE',  ( 5.034155109375821446, 4.767602470560229122, -0.7998128361456221525 ) ) ;
#117124 = EDGE_CURVE ( 'NONE', #179842, #13744, #74161, .T. ) ;
#117125 = CARTESIAN_POINT ( 'NONE',  ( -5.863297782511878609, 6.029266553239049919, -0.3729355709888391157 ) ) ;
#117126 = CARTESIAN_POINT ( 'NONE',  ( -5.823017895876262173, 7.308274721394978357, -1.333157625313810879 ) ) ;
#117127 = CARTESIAN_POINT ( 'NONE',  ( 0.5728089798012192535, 1.423622861147020302, -1.492835154123072883 ) ) ;
#117128 = CARTESIAN_POINT ( 'NONE',  ( -8.857554428429624593, 9.228235009456373206, 0.7998128361456462443 ) ) ;
#117129 = CARTESIAN_POINT ( 'NONE',  ( -2.941756144040963417, 6.375873234782333476, -0.7216878364870257245 ) ) ;
#117130 = CARTESIAN_POINT ( 'NONE',  ( 0.9895999521203084903, 1.994116446801162290, -1.068836969126084835 ) ) ;
#117131 = ORIENTED_EDGE ( 'NONE', *, *, #119697, .F. ) ;
#117132 = CARTESIAN_POINT ( 'NONE',  ( 1.499999999999989120, -0.1937499993171845625, 0.000000000000000000 ) ) ;
#117133 = CARTESIAN_POINT ( 'NONE',  ( 2.090876104454452378, 1.629797177321444579, -0.9178172146045021629 ) ) ;
#117134 = CARTESIAN_POINT ( 'NONE',  ( 0.9317525018172129192, -1.365947654462830618, -1.068275208499162909 ) ) ;
#117135 = CARTESIAN_POINT ( 'NONE',  ( 5.829655996829377962, 1.081331853127937448, -1.906115348727636549 ) ) ;
#117136 = CARTESIAN_POINT ( 'NONE',  ( 5.280430876874616430, -1.287285901688420608, 1.914989055045878352 ) ) ;
#117137 = CARTESIAN_POINT ( 'NONE',  ( 0.9892191112199534286, 1.817966452439750968, -0.9706697534878678812 ) ) ;
#117138 = CARTESIAN_POINT ( 'NONE',  ( 3.978411374042570170, -0.1916562231945718731, -1.932471992628071789 ) ) ;
#117139 = CARTESIAN_POINT ( 'NONE',  ( -4.487385655998893164, 6.258369236797239665, 1.443375672974064550 ) ) ;
#117140 = EDGE_CURVE ( 'NONE', #51039, #95128, #140194, .T. ) ;
#117141 = CARTESIAN_POINT ( 'NONE',  ( 6.098880659294531270, 1.529360415809786433, -1.076766019972655197 ) ) ;
#117142 = CARTESIAN_POINT ( 'NONE',  ( 0.6562500000000004441, -1.895863743164078130, 0.7852924748300215141 ) ) ;
#117143 = CARTESIAN_POINT ( 'NONE',  ( 1.129749100085160940, 13.30859003568858689, 0.8992454283418387373 ) ) ;
#117144 = CARTESIAN_POINT ( 'NONE',  ( 3.255366281057017197, 6.812028071292901998, -0.7216878364870338292 ) ) ;
#117145 = CARTESIAN_POINT ( 'NONE',  ( 1.360316468750000896, 0.7656250003413994643, 0.000000000000000000 ) ) ;
#117146 = CARTESIAN_POINT ( 'NONE',  ( 4.852185490356213826, 0.1948433276699329531, -2.006959737079899497 ) ) ;
#117147 = CARTESIAN_POINT ( 'NONE',  ( -4.406036734316900905, 5.203092947200234519, -1.082531754730543971 ) ) ;
#117148 =( BOUNDED_SURFACE ( )  B_SPLINE_SURFACE ( 3, 2, ( 
 ( #38951, #102885, #168943 ),
 ( #155904, #23749, #20545 ),
 ( #21589, #89853, #35738 ),
 ( #101813, #85556, #151646 ) ),
 .UNSPECIFIED., .F., .F., .T. ) 
 B_SPLINE_SURFACE_WITH_KNOTS ( ( 4, 4 ),
 ( 3, 3 ),
 ( 0.06089817005132014405, 0.06334004685008763624 ),
 ( 0.000000000000000000, 1.000000000000000000 ),
 .UNSPECIFIED. ) 
 GEOMETRIC_REPRESENTATION_ITEM ( )  RATIONAL_B_SPLINE_SURFACE ( (
 ( 1.000000000000000000, 0.7169883299104515828, 1.000000000000000000),
 ( 1.000000000000000000, 0.7174882367719609411, 1.000000000000000000),
 ( 1.000000000000000000, 0.7180609655865438645, 1.000000000000000000),
 ( 1.000000000000000000, 0.7187540731123145399, 1.000000000000000000) ) ) 
 REPRESENTATION_ITEM ( '' )  SURFACE ( )  );
#117149 = CARTESIAN_POINT ( 'NONE',  ( 7.397945374551106568, 11.78268670361832093, -0.7998128361456291469 ) ) ;
#117150 = CARTESIAN_POINT ( 'NONE',  ( 4.577813143269636065, 5.369812084349879555, -1.199719254218450271 ) ) ;
#117152 = CARTESIAN_POINT ( 'NONE',  ( -4.163329363839114450, 7.870638172372564689, 0.03594691204382176319 ) ) ;
#117151 = CARTESIAN_POINT ( 'NONE',  ( 2.683998146737070378, -0.9385614705539682134, 1.565816405032012470 ) ) ;
#117153 = CARTESIAN_POINT ( 'NONE',  ( -6.283277845290492714, 6.295188672452495915, -0.7998128361456362523 ) ) ;
#117154 = CARTESIAN_POINT ( 'NONE',  ( -1.499999999999997780, 5.150000000000022560, 1.214306433183764966E-14 ) ) ;
#117155 = CARTESIAN_POINT ( 'NONE',  ( 1.387778780781441485E-16, 2.099999999999997868, -2.500000000000000000 ) ) ;
#117156 = ORIENTED_EDGE ( 'NONE', *, *, #63645, .F. ) ;
#117157 = CARTESIAN_POINT ( 'NONE',  ( -5.383996397958228819, 8.335060660042973524, 1.082531754730550855 ) ) ;
#117158 = CARTESIAN_POINT ( 'NONE',  ( -3.521367211247373508, 5.131347717920458962, -1.599625672291256295 ) ) ;
#117159 = CARTESIAN_POINT ( 'NONE',  ( -9.833741488613570780, 10.36711991300432345, 0.7998128361456462443 ) ) ;
#117160 = CARTESIAN_POINT ( 'NONE',  ( -0.1403647893034008221, -1.563942476893056543, -1.277904792927646582 ) ) ;
#117162 = VERTEX_POINT ( 'NONE', #41621 ) ;
#117161 = CARTESIAN_POINT ( 'NONE',  ( 0.2410938523699951708, 2.030451451530786766, 0.6113826261911479154 ) ) ;
#117163 = CARTESIAN_POINT ( 'NONE',  ( -5.912237504011027767, 9.055304967058290799, 1.199719254218454489 ) ) ;
#117164 = CARTESIAN_POINT ( 'NONE',  ( 6.179819089730593795, 6.104210447640811665, 1.040834085586084257E-14 ) ) ;
#117165 = CARTESIAN_POINT ( 'NONE',  ( 5.594623806460828241, -0.4985412361782278201, -1.999555476978178703 ) ) ;
#117166 = CARTESIAN_POINT ( 'NONE',  ( 4.764296165657141202, 1.880435471729305030, -0.7283773170061805802 ) ) ;
#117167 = ORIENTED_EDGE ( 'NONE', *, *, #41532, .F. ) ;
#117168 = ORIENTED_EDGE ( 'NONE', *, *, #99878, .T. ) ;
#117169 = CARTESIAN_POINT ( 'NONE',  ( 4.732378691258949388, 4.890468360863969188, -0.8126286185507647364 ) ) ;
#117170 = CARTESIAN_POINT ( 'NONE',  ( 3.475000000000000533, -1.181249999044085897, 0.000000000000000000 ) ) ;
#117171 = AXIS2_PLACEMENT_3D ( 'NONE', #79965, #47501, #113610 ) ;
#117173 = ORIENTED_EDGE ( 'NONE', *, *, #80137, .F. ) ;
#117172 = CARTESIAN_POINT ( 'NONE',  ( -6.629010762438975135, 6.698543742459062145, -0.7998128361456362523 ) ) ;
#117174 = CARTESIAN_POINT ( 'NONE',  ( 4.641000714467984345, 8.433135692799648808, 0.4354600853693716411 ) ) ;
#117175 = CARTESIAN_POINT ( 'NONE',  ( 4.973982425466109802, 1.752763018817087293, 0.9961474888594208377 ) ) ;
#117176 = CARTESIAN_POINT ( 'NONE',  ( 4.804558796598876746, 1.603369264058150279, 0.9048477820690554729 ) ) ;
#117177 = EDGE_CURVE ( 'NONE', #116778, #86803, #142218, .T. ) ;
#117178 = CARTESIAN_POINT ( 'NONE',  ( -0.02338929933909209696, 6.948787603726593431, -2.306014233525994772 ) ) ;
#117179 = CARTESIAN_POINT ( 'NONE',  ( 2.842713172187049331, 2.290369893530233902, 0.2817356681584815004 ) ) ;
#117180 = CARTESIAN_POINT ( 'NONE',  ( 5.508355548902068577, 9.648441583686274470, 0.7998128361456331437 ) ) ;
#117181 = CARTESIAN_POINT ( 'NONE',  ( 4.868538603872567982, -1.416007186031362330, 1.633285015310452115 ) ) ;
#117182 = CARTESIAN_POINT ( 'NONE',  ( 8.308449207076147758, 8.587612251210650527, -0.7998128361456281477 ) ) ;
#117183 = CARTESIAN_POINT ( 'NONE',  ( 0.2572359396431650458, 1.920763697077633614, -0.2861409625158922165 ) ) ;
#117184 = CARTESIAN_POINT ( 'NONE',  ( -5.057354993097396445, 5.859001232490445688, -1.199719254218446718 ) ) ;
#117185 = CARTESIAN_POINT ( 'NONE',  ( -9.437944175038655459, 15.48612576208931735, -7.411204044582823336 ) ) ;
#117186 = CARTESIAN_POINT ( 'NONE',  ( -5.004894982100124068, 5.868074229652107121, 1.199719254218452935 ) ) ;
#117187 = CARTESIAN_POINT ( 'NONE',  ( 3.309304339999539657, -0.3661640501408692794, 1.834289908569000538 ) ) ;
#117188 = AXIS2_PLACEMENT_3D ( 'NONE', #102539, #118851, #39678 ) ;
#117192 = ADVANCED_FACE ( 'NONE', ( #194244 ), #167539, .T. ) ;
#117191 = CARTESIAN_POINT ( 'NONE',  ( -6.771371375382467583, 6.864631124226471037, -0.7998128361456362523 ) ) ;
#117190 = CARTESIAN_POINT ( 'NONE',  ( -1.364683531250010295, 5.488541667008087543, -0.7879004041258300672 ) ) ;
#117189 = CARTESIAN_POINT ( 'NONE',  ( 1.371198541116287917, -1.641758494746584418, -0.9804709962101465504 ) ) ;
#117193 = CARTESIAN_POINT ( 'NONE',  ( 3.106307083854151774, -2.204334110825040494, 0.1085914373066959593 ) ) ;
#117194 = LINE ( 'NONE', #135528, #84972 ) ;
#117195 = CARTESIAN_POINT ( 'NONE',  ( 5.030238685870051185, 5.827365540725222282, -1.199719254218452047 ) ) ;
#117196 = CARTESIAN_POINT ( 'NONE',  ( 6.143253000323500856, 10.18122924377050609, -0.7216878364870458196 ) ) ;
#117197 = CARTESIAN_POINT ( 'NONE',  ( -5.108724954250998707, 4.854600622914589714, -0.7998128361456221525 ) ) ;
#117198 = CARTESIAN_POINT ( 'NONE',  ( -6.061904078641520144, 10.08632216847484031, 0.7216878364870267237 ) ) ;
#117199 = CARTESIAN_POINT ( 'NONE',  ( 0.8429695343807745989, -1.692941477971823483, 1.009804834249914851 ) ) ;
#117200 = EDGE_CURVE ( 'NONE', #198620, #41470, #153813, .T. ) ;
#117201 = CARTESIAN_POINT ( 'NONE',  ( 6.481126831302748137, -0.1059855822947413234, -2.305399816445557359 ) ) ;
#117202 = CARTESIAN_POINT ( 'NONE',  ( 1.328483007144948935, -1.247240240105648601, 1.514344512384787622 ) ) ;
#117203 = CARTESIAN_POINT ( 'NONE',  ( 4.293840196874755044, -1.418639180022958080, -1.497458912744116022 ) ) ;
#117204 = CARTESIAN_POINT ( 'NONE',  ( 6.209271165378815738, 7.306866450105836464, -1.082531754730543083 ) ) ;
#117205 = CARTESIAN_POINT ( 'NONE',  ( 6.866278450678116485, 6.975356045404744521, 0.000000000000000000 ) ) ;
#117206 = ORIENTED_EDGE ( 'NONE', *, *, #202925, .F. ) ;
#117207 = CARTESIAN_POINT ( 'NONE',  ( 8.731087737076324018, 9.288616569451617622, 1.040834085586084257E-14 ) ) ;
#117208 = CARTESIAN_POINT ( 'NONE',  ( -1.201851678989727383E-14, 4.259375000341417028, -1.575800808251660134 ) ) ;
#117209 = LINE ( 'NONE', #66225, #152712 ) ;
#117210 = CARTESIAN_POINT ( 'NONE',  ( 4.324687812634892659, 5.108185871904570519, 1.082531754730560403 ) ) ;
#117211 = CARTESIAN_POINT ( 'NONE',  ( 6.865710891575433905, -0.4862813381408522817, 2.124062634707358566 ) ) ;
#117212 = CARTESIAN_POINT ( 'NONE',  ( 6.480030769895370746, -1.807141314969593848, -0.3518929191878711338 ) ) ;
#117213 = CARTESIAN_POINT ( 'NONE',  ( -2.088542702721619460, 3.956598013261175772, 11.35310118413588931 ) ) ;
#117214 = CARTESIAN_POINT ( 'NONE',  ( 1.469576158976824144E-15, 19.00000000000000000, 12.00000000000000178 ) ) ;
#117215 = CARTESIAN_POINT ( 'NONE',  ( 1.897508810457830153, -0.6348907881138059484, 1.759622905829677508 ) ) ;
#117216 = CARTESIAN_POINT ( 'NONE',  ( -6.048854636777848626, 6.051613005247792998, 0.5441514604978964220 ) ) ;
#117217 =( NAMED_UNIT ( * ) SI_UNIT ( $, .STERADIAN. ) SOLID_ANGLE_UNIT ( ) );
#117218 = CARTESIAN_POINT ( 'NONE',  ( 5.595231165798738360, 7.497995327707586810, -1.335214257040851615 ) ) ;
#117219 = CARTESIAN_POINT ( 'NONE',  ( -0.6823417656250212460, 5.363541667008087543, 1.181850606188767472 ) ) ;
#117220 = AXIS2_PLACEMENT_3D ( 'NONE', #139521, #140609, #109208 ) ;
#117221 = CARTESIAN_POINT ( 'NONE',  ( 1.453610327690219473, -1.385809040371610346, -1.317956379189986871 ) ) ;
#117222 = CARTESIAN_POINT ( 'NONE',  ( 2.746659024021454787, -1.472625519509669134, 0.9813492100937453166 ) ) ;
#117223 = CARTESIAN_POINT ( 'NONE',  ( 0.8910925258837493201, -0.04752833427993513604, -1.911862225341356858 ) ) ;
#117225 = CARTESIAN_POINT ( 'NONE',  ( 3.954619794068328087, -1.788705220947036878, -0.6861305607534126105 ) ) ;
#117224 = CARTESIAN_POINT ( 'NONE',  ( 2.890748560597784955, -3.175295894664973417, -1.688109688813533626 ) ) ;
#117226 = CARTESIAN_POINT ( 'NONE',  ( 5.969198390587827419, 1.736284540159404033, 0.9297856951416498816 ) ) ;
#117227 = CARTESIAN_POINT ( 'NONE',  ( 1.072698285844303934, 0.8645715524648779349, 1.936551149067309741 ) ) ;
#117228 = CARTESIAN_POINT ( 'NONE',  ( 0.1305260785387470923, -7.912329794880671230, -10.96023284214814986 ) ) ;
#117229 = CARTESIAN_POINT ( 'NONE',  ( 4.170664822833985319, -1.745344833062393075, -0.6735866001992969476 ) ) ;
#117231 = ORIENTED_EDGE ( 'NONE', *, *, #202906, .T. ) ;
#117230 = CARTESIAN_POINT ( 'NONE',  ( 0.4338677482375961070, 0.9413943332680120291, -1.564114433284753636 ) ) ;
#117233 = CARTESIAN_POINT ( 'NONE',  ( -1.817809523595264043, -0.8386016503486174445, 1.021477770318699241 ) ) ;
#117232 = CARTESIAN_POINT ( 'NONE',  ( 3.440233207309027375, 0.9924059104887033023, -1.971224004288201881 ) ) ;
#117234 = CARTESIAN_POINT ( 'NONE',  ( 0.6823417656249899377, 4.738541667008086655, -1.181850606188754593 ) ) ;
#117235 = CARTESIAN_POINT ( 'NONE',  ( 0.6431264911748921786, -0.2508561283167276557, -2.047287668789533832 ) ) ;
#117236 = CARTESIAN_POINT ( 'NONE',  ( 5.940443861082012944, 10.08226827123770697, 0.7998128361456462443 ) ) ;
#117237 = CARTESIAN_POINT ( 'NONE',  ( -9.179033691651859783, 10.66762638080401260, 1.199719254218462483 ) ) ;
#117238 = CARTESIAN_POINT ( 'NONE',  ( -8.919266336782142091, 2.972657967447086769, -7.510420563958255968 ) ) ;
#117239 = CARTESIAN_POINT ( 'NONE',  ( -3.425394108783801794, -0.02028796577872097814, -0.4182871798345951797 ) ) ;
#117240 = CARTESIAN_POINT ( 'NONE',  ( 5.982890925380405456, 10.20206618957764100, 0.000000000000000000 ) ) ;
#117241 = ORIENTED_EDGE ( 'NONE', *, *, #40298, .F. ) ;
#117242 = CARTESIAN_POINT ( 'NONE',  ( 4.299325596424930396, -1.802881993240162961, 1.017688063649782482 ) ) ;
#117243 = CARTESIAN_POINT ( 'NONE',  ( 1.499999999999987121, 4.045833333333359150, -0.8660254037844323793 ) ) ;
#117244 = CARTESIAN_POINT ( 'NONE',  ( 1.739762150092131643, -1.564342989677082629, -1.491970722459233123 ) ) ;
#117245 = CARTESIAN_POINT ( 'NONE',  ( -6.300768610526733760, 6.888587422923714954, -0.7334343799849201151 ) ) ;
#117246 = CARTESIAN_POINT ( 'NONE',  ( 1.524088222275731486, -2.004166515738073695, 0.2493262195080257204 ) ) ;
#117247 = DIRECTION ( 'NONE',  ( 0.000000000000000000, -1.000000000000000000, 0.000000000000000000 ) ) ;
#117248 = B_SPLINE_CURVE_WITH_KNOTS ( 'NONE', 3,
 ( #42541, #71780, #174672, #38244, #158401, #170368 ),
 .UNSPECIFIED., .F., .F.,
 ( 4, 2, 4 ),
 ( 0.000000000000000000, 0.0003845013059668467856, 0.0007690026119336935712 ),
 .UNSPECIFIED. ) ;
#117249 = EDGE_LOOP ( 'NONE', ( #173220, #204371, #24504, #151828 ) ) ;
#117251 = CARTESIAN_POINT ( 'NONE',  ( 9.259855728453651125, 9.905512559391842942, 1.040834085586084257E-14 ) ) ;
#117250 = CARTESIAN_POINT ( 'NONE',  ( -3.474999999999998312, -3.820833333333332416, 2.006292185433951047 ) ) ;
#117252 = CARTESIAN_POINT ( 'NONE',  ( 1.777638883463123598, -0.9165151389911446733, 1.199999999999999734 ) ) ;
#117253 = CARTESIAN_POINT ( 'NONE',  ( -0.1355283706049141557, -1.957205112593700003, -0.4852584411360050254 ) ) ;
#117254 = CARTESIAN_POINT ( 'NONE',  ( 4.388337494309430653, -0.4807229498768311182, -2.138019847805587403 ) ) ;
#117255 = EDGE_CURVE ( 'NONE', #2289, #166897, #192540, .T. ) ;
#117256 = CARTESIAN_POINT ( 'NONE',  ( 1.499999999999989120, 3.785416667349481123, 0.8660254037844524744 ) ) ;
#117257 = CARTESIAN_POINT ( 'NONE',  ( 3.357576282340120066, -1.451192137084562628, -1.245647637661301044 ) ) ;
#117258 = CARTESIAN_POINT ( 'NONE',  ( -4.229253852459088137, 7.021547696922494808, 1.199719254218464037 ) ) ;
#117259 = CARTESIAN_POINT ( 'NONE',  ( 3.334942598837264960, 6.834590765378040444, 1.214306433183764966E-14 ) ) ;
#117261 = CARTESIAN_POINT ( 'NONE',  ( 1.071888921174158016, -0.9040910708146729924, 1.802427947461216373 ) ) ;
#117260 = CARTESIAN_POINT ( 'NONE',  ( -1.387358672535449200, 7.315968950355252076, 4.254625267135948796 ) ) ;
#117262 = CARTESIAN_POINT ( 'NONE',  ( 1.364683531250000303, 12.56770833367473372, -0.7879004041258355073 ) ) ;
#117263 = AXIS2_PLACEMENT_3D ( 'NONE', #70723, #199670, #200728 ) ;
#117265 = CARTESIAN_POINT ( 'NONE',  ( -4.468294144155606773, 7.370704380560280100, 1.199719254218452935 ) ) ;
#117264 = CARTESIAN_POINT ( 'NONE',  ( 0.8906306365582180584, -0.5635816346751547634, -2.221901885516941899 ) ) ;
#117266 = CARTESIAN_POINT ( 'NONE',  ( 3.996854971928843092, 1.456802638785438475, -0.9229968019349673591 ) ) ;
#117267 = CARTESIAN_POINT ( 'NONE',  ( -0.1399997263889819765, 0.7174702203470960660, -2.082715917450683740 ) ) ;
#117268 = CARTESIAN_POINT ( 'NONE',  ( 3.684065054611349144, 5.321161868511784299, -1.599625672291262513 ) ) ;
#117269 = DIRECTION ( 'NONE',  ( 0.000000000000000000, -1.000000000000000000, 0.000000000000000000 ) ) ;
#117270 = CARTESIAN_POINT ( 'NONE',  ( 1.715213470010600538, -1.680963409367957295, -1.011360081469035999 ) ) ;
#117271 = CARTESIAN_POINT ( 'NONE',  ( 11.41381675112453031, 10.19999999999999929, -3.704697986577182078 ) ) ;
#117272 = CARTESIAN_POINT ( 'NONE',  ( 6.003563092752934871, 5.898578451166879510, 0.7998128361456341429 ) ) ;
#117273 = CARTESIAN_POINT ( 'NONE',  ( 0.1751657365761547791, 2.016170943927285908, -2.458682602970231112 ) ) ;
#117274 = EDGE_LOOP ( 'NONE', ( #155133, #76149, #60230, #79907 ) ) ;
#117275 = CARTESIAN_POINT ( 'NONE',  ( 2.535011536075336913, 5.133042487381361596, 2.420000000000000373 ) ) ;
#117276 = ORIENTED_EDGE ( 'NONE', *, *, #2431, .T. ) ;
#117277 = CARTESIAN_POINT ( 'NONE',  ( 4.125510307337266980, -0.3055505145112321075, 1.785335377935037826 ) ) ;
#117278 = ORIENTED_EDGE ( 'NONE', *, *, #80620, .F. ) ;
#117279 = CARTESIAN_POINT ( 'NONE',  ( 5.855142236255289845, 7.924361590421551860, -1.599625672291281386 ) ) ;
#117280 = CARTESIAN_POINT ( 'NONE',  ( 2.925527285498711549, 6.635141943048991742, 0.7998128361456281477 ) ) ;
#117281 = CARTESIAN_POINT ( 'NONE',  ( 4.969312858920484466, -1.533218896822113653, -0.9643851972171797460 ) ) ;
#117282 = CARTESIAN_POINT ( 'NONE',  ( 5.356880090730857802, 8.303424968277756335, 1.082531754730548412 ) ) ;
#117283 = AXIS2_PLACEMENT_3D ( 'NONE', #209075, #176609, #11958 ) ;
#117284 = FILL_AREA_STYLE_COLOUR ( '', #194040 ) ;
#117285 = CARTESIAN_POINT ( 'NONE',  ( 5.160031065370225711, 6.461479299918838848, -1.191482946479218485 ) ) ;
#117286 = ORIENTED_EDGE ( 'NONE', *, *, #178754, .T. ) ;
#117288 = CARTESIAN_POINT ( 'NONE',  ( 10.05353459973327368, 11.68787744023238417, -1.199719254218440723 ) ) ;
#117287 = CARTESIAN_POINT ( 'NONE',  ( 5.969184020103408095, 1.641702931788184383, 0.8765767931452476125 ) ) ;
#117289 = CARTESIAN_POINT ( 'NONE',  ( 4.271028807069753519, 1.709443138559762376, -0.8646770750302870123 ) ) ;
#117290 = CARTESIAN_POINT ( 'NONE',  ( -6.731761806397366321, -7.792646766724930174, -6.779954559072856490 ) ) ;
#117291 = CARTESIAN_POINT ( 'NONE',  ( -12.04274103669372309, 7.374159847806027734, 3.963224530603232765 ) ) ;
#117292 = CARTESIAN_POINT ( 'NONE',  ( 11.48243876534946217, 13.87999999999998302, 3.199999999999997957 ) ) ;
#117293 = CARTESIAN_POINT ( 'NONE',  ( -15.75000000000000000, 12.30000000000000071, -0.7000000000000009548 ) ) ;
#117294 = CARTESIAN_POINT ( 'NONE',  ( 6.670248388243460447, 6.884303995813253252, -0.7216878364870257245 ) ) ;
#117295 = CARTESIAN_POINT ( 'NONE',  ( -9.869972641068651242, 11.57768483841065787, 1.082531754730558626 ) ) ;
#117296 = CARTESIAN_POINT ( 'NONE',  ( 0.9015118058452382677, 1.767791302423503685, 1.243857928393626633 ) ) ;
#117297 = CARTESIAN_POINT ( 'NONE',  ( -4.960304097753355457, 6.880383762169266504, 1.599625672291263179 ) ) ;
#117298 = CARTESIAN_POINT ( 'NONE',  ( 5.448397627845284141, 7.449826213943242514, 1.599625672291268286 ) ) ;
#117299 = CARTESIAN_POINT ( 'NONE',  ( 0.3756504392133250825, 1.046533627790873000, 1.495644344755318045 ) ) ;
#117300 = CARTESIAN_POINT ( 'NONE',  ( -4.928552533767591726, 5.708731696605642725, 1.199719254218462483 ) ) ;
#117301 = CARTESIAN_POINT ( 'NONE',  ( 3.100428009929767637, -0.5284298666012043899, -1.747434388548900541 ) ) ;
#117302 = CARTESIAN_POINT ( 'NONE',  ( -5.381422217466665714, 4.322449550048943046, 2.440471613107408011 ) ) ;
#117303 = CARTESIAN_POINT ( 'NONE',  ( 1.951281838316549777, -1.706683157587106425, 0.8630329916254894096 ) ) ;
#117304 = ORIENTED_EDGE ( 'NONE', *, *, #47755, .T. ) ;
#117305 = CARTESIAN_POINT ( 'NONE',  ( 2.172252323668334206, -0.9256296301539097549, -1.738465135635240522 ) ) ;
#117306 = CARTESIAN_POINT ( 'NONE',  ( 4.757337479089009058, 1.920383491809660503, -0.2886861380682907430 ) ) ;
#117307 = CARTESIAN_POINT ( 'NONE',  ( -7.587723245503481095, 8.881373870289390737, 1.199719254218452047 ) ) ;
#117309 = CARTESIAN_POINT ( 'NONE',  ( 3.656581996618038843, 2.110704406498860486, 0.2042969539849878724 ) ) ;
#117308 = CARTESIAN_POINT ( 'NONE',  ( 4.435452530326143616, 5.203724702582467998, -1.199719254218452047 ) ) ;
#117310 = CARTESIAN_POINT ( 'NONE',  ( -3.855102659574312973, 8.506872032339167333, -2.500000000000000888 ) ) ;
#117311 = CARTESIAN_POINT ( 'NONE',  ( 8.910733272679570049, 11.41894145625809820, -1.599625672291255185 ) ) ;
#117312 = CARTESIAN_POINT ( 'NONE',  ( 5.993251976321238850, 6.092249680885792884, 0.6249505139499841322 ) ) ;
#117313 = DIRECTION ( 'NONE',  ( 0.000000000000000000, -9.023263958591318651E-17, 1.000000000000000000 ) ) ;
#117314 = ORIENTED_EDGE ( 'NONE', *, *, #86107, .F. ) ;
#117315 = CARTESIAN_POINT ( 'NONE',  ( 1.364683531249996529, 13.21354166700806410, 0.7879004041258403923 ) ) ;
#117316 = CARTESIAN_POINT ( 'NONE',  ( 3.705121118284530279, 7.544668081299086282, -1.734723475976807094E-15 ) ) ;
#117317 = CARTESIAN_POINT ( 'NONE',  ( 4.955668840994886359, 5.740367388370866131, 1.199719254218462483 ) ) ;
#117318 = CARTESIAN_POINT ( 'NONE',  ( 5.550083779947807550, 7.568460058062819407, -1.599625672291283607 ) ) ;
#117319 = CARTESIAN_POINT ( 'NONE',  ( -11.86239285000045918, 11.37999999999998302, 1.812080536912751061 ) ) ;
#117320 = CARTESIAN_POINT ( 'NONE',  ( 4.477060521952030747, -0.002618581577289170060, -1.825872481161804561 ) ) ;
#117321 = DIRECTION ( 'NONE',  ( 0.000000000000000000, -1.000000000000000000, 0.000000000000000000 ) ) ;
#117322 = CARTESIAN_POINT ( 'NONE',  ( -9.056483424248693126, 10.62861408545402675, 1.082531754730558626 ) ) ;
#117323 = CARTESIAN_POINT ( 'NONE',  ( -6.611092229237963025, 6.760716375176868631, -0.1380881291089108287 ) ) ;
#117324 = LINE ( 'NONE', #97835, #174538 ) ;
#117325 = CARTESIAN_POINT ( 'NONE',  ( 5.823093596695693819, -0.04436734784114480107, 1.870300906237104988 ) ) ;
#117326 = CARTESIAN_POINT ( 'NONE',  ( 7.558834334818744338, 8.777393797832065303, 1.199719254218462483 ) ) ;
#117327 = CARTESIAN_POINT ( 'NONE',  ( -3.425406365747000859, 7.148057860013469877, 1.040834085586084257E-14 ) ) ;
#117328 = B_SPLINE_CURVE_WITH_KNOTS ( 'NONE', 3,
 ( #5262, #35656, #167804, #85482, #37803, #4203, #71338, #137455, #203470, #55124, #38871, #88701, #154760, #6344, #188307, #141748, #72416, #176342, #138517, #90840, #156903, #42094, #157974, #173158, #9564, #89781, #204541, #140677, #8491, #73494 ),
 .UNSPECIFIED., .F., .F.,
 ( 4, 2, 2, 2, 2, 2, 2, 2, 2, 2, 2, 2, 2, 2, 4 ),
 ( 0.001318931363626723533, 0.001984147519712246236, 0.002649363675797769373, 0.003314579831883291642, 0.003979795987968814779, 0.004645012144054337482, 0.005310228300139859317, 0.005975444456225382020, 0.006640660612310906458, 0.007971092924481951864, 0.008636309080567474566, 0.009301525236652995535, 0.009966741392738518238, 0.01063195754882404094, 0.01196238986099508982 ),
 .UNSPECIFIED. ) ;
#117329 = CARTESIAN_POINT ( 'NONE',  ( 3.704402285031850539, 5.344888637335695414, -1.599625672291262513 ) ) ;
#117330 = CARTESIAN_POINT ( 'NONE',  ( 1.364683531249996529, 11.02604166700807120, 0.7879004041258405033 ) ) ;
#117331 = CARTESIAN_POINT ( 'NONE',  ( -3.927058049452637700, 7.733318157670055371, -0.7998128361456281477 ) ) ;
#117332 = CARTESIAN_POINT ( 'NONE',  ( 4.142179624174931796, 4.791296635414242111, 1.199719254218464037 ) ) ;
#117333 = EDGE_CURVE ( 'NONE', #66261, #59479, #171089, .T. ) ;
#117334 = CARTESIAN_POINT ( 'NONE',  ( -7.944151662964566540, 8.232874793072271657, 0.000000000000000000 ) ) ;
#117335 = VECTOR ( 'NONE', #127203, 1000.000000000000000 ) ;
#117336 = CARTESIAN_POINT ( 'NONE',  ( 0.6200890622066607127, 2.048230590617374336, -0.3001980380039070972 ) ) ;
#117337 = CARTESIAN_POINT ( 'NONE',  ( 1.616979318382205433, 0.2114564432566454211, 2.106663336370690143 ) ) ;
#117338 = CARTESIAN_POINT ( 'NONE',  ( 7.716561984472250835, 12.15440608185967086, 1.040834085586084257E-14 ) ) ;
#117339 = CARTESIAN_POINT ( 'NONE',  ( -1.792484642137049056, 2.460830816602578075, 2.500000000000000000 ) ) ;
#117340 = CARTESIAN_POINT ( 'NONE',  ( 5.770397209236588942, -0.9257025293247715947, -1.851810055641222252 ) ) ;
#117342 = CARTESIAN_POINT ( 'NONE',  ( 4.061730550730160871, 7.744580798899280971, -0.5443347154160914636 ) ) ;
#117341 = CARTESIAN_POINT ( 'NONE',  ( 2.032514702046281485, -1.644074058028240692, 0.8291662819630771786 ) ) ;
#117343 = CARTESIAN_POINT ( 'NONE',  ( 6.209271165378815738, 7.306866450105836464, -1.082531754730543083 ) ) ;
#117345 = CARTESIAN_POINT ( 'NONE',  ( 1.499999999999993117, 9.635416667349465669, 0.8660254037844408170 ) ) ;
#117344 = CARTESIAN_POINT ( 'NONE',  ( -3.475000000000000533, -3.179166666666664476, -2.006292185433948827 ) ) ;
#117346 = CARTESIAN_POINT ( 'NONE',  ( 1.517954844142660464, -1.276539353255158105, -1.903739821206115623 ) ) ;
#117348 = CARTESIAN_POINT ( 'NONE',  ( -1.419999999999997708, 6.280000000000042881, -2.873333333333329520 ) ) ;
#117347 = CARTESIAN_POINT ( 'NONE',  ( -1.337789648166264334, 3.300000000000025135, 0.2994557852716039359 ) ) ;
#117349 = ORIENTED_EDGE ( 'NONE', *, *, #193907, .F. ) ;
#117350 = CARTESIAN_POINT ( 'NONE',  ( 7.239690839573049708, 11.39013037956983965, 1.040834085586084257E-14 ) ) ;
#117351 = CARTESIAN_POINT ( 'NONE',  ( 0.1408853756387764278, 1.927792606564913136, 0.5802787064154624197 ) ) ;
#117352 = CARTESIAN_POINT ( 'NONE',  ( 0.6374591745182572877, 1.832550977151351290, -0.7006947966294306829 ) ) ;
#117353 = CARTESIAN_POINT ( 'NONE',  ( 6.491432910188612126, -0.4373703761123280964, 1.975813455233149218 ) ) ;
#117355 = CARTESIAN_POINT ( 'NONE',  ( -9.510997388311002609, 3.006837337344905325, -6.782141846552069531 ) ) ;
#117354 = CARTESIAN_POINT ( 'NONE',  ( -8.850775351622791831, 9.220326086515070685, -0.7998128361456291469 ) ) ;
#117356 = CARTESIAN_POINT ( 'NONE',  ( -6.645558177068566330, 6.717849059526919575, 0.1763403335921341630 ) ) ;
#117358 = CARTESIAN_POINT ( 'NONE',  ( 2.078617942332625201, -0.08328603760934982780, -1.768007077409910588 ) ) ;
#117357 = CARTESIAN_POINT ( 'NONE',  ( 4.101575158799015242, -2.085053422979638693, 0.1536182331017873492 ) ) ;
#117359 = CARTESIAN_POINT ( 'NONE',  ( 3.895595285070167169, 2.800000000000017586, 0.7750000000000135669 ) ) ;
#117361 = CARTESIAN_POINT ( 'NONE',  ( 5.296947879282962290, 1.871547875688117424, 1.323312301801358393 ) ) ;
#117360 = CARTESIAN_POINT ( 'NONE',  ( -11.73399103866650073, 7.418623464565952119, 2.524040681687853560 ) ) ;
#117362 = CARTESIAN_POINT ( 'NONE',  ( 3.398151218454207090, 1.370964323331394397, -1.071876607410700677 ) ) ;
#117363 = EDGE_CURVE ( 'NONE', #132416, #94694, #178067, .T. ) ;
#117364 = CARTESIAN_POINT ( 'NONE',  ( 2.191614386903386613, 5.708633884695917260, -0.7998128361456281477 ) ) ;
#117365 = AXIS2_PLACEMENT_3D ( 'NONE', #58802, #41507, #171482 ) ;
#117366 = CARTESIAN_POINT ( 'NONE',  ( 1.284279953904119864, 3.296639714193937198, -0.7749999999999910294 ) ) ;
#117367 = CARTESIAN_POINT ( 'NONE',  ( 2.811537702714523856, -1.443443483380968173, 0.9601682615991720127 ) ) ;
#117368 = CARTESIAN_POINT ( 'NONE',  ( 3.068971866484587530, 1.574395709666128296, -1.495330859492151943 ) ) ;
#117369 = CARTESIAN_POINT ( 'NONE',  ( 4.202137545231717120, 6.989912005157271402, 1.199719254218462483 ) ) ;
#117370 = CARTESIAN_POINT ( 'NONE',  ( 5.067592334412735156, 1.357865985192594271, 1.490972259599515848 ) ) ;
#117371 = CARTESIAN_POINT ( 'NONE',  ( 1.062500000000000888, -1.451031289061164742, -1.451031289061077922 ) ) ;
#117372 = CARTESIAN_POINT ( 'NONE',  ( -0.7500000000000215383, 4.222916667349481123, 1.299038105676671107 ) ) ;
#117373 = CARTESIAN_POINT ( 'NONE',  ( 1.870020283345479539, 0.9883514471830873171, 1.653387599232780447 ) ) ;
#117374 = CARTESIAN_POINT ( 'NONE',  ( 0.7500000000000006661, 8.864583334016129967, 1.299038105676657340 ) ) ;
#117375 = CARTESIAN_POINT ( 'NONE',  ( 5.994412725124051100, -1.189069957525538124, 1.876188141934010956 ) ) ;
#117376 = ORIENTED_EDGE ( 'NONE', *, *, #112850, .T. ) ;
#117377 = CARTESIAN_POINT ( 'NONE',  ( -0.1110810684432622653, 2.888487728959455936, -2.285870655067727242 ) ) ;
#117378 = CARTESIAN_POINT ( 'NONE',  ( -1.201851678989727383E-14, 1.212500000000025002, 1.732050807568877637 ) ) ;
#117379 = CARTESIAN_POINT ( 'NONE',  ( 6.449928391799196525, 8.548002428564306143, -1.599625672291262513 ) ) ;
#117380 = CARTESIAN_POINT ( 'NONE',  ( 3.823036128929238942, 7.404033217152015567, 1.040834085586084257E-14 ) ) ;
#117381 = DIRECTION ( 'NONE',  ( 0.000000000000000000, -1.000000000000000000, 0.000000000000000000 ) ) ;
#117382 = CARTESIAN_POINT ( 'NONE',  ( 1.524421784905782618, -2.203991335649616357, 0.2763902372489163151 ) ) ;
#117383 = CARTESIAN_POINT ( 'NONE',  ( 6.514115657861259123, 1.956686900881845714, -0.1430618042221123987 ) ) ;
#117384 = CARTESIAN_POINT ( 'NONE',  ( 9.083599731475988648, 10.66024977721925104, 1.082531754730549967 ) ) ;
#117385 = TOROIDAL_SURFACE ( 'NONE', #196796, 2.649999999999999911, 0.1000000000000000056 ) ;
#117386 = CARTESIAN_POINT ( 'NONE',  ( 0.3866926556112008639, 2.897682894409560284, 2.027578619373314073 ) ) ;
#117387 = CARTESIAN_POINT ( 'NONE',  ( 0.3159878724818787066, -2.119942686789745068, 0.4214050671751194410 ) ) ;
#117388 = CARTESIAN_POINT ( 'NONE',  ( 4.258142763143749399, 7.125527769379820242, 1.199719254218451159 ) ) ;
#117389 = CARTESIAN_POINT ( 'NONE',  ( -3.336715202739028552, 6.906935146588564223, 0.7216878364870338292 ) ) ;
#117390 = CARTESIAN_POINT ( 'NONE',  ( 4.457523014600942801, 1.654850327679569633, 1.231099151980449724 ) ) ;
#117391 = CARTESIAN_POINT ( 'NONE',  ( -3.567766978690493307, 7.314145241780881435, 1.040834085586084257E-14 ) ) ;
#117392 = CARTESIAN_POINT ( 'NONE',  ( 1.499999999999987121, 3.827083334016153415, -0.8660254037844323793 ) ) ;
#117393 = CARTESIAN_POINT ( 'NONE',  ( -1.402160292154681736E-14, -0.3031249996585801965, -1.575800808251665908 ) ) ;
#117394 = CARTESIAN_POINT ( 'NONE',  ( 6.415307259278708152, -0.2288938695442776505, 1.856442058181500654 ) ) ;
#117395 = CARTESIAN_POINT ( 'NONE',  ( 4.553154410594215662, -1.128159591824983377, 1.317121951208845454 ) ) ;
#117396 = CARTESIAN_POINT ( 'NONE',  ( 4.845099162036492046, 0.5397016130457911176, -1.654733517006673482 ) ) ;
#117397 = CARTESIAN_POINT ( 'NONE',  ( 5.169736645512481132, 4.925780929386339935, 0.7998128361456341429 ) ) ;
#117398 = CARTESIAN_POINT ( 'NONE',  ( 2.033172958078794501, -2.045629734292064850, 1.034765616053961557 ) ) ;
#117399 = CARTESIAN_POINT ( 'NONE',  ( 1.364683531249990311, 4.676041667008083103, 0.7879004041258500513 ) ) ;
#117400 = CARTESIAN_POINT ( 'NONE',  ( 5.741762370215764300, 2.088391581209507741, 0.1015199779932918489 ) ) ;
#117401 = CARTESIAN_POINT ( 'NONE',  ( 6.263619209540105537, 1.000520857970560895, 1.664240579554799648 ) ) ;
#117402 = EDGE_CURVE ( 'NONE', #140322, #28319, #117324, .T. ) ;
#117403 = CARTESIAN_POINT ( 'NONE',  ( -1.420000000000021911, 6.200000000000045475, 2.900000000000013678 ) ) ;
#117404 = PRESENTATION_STYLE_ASSIGNMENT (( #82694 ) ) ;
#117405 = CARTESIAN_POINT ( 'NONE',  ( 1.231092510272915552, 2.014232830173094513, 0.09613330637052441840 ) ) ;
#117406 = CARTESIAN_POINT ( 'NONE',  ( 0.4104466507391414387, 1.508250410577081979, -1.590083307377434974 ) ) ;
#117407 = CARTESIAN_POINT ( 'NONE',  ( 8.344868292979940705, 13.15147191686607364, -8.540160728547430580 ) ) ;
#117408 = CARTESIAN_POINT ( 'NONE',  ( -8.528242318195895066, 9.908369778438709474, 1.199719254218462483 ) ) ;
#117409 = CARTESIAN_POINT ( 'NONE',  ( 6.006425746053997372, 6.966250444273174303, -1.199719254218445830 ) ) ;
#117410 = CARTESIAN_POINT ( 'NONE',  ( 3.492942606646631809, -2.044086983709763050, -0.5638711869686771072 ) ) ;
#117411 = CARTESIAN_POINT ( 'NONE',  ( -1.402160292154681736E-14, -0.3031249996585801965, -1.575800808251665908 ) ) ;
#117412 = CARTESIAN_POINT ( 'NONE',  ( 5.356004772612798170, 1.823420152956479523, -0.09349780940721279243 ) ) ;
#117413 = ORIENTED_EDGE ( 'NONE', *, *, #53950, .T. ) ;
#117414 = CARTESIAN_POINT ( 'NONE',  ( -5.875479466675803231, 7.948088359245467416, -1.599625672291271394 ) ) ;
#117415 = CARTESIAN_POINT ( 'NONE',  ( -4.905110356762790502, 4.827649200395154772, -0.06592220986076716138 ) ) ;
#117416 = CARTESIAN_POINT ( 'NONE',  ( 0.000000000000000000, -0.6343749995220417937, -3.793834371823813001 ) ) ;
#117417 = CIRCLE ( 'NONE', #199922, 0.08000000000000041800 ) ;
#117418 = CARTESIAN_POINT ( 'NONE',  ( -6.905180308061733996, 6.950465202360470052, 0.7998128361456341429 ) ) ;
#117419 = CARTESIAN_POINT ( 'NONE',  ( 3.463153198524880239, -1.648742896667846125, 1.166392943622736267 ) ) ;
#117420 = CARTESIAN_POINT ( 'NONE',  ( 0.3586045525620683017, 0.8063113102214304329, 1.945692106844071789 ) ) ;
#117421 = CARTESIAN_POINT ( 'NONE',  ( -2.810282979782591006, 6.500690253046801814, 0.000000000000000000 ) ) ;
#117422 = CARTESIAN_POINT ( 'NONE',  ( 4.522197165953073750, 0.8743044213657903407, 1.642730557785059053 ) ) ;
#117423 = CARTESIAN_POINT ( 'NONE',  ( 8.215351014876830504, 11.67199438640995801, -1.199719254218446718 ) ) ;
#117424 = EDGE_CURVE ( 'NONE', #15383, #177247, #14984, .T. ) ;
#117425 = CARTESIAN_POINT ( 'NONE',  ( 3.294557018017927330, 6.403080317724275439, 0.9028181842051991035 ) ) ;
#117426 = CARTESIAN_POINT ( 'NONE',  ( -3.144601563365788444, 5.756120026313656268, -1.199719254218452935 ) ) ;
#117427 = CARTESIAN_POINT ( 'NONE',  ( -8.369460898337653276, 8.658792557682392754, 0.7998128361456462443 ) ) ;
#117429 = CARTESIAN_POINT ( 'NONE',  ( -4.549609453380520030, 7.192579769413725010, 1.336992641046318875 ) ) ;
#117428 = CARTESIAN_POINT ( 'NONE',  ( -5.752402313948099533, 9.933162809573264695, -0.7998128361456362523 ) ) ;
#117430 = CARTESIAN_POINT ( 'NONE',  ( -0.6823417656250246877, -0.9489583329919115684, 1.181850606188755259 ) ) ;
#117431 = CARTESIAN_POINT ( 'NONE',  ( 2.038076752987047602, 1.660595340560795607, -0.4986328326925906773 ) ) ;
#117432 = CARTESIAN_POINT ( 'NONE',  ( 0.9193797689642355664, 1.039780534333001771, -1.395406566618085709 ) ) ;
#117433 = VECTOR ( 'NONE', #48798, 1000.000000000000000 ) ;
#117435 = CARTESIAN_POINT ( 'NONE',  ( 8.270110514656034084, 9.711179024262627024, 1.082531754730558626 ) ) ;
#117434 = CARTESIAN_POINT ( 'NONE',  ( 0.4820102390354238375, 2.151571070674349606, -0.8345519191893053801 ) ) ;
#117436 = CARTESIAN_POINT ( 'NONE',  ( 3.770049233051776749, 6.556085317605844232, 1.199719254218451159 ) ) ;
#117437 = CARTESIAN_POINT ( 'NONE',  ( 0.9134385407369073340, -0.3049482027854091837, 2.037980195292460550 ) ) ;
#117438 = CARTESIAN_POINT ( 'NONE',  ( 4.171104814498611368, 8.018039383557042044, 0.7998128361456321445 ) ) ;
#117439 = CONICAL_SURFACE ( 'NONE', #6651, 10.75000000000000000, 0.5235987755983064762 ) ;
#117440 = CARTESIAN_POINT ( 'NONE',  ( 0.3333609138582178111, -1.319029705771988858, 1.524807370920200356 ) ) ;
#117441 = CARTESIAN_POINT ( 'NONE',  ( 3.947104627881618200, 8.980740528188865923, 0.7749999999999996891 ) ) ;
#117442 = CARTESIAN_POINT ( 'NONE',  ( -4.936050443827081580, 7.916420063510339666, 1.199719254218452935 ) ) ;
#117443 = CARTESIAN_POINT ( 'NONE',  ( 6.719622092096638966, -1.813896567892055112, 0.4569536213836836169 ) ) ;
#117446 = EDGE_CURVE ( 'NONE', #196061, #109058, #70725, .T. ) ;
#117445 = CARTESIAN_POINT ( 'NONE',  ( -7.621091744657483069, 8.063897588288083895, 0.7216878364870317197 ) ) ;
#117444 = CARTESIAN_POINT ( 'NONE',  ( 4.271672842113056312, 0.4137096367802223784, -1.866957553337177611 ) ) ;
#117447 = CARTESIAN_POINT ( 'NONE',  ( 5.988949835885216011, -0.3198878037087344306, -2.183464699167809275 ) ) ;
#117448 = CARTESIAN_POINT ( 'NONE',  ( -0.6125000000000019318, 1.270833334016133076, -1.060881119635938008 ) ) ;
#117449 = CARTESIAN_POINT ( 'NONE',  ( -6.414416072596837104, 9.537216947121368804, -1.082531754730549967 ) ) ;
#117450 = CARTESIAN_POINT ( 'NONE',  ( 4.923019175093585886, 5.876515471431535076, -1.082531754730548412 ) ) ;
#117451 = CARTESIAN_POINT ( 'NONE',  ( -3.973948422136970748, 6.690004688251493192, -1.082531754730546636 ) ) ;
#117452 = CARTESIAN_POINT ( 'NONE',  ( 6.569000932001921811, -1.639521903533578850, 1.344440124909966450 ) ) ;
#117453 = ADVANCED_FACE ( 'NONE', ( #133550 ), #37152, .T. ) ;
#117454 = CARTESIAN_POINT ( 'NONE',  ( 2.925200879784293218, 2.172439923367448067, 0.7784344579512092466 ) ) ;
#117455 = CARTESIAN_POINT ( 'NONE',  ( 4.650807877244386823, -0.4278111053654386486, -1.914496481071884970 ) ) ;
#117456 = CARTESIAN_POINT ( 'NONE',  ( 1.287862062775881666, -1.240280065097350448, -1.519972987346601023 ) ) ;
#117457 = DIRECTION ( 'NONE',  ( 0.000000000000000000, 0.000000000000000000, -1.000000000000000000 ) ) ;
#117458 = DIRECTION ( 'NONE',  ( 0.000000000000000000, 8.546850786086437571E-32, 1.000000000000000000 ) ) ;
#117459 = EDGE_LOOP ( 'NONE', ( #126737, #213397, #36950, #25174 ) ) ;
#117460 = CARTESIAN_POINT ( 'NONE',  ( 0.3392563814038212500, -1.792290195912203954, -1.127034558586788249 ) ) ;
#117461 = CARTESIAN_POINT ( 'NONE',  ( -5.447678794592645701, 5.250046769979851646, 0.000000000000000000 ) ) ;
#117462 = DIRECTION ( 'NONE',  ( 1.000000000000000000, 0.000000000000000000, 0.000000000000000000 ) ) ;
#117463 = CARTESIAN_POINT ( 'NONE',  ( 4.030270078087188068, 1.201442806954319487, 1.808153907555063000 ) ) ;
#117464 = CARTESIAN_POINT ( 'NONE',  ( 1.423205080756849483, 7.980384757729337863, -10.65537363484302524 ) ) ;
#117465 = CARTESIAN_POINT ( 'NONE',  ( 1.881254504445781794, -1.940830296247602949, -0.8548571619346673200 ) ) ;
#117466 = CARTESIAN_POINT ( 'NONE',  ( 1.499999999999987121, 3.327083334016150751, -0.8660254037844262731 ) ) ;
#117467 = CARTESIAN_POINT ( 'NONE',  ( 9.215791728987056786, 11.77484298861683598, -1.599625672291262513 ) ) ;
#117468 = CARTESIAN_POINT ( 'NONE',  ( -1.040834085586084257E-14, 0.000000000000000000, -9.579665964948867796 ) ) ;
#117469 = CARTESIAN_POINT ( 'NONE',  ( 6.512538272292041519, 6.827515365185738538, -0.5364851146780359459 ) ) ;
#117470 = ORIENTED_EDGE ( 'NONE', *, *, #98066, .T. ) ;
#117471 = CARTESIAN_POINT ( 'NONE',  ( 1.880222553438152033, -1.104958259108330898, 1.739320704499922154 ) ) ;
#117473 = CARTESIAN_POINT ( 'NONE',  ( 1.479373551132449505, 3.300000000000025135, 0.2478989637125245671 ) ) ;
#117472 = CARTESIAN_POINT ( 'NONE',  ( -7.818248136574758256, 12.27303992597924420, 0.000000000000000000 ) ) ;
#117474 = CARTESIAN_POINT ( 'NONE',  ( -1.201851678989727383E-14, 2.071875000341422801, 1.575800808251672791 ) ) ;
#117475 = CARTESIAN_POINT ( 'NONE',  ( 0.07775346131144719730, 4.079442786094135798, -2.843586357576178614 ) ) ;
#117476 = CARTESIAN_POINT ( 'NONE',  ( -2.373851744317279522, 1.000000000000000888, 11.76285798163022100 ) ) ;
#117477 = ORIENTED_EDGE ( 'NONE', *, *, #154446, .T. ) ;
#117478 = CARTESIAN_POINT ( 'NONE',  ( 5.039673278062164918, -1.814583965733532978, 0.6035816954967700987 ) ) ;
#117479 = AXIS2_PLACEMENT_3D ( 'NONE', #201447, #18449, #5373 ) ;
#117480 = CARTESIAN_POINT ( 'NONE',  ( 7.204675194429079505E-15, -1.137499999999999512, -3.475000000000000089 ) ) ;
#117481 = CARTESIAN_POINT ( 'NONE',  ( 2.056323133375201007, 2.256402538945650349, -0.1652075827990733270 ) ) ;
#117482 = CARTESIAN_POINT ( 'NONE',  ( -4.437596350374534815, 4.071617251725375475, -0.7998128361456221525 ) ) ;
#117483 = CARTESIAN_POINT ( 'NONE',  ( 1.845701740803426194, -1.185437281251604746, -1.369922693571566485 ) ) ;
#117484 = CARTESIAN_POINT ( 'NONE',  ( 1.042033841529757421, 0.7795281806207611242, 1.750150644309953041 ) ) ;
#117485 = CARTESIAN_POINT ( 'NONE',  ( 2.541538742049511246, 1.893869637037654208, -0.8368498079355383146 ) ) ;
#117486 = CARTESIAN_POINT ( 'NONE',  ( -1.364683531250000748, 1.571875000341421691, 0.000000000000000000 ) ) ;
#117487 = CARTESIAN_POINT ( 'NONE',  ( 0.1980364362535640133, -1.970970528886636153, -0.05095907160383715551 ) ) ;
#117488 = CARTESIAN_POINT ( 'NONE',  ( 6.041620323887018529, -1.397190737843529540, -1.326607404314980254 ) ) ;
#117490 = CARTESIAN_POINT ( 'NONE',  ( 6.423677080210483226, 6.791898735554919853, -0.4454198846488600649 ) ) ;
#117489 = CARTESIAN_POINT ( 'NONE',  ( 0.3293365701910222487, 2.210228212078951149, 0.6636047247109229108 ) ) ;
#117491 = CARTESIAN_POINT ( 'NONE',  ( 1.364683531249988535, 1.363541667008083769, 0.7879004041258500513 ) ) ;
#117492 = CARTESIAN_POINT ( 'NONE',  ( 4.738769042418014443, -1.999979230503599048, -0.5042011814720639418 ) ) ;
#117493 = CARTESIAN_POINT ( 'NONE',  ( -5.930802130974132780, 9.006687355190106103, -1.199719254218440723 ) ) ;
#117494 = CARTESIAN_POINT ( 'NONE',  ( 7.507464373665139412, 9.781794407407920389, 1.599625672291281386 ) ) ;
#117495 = CARTESIAN_POINT ( 'NONE',  ( 3.194917754314666514, 6.879154480009089134, 0.7998128361456321445 ) ) ;
#117496 = CARTESIAN_POINT ( 'NONE',  ( 5.144429221381498607, 8.089252293998699272, -1.199719254218452047 ) ) ;
#117498 = CARTESIAN_POINT ( 'NONE',  ( -1.500000000000013101, 4.129166666666687746, -0.8660254037844313801 ) ) ;
#117497 = CARTESIAN_POINT ( 'NONE',  ( 5.649480931864863109, -1.658039504894607719, -1.298324887859639842 ) ) ;
#117499 = CARTESIAN_POINT ( 'NONE',  ( 0.6081839208269465002, 0.6806018353129331677, -2.061787349250172596 ) ) ;
#117500 = CARTESIAN_POINT ( 'NONE',  ( -0.6823417656249969321, 3.280208333674754062, -1.181850606188749264 ) ) ;
#117501 = CARTESIAN_POINT ( 'NONE',  ( 5.167319818800252484, 0.2175342549677051207, -2.150644138106901693 ) ) ;
#117502 = CARTESIAN_POINT ( 'NONE',  ( 4.899084735882781594, -0.2492385452713632155, -2.004177415419911679 ) ) ;
#117503 = CARTESIAN_POINT ( 'NONE',  ( -5.748293942514174582, 5.808690475795755148, -0.7216878364870319418 ) ) ;
#117506 = CARTESIAN_POINT ( 'NONE',  ( 4.351804120306567825, 8.020929207092235558, 1.040834085586084257E-14 ) ) ;
#117505 = CARTESIAN_POINT ( 'NONE',  ( -3.285556943750000514, -1.188541666188710044, -1.896917185911906500 ) ) ;
#117504 = CARTESIAN_POINT ( 'NONE',  ( 6.556249800660121529, 9.806652646482286073, 1.199719254218452047 ) ) ;
#117507 = CARTESIAN_POINT ( 'NONE',  ( -5.981082042284069367, 7.006959133200059142, 1.199719254218452935 ) ) ;
#117508 = CARTESIAN_POINT ( 'NONE',  ( 4.065638850954083061, 1.320825628876612479, 1.523796413913918846 ) ) ;
#117509 = CARTESIAN_POINT ( 'NONE',  ( -7.492852449846775897, 11.89341162479659531, 0.000000000000000000 ) ) ;
#117511 = CARTESIAN_POINT ( 'NONE',  ( -8.041394506236766659, 8.554250810130591631, -0.7216878364870338292 ) ) ;
#117510 = CARTESIAN_POINT ( 'NONE',  ( -4.437596350374534815, 4.071617251725375475, -0.7998128361456221525 ) ) ;
#117512 = CARTESIAN_POINT ( 'NONE',  ( 4.909125497034264818, 1.879091090907711425, 1.068517025386829467 ) ) ;
#117513 = CARTESIAN_POINT ( 'NONE',  ( 0.4694063952341808177, -6.893137084989842123, 10.98997987423603995 ) ) ;
#117514 = CARTESIAN_POINT ( 'NONE',  ( 7.346809171966453889, -6.836568542494980250, 8.002408263930263388 ) ) ;
#117516 = CARTESIAN_POINT ( 'NONE',  ( 5.730092268227672037, 2.014234620932173758, 0.09611943034040781875 ) ) ;
#117515 = CARTESIAN_POINT ( 'NONE',  ( -6.304178240230145391, 9.338329799368375816, 1.082531754730548412 ) ) ;
#117517 = CARTESIAN_POINT ( 'NONE',  ( 0.7499999999999902300, 5.316666666666685082, -1.299038105676658228 ) ) ;
#117518 = CARTESIAN_POINT ( 'NONE',  ( 0.6270765232691848379, -1.639361371195736439, 0.5365680580288884061 ) ) ;
#117519 = CARTESIAN_POINT ( 'NONE',  ( 5.037736595929563244, 8.035053907629919223, -1.199719254218452047 ) ) ;
#117521 = CARTESIAN_POINT ( 'NONE',  ( 6.831329296439236032, 9.063246493969506545, -1.599625672291267398 ) ) ;
#117520 = CARTESIAN_POINT ( 'NONE',  ( 8.771762198361678031, 9.336070107617867819, 1.040834085586084257E-14 ) ) ;
#117522 = CARTESIAN_POINT ( 'NONE',  ( 6.966220764712121927, 6.002124920821316323, 2.500000000000000444 ) ) ;
#117523 = CARTESIAN_POINT ( 'NONE',  ( 5.501189692264965458, 1.528658022856645315, 1.077728667985423661 ) ) ;
#117524 = CARTESIAN_POINT ( 'NONE',  ( 6.011982430150495382, -0.6741147929612385514, 1.897138445369117354 ) ) ;
#117525 = SURFACE_STYLE_FILL_AREA ( #184577 ) ;
#117526 = CARTESIAN_POINT ( 'NONE',  ( -7.078765599666485997, 7.431183752465250869, 0.000000000000000000 ) ) ;
#117527 = ORIENTED_EDGE ( 'NONE', *, *, #51328, .F. ) ;
#117528 = CARTESIAN_POINT ( 'NONE',  ( 10.37162432432990755, 11.20257592124748136, -0.7216878364870257245 ) ) ;
#117530 = CARTESIAN_POINT ( 'NONE',  ( 1.775017769237042353, 1.753020666602569166, -0.9963212463810557917 ) ) ;
#117529 = CARTESIAN_POINT ( 'NONE',  ( 2.350376503035214615, 0.9972050307137376723, -1.871358364749615033 ) ) ;
#117531 = CARTESIAN_POINT ( 'NONE',  ( 1.652323331381430283, 1.792179557038487303, 0.2633440673391762576 ) ) ;
#117532 = CARTESIAN_POINT ( 'NONE',  ( 6.770317605177710085, 8.992066187497757213, 1.599625672291268286 ) ) ;
#117533 = CARTESIAN_POINT ( 'NONE',  ( 6.719591497160966931, -2.098179372288328182, 0.5198544864785522579 ) ) ;
#117534 = CIRCLE ( 'NONE', #110593, 2.750000000000008438 ) ;
#117535 = CARTESIAN_POINT ( 'NONE',  ( 7.558834334818744338, 8.777393797832065303, 1.199719254218462483 ) ) ;
#117537 = CARTESIAN_POINT ( 'NONE',  ( -0.08300117844089061059, -1.750507139949438296, 0.7787328797612643738 ) ) ;
#117536 = CARTESIAN_POINT ( 'NONE',  ( -3.879604511804807032, 7.677955697080923514, 0.7998128361456341429 ) ) ;
#117538 = CARTESIAN_POINT ( 'NONE',  ( -1.499999999999997780, 5.150000000000022560, 1.214306433183764808E-14 ) ) ;
#117539 = LINE ( 'NONE', #165159, #162976 ) ;
#117540 =( BOUNDED_CURVE ( )  B_SPLINE_CURVE ( 2, ( #11998, #127997, #161481, #111715, #79139, #50904, #134320, #34643, #17310 ),
 .UNSPECIFIED., .F., .T. ) 
 B_SPLINE_CURVE_WITH_KNOTS ( ( 3, 2, 2, 2, 3 ),
 ( 0.3281250000000001665, 0.3333333333333333148, 0.3437500000000000000, 0.3541666666666666852, 0.3593749999999997224 ),
 .UNSPECIFIED. ) 
 CURVE ( )  GEOMETRIC_REPRESENTATION_ITEM ( )  RATIONAL_B_SPLINE_CURVE ( ( 0.9330127018922194093, 0.9330127018922215187, 1.000000000000000000, 0.8660254037844387076, 1.000000000000000000, 0.8660254037844387076, 1.000000000000000000, 0.9330127018922229620, 0.9330127018922194093 ) ) 
 REPRESENTATION_ITEM ( '' )  );
#117541 = CARTESIAN_POINT ( 'NONE',  ( 5.463572716182824252, 7.397254140345190798, 1.443375672974062551 ) ) ;
#117542 = CARTESIAN_POINT ( 'NONE',  ( 5.514321724087592358, 5.998106097858366681, 0.7610078497430600164 ) ) ;
#117543 = CARTESIAN_POINT ( 'NONE',  ( 3.172244755917638770, 5.684407401003788607, -1.082531754730543083 ) ) ;
#117544 = CARTESIAN_POINT ( 'NONE',  ( -3.379006598303881059, 4.965260336153046516, -1.599625672291256295 ) ) ;
#117545 = CARTESIAN_POINT ( 'NONE',  ( 4.504844740329728481, 1.672958716126593082, -1.369014088531981255 ) ) ;
#117546 = CARTESIAN_POINT ( 'NONE',  ( -6.834718835064852449, 8.106831741398025315, 1.082531754730549078 ) ) ;
#117547 = CARTESIAN_POINT ( 'NONE',  ( 5.180624094197585627, 8.097792972322238825, -1.082531754730548412 ) ) ;
#117548 = CARTESIAN_POINT ( 'NONE',  ( 1.582450481569739331, 1.094613367649547309, 1.816135667671102016 ) ) ;
#117549 = DIRECTION ( 'NONE',  ( -1.000000000000000000, 0.000000000000000000, 0.000000000000000000 ) ) ;
#117550 = CARTESIAN_POINT ( 'NONE',  ( 2.143765197515819843, 0.7580581125649475949, -1.819971111534921970 ) ) ;
#117551 = CARTESIAN_POINT ( 'NONE',  ( 4.447458312869024155, -1.746245811230532130, 0.7801085911468002010 ) ) ;
#117552 = VERTEX_POINT ( 'NONE', #17599 ) ;
#117553 = CARTESIAN_POINT ( 'NONE',  ( 9.496663239506002441, -6.863887327018314721, 0.01979922387980803319 ) ) ;
#117554 = CARTESIAN_POINT ( 'NONE',  ( 6.531706384513794816, 1.885137803977337656, -0.5704747015483744299 ) ) ;
#117555 = CARTESIAN_POINT ( 'NONE',  ( 1.236160255307724665, 0.3784122030587311336, 1.904561997804487428 ) ) ;
#117556 = ORIENTED_EDGE ( 'NONE', *, *, #24376, .T. ) ;
#117557 = CARTESIAN_POINT ( 'NONE',  ( -4.176793841461789114, 7.030620694084159794, -1.199719254218455378 ) ) ;
#117558 = CARTESIAN_POINT ( 'NONE',  ( -2.810282979782591006, 6.500690253046801814, 0.000000000000000000 ) ) ;
#117559 = CARTESIAN_POINT ( 'NONE',  ( 6.982612806237943559, 8.105135347821125436, -1.199719254218446718 ) ) ;
#117561 = CARTESIAN_POINT ( 'NONE',  ( 4.868786560638885597, 7.733982516503781213, 1.082531754730548412 ) ) ;
#117560 = CARTESIAN_POINT ( 'NONE',  ( 7.470706336329915764, 8.674577799595093452, -1.199719254218441611 ) ) ;
#117563 = VERTEX_POINT ( 'NONE', #83683 ) ;
#117562 = CARTESIAN_POINT ( 'NONE',  ( 5.918603479541379109, -0.6925943527147163659, -1.782627650866043911 ) ) ;
#117564 = CARTESIAN_POINT ( 'NONE',  ( 3.264504910713565078, 0.9923201075644829672, 1.971275125648555449 ) ) ;
#117565 = EDGE_CURVE ( 'NONE', #197638, #74053, #140796, .T. ) ;
#117566 = CARTESIAN_POINT ( 'NONE',  ( 1.747397587315654865, -1.864034986486883261, 1.180896971623420999 ) ) ;
#117567 = CARTESIAN_POINT ( 'NONE',  ( 0.000000000000000000, 8.980740528189222971, 0.000000000000000000 ) ) ;
#117568 = CARTESIAN_POINT ( 'NONE',  ( 0.7504700684401002242, 1.884043224930329385, 0.3264296256808990049 ) ) ;
#117569 = CARTESIAN_POINT ( 'NONE',  ( -4.741649638052999549, 5.202212439478444139, 1.069586989871945670 ) ) ;
#117570 = CARTESIAN_POINT ( 'NONE',  ( -6.692370362267773487, -7.020359948792200377, -6.743487189266383908 ) ) ;
#117571 = CARTESIAN_POINT ( 'NONE',  ( 3.420434311836465291, 0.9283866757503268508, 1.850595421526677775 ) ) ;
#117572 = CARTESIAN_POINT ( 'NONE',  ( -6.033542053281340856, 6.997886136038390603, -1.199719254218446718 ) ) ;
#117573 = CARTESIAN_POINT ( 'NONE',  ( -5.076314662610137418, 7.858265529090583179, 1.124058833742283436 ) ) ;
#117575 = CARTESIAN_POINT ( 'NONE',  ( 1.393688021309073433, 1.637156065531343740, 1.411701162175371893 ) ) ;
#117574 = CARTESIAN_POINT ( 'NONE',  ( -3.093231602212184850, 6.760520635889515795, -0.7998128361456281477 ) ) ;
#117576 = CARTESIAN_POINT ( 'NONE',  ( 3.948915171154475878, -1.822730400009948237, -1.216494452853926322 ) ) ;
#117577 = CARTESIAN_POINT ( 'NONE',  ( -0.3282377607281493637, 0.8013354503153625741, 1.224999999999967004 ) ) ;
#117578 = ADVANCED_FACE ( 'NONE', ( #33871 ), #116257, .F. ) ;
#117579 = CARTESIAN_POINT ( 'NONE',  ( 3.553645660557675612, 6.199651466408984568, -1.082531754730549967 ) ) ;
#117580 = CARTESIAN_POINT ( 'NONE',  ( -1.225000000000024736, 1.062500000682836676, -3.122502256758252770E-14 ) ) ;
#117581 = AXIS2_PLACEMENT_3D ( 'NONE', #102297, #182469, #15704 ) ;
#117582 = CARTESIAN_POINT ( 'NONE',  ( -1.364683531250010295, 14.19270833367473195, 0.7879004041258445001 ) ) ;
#117583 = CARTESIAN_POINT ( 'NONE',  ( -5.224688093219839402, 7.188831756880171397, -1.599625672291271394 ) ) ;
#117585 = EDGE_CURVE ( 'NONE', #5998, #6228, #164320, .T. ) ;
#117584 = PRODUCT_DEFINITION_CONTEXT ( 'detailed design', #162660, 'design' ) ;
#117586 = CARTESIAN_POINT ( 'NONE',  ( 6.311143239517568837, 0.9901597221020401740, -1.423469027432751943 ) ) ;
#117587 = CARTESIAN_POINT ( 'NONE',  ( -3.277320446201389181, 4.846626492033466072, 1.599625672291267398 ) ) ;
#117588 = CARTESIAN_POINT ( 'NONE',  ( 3.854399998794607818, -2.067664388167046674, -0.1065051105964970740 ) ) ;
#117589 = CARTESIAN_POINT ( 'NONE',  ( 4.675474996081856460, 1.569897879423647336, 1.420792320860002178 ) ) ;
#117590 = CARTESIAN_POINT ( 'NONE',  ( 6.959412922516382771, 7.013736585890911535, 0.7998128361456341429 ) ) ;
#117591 = CARTESIAN_POINT ( 'NONE',  ( 1.364683531249988535, 4.155208333674753618, -0.7879004041258239610 ) ) ;
#117592 = CARTESIAN_POINT ( 'NONE',  ( 2.623828205405827507, 1.932375918485039756, -0.3793698109293401344 ) ) ;
#117593 = CARTESIAN_POINT ( 'NONE',  ( 0.5449873876890098945, 0.1430962203496731200, 1.907122450762772647 ) ) ;
#117594 = CARTESIAN_POINT ( 'NONE',  ( 4.295090358266894448, 1.839821235612853600, 1.367129665020486273 ) ) ;
#117595 = CARTESIAN_POINT ( 'NONE',  ( 2.807047293222181494, 1.542382716246639696, 0.9765254425028800922 ) ) ;
#117596 = CARTESIAN_POINT ( 'NONE',  ( 5.252858170651868441, 5.093032385374103299, -0.7998128361456481317 ) ) ;
#117597 = CARTESIAN_POINT ( 'NONE',  ( 5.300874872818830852, 7.207439989753867238, 1.443375672974062551 ) ) ;
#117598 = CARTESIAN_POINT ( 'NONE',  ( -6.235860587281615075, 9.362588887548838557, -1.199719254218440723 ) ) ;
#117599 = ORIENTED_EDGE ( 'NONE', *, *, #203936, .F. ) ;
#117600 = EDGE_LOOP ( 'NONE', ( #70909, #87796, #50620, #10134 ) ) ;
#117601 = CARTESIAN_POINT ( 'NONE',  ( 4.271743731491533858, 0.4368499997736470797, -1.965098791395853750 ) ) ;
#117602 = CARTESIAN_POINT ( 'NONE',  ( 4.082823661314609609, 1.861412734803047142, 0.6194944872321901386 ) ) ;
#117603 = CARTESIAN_POINT ( 'NONE',  ( -6.184490626128011925, 10.36698949712469364, -0.7998128361456291469 ) ) ;
#117604 = CARTESIAN_POINT ( 'NONE',  ( -4.791917227426195858, 7.677988301050826969, -1.199719254218452047 ) ) ;
#117605 = FACE_OUTER_BOUND ( 'NONE', #201402, .T. ) ;
#117607 = CARTESIAN_POINT ( 'NONE',  ( 5.383597848809928088, 1.190821987996647513, 1.309499010278234898 ) ) ;
#117606 = CARTESIAN_POINT ( 'NONE',  ( 0.6090670738765286973, -0.3027767823605455599, 2.068569423397928819 ) ) ;
#117608 = CARTESIAN_POINT ( 'NONE',  ( -3.621833129746846680, 4.096114899008192367, 2.420000000000010587 ) ) ;
#117609 = CARTESIAN_POINT ( 'NONE',  ( 2.220887445055406584, 0.001640320231081903845, 2.191629467496846839 ) ) ;
#117610 = CARTESIAN_POINT ( 'NONE',  ( 0.1865103356883268948, 1.287481616103260063, 1.171338548376497535 ) ) ;
#117611 = CARTESIAN_POINT ( 'NONE',  ( 6.642605195691581699, 9.837124264027149678, 1.199719254218462483 ) ) ;
#117612 = CARTESIAN_POINT ( 'NONE',  ( 0.1333692844072559280, 0.001398348041498076455, -2.053671342968105051 ) ) ;
#117613 = CARTESIAN_POINT ( 'NONE',  ( 0.3985097114710112742, 1.437023721582047830, -0.9536953323180746844 ) ) ;
#117614 = CARTESIAN_POINT ( 'NONE',  ( 1.124856824619735463, 0.4467566299657543816, -2.254411929275771609 ) ) ;
#117615 = CARTESIAN_POINT ( 'NONE',  ( 0.9607770615731696662, -1.983481723135366304, -0.9323335341336475013 ) ) ;
#117616 = CARTESIAN_POINT ( 'NONE',  ( 6.661516750719080449, -0.4673772157907078451, -1.669595843636323185 ) ) ;
#117617 = CARTESIAN_POINT ( 'NONE',  ( 3.264504910713565078, 0.9923201075644829672, 1.971275125648555449 ) ) ;
#117618 = CARTESIAN_POINT ( 'NONE',  ( 6.503150282362620160, -0.1410805869419759218, 1.984311032119711715 ) ) ;
#117619 =( BOUNDED_SURFACE ( )  B_SPLINE_SURFACE ( 1, 2, ( 
 ( #157256, #204895, #122709, #71697, #55473, #188672, #58675, #40305, #7768, #25095, #91196, #8848, #121628, #74928, #124824, #190790, #42452, #170281, #21869, #33472, #133145, #212207, #112667, #30290, #63843, #17199, #48673, #213272, #15070, #145140, #16130, #199145, #113735, #32413, #164545, #98479, #132086, #128932, #82214, #943, #214306, #198096, #148308, #65937, #49723, #80088, #50789, #64901, #115852, #181837, #99546, #165610, #96376, #83273, #62768, #149361, #194909, #46547, #146192, #31358, #147245, #179741, #131049, #67008, #116918, #182919, #34534, #81162, #161361, #12944, #130000, #79024, #178675, #114790, #195990, #14004, #211146, #162427, #47623, #97433, #197038, #163488, #180790, #117991, #137393, #151505, #72355, #88642, #187182, #183984, #37744, #122289, #103819, #86491, #138458, #2007, #204477, #150445, #68073, #3074, #153633, #20409, #188246, #87565, #19342, #100605, #203410, #56130, #6282, #69145, #166681, #201280, #18273, #101673, #38809, #53994, #167743, #104895, #84355, #135266, #51870, #35595, #52921, #170934, #202342, #152555, #168803, #134209, #169866, #200219, #119052, #186110, #21457, #5206, #71279, #85421, #55063, #154699, #121213, #22533, #185037, #36662, #4142, #102747, #70212, #136324, #120133, #173096, #110283, #209824, #105997, #75583, #74518, #124421, #189324, #109225, #8430, #156846, #175235, #59326, #61460, #90783, #206633, #157916, #7352, #58264, #174177, #141693, #126550, #40965, #140621, #191445, #207706, #42039, #73431, #139534, #160032, #107073, #125483, #43110, #92923, #176292, #123359, #205559, #190379, #57199, #24677, #9511, #77707, #108151, #26819, #25748, #91861, #158969, #10563, #39887, #23609, #76638, #127626, #93991, #11634, #89718, #142752, #208761, #60386, #192511, #44163, #27896, #172018, #143827, #155768, #96120, #161102, #31112, #162175, #195735, #81967, #46298, #144889, #131836, #178425, #145946, #177354, #28968, #13761, #99303, #79838, #112413, #30034, #211957, #63595, #95051, #129750, #210896, #180539, #47370, #97186, #680, #113483, #128685, #12690, #130797, #163239, #179490, #114548, #194654, #14821, #80913, #62523, #193590, #147003, #15883, #213021, #64656, #196791, #48432, #32162, #181590, #148054, #65688, #78766, #98239, #164294, #214060, #45234, #197843, #49476, #115596, #33219, #165351, #16945, #83024, #149101, #66747, #111349, #50537, #34278, #87303, #100351, #4943, #201023, #133960, #68890, #153372, #151250, #67813, #101418, #36408, #135009, #154443, #132888, #84100, #52666, #169617, #199968, #35338, #38557, #6023, #20150, #118795, #185849, #203161, #1756, #166419, #183732, #150187, #51616, #102487, #170680, #117739, #168551, #167490, #184782, #86235, #19086, #198891, #116660, #152306, #182658, #186925, #104633, #18011, #3883, #69953, #136065, #202078, #85166, #2819, #53738, #119870, #103558, #37481, #21201, #71019, #137132, #54806, #120954, #22267, #88376, #10306, #56938, #24407, #55868, #122024, #106807, #192247, #40703, #139269, #123110, #172836, #189068, #187991, #90522, #23345, #59063, #8178, #190126, #93729, #156584, #7090, #39616, #9250, #41780, #74262, #207444, #73163, #140355, #205299, #89456, #72093, #206373, #108956, #155508, #58000, #124164, #107894, #173921, #60130, #174976, #158709, #105720, #25494, #125223, #91601, #138203, #157652, #75321, #141438, #191181, #126288, #42849, #26558, #92665, #76380, #142489, #204215, #171749, #208495, #43909, #110023, #176037, #27629, #159769, #31916, #29780, #160841, #194399, #129496, #13511, #32970, #11368, #177092, #79583, #48183, #78513, #128432, #131587, #99046, #113226, #145701, #179230, #211701, #193331, #111085, #197589, #12433, #30856, #47110, #210645, #46041, #144630, #28707, #213818, #62271, #63337, #180293, #97994, #212769, #143565, #127361, #164052, #44977, #15631, #195477, #112162, #161920, #81718, #95864, #178165, #96933, #162983, #14564, #77447, #209558, #94793, #80660, #114295, #146751, #64405, #49233, #61203, #130549, #196540, #147800, #65436, #115352, #181343, #70764, #166161, #118546, #200769, #3627, #20948, #34027, #198641, #1497, #182398, #100101, #68637, #202904, #149928 ),
 ( #167237, #18826, #17748, #35080, #16692, #152057, #135809, #67563, #132635, #2566, #133706, #84910, #53477, #83838, #116408, #103301, #199712, #117482, #148850, #423, #51358, #136878, #183473, #101152, #150998, #134761, #52420, #66496, #184528, #36150, #69705, #102230, #168301, #186671, #19897, #85981, #50289, #201832, #119614, #185599, #37230, #169363, #87045, #153118, #4689, #165101, #54549, #120696, #38298, #82778, #56688, #122855, #105463, #92416, #141182, #190932, #88120, #74002, #91342, #72916, #170423, #155256, #188816, #7916, #71837, #40450, #24160, #206122, #42596, #39366, #205045, #41522, #107634, #23088, #76132, #140095, #157402, #173666, #25241, #8994, #171497, #207191, #5758, #26302, #137946, #203968, #89203, #106552, #90263, #172579, #156331, #75069, #58817, #124970, #108701, #57752, #158456, #174730, #6838, #10055, #55614, #123912, #139021, #189879, #142235, #208247, #22010, #59881, #126030, #191993, #104376, #121769, #154190, #187738, #18306, #34568, #130299, #127107, #195222, #68109, #46859, #29525, #84392, #159515, #150479, #93477, #11114, #94544, #96685, #177911, #134245, #30598, #176837, #43658, #80401, #2039, #166716, #160582, #109775, #144384, #175784, #44723, #196287, #211448, #110832, #50827, #27376, #12189, #209303, #193072, #78260, #116954, #145451, #95617, #111911, #77190, #112972, #143311, #210384, #129251, #178984, #162734, #14306, #60950, #146498, #100639, #212515, #64157, #182953, #28451, #161667, #62025, #128181, #194142, #45791, #13261, #79333, #63082, #51904, #21490, #20443, #70246, #135299, #55100, #168839, #102782, #121249, #5239, #155806, #201313, #72394, #153671, #52953, #138494, #172055, #36697, #151540, #69179, #86525, #56163, #87600, #37779, #54031, #184014, #187219, #23648, #152590, #71315, #203446, #137427, #170973, #167779, #38848, #39925, #104931, #22572, #88678, #154737, #120168, #118026, #119091, #204515, #6320, #185071, #122327, #7389, #35629, #188284, #4177, #136361, #202381, #106033, #186144, #103853, #89757, #73469, #200252, #169902, #101707, #19375, #85455, #3108, #59359, #26852, #11667, #74553, #25783, #76672, #142787, #58299, #111383, #43146, #192544, #208793, #60423, #126583, #140654, #176324, #40999, #61493, #107110, #24714, #124455, #9543, #125516, #91895, #191478, #110317, #44197, #27930, #160063, #109259, #193622, #143862, #190414, #94024, #90816, #92956, #42070, #206667, #177386, #77741, #57234, #174210, #175267, #157951, #108184, #156880, #209855, #75617, #29000, #127658, #45263, #8467, #95087, #161135, #12723, #159003, #139570, #173133, #205597, #189359, #141728, #207736, #123395, #10596, #166456, #65719, #211988, #100384, #115626, #116692, #198924, #129783, #182691, #179523, #34309, #62552, #48464, #131867, #47403, #144919, #63629, #113515, #145976, #96155, #66778, #79867, #130830, #33250, #165383, #197874, #210926, #194686, #99334, #46328, #16976, #147033, #195764, #14851, #83057, #97217, #13793, #31142, #196822, #80941, #78796, #128715, #30066, #213055, #181621, #163269, #64684, #50570, #112444, #180570, #114578, #32192, #98268, #178457, #162206, #164326, #15916, #81999, #148086, #49506, #149133, #214091, #714, #132919, #35376, #167523, #136100, #55905, #2855, #202116, #52699, #152341, #185884, #19120, #18047, #1792, #86270, #105764, #72132, #138239, #67849, #119909, #69988, #20183, #3919, #85199, #102520, #84134, #4979, #203197, #135045, #200002, #53776, #201058, #37519, #120994, #151284, #183766, #170718, #68924, #184816, #133996, #51652, #118830, #204253, #36446, #168583, #103595, #169652, #21237, #117775, #87342, #101450, #71057, #153410, #137173, #39655, #54843, #186961, #38593, #104670, #22304, #88415, #154483, #6061, #122062, #188026, #150220, #171789, #190164, #208530, #189106, #124200, #41818, #107931, #172876, #159802, #60166, #43942, #139308, #56975, #77483, #24448, #125259, #207479, #10337, #27668, #40739, #205337, #8212, #106845, #90560, #75360, #209594, #156622, #141472, #206412, #91637, #191219, #74297, #23384, #155550, #25529, #45013, #11406, #143602, #7129, #59099, #9287, #173955, #157689, #140393, #42882, #89496, #158743 ) ),
 .UNSPECIFIED., .F., .F., .T. ) 
 B_SPLINE_SURFACE_WITH_KNOTS ( ( 2, 2 ),
 ( 3, 2, 2, 2, 2, 2, 2, 2, 2, 2, 2, 2, 2, 2, 2, 2, 2, 2, 2, 2, 2, 2, 2, 2, 2, 2, 2, 2, 2, 2, 2, 2, 2, 2, 2, 2, 2, 2, 2, 2, 2, 2, 2, 2, 2, 2, 2, 2, 2, 2, 2, 2, 2, 2, 2, 2, 2, 2, 2, 2, 2, 2, 2, 2, 2, 2, 2, 2, 2, 2, 2, 2, 2, 2, 2, 2, 2, 2, 2, 2, 2, 2, 2, 2, 2, 2, 2, 2, 2, 2, 2, 2, 2, 2, 2, 2, 2, 2, 2, 2, 2, 2, 2, 2, 2, 2, 2, 2, 2, 2, 2, 2, 2, 2, 2, 2, 2, 2, 2, 2, 2, 2, 2, 2, 2, 2, 2, 2, 2, 2, 2, 2, 2, 2, 2, 2, 2, 2, 2, 2, 2, 2, 2, 2, 2, 2, 2, 2, 2, 2, 2, 2, 2, 2, 2, 2, 2, 2, 2, 2, 2, 2, 2, 2, 2, 2, 2, 2, 2, 2, 2, 2, 2, 2, 2, 2, 2, 2, 2, 2, 2, 2, 2, 2, 2, 2, 2, 2, 2, 2, 2, 2, 2, 2, 2, 2, 2, 2, 2, 2, 2, 2, 2, 2, 2, 2, 2, 2, 2, 2, 2, 2, 2, 2, 2, 2, 2, 2, 2, 2, 2, 2, 2, 2, 2, 2, 2, 2, 2, 2, 2, 2, 2, 2, 2, 2, 2, 2, 2, 2, 3 ),
 ( 0.000000000000000000, 1.000000000000000000 ),
 ( 0.000000000000000000, 0.004166666666666666609, 0.008333333333333333218, 0.01250000000000000069, 0.01666666666666666644, 0.02083333333333333218, 0.02500000000000000139, 0.02916666666666666713, 0.03333333333333333287, 0.03749999999999999861, 0.04166666666666666435, 0.04583333333333333010, 0.05000000000000000278, 0.05416666666666666852, 0.05833333333333333426, 0.06250000000000000000, 0.06666666666666666574, 0.07083333333333333148, 0.07499999999999999722, 0.07916666666666666297, 0.08333333333333332871, 0.08749999999999999445, 0.09166666666666666019, 0.09583333333333333981, 0.1000000000000000056, 0.1041666666666666713, 0.1083333333333333370, 0.1125000000000000028, 0.1166666666666666685, 0.1208333333333333343, 0.1250000000000000000, 0.1291666666666666796, 0.1333333333333333315, 0.1375000000000000111, 0.1416666666666666630, 0.1458333333333333426, 0.1499999999999999944, 0.1541666666666666741, 0.1583333333333333259, 0.1625000000000000056, 0.1666666666666666574, 0.1708333333333333370, 0.1749999999999999889, 0.1791666666666666685, 0.1833333333333333204, 0.1875000000000000000, 0.1916666666666666796, 0.1958333333333333315, 0.2000000000000000111, 0.2041666666666666630, 0.2083333333333333426, 0.2124999999999999944, 0.2166666666666666741, 0.2208333333333333259, 0.2250000000000000056, 0.2291666666666666574, 0.2333333333333333370, 0.2374999999999999889, 0.2416666666666666685, 0.2458333333333333204, 0.2500000000000000000, 0.2541666666666666519, 0.2583333333333333592, 0.2625000000000000111, 0.2666666666666666630, 0.2708333333333333148, 0.2750000000000000222, 0.2791666666666666741, 0.2833333333333333259, 0.2874999999999999778, 0.2916666666666666852, 0.2958333333333333370, 0.2999999999999999889, 0.3041666666666666408, 0.3083333333333333481, 0.3125000000000000000, 0.3166666666666666519, 0.3208333333333333592, 0.3250000000000000111, 0.3291666666666666630, 0.3333333333333333148, 0.3375000000000000222, 0.3416666666666666741, 0.3458333333333333259, 0.3499999999999999778, 0.3541666666666666852, 0.3583333333333333370, 0.3624999999999999889, 0.3666666666666666408, 0.3708333333333333481, 0.3750000000000000000, 0.3791666666666666519, 0.3833333333333333592, 0.3875000000000000111, 0.3916666666666666630, 0.3958333333333333148, 0.4000000000000000222, 0.4041666666666666741, 0.4083333333333333259, 0.4124999999999999778, 0.4166666666666666852, 0.4208333333333333370, 0.4249999999999999889, 0.4291666666666666408, 0.4333333333333333481, 0.4375000000000000000, 0.4416666666666666519, 0.4458333333333333592, 0.4500000000000000111, 0.4541666666666666630, 0.4583333333333333148, 0.4625000000000000222, 0.4666666666666666741, 0.4708333333333333259, 0.4749999999999999778, 0.4791666666666666852, 0.4833333333333333370, 0.4874999999999999889, 0.4916666666666666408, 0.4958333333333333481, 0.5000000000000000000, 0.5041666666666666519, 0.5083333333333333037, 0.5124999999999999556, 0.5166666666666667185, 0.5208333333333333703, 0.5250000000000000222, 0.5291666666666666741, 0.5333333333333333259, 0.5374999999999999778, 0.5416666666666666297, 0.5458333333333332815, 0.5500000000000000444, 0.5541666666666666963, 0.5583333333333333481, 0.5625000000000000000, 0.5666666666666666519, 0.5708333333333333037, 0.5749999999999999556, 0.5791666666666667185, 0.5833333333333333703, 0.5875000000000000222, 0.5916666666666666741, 0.5958333333333333259, 0.5999999999999999778, 0.6041666666666666297, 0.6083333333333332815, 0.6125000000000000444, 0.6166666666666666963, 0.6208333333333333481, 0.6250000000000000000, 0.6291666666666666519, 0.6333333333333333037, 0.6374999999999999556, 0.6416666666666667185, 0.6458333333333333703, 0.6500000000000000222, 0.6541666666666666741, 0.6583333333333333259, 0.6624999999999999778, 0.6666666666666666297, 0.6708333333333332815, 0.6750000000000000444, 0.6791666666666666963, 0.6833333333333333481, 0.6875000000000000000, 0.6916666666666666519, 0.6958333333333333037, 0.6999999999999999556, 0.7041666666666667185, 0.7083333333333333703, 0.7125000000000000222, 0.7166666666666666741, 0.7208333333333333259, 0.7249999999999999778, 0.7291666666666666297, 0.7333333333333332815, 0.7375000000000000444, 0.7416666666666666963, 0.7458333333333333481, 0.7500000000000000000, 0.7541666666666666519, 0.7583333333333333037, 0.7624999999999999556, 0.7666666666666667185, 0.7708333333333333703, 0.7750000000000000222, 0.7791666666666666741, 0.7833333333333333259, 0.7874999999999999778, 0.7916666666666666297, 0.7958333333333332815, 0.8000000000000000444, 0.8041666666666666963, 0.8083333333333333481, 0.8125000000000000000, 0.8166666666666666519, 0.8208333333333333037, 0.8249999999999999556, 0.8291666666666667185, 0.8333333333333333703, 0.8375000000000000222, 0.8416666666666666741, 0.8458333333333333259, 0.8499999999999999778, 0.8541666666666666297, 0.8583333333333332815, 0.8625000000000000444, 0.8666666666666666963, 0.8708333333333333481, 0.8750000000000000000, 0.8791666666666666519, 0.8833333333333333037, 0.8874999999999999556, 0.8916666666666667185, 0.8958333333333333703, 0.9000000000000000222, 0.9041666666666666741, 0.9083333333333333259, 0.9124999999999999778, 0.9166666666666666297, 0.9208333333333332815, 0.9250000000000000444, 0.9291666666666666963, 0.9333333333333333481, 0.9375000000000000000, 0.9416666666666666519, 0.9458333333333333037, 0.9499999999999999556, 0.9541666666666667185, 0.9583333333333333703, 0.9625000000000000222, 0.9666666666666666741, 0.9708333333333333259, 0.9749999999999999778, 0.9791666666666666297, 0.9833333333333332815, 0.9875000000000000444, 0.9916666666666666963, 0.9958333333333333481, 1.000000000000000000 ),
 .UNSPECIFIED. ) 
 GEOMETRIC_REPRESENTATION_ITEM ( )  RATIONAL_B_SPLINE_SURFACE ( (
 ( 1.000000000000000000, 0.8660254037844387076, 1.000000000000000000, 0.8660254037844387076, 1.000000000000000000, 0.8660254037844387076, 1.000000000000000000, 0.8660254037844387076, 1.000000000000000000, 0.8660254037844387076, 1.000000000000000000, 0.8660254037844387076, 1.000000000000000000, 0.8660254037844387076, 1.000000000000000000, 0.8660254037844387076, 1.000000000000000000, 0.8660254037844387076, 1.000000000000000000, 0.8660254037844387076, 1.000000000000000000, 0.8660254037844387076, 1.000000000000000000, 0.8660254037844387076, 1.000000000000000000, 0.8660254037844387076, 1.000000000000000000, 0.8660254037844387076, 1.000000000000000000, 0.8660254037844387076, 1.000000000000000000, 0.8660254037844387076, 1.000000000000000000, 0.8660254037844387076, 1.000000000000000000, 0.8660254037844387076, 1.000000000000000000, 0.8660254037844387076, 1.000000000000000000, 0.8660254037844387076, 1.000000000000000000, 0.8660254037844387076, 1.000000000000000000, 0.8660254037844387076, 1.000000000000000000, 0.8660254037844387076, 1.000000000000000000, 0.8660254037844387076, 1.000000000000000000, 0.8660254037844387076, 1.000000000000000000, 0.8660254037844387076, 1.000000000000000000, 0.8660254037844387076, 1.000000000000000000, 0.8660254037844387076, 1.000000000000000000, 0.8660254037844387076, 1.000000000000000000, 0.8660254037844387076, 1.000000000000000000, 0.8660254037844387076, 1.000000000000000000, 0.8660254037844387076, 1.000000000000000000, 0.8660254037844387076, 1.000000000000000000, 0.8660254037844387076, 1.000000000000000000, 0.8660254037844387076, 1.000000000000000000, 0.8660254037844387076, 1.000000000000000000, 0.8660254037844387076, 1.000000000000000000, 0.8660254037844387076, 1.000000000000000000, 0.8660254037844387076, 1.000000000000000000, 0.8660254037844387076, 1.000000000000000000, 0.8660254037844387076, 1.000000000000000000, 0.8660254037844387076, 1.000000000000000000, 0.8660254037844387076, 1.000000000000000000, 0.8660254037844387076, 1.000000000000000000, 0.8660254037844387076, 1.000000000000000000, 0.8660254037844387076, 1.000000000000000000, 0.8660254037844387076, 1.000000000000000000, 0.8660254037844387076, 1.000000000000000000, 0.8660254037844387076, 1.000000000000000000, 0.8660254037844387076, 1.000000000000000000, 0.8660254037844387076, 1.000000000000000000, 0.8660254037844387076, 1.000000000000000000, 0.8660254037844387076, 1.000000000000000000, 0.8660254037844387076, 1.000000000000000000, 0.8660254037844387076, 1.000000000000000000, 0.8660254037844387076, 1.000000000000000000, 0.8660254037844387076, 1.000000000000000000, 0.8660254037844387076, 1.000000000000000000, 0.8660254037844387076, 1.000000000000000000, 0.8660254037844387076, 1.000000000000000000, 0.8660254037844387076, 1.000000000000000000, 0.8660254037844387076, 1.000000000000000000, 0.8660254037844387076, 1.000000000000000000, 0.8660254037844387076, 1.000000000000000000, 0.8660254037844387076, 1.000000000000000000, 0.8660254037844387076, 1.000000000000000000, 0.8660254037844387076, 1.000000000000000000, 0.8660254037844387076, 1.000000000000000000, 0.8660254037844387076, 1.000000000000000000, 0.8660254037844387076, 1.000000000000000000, 0.8660254037844387076, 1.000000000000000000, 0.8660254037844387076, 1.000000000000000000, 0.8660254037844387076, 1.000000000000000000, 0.8660254037844387076, 1.000000000000000000, 0.8660254037844387076, 1.000000000000000000, 0.8660254037844387076, 1.000000000000000000, 0.8660254037844387076, 1.000000000000000000, 0.8660254037844387076, 1.000000000000000000, 0.8660254037844387076, 1.000000000000000000, 0.8660254037844387076, 1.000000000000000000, 0.8660254037844387076, 1.000000000000000000, 0.8660254037844387076, 1.000000000000000000, 0.8660254037844387076, 1.000000000000000000, 0.8660254037844387076, 1.000000000000000000, 0.8660254037844387076, 1.000000000000000000, 0.8660254037844387076, 1.000000000000000000, 0.8660254037844387076, 1.000000000000000000, 0.8660254037844387076, 1.000000000000000000, 0.8660254037844387076, 1.000000000000000000, 0.8660254037844387076, 1.000000000000000000, 0.8660254037844387076, 1.000000000000000000, 0.8660254037844387076, 1.000000000000000000, 0.8660254037844387076, 1.000000000000000000, 0.8660254037844387076, 1.000000000000000000, 0.8660254037844387076, 1.000000000000000000, 0.8660254037844387076, 1.000000000000000000, 0.8660254037844387076, 1.000000000000000000, 0.8660254037844387076, 1.000000000000000000, 0.8660254037844387076, 1.000000000000000000, 0.8660254037844387076, 1.000000000000000000, 0.8660254037844387076, 1.000000000000000000, 0.8660254037844387076, 1.000000000000000000, 0.8660254037844387076, 1.000000000000000000, 0.8660254037844387076, 1.000000000000000000, 0.8660254037844387076, 1.000000000000000000, 0.8660254037844387076, 1.000000000000000000, 0.8660254037844387076, 1.000000000000000000, 0.8660254037844387076, 1.000000000000000000, 0.8660254037844387076, 1.000000000000000000, 0.8660254037844387076, 1.000000000000000000, 0.8660254037844387076, 1.000000000000000000, 0.8660254037844387076, 1.000000000000000000, 0.8660254037844387076, 1.000000000000000000, 0.8660254037844387076, 1.000000000000000000, 0.8660254037844387076, 1.000000000000000000, 0.8660254037844387076, 1.000000000000000000, 0.8660254037844387076, 1.000000000000000000, 0.8660254037844387076, 1.000000000000000000, 0.8660254037844387076, 1.000000000000000000, 0.8660254037844387076, 1.000000000000000000, 0.8660254037844387076, 1.000000000000000000, 0.8660254037844387076, 1.000000000000000000, 0.8660254037844387076, 1.000000000000000000, 0.8660254037844387076, 1.000000000000000000, 0.8660254037844387076, 1.000000000000000000, 0.8660254037844387076, 1.000000000000000000, 0.8660254037844387076, 1.000000000000000000, 0.8660254037844387076, 1.000000000000000000, 0.8660254037844387076, 1.000000000000000000, 0.8660254037844387076, 1.000000000000000000, 0.8660254037844387076, 1.000000000000000000, 0.8660254037844387076, 1.000000000000000000, 0.8660254037844387076, 1.000000000000000000, 0.8660254037844387076, 1.000000000000000000, 0.8660254037844387076, 1.000000000000000000, 0.8660254037844387076, 1.000000000000000000, 0.8660254037844387076, 1.000000000000000000, 0.8660254037844387076, 1.000000000000000000, 0.8660254037844387076, 1.000000000000000000, 0.8660254037844387076, 1.000000000000000000, 0.8660254037844387076, 1.000000000000000000, 0.8660254037844387076, 1.000000000000000000, 0.8660254037844387076, 1.000000000000000000, 0.8660254037844387076, 1.000000000000000000, 0.8660254037844387076, 1.000000000000000000, 0.8660254037844387076, 1.000000000000000000, 0.8660254037844387076, 1.000000000000000000, 0.8660254037844387076, 1.000000000000000000, 0.8660254037844387076, 1.000000000000000000, 0.8660254037844387076, 1.000000000000000000, 0.8660254037844387076, 1.000000000000000000, 0.8660254037844387076, 1.000000000000000000, 0.8660254037844387076, 1.000000000000000000, 0.8660254037844387076, 1.000000000000000000, 0.8660254037844387076, 1.000000000000000000, 0.8660254037844387076, 1.000000000000000000, 0.8660254037844387076, 1.000000000000000000, 0.8660254037844387076, 1.000000000000000000, 0.8660254037844387076, 1.000000000000000000, 0.8660254037844387076, 1.000000000000000000, 0.8660254037844387076, 1.000000000000000000, 0.8660254037844387076, 1.000000000000000000, 0.8660254037844387076, 1.000000000000000000, 0.8660254037844387076, 1.000000000000000000, 0.8660254037844387076, 1.000000000000000000, 0.8660254037844387076, 1.000000000000000000, 0.8660254037844387076, 1.000000000000000000, 0.8660254037844387076, 1.000000000000000000, 0.8660254037844387076, 1.000000000000000000, 0.8660254037844387076, 1.000000000000000000, 0.8660254037844387076, 1.000000000000000000, 0.8660254037844387076, 1.000000000000000000, 0.8660254037844387076, 1.000000000000000000, 0.8660254037844387076, 1.000000000000000000, 0.8660254037844387076, 1.000000000000000000, 0.8660254037844387076, 1.000000000000000000, 0.8660254037844387076, 1.000000000000000000, 0.8660254037844387076, 1.000000000000000000, 0.8660254037844387076, 1.000000000000000000, 0.8660254037844387076, 1.000000000000000000, 0.8660254037844387076, 1.000000000000000000, 0.8660254037844387076, 1.000000000000000000, 0.8660254037844387076, 1.000000000000000000, 0.8660254037844387076, 1.000000000000000000, 0.8660254037844387076, 1.000000000000000000, 0.8660254037844387076, 1.000000000000000000, 0.8660254037844387076, 1.000000000000000000, 0.8660254037844387076, 1.000000000000000000, 0.8660254037844387076, 1.000000000000000000, 0.8660254037844387076, 1.000000000000000000, 0.8660254037844387076, 1.000000000000000000, 0.8660254037844387076, 1.000000000000000000, 0.8660254037844387076, 1.000000000000000000, 0.8660254037844387076, 1.000000000000000000, 0.8660254037844387076, 1.000000000000000000, 0.8660254037844387076, 1.000000000000000000, 0.8660254037844387076, 1.000000000000000000, 0.8660254037844387076, 1.000000000000000000, 0.8660254037844387076, 1.000000000000000000, 0.8660254037844387076, 1.000000000000000000, 0.8660254037844387076, 1.000000000000000000, 0.8660254037844387076, 1.000000000000000000, 0.8660254037844387076, 1.000000000000000000, 0.8660254037844387076, 1.000000000000000000, 0.8660254037844387076, 1.000000000000000000, 0.8660254037844387076, 1.000000000000000000, 0.8660254037844387076, 1.000000000000000000, 0.8660254037844387076, 1.000000000000000000, 0.8660254037844387076, 1.000000000000000000, 0.8660254037844387076, 1.000000000000000000, 0.8660254037844387076, 1.000000000000000000, 0.8660254037844387076, 1.000000000000000000, 0.8660254037844387076, 1.000000000000000000, 0.8660254037844387076, 1.000000000000000000, 0.8660254037844387076, 1.000000000000000000, 0.8660254037844387076, 1.000000000000000000, 0.8660254037844387076, 1.000000000000000000, 0.8660254037844387076, 1.000000000000000000, 0.8660254037844387076, 1.000000000000000000, 0.8660254037844387076, 1.000000000000000000, 0.8660254037844387076, 1.000000000000000000, 0.8660254037844387076, 1.000000000000000000, 0.8660254037844387076, 1.000000000000000000, 0.8660254037844387076, 1.000000000000000000, 0.8660254037844387076, 1.000000000000000000, 0.8660254037844387076, 1.000000000000000000, 0.8660254037844387076, 1.000000000000000000, 0.8660254037844387076, 1.000000000000000000, 0.8660254037844387076, 1.000000000000000000, 0.8660254037844387076, 1.000000000000000000, 0.8660254037844387076, 1.000000000000000000, 0.8660254037844387076, 1.000000000000000000, 0.8660254037844387076, 1.000000000000000000, 0.8660254037844387076, 1.000000000000000000, 0.8660254037844387076, 1.000000000000000000, 0.8660254037844387076, 1.000000000000000000, 0.8660254037844387076, 1.000000000000000000, 0.8660254037844387076, 1.000000000000000000, 0.8660254037844387076, 1.000000000000000000, 0.8660254037844387076, 1.000000000000000000),
 ( 1.000000000000000000, 0.8660254037844387076, 1.000000000000000000, 0.8660254037844387076, 1.000000000000000000, 0.8660254037844387076, 1.000000000000000000, 0.8660254037844387076, 1.000000000000000000, 0.8660254037844387076, 1.000000000000000000, 0.8660254037844387076, 1.000000000000000000, 0.8660254037844387076, 1.000000000000000000, 0.8660254037844387076, 1.000000000000000000, 0.8660254037844387076, 1.000000000000000000, 0.8660254037844387076, 1.000000000000000000, 0.8660254037844387076, 1.000000000000000000, 0.8660254037844387076, 1.000000000000000000, 0.8660254037844387076, 1.000000000000000000, 0.8660254037844387076, 1.000000000000000000, 0.8660254037844387076, 1.000000000000000000, 0.8660254037844387076, 1.000000000000000000, 0.8660254037844387076, 1.000000000000000000, 0.8660254037844387076, 1.000000000000000000, 0.8660254037844387076, 1.000000000000000000, 0.8660254037844387076, 1.000000000000000000, 0.8660254037844387076, 1.000000000000000000, 0.8660254037844387076, 1.000000000000000000, 0.8660254037844387076, 1.000000000000000000, 0.8660254037844387076, 1.000000000000000000, 0.8660254037844387076, 1.000000000000000000, 0.8660254037844387076, 1.000000000000000000, 0.8660254037844387076, 1.000000000000000000, 0.8660254037844387076, 1.000000000000000000, 0.8660254037844387076, 1.000000000000000000, 0.8660254037844387076, 1.000000000000000000, 0.8660254037844387076, 1.000000000000000000, 0.8660254037844387076, 1.000000000000000000, 0.8660254037844387076, 1.000000000000000000, 0.8660254037844387076, 1.000000000000000000, 0.8660254037844387076, 1.000000000000000000, 0.8660254037844387076, 1.000000000000000000, 0.8660254037844387076, 1.000000000000000000, 0.8660254037844387076, 1.000000000000000000, 0.8660254037844387076, 1.000000000000000000, 0.8660254037844387076, 1.000000000000000000, 0.8660254037844387076, 1.000000000000000000, 0.8660254037844387076, 1.000000000000000000, 0.8660254037844387076, 1.000000000000000000, 0.8660254037844387076, 1.000000000000000000, 0.8660254037844387076, 1.000000000000000000, 0.8660254037844387076, 1.000000000000000000, 0.8660254037844387076, 1.000000000000000000, 0.8660254037844387076, 1.000000000000000000, 0.8660254037844387076, 1.000000000000000000, 0.8660254037844387076, 1.000000000000000000, 0.8660254037844387076, 1.000000000000000000, 0.8660254037844387076, 1.000000000000000000, 0.8660254037844387076, 1.000000000000000000, 0.8660254037844387076, 1.000000000000000000, 0.8660254037844387076, 1.000000000000000000, 0.8660254037844387076, 1.000000000000000000, 0.8660254037844387076, 1.000000000000000000, 0.8660254037844387076, 1.000000000000000000, 0.8660254037844387076, 1.000000000000000000, 0.8660254037844387076, 1.000000000000000000, 0.8660254037844387076, 1.000000000000000000, 0.8660254037844387076, 1.000000000000000000, 0.8660254037844387076, 1.000000000000000000, 0.8660254037844387076, 1.000000000000000000, 0.8660254037844387076, 1.000000000000000000, 0.8660254037844387076, 1.000000000000000000, 0.8660254037844387076, 1.000000000000000000, 0.8660254037844387076, 1.000000000000000000, 0.8660254037844387076, 1.000000000000000000, 0.8660254037844387076, 1.000000000000000000, 0.8660254037844387076, 1.000000000000000000, 0.8660254037844387076, 1.000000000000000000, 0.8660254037844387076, 1.000000000000000000, 0.8660254037844387076, 1.000000000000000000, 0.8660254037844387076, 1.000000000000000000, 0.8660254037844387076, 1.000000000000000000, 0.8660254037844387076, 1.000000000000000000, 0.8660254037844387076, 1.000000000000000000, 0.8660254037844387076, 1.000000000000000000, 0.8660254037844387076, 1.000000000000000000, 0.8660254037844387076, 1.000000000000000000, 0.8660254037844387076, 1.000000000000000000, 0.8660254037844387076, 1.000000000000000000, 0.8660254037844387076, 1.000000000000000000, 0.8660254037844387076, 1.000000000000000000, 0.8660254037844387076, 1.000000000000000000, 0.8660254037844387076, 1.000000000000000000, 0.8660254037844387076, 1.000000000000000000, 0.8660254037844387076, 1.000000000000000000, 0.8660254037844387076, 1.000000000000000000, 0.8660254037844387076, 1.000000000000000000, 0.8660254037844387076, 1.000000000000000000, 0.8660254037844387076, 1.000000000000000000, 0.8660254037844387076, 1.000000000000000000, 0.8660254037844387076, 1.000000000000000000, 0.8660254037844387076, 1.000000000000000000, 0.8660254037844387076, 1.000000000000000000, 0.8660254037844387076, 1.000000000000000000, 0.8660254037844387076, 1.000000000000000000, 0.8660254037844387076, 1.000000000000000000, 0.8660254037844387076, 1.000000000000000000, 0.8660254037844387076, 1.000000000000000000, 0.8660254037844387076, 1.000000000000000000, 0.8660254037844387076, 1.000000000000000000, 0.8660254037844387076, 1.000000000000000000, 0.8660254037844387076, 1.000000000000000000, 0.8660254037844387076, 1.000000000000000000, 0.8660254037844387076, 1.000000000000000000, 0.8660254037844387076, 1.000000000000000000, 0.8660254037844387076, 1.000000000000000000, 0.8660254037844387076, 1.000000000000000000, 0.8660254037844387076, 1.000000000000000000, 0.8660254037844387076, 1.000000000000000000, 0.8660254037844387076, 1.000000000000000000, 0.8660254037844387076, 1.000000000000000000, 0.8660254037844387076, 1.000000000000000000, 0.8660254037844387076, 1.000000000000000000, 0.8660254037844387076, 1.000000000000000000, 0.8660254037844387076, 1.000000000000000000, 0.8660254037844387076, 1.000000000000000000, 0.8660254037844387076, 1.000000000000000000, 0.8660254037844387076, 1.000000000000000000, 0.8660254037844387076, 1.000000000000000000, 0.8660254037844387076, 1.000000000000000000, 0.8660254037844387076, 1.000000000000000000, 0.8660254037844387076, 1.000000000000000000, 0.8660254037844387076, 1.000000000000000000, 0.8660254037844387076, 1.000000000000000000, 0.8660254037844387076, 1.000000000000000000, 0.8660254037844387076, 1.000000000000000000, 0.8660254037844387076, 1.000000000000000000, 0.8660254037844387076, 1.000000000000000000, 0.8660254037844387076, 1.000000000000000000, 0.8660254037844387076, 1.000000000000000000, 0.8660254037844387076, 1.000000000000000000, 0.8660254037844387076, 1.000000000000000000, 0.8660254037844387076, 1.000000000000000000, 0.8660254037844387076, 1.000000000000000000, 0.8660254037844387076, 1.000000000000000000, 0.8660254037844387076, 1.000000000000000000, 0.8660254037844387076, 1.000000000000000000, 0.8660254037844387076, 1.000000000000000000, 0.8660254037844387076, 1.000000000000000000, 0.8660254037844387076, 1.000000000000000000, 0.8660254037844387076, 1.000000000000000000, 0.8660254037844387076, 1.000000000000000000, 0.8660254037844387076, 1.000000000000000000, 0.8660254037844387076, 1.000000000000000000, 0.8660254037844387076, 1.000000000000000000, 0.8660254037844387076, 1.000000000000000000, 0.8660254037844387076, 1.000000000000000000, 0.8660254037844387076, 1.000000000000000000, 0.8660254037844387076, 1.000000000000000000, 0.8660254037844387076, 1.000000000000000000, 0.8660254037844387076, 1.000000000000000000, 0.8660254037844387076, 1.000000000000000000, 0.8660254037844387076, 1.000000000000000000, 0.8660254037844387076, 1.000000000000000000, 0.8660254037844387076, 1.000000000000000000, 0.8660254037844387076, 1.000000000000000000, 0.8660254037844387076, 1.000000000000000000, 0.8660254037844387076, 1.000000000000000000, 0.8660254037844387076, 1.000000000000000000, 0.8660254037844387076, 1.000000000000000000, 0.8660254037844387076, 1.000000000000000000, 0.8660254037844387076, 1.000000000000000000, 0.8660254037844387076, 1.000000000000000000, 0.8660254037844387076, 1.000000000000000000, 0.8660254037844387076, 1.000000000000000000, 0.8660254037844387076, 1.000000000000000000, 0.8660254037844387076, 1.000000000000000000, 0.8660254037844387076, 1.000000000000000000, 0.8660254037844387076, 1.000000000000000000, 0.8660254037844387076, 1.000000000000000000, 0.8660254037844387076, 1.000000000000000000, 0.8660254037844387076, 1.000000000000000000, 0.8660254037844387076, 1.000000000000000000, 0.8660254037844387076, 1.000000000000000000, 0.8660254037844387076, 1.000000000000000000, 0.8660254037844387076, 1.000000000000000000, 0.8660254037844387076, 1.000000000000000000, 0.8660254037844387076, 1.000000000000000000, 0.8660254037844387076, 1.000000000000000000, 0.8660254037844387076, 1.000000000000000000, 0.8660254037844387076, 1.000000000000000000, 0.8660254037844387076, 1.000000000000000000, 0.8660254037844387076, 1.000000000000000000, 0.8660254037844387076, 1.000000000000000000, 0.8660254037844387076, 1.000000000000000000, 0.8660254037844387076, 1.000000000000000000, 0.8660254037844387076, 1.000000000000000000, 0.8660254037844387076, 1.000000000000000000, 0.8660254037844387076, 1.000000000000000000, 0.8660254037844387076, 1.000000000000000000, 0.8660254037844387076, 1.000000000000000000, 0.8660254037844387076, 1.000000000000000000, 0.8660254037844387076, 1.000000000000000000, 0.8660254037844387076, 1.000000000000000000, 0.8660254037844387076, 1.000000000000000000, 0.8660254037844387076, 1.000000000000000000, 0.8660254037844387076, 1.000000000000000000, 0.8660254037844387076, 1.000000000000000000, 0.8660254037844387076, 1.000000000000000000, 0.8660254037844387076, 1.000000000000000000, 0.8660254037844387076, 1.000000000000000000, 0.8660254037844387076, 1.000000000000000000, 0.8660254037844387076, 1.000000000000000000, 0.8660254037844387076, 1.000000000000000000, 0.8660254037844387076, 1.000000000000000000, 0.8660254037844387076, 1.000000000000000000, 0.8660254037844387076, 1.000000000000000000, 0.8660254037844387076, 1.000000000000000000, 0.8660254037844387076, 1.000000000000000000, 0.8660254037844387076, 1.000000000000000000, 0.8660254037844387076, 1.000000000000000000, 0.8660254037844387076, 1.000000000000000000, 0.8660254037844387076, 1.000000000000000000, 0.8660254037844387076, 1.000000000000000000, 0.8660254037844387076, 1.000000000000000000, 0.8660254037844387076, 1.000000000000000000, 0.8660254037844387076, 1.000000000000000000, 0.8660254037844387076, 1.000000000000000000, 0.8660254037844387076, 1.000000000000000000, 0.8660254037844387076, 1.000000000000000000, 0.8660254037844387076, 1.000000000000000000, 0.8660254037844387076, 1.000000000000000000, 0.8660254037844387076, 1.000000000000000000, 0.8660254037844387076, 1.000000000000000000, 0.8660254037844387076, 1.000000000000000000, 0.8660254037844387076, 1.000000000000000000, 0.8660254037844387076, 1.000000000000000000, 0.8660254037844387076, 1.000000000000000000, 0.8660254037844387076, 1.000000000000000000, 0.8660254037844387076, 1.000000000000000000, 0.8660254037844387076, 1.000000000000000000, 0.8660254037844387076, 1.000000000000000000, 0.8660254037844387076, 1.000000000000000000, 0.8660254037844387076, 1.000000000000000000, 0.8660254037844387076, 1.000000000000000000, 0.8660254037844387076, 1.000000000000000000) ) ) 
 REPRESENTATION_ITEM ( '' )  SURFACE ( )  );
#117620 = COLOUR_RGB ( '', 0.31764706, 0.68627451, 0.89019608) ;
#117621 = CARTESIAN_POINT ( 'NONE',  ( 6.725048307591657171, -1.982231927674932948, -0.8863045971672071088 ) ) ;
#117622 = FACE_OUTER_BOUND ( 'NONE', #40670, .T. ) ;
#117623 = CARTESIAN_POINT ( 'NONE',  ( 2.255205753237074617, 0.09875464746901543855, -2.115135400419057010 ) ) ;
#117624 = CARTESIAN_POINT ( 'NONE',  ( 6.620655732516651071, 4.689394895873098434, 2.736297475404291024 ) ) ;
#117625 = CARTESIAN_POINT ( 'NONE',  ( 5.086904980214876915, -0.2357887182157791250, -1.911833357141810241 ) ) ;
#117626 = EDGE_LOOP ( 'NONE', ( #49707, #125959, #57173, #121424 ) ) ;
#117628 = CARTESIAN_POINT ( 'NONE',  ( -1.201851678989727383E-14, 5.837500000000023448, -1.732050807568863648 ) ) ;
#117627 = CARTESIAN_POINT ( 'NONE',  ( 2.226505721922732661, 2.224568380592424344, 0.5530147644091478742 ) ) ;
#117629 = CARTESIAN_POINT ( 'NONE',  ( 2.849184837166184536, 6.475799410002530898, 0.7998128361456362523 ) ) ;
#117630 = CARTESIAN_POINT ( 'NONE',  ( 5.250031796989762967, 7.148123067953287446, 1.599625672291267398 ) ) ;
#117631 = CARTESIAN_POINT ( 'NONE',  ( 4.319114520555938697, 1.717138752081597719, -1.409087234901666763 ) ) ;
#117632 = CARTESIAN_POINT ( 'NONE',  ( -7.592202833972775622, 8.920286730132099606, 1.082531754730558626 ) ) ;
#117633 = FACE_OUTER_BOUND ( 'NONE', #75300, .T. ) ;
#117634 = CARTESIAN_POINT ( 'NONE',  ( 5.829642864196168617, 6.863966765392747860, 1.082531754730558626 ) ) ;
#117635 = CARTESIAN_POINT ( 'NONE',  ( -7.009202228140739344, 11.12122699956546334, -0.7216878364870267237 ) ) ;
#117636 = CARTESIAN_POINT ( 'NONE',  ( 5.017926250833595780, 7.907978821730911712, -1.082531754730548412 ) ) ;
#117637 = ORIENTED_EDGE ( 'NONE', *, *, #111400, .T. ) ;
#117638 = CARTESIAN_POINT ( 'NONE',  ( 3.111954093273407107, 0.05229746705895028935, 2.015912966248374349 ) ) ;
#117640 = CARTESIAN_POINT ( 'NONE',  ( 0.7782751772977951621, -1.100228457372550261, -1.744432094316533677 ) ) ;
#117639 = CARTESIAN_POINT ( 'NONE',  ( 7.962716289927667113, 8.184257181204083409, -0.7998128361456291469 ) ) ;
#117641 = DIRECTION ( 'NONE',  ( 0.000000000000000000, 1.000000000000000000, 0.000000000000000000 ) ) ;
#117642 = CARTESIAN_POINT ( 'NONE',  ( 6.685579144870162693, 6.972466221869550118, -0.7216878364870458196 ) ) ;
#117643 = DIRECTION ( 'NONE',  ( 0.000000000000000000, -1.000000000000000000, -0.000000000000000000 ) ) ;
#117644 = CARTESIAN_POINT ( 'NONE',  ( -1.364683531250012516, 4.238541667008090208, -0.7879004041258300672 ) ) ;
#117645 = CARTESIAN_POINT ( 'NONE',  ( 4.224703044441734612, 0.1064595904514322594, 2.188988589495489911 ) ) ;
#117646 = CARTESIAN_POINT ( 'NONE',  ( 0.8971115437808926396, -0.9091470795906559932, -1.799921601489597123 ) ) ;
#117647 = CARTESIAN_POINT ( 'NONE',  ( 1.153568636672014369, 0.7464410156945017194, 1.683350060182234209 ) ) ;
#117648 = CARTESIAN_POINT ( 'NONE',  ( 4.862941710081361002, 0.2263591102839345448, -2.281146386033555462 ) ) ;
#117649 = CARTESIAN_POINT ( 'NONE',  ( 3.046634964419430158, -1.505538468004435027, -1.059505732788845966 ) ) ;
#117650 = ADVANCED_FACE ( 'NONE', ( #180137, #71684 ), #102079, .F. ) ;
#117651 = CARTESIAN_POINT ( 'NONE',  ( 7.262363838414439776, 11.62450824479221900, 0.7998128361456462443 ) ) ;
#117652 = FILL_AREA_STYLE_COLOUR ( '', #117620 ) ;
#117653 = CARTESIAN_POINT ( 'NONE',  ( 4.067279105520240634, 0.2236234833344897255, -1.811772463268163547 ) ) ;
#117654 = CARTESIAN_POINT ( 'NONE',  ( 5.221327349844218091, 1.987046161919112430, 0.3419379449052239450 ) ) ;
#117655 = CARTESIAN_POINT ( 'NONE',  ( -7.828943636887387925, 11.22118577875556156, 1.199719254218453823 ) ) ;
#117657 = CARTESIAN_POINT ( 'NONE',  ( 3.469446951953614189E-15, 5.290451655907108197, 1.214306433183764966E-14 ) ) ;
#117656 = CARTESIAN_POINT ( 'NONE',  ( 5.032209928657234599, 1.167594373104458461, -1.937845176762391874 ) ) ;
#117658 = CARTESIAN_POINT ( 'NONE',  ( 6.668975466350578252, -1.923848446808050783, -0.8571054451525415008 ) ) ;
#117659 = CARTESIAN_POINT ( 'NONE',  ( -1.898855744251342514, 3.739179606816304346, -0.4000000000000286104 ) ) ;
#117660 = CARTESIAN_POINT ( 'NONE',  ( 4.176279081494421952, -1.061646348645030713, -1.777293304589353085 ) ) ;
#117661 = CARTESIAN_POINT ( 'NONE',  ( 10.56588178375152864, 11.22128359066528169, -0.7998128361456281477 ) ) ;
#117662 = CARTESIAN_POINT ( 'NONE',  ( -1.360316468750006669, 2.442708333674733723, 0.7853790794158861388 ) ) ;
#117663 = PRODUCT_CONTEXT ( 'NONE', #122578, 'mechanical' ) ;
#117665 = CARTESIAN_POINT ( 'NONE',  ( 2.104012753913253153, -1.926084867047285654, 0.04718631861246740111 ) ) ;
#117664 = CARTESIAN_POINT ( 'NONE',  ( -9.528683032306089373, 10.01121838064558744, 0.7998128361456462443 ) ) ;
#117666 = CARTESIAN_POINT ( 'NONE',  ( -3.492107083971660586, 6.231819477012331632, 1.199719254218452935 ) ) ;
#117667 = CARTESIAN_POINT ( 'NONE',  ( 6.877801621836153068, -1.911143888484008846, 0.4753377615324301253 ) ) ;
#117668 = CARTESIAN_POINT ( 'NONE',  ( 5.533136087708556694, 5.627949321847663278, 0.000000000000000000 ) ) ;
#117669 = CARTESIAN_POINT ( 'NONE',  ( 5.726377019126981160, 6.078880280049443918, 0.6665230057388837892 ) ) ;
#117670 = CARTESIAN_POINT ( 'NONE',  ( -4.600294193738529103, 4.261431402316699035, -0.7998128361456221525 ) ) ;
#117672 = CARTESIAN_POINT ( 'NONE',  ( 1.969254952099579459, -1.713688747078499830, 1.413451004025434665 ) ) ;
#117671 = CARTESIAN_POINT ( 'NONE',  ( 1.301209403646291118, -0.3165094942152619772, -2.096747597609450953 ) ) ;
#117673 = CARTESIAN_POINT ( 'NONE',  ( 3.346800460960248191, 0.5101267414385314281, 2.043117269239830947 ) ) ;
#117675 = AXIS2_PLACEMENT_3D ( 'NONE', #52692, #104662, #182683 ) ;
#117674 = CARTESIAN_POINT ( 'NONE',  ( -7.045397100956844127, 8.248660034984974132, -1.199719254218452047 ) ) ;
#117676 = CARTESIAN_POINT ( 'NONE',  ( 6.479907352327590964, 9.647310113435821677, 1.199719254218462483 ) ) ;
#117677 = CARTESIAN_POINT ( 'NONE',  ( 0.7482324461028444507, -1.846328264857381996, -0.2332022352751206007 ) ) ;
#117678 = CARTESIAN_POINT ( 'NONE',  ( 5.774883364416965037, 8.824782127540085952, -1.199719254218440723 ) ) ;
#117679 = CARTESIAN_POINT ( 'NONE',  ( -4.295541959788370612, 7.266047401097770475, -0.9601269197386901322 ) ) ;
#117680 = EDGE_CURVE ( 'NONE', #40498, #29327, #5602, .T. ) ;
#117681 = CARTESIAN_POINT ( 'NONE',  ( 4.847203612085560387, 5.613824621309978724, -1.199719254218452047 ) ) ;
#117682 = CARTESIAN_POINT ( 'NONE',  ( -5.397554552016258889, 7.390509292142662723, 1.443375672974058777 ) ) ;
#117683 = CARTESIAN_POINT ( 'NONE',  ( -6.710922849084449915, 10.77323439066645783, 0.000000000000000000 ) ) ;
#117684 = CARTESIAN_POINT ( 'NONE',  ( 1.107859837811319581, 1.609452232531217275, 1.380942675281403353 ) ) ;
#117685 = CARTESIAN_POINT ( 'NONE',  ( -7.273023059088104425, 7.449891421883056530, 0.000000000000000000 ) ) ;
#117687 = CARTESIAN_POINT ( 'NONE',  ( 4.334394203492665909, -1.131343785558375226, 1.602600411086833931 ) ) ;
#117686 = CARTESIAN_POINT ( 'NONE',  ( -4.156403723172807449E-14, 0.8124999999999957812, 1.414508159514549446 ) ) ;
#117688 = CARTESIAN_POINT ( 'NONE',  ( 3.239309987758617115, -1.907233169736745060, 1.017530501952010447 ) ) ;
#117689 = CARTESIAN_POINT ( 'NONE',  ( 2.225889136967126536, 1.786374552192676823, 0.4457033907802817052 ) ) ;
#117690 = CARTESIAN_POINT ( 'NONE',  ( -4.339127873110165901, 7.217636166161084610, -1.009937615098016606 ) ) ;
#117691 = CARTESIAN_POINT ( 'NONE',  ( 4.193801852926431373, 7.579907728022624802, -0.9040490846396221913 ) ) ;
#117692 = CARTESIAN_POINT ( 'NONE',  ( 4.136439897933008147, -1.512742658674090857, 0.8602829033797516622 ) ) ;
#117693 = CARTESIAN_POINT ( 'NONE',  ( -6.671583288098391407, 15.00000000000335731, -9.747470831326879193 ) ) ;
#117694 = CARTESIAN_POINT ( 'NONE',  ( 5.422898255786183341, 7.349800603215774331, -1.443375672974051449 ) ) ;
#117695 = CARTESIAN_POINT ( 'NONE',  ( -10.52284260640670688, 5.420240069097000735, -5.071998063130033430 ) ) ;
#117696 = CARTESIAN_POINT ( 'NONE',  ( 1.938557520917514987, 2.138169252768943984, 0.3173444169591658204 ) ) ;
#117697 = PRESENTATION_LAYER_ASSIGNMENT (  '', '', ( #124515 ) ) ;
#117698 = CARTESIAN_POINT ( 'NONE',  ( 3.057970071934034362, 1.730601471501746147, -1.034006501934421784 ) ) ;
#117699 = CARTESIAN_POINT ( 'NONE',  ( -10.10046125205658463, 11.84658821789661509, -1.082531754730537976 ) ) ;
#117700 = CARTESIAN_POINT ( 'NONE',  ( 0.8663662989462637132, 1.066309655776727539, 1.880320099339624296 ) ) ;
#117701 = CARTESIAN_POINT ( 'NONE',  ( 3.221511537501456690, -1.900432112322864464, 0.5242411554721800870 ) ) ;
#117702 = CARTESIAN_POINT ( 'NONE',  ( 6.609000000000047947, 2.072800852438889230, 2.208748404276588584 ) ) ;
#117703 = CARTESIAN_POINT ( 'NONE',  ( 2.929168808825276749, -1.306124965484034117, -1.437377093338227496 ) ) ;
#117706 = EDGE_CURVE ( 'NONE', #43490, #15455, #112265, .T. ) ;
#117705 = CARTESIAN_POINT ( 'NONE',  ( -4.177320726786328819, 5.966903162707725805, -1.443375672974066548 ) ) ;
#117704 = CARTESIAN_POINT ( 'NONE',  ( -9.937763408692596556, 11.65677406730528887, -1.082531754730537976 ) ) ;
#117707 = CARTESIAN_POINT ( 'NONE',  ( -4.299344108864961989, 6.109263775132799168, -1.443375672974066548 ) ) ;
#117708 = CARTESIAN_POINT ( 'NONE',  ( 5.110497557708379546, 4.926945003606695295, -0.7998128361456481317 ) ) ;
#117709 = CARTESIAN_POINT ( 'NONE',  ( -5.276058054373441664, 6.184431147304315424, -1.199719254218453823 ) ) ;
#117710 = CARTESIAN_POINT ( 'NONE',  ( -6.466312919074983512, 6.508729591867735031, -0.7998128361456362523 ) ) ;
#117711 = CARTESIAN_POINT ( 'NONE',  ( -8.798878505144648088, 12.24881344176869469, -1.082531754730543083 ) ) ;
#117712 = EDGE_CURVE ( 'NONE', #47720, #140937, #81112, .T. ) ;
#117713 = CARTESIAN_POINT ( 'NONE',  ( 0.2884678563945877738, -1.037960011796670523, 1.947446179978419512 ) ) ;
#117714 = CARTESIAN_POINT ( 'NONE',  ( -1.642778471875000035, -2.617708332855375186, -2.845375778867859751 ) ) ;
#117715 = CARTESIAN_POINT ( 'NONE',  ( 5.594571816639393624, 1.932094781187740917, 0.3390067100078468232 ) ) ;
#117716 = CARTESIAN_POINT ( 'NONE',  ( 1.899064777474347654, -0.9530127170578571727, -1.777010740487514173 ) ) ;
#117717 = ORIENTED_EDGE ( 'NONE', *, *, #37600, .F. ) ;
#117718 = CARTESIAN_POINT ( 'NONE',  ( 4.030539441936417333, 0.5683090829115284848, 2.039553408600587758 ) ) ;
#117719 = CARTESIAN_POINT ( 'NONE',  ( 0.7499999999999902300, 3.264583334016149418, 1.299038105676669330 ) ) ;
#117721 = CARTESIAN_POINT ( 'NONE',  ( -4.880045225915050189, 7.780804299287790826, 1.199719254218464037 ) ) ;
#117720 = CARTESIAN_POINT ( 'NONE',  ( 9.500370076773496208, -7.189371949516623950, -0.005973655271256667759 ) ) ;
#117722 = CARTESIAN_POINT ( 'NONE',  ( 3.011469152984513009, -0.9080073089506625061, -1.601583425259824001 ) ) ;
#117723 = EDGE_LOOP ( 'NONE', ( #161696, #33044, #20201, #157103 ) ) ;
#117724 = UNCERTAINTY_MEASURE_WITH_UNIT (LENGTH_MEASURE( 1.000000000000000082E-05 ), #20792, 'distance_accuracy_value', 'NONE');
#117725 = CARTESIAN_POINT ( 'NONE',  ( -7.309817376062285099, 11.67987070538135264, 0.000000000000000000 ) ) ;
#117726 = DIRECTION ( 'NONE',  ( 0.000000000000000000, 0.000000000000000000, 1.000000000000000000 ) ) ;
#117727 = CARTESIAN_POINT ( 'NONE',  ( 5.484674493353773883, -1.343714522216314489, 1.640574901390474460 ) ) ;
#117728 = CARTESIAN_POINT ( 'NONE',  ( -1.201851678989727383E-14, 4.368750000682820378, -1.732050807568863648 ) ) ;
#117729 = CARTESIAN_POINT ( 'NONE',  ( 7.070740804726770357, 8.207951346058097286, 1.199719254218462483 ) ) ;
#117730 = CARTESIAN_POINT ( 'NONE',  ( 5.026665581557772100, 1.970771621317930045, 0.6023086073758465719 ) ) ;
#117733 = CARTESIAN_POINT ( 'NONE',  ( 2.454439063956286304, -1.602943312447857593, -0.9057913635923324769 ) ) ;
#117732 = CARTESIAN_POINT ( 'NONE',  ( 0.6954782174160825114, -1.312119466559122927, -1.320074052667360665 ) ) ;
#117731 = DIRECTION ( 'NONE',  ( -0.9992060137953822085, -3.484297484817962848E-16, 0.03984146075563036599 ) ) ;
#117734 = CARTESIAN_POINT ( 'NONE',  ( 7.899597058256738968, 12.36794700127490820, 1.040834085586084257E-14 ) ) ;
#117735 = CARTESIAN_POINT ( 'NONE',  ( -8.093291352714894415, 8.406871097780989288, -0.7998128361456362523 ) ) ;
#117736 = CARTESIAN_POINT ( 'NONE',  ( -7.334597915313094241, 9.580116872663850813, 1.040834085586084257E-14 ) ) ;
#117737 = CARTESIAN_POINT ( 'NONE',  ( 2.104404934925046877, -2.206339196854599116, 0.05594281105186085790 ) ) ;
#117738 = CARTESIAN_POINT ( 'NONE',  ( 4.886124051547468206, -1.072500323723464932, 1.992072436074944219 ) ) ;
#117739 = CARTESIAN_POINT ( 'NONE',  ( -7.293923454472094114, 9.532663335016016148, 1.443375672974090751 ) ) ;
#117740 = CARTESIAN_POINT ( 'NONE',  ( 4.640750240102114788, 1.735609681454729492, 0.5192115853321179753 ) ) ;
#117741 = CARTESIAN_POINT ( 'NONE',  ( 4.821452977306352139, -1.359283356373307328, -1.350213215339219897 ) ) ;
#117742 = EDGE_CURVE ( 'NONE', #152353, #212749, #3748, .T. ) ;
#117743 = CARTESIAN_POINT ( 'NONE',  ( -1.364683531250010295, 5.801041667008088432, -0.7879004041258300672 ) ) ;
#117744 = TOROIDAL_SURFACE ( 'NONE', #3534, 11.92000000000000171, 0.08000000000000000167 ) ;
#117745 = CARTESIAN_POINT ( 'NONE',  ( 3.608241331778249350, -0.7978255515562487910, -1.802987302761626998 ) ) ;
#117746 = CARTESIAN_POINT ( 'NONE',  ( 5.137510444216992767, -1.323429205136433140, -1.322332877454430955 ) ) ;
#117747 = CARTESIAN_POINT ( 'NONE',  ( 4.404655029226283602, 0.4953248787317258706, 1.793866421858918869 ) ) ;
#117748 = CARTESIAN_POINT ( 'NONE',  ( 3.449547071718269020, 5.999999999999998224, 2.024999999999999023 ) ) ;
#117749 = ADVANCED_FACE ( 'NONE', ( #183322 ), #69547, .F. ) ;
#117750 = CARTESIAN_POINT ( 'NONE',  ( 0.4621254960020632074, -1.116205757145168231, 1.679226196708947239 ) ) ;
#117752 = CARTESIAN_POINT ( 'NONE',  ( 1.295691649255722888, 1.595764685746006384, 1.374534258749359861 ) ) ;
#117751 = CARTESIAN_POINT ( 'NONE',  ( -2.602802303699316866, 5.980427087717073320, 1.040834085586084257E-14 ) ) ;
#117753 = CARTESIAN_POINT ( 'NONE',  ( 9.154780037725547714, 11.70366268214508487, 1.599625672291279388 ) ) ;
#117755 = CARTESIAN_POINT ( 'NONE',  ( 0.07479286986305545837, 0.7422478802248284602, -1.939684878352589070 ) ) ;
#117754 = DIRECTION ( 'NONE',  ( -5.578564026256490882E-16, -1.000000000000000000, -9.066213480720158442E-32 ) ) ;
#117756 = CARTESIAN_POINT ( 'NONE',  ( 3.445663904809421307, -1.957918079443463855, 0.8150281543025169606 ) ) ;
#117757 = CARTESIAN_POINT ( 'NONE',  ( 2.998579151156815392, 6.400053006662376198, -0.4921665831622086817 ) ) ;
#117758 = CARTESIAN_POINT ( 'NONE',  ( 2.302995500392619022, -0.3493979467522835836, -1.989178256620740548 ) ) ;
#117759 = CARTESIAN_POINT ( 'NONE',  ( -0.6823417656250212460, 2.801041667008084879, 1.181850606188767472 ) ) ;
#117760 = CARTESIAN_POINT ( 'NONE',  ( 6.720655732516641834, 0.008434553976904584152, 1.726293928996263771 ) ) ;
#117761 = CARTESIAN_POINT ( 'NONE',  ( 5.020596955762157698, 4.751784624677624080, 1.040834085586084257E-14 ) ) ;
#117762 = ORIENTED_EDGE ( 'NONE', *, *, #142352, .F. ) ;
#117763 = CARTESIAN_POINT ( 'NONE',  ( 2.003414267471514965, 1.795956895356983551, 1.202623776965026536 ) ) ;
#117764 = CARTESIAN_POINT ( 'NONE',  ( 6.610000000000009202, 1.996100381701769289, 2.581056663040970811 ) ) ;
#117767 = FACE_OUTER_BOUND ( 'NONE', #180918, .T. ) ;
#117766 = CARTESIAN_POINT ( 'NONE',  ( 11.97178994924802353, 9.720000062027946086, -0.8322011300497146324 ) ) ;
#117765 = CARTESIAN_POINT ( 'NONE',  ( 4.947799714344386146, 4.737130853015369958, -0.7998128361456481317 ) ) ;
#117768 = CARTESIAN_POINT ( 'NONE',  ( -1.992711204631002198E-15, 2.999999999999989342, 1.224999999999989875 ) ) ;
#117769 = CARTESIAN_POINT ( 'NONE',  ( -7.712222144929068435, -6.293595771080859436, 7.712222144929100409 ) ) ;
#117770 = CARTESIAN_POINT ( 'NONE',  ( -8.378575743565381373, 8.877352577022161739, 0.7216878364870438212 ) ) ;
#117771 = CARTESIAN_POINT ( 'NONE',  ( 1.224469250947546328, 2.113408192816915943, 0.5798510048089372537 ) ) ;
#117772 = CARTESIAN_POINT ( 'NONE',  ( -9.860259297219579722, -8.821010173593817782, 0.6081441828345716116 ) ) ;
#117774 = CARTESIAN_POINT ( 'NONE',  ( 0.6823417656249934904, 11.69270833367473017, 1.181850606188764807 ) ) ;
#117773 = CARTESIAN_POINT ( 'NONE',  ( 1.235668275047563380, -2.044475609799735416, 0.9693208282701860634 ) ) ;
#117775 = CARTESIAN_POINT ( 'NONE',  ( -9.321394304595349567, 10.83371376257142416, 1.199719254218462483 ) ) ;
#117776 = CARTESIAN_POINT ( 'NONE',  ( -3.755245360860925086, 6.364574773437617239, -1.082531754730548412 ) ) ;
#117777 = CARTESIAN_POINT ( 'NONE',  ( 1.364683531249988757, 2.196875000341415252, 1.214306433183764966E-14 ) ) ;
#117778 = CARTESIAN_POINT ( 'NONE',  ( 4.666668778386947380, 8.284408874816399759, 0.5204741841226891985 ) ) ;
#117779 = CARTESIAN_POINT ( 'NONE',  ( -0.7500000000000179856, 9.291666666666669627, 1.299038105676658228 ) ) ;
#117780 = CARTESIAN_POINT ( 'NONE',  ( 4.512129967005336084, -0.7409026826630369378, -1.557792038885176700 ) ) ;
#117781 = CARTESIAN_POINT ( 'NONE',  ( 6.048345925472166762, 10.07050432311064903, 0.7216878364870317197 ) ) ;
#117782 = CARTESIAN_POINT ( 'NONE',  ( 2.618099050500310998, 1.159573672392331112, -1.336980558935680241 ) ) ;
#117783 = EDGE_CURVE ( 'NONE', #78316, #29472, #150395, .T. ) ;
#117784 = CARTESIAN_POINT ( 'NONE',  ( 8.224992744984721327, 12.74757530245756243, 1.040834085586084257E-14 ) ) ;
#117785 = CARTESIAN_POINT ( 'NONE',  ( 5.790102700048295858, -0.9971039342967463748, 1.968745932239771568 ) ) ;
#117786 = EDGE_LOOP ( 'NONE', ( #194070, #138965, #172234, #97081, #29257 ) ) ;
#117787 = CARTESIAN_POINT ( 'NONE',  ( 4.289322773248661846, -0.004189350761124934451, -2.019972750201783906 ) ) ;
#117788 = CARTESIAN_POINT ( 'NONE',  ( -6.622231685632140596, 6.690634819517756959, 0.000000000000000000 ) ) ;
#117789 = CARTESIAN_POINT ( 'NONE',  ( 5.237907724141787291, 2.013986247903374327, -0.1017665992488273330 ) ) ;
#117790 = VERTEX_POINT ( 'NONE', #105302 ) ;
#117791 = CARTESIAN_POINT ( 'NONE',  ( 2.166681600665042229, -1.709288833360942617, -0.7604731621856930524 ) ) ;
#117792 = LINE ( 'NONE', #63646, #127585 ) ;
#117793 = CARTESIAN_POINT ( 'NONE',  ( 1.687617486097678476, 1.829050272730630144, -0.5582976189952293389 ) ) ;
#117794 = CARTESIAN_POINT ( 'NONE',  ( -4.485769045089750939, 8.247486273217061736, 0.1636802980241918171 ) ) ;
#117795 = CARTESIAN_POINT ( 'NONE',  ( -10.48363756508902611, 5.078564944783316548, -7.119907325005036647 ) ) ;
#117796 = DIRECTION ( 'NONE',  ( -0.000000000000000000, 1.000000000000000000, -0.000000000000000000 ) ) ;
#117797 = CARTESIAN_POINT ( 'NONE',  ( 0.6823417656249899377, 4.238541667008085767, -1.181850606188754593 ) ) ;
#117798 = CARTESIAN_POINT ( 'NONE',  ( -0.05268457437105151381, -1.747710896673961400, 0.7768168958157273263 ) ) ;
#117799 = CARTESIAN_POINT ( 'NONE',  ( 5.804299160426222848, 7.865044668620976509, -1.443375672974078761 ) ) ;
#117800 = CARTESIAN_POINT ( 'NONE',  ( 2.224987305166142626, -1.792472147789250236, -0.7979012372742313453 ) ) ;
#117801 = CARTESIAN_POINT ( 'NONE',  ( 7.334597915313080918, 9.580116872663850813, 1.040834085586084257E-14 ) ) ;
#117802 = CARTESIAN_POINT ( 'NONE',  ( -4.553559489343377287, 6.405848385690952718, -1.599625672291271394 ) ) ;
#117803 = CARTESIAN_POINT ( 'NONE',  ( 5.256147377898004791, 0.8573370980917978113, -1.939729252509444279 ) ) ;
#117805 = CARTESIAN_POINT ( 'NONE',  ( 6.620655732516647518, 0.007553340620044743381, 1.826407896915738238 ) ) ;
#117804 = CARTESIAN_POINT ( 'NONE',  ( 8.910733272679570049, 11.41894145625809820, -1.599625672291255185 ) ) ;
#117806 =( BOUNDED_CURVE ( )  B_SPLINE_CURVE ( 2, ( #99719, #132257, #84530, #198264, #148482, #167919, #101850, #52040, #51 ),
 .UNSPECIFIED., .F., .T. ) 
 B_SPLINE_CURVE_WITH_KNOTS ( ( 3, 2, 2, 2, 3 ),
 ( 0.3906250000000002220, 0.3958333333333333148, 0.4062500000000000000, 0.4166666666666666852, 0.4218749999999998890 ),
 .UNSPECIFIED. ) 
 CURVE ( )  GEOMETRIC_REPRESENTATION_ITEM ( )  RATIONAL_B_SPLINE_CURVE ( ( 0.9330127018922194093, 0.9330127018922221849, 1.000000000000000000, 0.8660254037844387076, 1.000000000000000000, 0.8660254037844387076, 1.000000000000000000, 0.9330127018922207416, 0.9330127018922192983 ) ) 
 REPRESENTATION_ITEM ( '' )  );
#117807 = CARTESIAN_POINT ( 'NONE',  ( 6.696557531595894730, -0.5234078932761144776, -1.900562160593147754 ) ) ;
#117808 = CARTESIAN_POINT ( 'NONE',  ( 0.6823417656249899377, 1.842708333674752952, 1.181850606188755259 ) ) ;
#117809 = CARTESIAN_POINT ( 'NONE',  ( 1.617441171277278711, 1.676116182522195519, 1.114898189108826543 ) ) ;
#117810 = VERTEX_POINT ( 'NONE', #150846 ) ;
#117812 = CARTESIAN_POINT ( 'NONE',  ( 0.9665973488726641305, -2.066607521123296376, -0.4595904307344770290 ) ) ;
#117811 = CARTESIAN_POINT ( 'NONE',  ( -8.188761592974051595, 9.616271948966963024, -1.082531754730543971 ) ) ;
#117813 = CARTESIAN_POINT ( 'NONE',  ( 10.92756393739431076, 8.276992061150025393, 4.974981638007045959 ) ) ;
#117814 = CARTESIAN_POINT ( 'NONE',  ( 3.121598655985452275, 0.3063859900464052100, -2.047459029603612368 ) ) ;
#117815 = CARTESIAN_POINT ( 'NONE',  ( 5.903649544107831382, 5.852288987739402870, -0.7998128361456481317 ) ) ;
#117816 = CARTESIAN_POINT ( 'NONE',  ( 5.408776937209000657, 5.274937613024121674, 0.7998128361456352531 ) ) ;
#117817 = EDGE_LOOP ( 'NONE', ( #10386, #15358, #7743 ) ) ;
#117819 = CARTESIAN_POINT ( 'NONE',  ( 4.542145155778077203, 5.257923088951247159, -1.199719254218452047 ) ) ;
#117818 = CARTESIAN_POINT ( 'NONE',  ( 5.085920031106448747, -2.074780370831377230, -0.2563659892118006489 ) ) ;
#117822 = ORIENTED_EDGE ( 'NONE', *, *, #76293, .T. ) ;
#117821 = CARTESIAN_POINT ( 'NONE',  ( 3.193826918316445163, 1.151326796633693084, 1.398496967315324246 ) ) ;
#117820 = CARTESIAN_POINT ( 'NONE',  ( 3.012524388372894713, 1.323457619556423381, -1.257707024427484388 ) ) ;
#117823 = CARTESIAN_POINT ( 'NONE',  ( 6.551417122825020201, -1.769646310455679217, -1.318412661681533260 ) ) ;
#117824 = CARTESIAN_POINT ( 'NONE',  ( 6.890000000000000568, 2.439643239904603966, 2.382311923195524095 ) ) ;
#117825 = CARTESIAN_POINT ( 'NONE',  ( 10.27857769538790933, 8.980592535482619709, 4.146738271564137435 ) ) ;
#117826 = CARTESIAN_POINT ( 'NONE',  ( 5.157340341976529352, -1.861842412690998039, -1.184373046124863160 ) ) ;
#117827 = CARTESIAN_POINT ( 'NONE',  ( -1.364683531250010740, 9.442708333674735499, 0.7879004041258445001 ) ) ;
#117828 = CARTESIAN_POINT ( 'NONE',  ( 4.231050068913538631, 1.749697241329374098, 0.7720063087622434095 ) ) ;
#117829 = CARTESIAN_POINT ( 'NONE',  ( -4.569261463005423352, 5.289558780716470565, -1.199719254218446718 ) ) ;
#117830 = CARTESIAN_POINT ( 'NONE',  ( 8.769426429940780920, 9.125419011219408461, 0.7998128361456462443 ) ) ;
#117831 = CARTESIAN_POINT ( 'NONE',  ( -1.360316468750042862, 0.1510416670080827195, -0.7853790794159281052 ) ) ;
#117832 = CARTESIAN_POINT ( 'NONE',  ( 5.788968402910816380, 5.856144012925152076, 0.7216878364870317197 ) ) ;
#117833 = DIRECTION ( 'NONE',  ( 0.000000000000000000, 0.000000000000000000, 1.000000000000000000 ) ) ;
#117834 = CARTESIAN_POINT ( 'NONE',  ( 7.602957498476571097, 14.40772565114494341, -9.284908058097229855 ) ) ;
#117835 = CARTESIAN_POINT ( 'NONE',  ( -6.748594069003817530, 15.46991018063243928, -9.932583631540687463 ) ) ;
#117836 = ORIENTED_EDGE ( 'NONE', *, *, #31880, .T. ) ;
#117837 = EDGE_CURVE ( 'NONE', #47238, #59570, #85827, .T. ) ;
#117838 = CARTESIAN_POINT ( 'NONE',  ( 3.743291833738107144, -1.414529149469236691, -1.224010458943748603 ) ) ;
#117839 = CARTESIAN_POINT ( 'NONE',  ( 7.828907357248368726, 8.098423103070084395, 0.7998128361456281477 ) ) ;
#117840 = CARTESIAN_POINT ( 'NONE',  ( -0.2409995289980003397, 2.873648158547074338, -2.488896373646624749 ) ) ;
#117841 = CARTESIAN_POINT ( 'NONE',  ( -6.399085315970137522, 9.449054721065074602, -1.082531754730538864 ) ) ;
#117842 = CARTESIAN_POINT ( 'NONE',  ( 0.1934256698341470238, 1.783621342183003389, -0.6902995980747894667 ) ) ;
#117843 = CARTESIAN_POINT ( 'NONE',  ( 3.985207087413062066, 6.736826471035503694, -1.199719254218452047 ) ) ;
#117844 = CARTESIAN_POINT ( 'NONE',  ( 0.5671661303022774714, 1.710823773062917219, 0.9755123711343968163 ) ) ;
#117845 = CARTESIAN_POINT ( 'NONE',  ( 2.724232643812212196, 2.001515029240468646, 0.2440086781289458329 ) ) ;
#117846 = CARTESIAN_POINT ( 'NONE',  ( -8.453672473320708036, 9.821371626084353323, -1.199719254218446718 ) ) ;
#117847 = CARTESIAN_POINT ( 'NONE',  ( 6.717138760927786834, 6.801359740696030443, -0.7998128361456481317 ) ) ;
#117848 = CARTESIAN_POINT ( 'NONE',  ( 2.431793384409334902, 1.031818167245980744, -1.933333044699904857 ) ) ;
#117849 = CARTESIAN_POINT ( 'NONE',  ( 6.217409598193539999, -0.2183660865492654257, 1.812524795094340835 ) ) ;
#117850 = CARTESIAN_POINT ( 'NONE',  ( -4.457933580795036654, 4.095344020549286590, -0.7998128361456221525 ) ) ;
#117851 = CARTESIAN_POINT ( 'NONE',  ( 3.594320121398666856, 7.207474218358159490, -1.734723475976807094E-15 ) ) ;
#117852 = CARTESIAN_POINT ( 'NONE',  ( 9.271078113646423091, 9.710679308875986848, 1.040834085586084257E-14 ) ) ;
#117853 = EDGE_CURVE ( 'NONE', #111709, #171149, #177926, .T. ) ;
#117854 = CARTESIAN_POINT ( 'NONE',  ( 2.920892028740289081, 5.495125569250587816, 1.199719254218452047 ) ) ;
#117855 = CARTESIAN_POINT ( 'NONE',  ( 6.319508997745523438, 9.426492026461511742, -1.082531754730548412 ) ) ;
#117856 = VERTEX_POINT ( 'NONE', #52264 ) ;
#117858 = CARTESIAN_POINT ( 'NONE',  ( 0.3639315877056762405, 0.6293089562653730873, -1.912281478549708202 ) ) ;
#117857 = CARTESIAN_POINT ( 'NONE',  ( 3.895923546780861724, -0.5813109859279729230, -1.747131793041277970 ) ) ;
#117859 = CARTESIAN_POINT ( 'NONE',  ( 3.234050759648151363, -2.122446487128562875, -0.8823414489649589187 ) ) ;
#117861 = CARTESIAN_POINT ( 'NONE',  ( 0.5493571781046421298, 1.373546829346812714, 1.255761559867879962 ) ) ;
#117860 = CARTESIAN_POINT ( 'NONE',  ( 2.412988153552339643, 5.758977245878946327, 0.7216878364870438212 ) ) ;
#117862 = CARTESIAN_POINT ( 'NONE',  ( -1.737499999999997824, -0.6416666666666653862, 3.009438278150925683 ) ) ;
#117863 = CARTESIAN_POINT ( 'NONE',  ( -3.958090780185743451, 6.705190779270287393, -1.199719254218452047 ) ) ;
#117864 = CARTESIAN_POINT ( 'NONE',  ( -1.193489751472043232E-16, 4.400000000000001243, 2.150000000000006573 ) ) ;
#117865 = CARTESIAN_POINT ( 'NONE',  ( 5.009976098083095408, -0.6827417919906975108, 1.786564173047608062 ) ) ;
#117866 = CARTESIAN_POINT ( 'NONE',  ( -7.947050595904583403, 12.42330946186405249, 0.7998128361456481317 ) ) ;
#117867 = CARTESIAN_POINT ( 'NONE',  ( 6.330867959801246059, 6.852818249511213544, -0.6651261847785728820 ) ) ;
#117868 = CARTESIAN_POINT ( 'NONE',  ( -5.750066545971566079, 8.762142499391876171, 1.082531754730550855 ) ) ;
#117870 = CARTESIAN_POINT ( 'NONE',  ( 1.990876257202532695, 1.628914321797021669, -0.9196232060951770038 ) ) ;
#117869 = CARTESIAN_POINT ( 'NONE',  ( 4.107036007299074143, -0.3554739980045698022, 2.060130632118581051 ) ) ;
#117871 = CARTESIAN_POINT ( 'NONE',  ( 7.958272981541723468, 8.386999354661243800, 1.040834085586084257E-14 ) ) ;
#117872 = CARTESIAN_POINT ( 'NONE',  ( -6.445605026751819899, -8.233137084989717636, -6.979380938965669579 ) ) ;
#117873 = CARTESIAN_POINT ( 'NONE',  ( 3.526658842500699720, -1.606625690567566656, 0.6697392890405767796 ) ) ;
#117874 = MECHANICAL_DESIGN_GEOMETRIC_PRESENTATION_REPRESENTATION (  '', ( #183515 ), #69392 ) ;
#117875 = CARTESIAN_POINT ( 'NONE',  ( 5.172599298813543633, 5.993452922492633839, -1.199719254218452047 ) ) ;
#117876 = CARTESIAN_POINT ( 'NONE',  ( -1.500000000000001110, 11.55208333401612997, 0.8660254037844418162 ) ) ;
#117877 = CARTESIAN_POINT ( 'NONE',  ( 4.476996172482918368, -0.003761094005936410634, -1.725068444937064349 ) ) ;
#117878 = CARTESIAN_POINT ( 'NONE',  ( -6.039267359883488950, 9.133230122250985517, 1.199719254218452047 ) ) ;
#117879 = CARTESIAN_POINT ( 'NONE',  ( 6.076841795016812320, -2.094286673724785164, -0.6961510500591641115 ) ) ;
#117880 = SURFACE_STYLE_USAGE ( .BOTH. , #150329 ) ;
#117881 = CARTESIAN_POINT ( 'NONE',  ( 3.731445244768144764, 0.05858319805804703545, -2.170454240781857003 ) ) ;
#117882 = CARTESIAN_POINT ( 'NONE',  ( 1.875362892791394787, 1.747422460009705913, -0.5287960245906262458 ) ) ;
#117883 = FACE_OUTER_BOUND ( 'NONE', #53375, .T. ) ;
#117884 = CARTESIAN_POINT ( 'NONE',  ( 6.104719058799578768, 1.976458628850938704, 0.7599229572291065216 ) ) ;
#117885 = ORIENTED_EDGE ( 'NONE', *, *, #200871, .T. ) ;
#117887 = CARTESIAN_POINT ( 'NONE',  ( -1.201851678989727383E-14, 3.259375000341420581, -1.575800808251660134 ) ) ;
#117886 = CARTESIAN_POINT ( 'NONE',  ( 6.058190142838977721, -1.623990863767441617, 1.618158029567408729 ) ) ;
#117888 = CARTESIAN_POINT ( 'NONE',  ( 9.562578416340237197, 10.05076299535211781, 0.7998128361456462443 ) ) ;
#117889 = VECTOR ( 'NONE', #2969, 1000.000000000000000 ) ;
#117890 = CARTESIAN_POINT ( 'NONE',  ( 1.559403367407938390, -1.789607135292633266, 1.137164086494051096 ) ) ;
#117891 = CARTESIAN_POINT ( 'NONE',  ( -5.314433026876900001, 6.262888621853549331, 1.082531754730548412 ) ) ;
#117892 = CARTESIAN_POINT ( 'NONE',  ( 2.412988153552339643, 5.758977245878946327, 0.7216878364870438212 ) ) ;
#117893 = CARTESIAN_POINT ( 'NONE',  ( -5.788968402910818156, 7.776882441527838807, 1.443375672974064550 ) ) ;
#117895 = CARTESIAN_POINT ( 'NONE',  ( -6.009258394948636914E-15, 12.21875000068279782, -1.732050807568875195 ) ) ;
#117894 = CARTESIAN_POINT ( 'NONE',  ( 0.08522875510948167699, -9.999176759342304877, 10.91956886450205033 ) ) ;
#117897 = ORIENTED_EDGE ( 'NONE', *, *, #63311, .F. ) ;
#117896 = CARTESIAN_POINT ( 'NONE',  ( 0.8037664367953377687, 1.956346004370253633, -1.052120880887427390 ) ) ;
#117898 = CARTESIAN_POINT ( 'NONE',  ( 0.08910568399025410591, -0.6041685166103001325, 2.217849651370594088 ) ) ;
#117900 = CARTESIAN_POINT ( 'NONE',  ( 4.926661567281545473, -1.351126562560464484, 1.558462338037209349 ) ) ;
#117899 = CARTESIAN_POINT ( 'NONE',  ( 3.635557746758808495, 7.393234471193928847, -0.7998128361456291469 ) ) ;
#117902 = CARTESIAN_POINT ( 'NONE',  ( 1.001543065824772753E-15, -3.062499999999998668, 4.012584370867899430 ) ) ;
#117901 = CARTESIAN_POINT ( 'NONE',  ( 7.693325821111733021, 7.940244644243982464, -0.7998128361456341429 ) ) ;
#117903 = CARTESIAN_POINT ( 'NONE',  ( 7.198453214212898743, 7.362893269528701268, 0.7998128361456291469 ) ) ;
#117904 = CARTESIAN_POINT ( 'NONE',  ( 1.001543065824772753E-15, -0.7218749995220414828, 3.793834371823811669 ) ) ;
#117905 =( LENGTH_UNIT ( ) NAMED_UNIT ( * ) SI_UNIT ( .MILLI., .METRE. ) );
#117906 = CARTESIAN_POINT ( 'NONE',  ( 1.043050037176814326, -1.649054093272810606, -1.284947313888247900 ) ) ;
#117907 = CARTESIAN_POINT ( 'NONE',  ( 4.817029820108094995, 1.034167108704350024, -1.730865207599366240 ) ) ;
#117908 = CARTESIAN_POINT ( 'NONE',  ( 3.878315922200573862, -0.1843894689829879696, -1.832007427040844183 ) ) ;
#117909 = EDGE_CURVE ( 'NONE', #141519, #102469, #119206, .T. ) ;
#117910 = CARTESIAN_POINT ( 'NONE',  ( 5.867981556616276073, 5.740399992340775803, -0.7998128361456281477 ) ) ;
#117911 = SURFACE_STYLE_FILL_AREA ( #182834 ) ;
#117912 = CARTESIAN_POINT ( 'NONE',  ( 0.6919144707170435948, -1.710882258413017221, -0.2179282654613586834 ) ) ;
#117913 = CARTESIAN_POINT ( 'NONE',  ( -0.1355283706049141557, -1.957205112593700003, -0.4852584411360050254 ) ) ;
#117914 = CARTESIAN_POINT ( 'NONE',  ( -4.550733115681270036, 8.460939068270139529, 0.7998128361456481317 ) ) ;
#117915 = CARTESIAN_POINT ( 'NONE',  ( 1.159873712335700802, 0.4409813497070895760, -2.218855480106549649 ) ) ;
#117916 = CARTESIAN_POINT ( 'NONE',  ( 2.895255201988570892, 1.806112693971681615, -1.083030686944158161 ) ) ;
#117917 = CARTESIAN_POINT ( 'NONE',  ( -4.716257332707368910, 6.595662536282280719, -1.599625672291271394 ) ) ;
#117918 = CARTESIAN_POINT ( 'NONE',  ( 5.961834861707224320, 7.978559976790334574, -1.599625672291262513 ) ) ;
#117919 = CARTESIAN_POINT ( 'NONE',  ( 5.356880090730850696, 9.263794182579101033, 0.7216878364870317197 ) ) ;
#117920 = CARTESIAN_POINT ( 'NONE',  ( 0.000000000000000000, 0.4651705836652164638, -2.021763587583139010 ) ) ;
#117921 = CARTESIAN_POINT ( 'NONE',  ( -5.168682875307782254, 7.053215992657626110, -1.599625672291256295 ) ) ;
#117922 = CARTESIAN_POINT ( 'NONE',  ( 7.429504990164394584, 7.770103364721017591, 1.040834085586084257E-14 ) ) ;
#117923 = CARTESIAN_POINT ( 'NONE',  ( 4.626555186793138930, 7.126393038833472637, 1.348983236782254957 ) ) ;
#117924 = CARTESIAN_POINT ( 'NONE',  ( -4.623494077460110319, 5.352830164246910272, 1.199719254218462483 ) ) ;
#117925 = CARTESIAN_POINT ( 'NONE',  ( 5.642908736356011978, 2.140874091242400912, 0.5926086046802480078 ) ) ;
#117926 = CARTESIAN_POINT ( 'NONE',  ( 3.170069416559752273, -1.305109287949431929, 1.760291797049506446 ) ) ;
#117927 = CARTESIAN_POINT ( 'NONE',  ( -6.600121851754250812, 6.594563670001734046, 0.7998128361456341429 ) ) ;
#117928 = CARTESIAN_POINT ( 'NONE',  ( -3.526002468005825286, 6.271364091718859335, -1.199719254218450271 ) ) ;
#117929 = CARTESIAN_POINT ( 'NONE',  ( 6.004347769543215030, 1.959566550440184907, 0.09775035808561728656 ) ) ;
#117930 = CARTESIAN_POINT ( 'NONE',  ( -0.6823417656249969321, 3.467708333674754506, -1.181850606188749264 ) ) ;
#117931 = CARTESIAN_POINT ( 'NONE',  ( 6.610000000000009202, 6.036727194997777879, 2.594899704271665275 ) ) ;
#117932 = CARTESIAN_POINT ( 'NONE',  ( -5.612712406377534435, 5.650512016969639895, 0.7216878364870317197 ) ) ;
#117933 = CARTESIAN_POINT ( 'NONE',  ( 4.658503719480325600, 2.115088938745744329, 0.1532479335744421078 ) ) ;
#117934 = CARTESIAN_POINT ( 'NONE',  ( -6.400857919427531684, 9.521399101757175742, 1.082531754730549967 ) ) ;
#117935 = ORIENTED_EDGE ( 'NONE', *, *, #112074, .T. ) ;
#117937 = CARTESIAN_POINT ( 'NONE',  ( 6.104392421991035711, -0.7735064434604683736, -2.018760209060527888 ) ) ;
#117936 = CARTESIAN_POINT ( 'NONE',  ( -6.129694847154222970, 7.284303755502281597, -1.082531754730549967 ) ) ;
#117938 = CARTESIAN_POINT ( 'NONE',  ( 4.008406971134620633, 7.828225232965717595, 0.7998128361456321445 ) ) ;
#117939 = CARTESIAN_POINT ( 'NONE',  ( 5.653808312887881549, 0.7519890275384639722, 1.680886247995525773 ) ) ;
#117940 = CIRCLE ( 'NONE', #204429, 0.08000000000000069555 ) ;
#117941 = CARTESIAN_POINT ( 'NONE',  ( 1.364683531249986537, 2.717708333674754062, -0.7879004041258239610 ) ) ;
#117942 = CARTESIAN_POINT ( 'NONE',  ( 1.311604768886602157, 1.169564267535606605, -1.289085965974474668 ) ) ;
#117943 = CARTESIAN_POINT ( 'NONE',  ( 11.48243876534946217, 12.29999999999998295, 3.199999999999997957 ) ) ;
#117944 = CARTESIAN_POINT ( 'NONE',  ( 3.606105671554957759, 4.269840040644637291, -1.082531754730543083 ) ) ;
#117945 = CARTESIAN_POINT ( 'NONE',  ( -0.4288785890452732064, 3.049942316455313218, 0.4196807566830707548 ) ) ;
#117946 = CARTESIAN_POINT ( 'NONE',  ( 5.577088068215094729, -0.04877400797019536272, -2.161318155665878038 ) ) ;
#117947 = CARTESIAN_POINT ( 'NONE',  ( -3.810004860640155311, 4.403759411290286252, 1.199719254218462483 ) ) ;
#117948 = CARTESIAN_POINT ( 'NONE',  ( -6.927853306458756855, 9.105581495667113501, 1.443375672974078761 ) ) ;
#117949 = CARTESIAN_POINT ( 'NONE',  ( 4.170900312159072421, -2.016029151617684256, -0.7805680927704603533 ) ) ;
#117950 = CARTESIAN_POINT ( 'NONE',  ( 1.364683531249986537, 2.405208333674752286, -0.7879004041258239610 ) ) ;
#117951 = CARTESIAN_POINT ( 'NONE',  ( 6.468046296993485988, 1.011472520757991767, 1.691939633080985272 ) ) ;
#117952 = CARTESIAN_POINT ( 'NONE',  ( 4.551880008920849541, 1.548817843433186736, -0.7794160303473545159 ) ) ;
#117953 = CARTESIAN_POINT ( 'NONE',  ( 1.751786407749492014, 2.185395279939935431, -0.1653414253460702699 ) ) ;
#117954 = CARTESIAN_POINT ( 'NONE',  ( 2.696638560983040112, -2.301352489519994382, -0.1704845361689636130 ) ) ;
#117955 = CARTESIAN_POINT ( 'NONE',  ( 4.973930670403752252, 1.183205397963146499, 1.687068388967316368 ) ) ;
#117956 = CARTESIAN_POINT ( 'NONE',  ( 0.1638716437233995460, -1.269140265717118465, 1.469938112931449270 ) ) ;
#117958 = EDGE_CURVE ( 'NONE', #47758, #135057, #185447, .T. ) ;
#117957 = CARTESIAN_POINT ( 'NONE',  ( -6.304178240230145391, 9.338329799368375816, 1.082531754730548412 ) ) ;
#117959 = CARTESIAN_POINT ( 'NONE',  ( -3.318713740295064163, 7.093859473644694269, 0.000000000000000000 ) ) ;
#117960 = CARTESIAN_POINT ( 'NONE',  ( -7.446209719563359641, -5.223431457505076203, -8.064677165291183059 ) ) ;
#117961 = DIRECTION ( 'NONE',  ( 0.000000000000000000, -1.000000000000000000, 0.000000000000000000 ) ) ;
#117962 = CARTESIAN_POINT ( 'NONE',  ( 1.723279953462612202, 1.994870059565261755, 0.2930690452552578429 ) ) ;
#117963 = CARTESIAN_POINT ( 'NONE',  ( -7.063434842595444962, 8.303390740191881392, 1.082531754730549967 ) ) ;
#117964 = CARTESIAN_POINT ( 'NONE',  ( 2.925073249431627165, 2.077443920948469192, 0.7446974470129495982 ) ) ;
#117965 = CARTESIAN_POINT ( 'NONE',  ( -3.285556943749998737, -1.917708332855377673, 1.896917185911908499 ) ) ;
#117966 = CARTESIAN_POINT ( 'NONE',  ( 1.375590602687895458, -1.817075280682054927, 0.4009801126106312674 ) ) ;
#117967 = EDGE_CURVE ( 'NONE', #83638, #200016, #101829, .T. ) ;
#117968 = CARTESIAN_POINT ( 'NONE',  ( 0.1399997263885794929, 4.089933038008564559, -2.554595152914000078 ) ) ;
#117969 = CARTESIAN_POINT ( 'NONE',  ( 0.000000000000000000, 0.000000000000000000, 0.000000000000000000 ) ) ;
#117970 = CARTESIAN_POINT ( 'NONE',  ( 2.750651594100012254, 2.940524554645664868, -2.453100423511232808 ) ) ;
#117972 = CARTESIAN_POINT ( 'NONE',  ( 6.825078400183544503, 3.684911640780349718, 2.658296617506946458 ) ) ;
#117971 = CARTESIAN_POINT ( 'NONE',  ( -5.594533863947632746, 7.496198557292433229, -1.347124935377568722 ) ) ;
#117973 = DIRECTION ( 'NONE',  ( 1.000000000000000000, 0.000000000000000000, 0.000000000000000000 ) ) ;
#117974 = ORIENTED_EDGE ( 'NONE', *, *, #135323, .T. ) ;
#117975 = CARTESIAN_POINT ( 'NONE',  ( 3.889569955515647326, 1.491445920024776051, 1.422513881352378107 ) ) ;
#117976 = CARTESIAN_POINT ( 'NONE',  ( -0.6801582343750282034, 2.432291667008048996, 1.178068619123807004 ) ) ;
#117977 = EDGE_CURVE ( 'NONE', #56620, #198793, #89049, .T. ) ;
#117978 = UNCERTAINTY_MEASURE_WITH_UNIT (LENGTH_MEASURE( 1.000000000000000082E-05 ), #194247, 'distance_accuracy_value', 'NONE');
#117979 = CARTESIAN_POINT ( 'NONE',  ( -6.878064000834399394, 6.918829510595249310, -0.7998128361456291469 ) ) ;
#117980 = CARTESIAN_POINT ( 'NONE',  ( 1.822921661270057836, 1.494980448624585234, -1.358156064218164927 ) ) ;
#117981 = CARTESIAN_POINT ( 'NONE',  ( 0.7499999999999867883, -0.9333333333333138082, -1.299038105676652011 ) ) ;
#117982 = CARTESIAN_POINT ( 'NONE',  ( 2.835626683552519012, 6.459981564119914310, 0.000000000000000000 ) ) ;
#117983 = CARTESIAN_POINT ( 'NONE',  ( 2.395450018592326646, 1.592181132671898869, 1.308497088967359723 ) ) ;
#117985 = CARTESIAN_POINT ( 'NONE',  ( 1.364683531250000303, 13.50520833367472839, -0.7879004041258355073 ) ) ;
#117984 = CARTESIAN_POINT ( 'NONE',  ( 3.975693637526477975E-16, -3.499999999999999556, -3.017800438942085606 ) ) ;
#117986 = CARTESIAN_POINT ( 'NONE',  ( 6.844168616800228477, 6.879284895888727824, -0.7998128361456281477 ) ) ;
#117987 = CARTESIAN_POINT ( 'NONE',  ( -0.1408020194049964258, 1.331054986036240173, -2.350941690117592575 ) ) ;
#117988 = CARTESIAN_POINT ( 'NONE',  ( 5.145248760827346501, -1.894204247122273088, 1.132176536499051700 ) ) ;
#117989 = CARTESIAN_POINT ( 'NONE',  ( 5.200434439293556643, 8.224868058221247225, -1.199719254218452047 ) ) ;
#117990 = CARTESIAN_POINT ( 'NONE',  ( 1.106953007505812492, 1.637591863572019690, -1.411084338363017832 ) ) ;
#117991 = CARTESIAN_POINT ( 'NONE',  ( -3.280709984826970516, 6.771319382366015383, 0.7216878364870317197 ) ) ;
#117992 = CARTESIAN_POINT ( 'NONE',  ( 1.639861632979456418, 2.010800986640928656, -0.1531718788195315928 ) ) ;
#117993 = FILL_AREA_STYLE ('',( #200222 ) ) ;
#117994 = CARTESIAN_POINT ( 'NONE',  ( 0.4791068267422092797, 1.747065859276742072, -0.6691465683838908607 ) ) ;
#117995 = CARTESIAN_POINT ( 'NONE',  ( -11.89942855770814134, 9.799999999999998934, 0.6999999999999992895 ) ) ;
#117997 = EDGE_CURVE ( 'NONE', #114100, #186393, #22326, .T. ) ;
#117996 = AXIS2_PLACEMENT_3D ( 'NONE', #130181, #44606, #109666 ) ;
#117998 = CARTESIAN_POINT ( 'NONE',  ( 2.412791964582483129, 1.669947582624079274, 0.8431454209596804805 ) ) ;
#117999 = CARTESIAN_POINT ( 'NONE',  ( 3.889861467948489082, -2.010801299972611478, 0.1531677096566556595 ) ) ;
#118001 = CARTESIAN_POINT ( 'NONE',  ( -0.008622031262367491067, 15.44736672593548299, 11.95585889282746450 ) ) ;
#118000 = CARTESIAN_POINT ( 'NONE',  ( -1.364683531250012516, 1.530208333674756505, 0.7879004041258379498 ) ) ;
#118002 = B_SPLINE_CURVE_WITH_KNOTS ( 'NONE', 3,
 ( #196441, #149833, #63235, #97893, #166070, #145604 ),
 .UNSPECIFIED., .F., .F.,
 ( 4, 2, 4 ),
 ( 0.000000000000000000, 0.001226111284895915667, 0.002452222569791831334 ),
 .UNSPECIFIED. ) ;
#118004 = CARTESIAN_POINT ( 'NONE',  ( 5.531892221078217098, -1.335191642697653336, -1.628727054747380887 ) ) ;
#118003 = CARTESIAN_POINT ( 'NONE',  ( -7.069687034522070590, 10.33538640932937724, -1.199719254218440723 ) ) ;
#118005 = CARTESIAN_POINT ( 'NONE',  ( 5.770966940911189447, 9.884545197705074671, -0.7998128361456291469 ) ) ;
#118006 = CARTESIAN_POINT ( 'NONE',  ( -6.364663046611467756, 9.512858423433634414, 1.199719254218452047 ) ) ;
#118007 = CARTESIAN_POINT ( 'NONE',  ( 6.639320575229286092, 2.965970653406803770, 2.456291990408800086 ) ) ;
#118008 = CARTESIAN_POINT ( 'NONE',  ( 5.150651408520660723, 1.990593866887302221, 0.3411176234145337216 ) ) ;
#118009 = CARTESIAN_POINT ( 'NONE',  ( 1.364683531249988535, 5.655208333674751842, -0.7879004041258300672 ) ) ;
#118010 = CARTESIAN_POINT ( 'NONE',  ( 0.4442778734073973279, -0.9756673871180139290, 1.817250197203540640 ) ) ;
#118011 = CARTESIAN_POINT ( 'NONE',  ( 7.863365906246055914, 10.19701286208565705, -1.443375672974057666 ) ) ;
#118012 = CARTESIAN_POINT ( 'NONE',  ( 6.638652492546827766, 7.774124658506663010, 1.199719254218452047 ) ) ;
#118013 = CARTESIAN_POINT ( 'NONE',  ( 6.398522151006641678, 6.429640362454684954, 0.000000000000000000 ) ) ;
#118014 = CARTESIAN_POINT ( 'NONE',  ( 1.364683531249986537, 0.1760416670080860446, 0.7879004041258500513 ) ) ;
#118016 = CARTESIAN_POINT ( 'NONE',  ( 8.912450614902654777, 3.507114751586604129, 8.024806578262976942 ) ) ;
#118015 = CARTESIAN_POINT ( 'NONE',  ( 4.746236293235721604, 7.694970221153795364, 1.199719254218451159 ) ) ;
#118017 = CARTESIAN_POINT ( 'NONE',  ( 7.090551149822728938, 10.25576486055978442, 1.082531754730558626 ) ) ;
#118019 = CARTESIAN_POINT ( 'NONE',  ( -5.345849613874695372, 4.689682906365682413, -2.440353602067509176 ) ) ;
#118018 = CARTESIAN_POINT ( 'NONE',  ( 3.508415132820621007, 2.171350060761201295, 0.003086831990101178078 ) ) ;
#118021 = CARTESIAN_POINT ( 'NONE',  ( 3.280630368989821743, 1.663260157205956880, -0.7901080472864712156 ) ) ;
#118020 = CARTESIAN_POINT ( 'NONE',  ( -4.284013352238255301, 6.981470763377843447, -1.082531754730549967 ) ) ;
#118022 = CARTESIAN_POINT ( 'NONE',  ( 1.364683531249988535, 3.113541667008083991, 0.7879004041258500513 ) ) ;
#118023 = CARTESIAN_POINT ( 'NONE',  ( 4.036819321710017228, -1.906298169312226953, 1.081085072550565407 ) ) ;
#118024 = CARTESIAN_POINT ( 'NONE',  ( 8.790098660144264997, 13.29414747594432278, 8.101455065885629026 ) ) ;
#118025 = CARTESIAN_POINT ( 'NONE',  ( 4.856464543430921488, 0.8614301073998543723, 2.092300974686135184 ) ) ;
#118026 = CARTESIAN_POINT ( 'NONE',  ( -6.124532705071231931, 8.168374127381657246, -1.599625672291263179 ) ) ;
#118027 = DIRECTION ( 'NONE',  ( -0.000000000000000000, -1.000000000000000000, -0.000000000000000000 ) ) ;
#118028 = CARTESIAN_POINT ( 'NONE',  ( 4.605689926069578277, 8.476745573306274650, -0.2140288463435610078 ) ) ;
#118029 = COLOUR_RGB ( '', 0.31764706, 0.68627451, 0.89019608) ;
#118030 = CARTESIAN_POINT ( 'NONE',  ( -6.427974226210522168, 6.671927150099951298, 0.000000000000000000 ) ) ;
#118031 = CARTESIAN_POINT ( 'NONE',  ( 5.560252395380222090, 5.659585014131299552, 0.7216878364870328300 ) ) ;
#118032 = CARTESIAN_POINT ( 'NONE',  ( 6.151566388294868126, 0.5118450565497618676, -1.694058711534670358 ) ) ;
#118033 = CARTESIAN_POINT ( 'NONE',  ( 4.336591701909254581, 1.236597081578957757, -1.588450131361287987 ) ) ;
#118034 = CARTESIAN_POINT ( 'NONE',  ( 7.202405917357655341, 9.425892875049191488, 1.599625672291281386 ) ) ;
#118035 = CARTESIAN_POINT ( 'NONE',  ( 2.766744854014174138, -1.453255750356880371, 1.524405782528108766 ) ) ;
#118036 = CARTESIAN_POINT ( 'NONE',  ( 0.8080361750046762825, 1.140156559909396128, -1.539198610912548171 ) ) ;
#118038 = CARTESIAN_POINT ( 'NONE',  ( -1.201851678989727383E-14, 3.087500000000026112, -1.732050807568863648 ) ) ;
#118037 = CARTESIAN_POINT ( 'NONE',  ( -0.6823417656250003738, 11.65104166700806765, 1.181850606188754593 ) ) ;
#118039 = CARTESIAN_POINT ( 'NONE',  ( 2.066797411385603578, 1.461431172244957333, -1.320572070109968799 ) ) ;
#118040 = CARTESIAN_POINT ( 'NONE',  ( 4.922131295886445379, -2.009687048479208205, 0.2019785858936548328 ) ) ;
#118041 = CARTESIAN_POINT ( 'NONE',  ( 1.024039198018782626, 1.117340804906666873, -1.500143343703803422 ) ) ;
#118042 = CARTESIAN_POINT ( 'NONE',  ( 1.328483007144948935, -1.247240240105648601, 1.514344512384787622 ) ) ;
#118044 = VERTEX_POINT ( 'NONE', #72766 ) ;
#118043 = CARTESIAN_POINT ( 'NONE',  ( 0.4043728756845180183, -1.898191424145349471, -0.2318213773434482650 ) ) ;
#118045 = CARTESIAN_POINT ( 'NONE',  ( 4.690757960648213931, 8.416375354157496602, 0.7216878364870438212 ) ) ;
#118046 = CIRCLE ( 'NONE', #83328, 10.25000000000000000 ) ;
#118047 = CARTESIAN_POINT ( 'NONE',  ( -1.402160292154681736E-14, 1.009375000341417916, -1.575800808251659024 ) ) ;
#118048 = CARTESIAN_POINT ( 'NONE',  ( 5.875831987524620992, 1.115552982110395330, 1.501486808359139946 ) ) ;
#118049 = CARTESIAN_POINT ( 'NONE',  ( 8.543609354905870035, 13.11929468069890525, 0.7998128361456462443 ) ) ;
#118050 = FACE_OUTER_BOUND ( 'NONE', #103726, .T. ) ;
#118051 = CARTESIAN_POINT ( 'NONE',  ( 5.823117640241993520, -1.869163851432435575, -0.8903994044791310181 ) ) ;
#118052 = CARTESIAN_POINT ( 'NONE',  ( 0.000000000000000000, 4.006659545634088992, 0.000000000000000000 ) ) ;
#118053 = CARTESIAN_POINT ( 'NONE',  ( -3.296040741453672318, 6.859481608422314025, 0.7216878364870338292 ) ) ;
#118054 = CARTESIAN_POINT ( 'NONE',  ( 0.07661050522433658638, 0.008287133257128469904, -1.710863442170394988 ) ) ;
#118055 = CARTESIAN_POINT ( 'NONE',  ( -1.500000000000001332, 0.1500000000000251132, 0.000000000000000000 ) ) ;
#118056 = CARTESIAN_POINT ( 'NONE',  ( 7.293396569147545527, 10.59638086639245280, 1.199719254218460707 ) ) ;
#118057 = CARTESIAN_POINT ( 'NONE',  ( -8.748035429315585532, 11.22912730566677553, -1.599625672291263179 ) ) ;
#118058 = CARTESIAN_POINT ( 'NONE',  ( 4.532168488718122390, 8.509556680138327778, 0.7998128361456271485 ) ) ;
#118059 = CARTESIAN_POINT ( 'NONE',  ( -0.6823417656250212460, 1.801041667008083991, 1.181850606188755259 ) ) ;
#118060 = CARTESIAN_POINT ( 'NONE',  ( 1.499999999999987121, 2.045833333333356929, -0.8660254037844262731 ) ) ;
#118062 = CARTESIAN_POINT ( 'NONE',  ( 3.499976210622149253, 7.235056012367825140, 0.7998128361456321445 ) ) ;
#118061 = CARTESIAN_POINT ( 'NONE',  ( 5.160583804383015227, -0.6592509027269661814, -1.847929681152965520 ) ) ;
#118063 = CARTESIAN_POINT ( 'NONE',  ( 2.653672528425448540, -0.3418824089525332455, -1.986742401007553172 ) ) ;
#118064 = CARTESIAN_POINT ( 'NONE',  ( 2.817496537900533671, -1.290266535947793392, -1.416188432289398058 ) ) ;
#118065 = CARTESIAN_POINT ( 'NONE',  ( 11.84668729410392274, 10.09379487675467146, -1.400000000000001688 ) ) ;
#118066 = CARTESIAN_POINT ( 'NONE',  ( 0.6971427418834205136, 1.794861059153027627, 1.257291590721874686 ) ) ;
#118067 = CARTESIAN_POINT ( 'NONE',  ( -2.926243505372967280E-18, -4.140708350189166609, -0.9999999999999991118 ) ) ;
#118068 = CARTESIAN_POINT ( 'NONE',  ( 3.145614842782416432, 0.6765965015090926737, -1.744060075730607950 ) ) ;
#118069 = CARTESIAN_POINT ( 'NONE',  ( 1.499999999999987121, 0.03541666734948738238, 0.8660254037844524744 ) ) ;
#118070 = CARTESIAN_POINT ( 'NONE',  ( -8.681298431451969222, 9.022603012982438386, 1.040834085586084257E-14 ) ) ;
#118072 = CARTESIAN_POINT ( 'NONE',  ( 3.937202496034042376, -1.761399977300786901, -1.174509457245224597 ) ) ;
#118071 = CARTESIAN_POINT ( 'NONE',  ( -4.202664430556263930, 5.926194473780837413, 1.443375672974064550 ) ) ;
#118073 = LINE ( 'NONE', #151588, #146067 ) ;
#118074 = CARTESIAN_POINT ( 'NONE',  ( 5.529760519541640384, 1.996289034380031913, -0.5486624943154896350 ) ) ;
#118076 = CARTESIAN_POINT ( 'NONE',  ( -4.333496373511149358, 7.757669579117222547, -0.6939643617286651578 ) ) ;
#118075 = CARTESIAN_POINT ( 'NONE',  ( 1.751626234865871767, 2.084932195785852649, -0.1569159079413025293 ) ) ;
#118078 = ORIENTED_EDGE ( 'NONE', *, *, #173979, .F. ) ;
#118077 = CARTESIAN_POINT ( 'NONE',  ( 0.8324923845523107824, 0.1201152365052655241, 1.720655618271366150 ) ) ;
#118079 = CARTESIAN_POINT ( 'NONE',  ( 6.265839547809997079, 10.46189657242035587, 0.7998128361456462443 ) ) ;
#118080 = CARTESIAN_POINT ( 'NONE',  ( 9.175356366548005127, 14.33556514466065757, 7.734832780443797517 ) ) ;
#118081 = CARTESIAN_POINT ( 'NONE',  ( -0.08118383494907006892, -9.908729948657656550, -9.499653137018302829 ) ) ;
#118082 = CARTESIAN_POINT ( 'NONE',  ( -9.911963570431085557, 5.384551446482307213, 6.114068938207696036 ) ) ;
#118083 = CARTESIAN_POINT ( 'NONE',  ( 6.060131475184119765, 9.053608573481392696, -1.082531754730537976 ) ) ;
#118084 = CARTESIAN_POINT ( 'NONE',  ( -1.364683531250010740, 13.19270833367472839, 0.7879004041258445001 ) ) ;
#118085 = PRODUCT_DEFINITION_FORMATION_WITH_SPECIFIED_SOURCE ( 'ANY', '', #176864, .NOT_KNOWN. ) ;
#118087 = CARTESIAN_POINT ( 'NONE',  ( 0.2229362713279548491, 1.575107908988721883, 0.8944890650159162959 ) ) ;
#118086 = CARTESIAN_POINT ( 'NONE',  ( 7.191674137406095291, 7.354984346587396082, 0.000000000000000000 ) ) ;
#118088 = CARTESIAN_POINT ( 'NONE',  ( -8.505042434474312074, 8.816971016508505343, -0.7998128361456291469 ) ) ;
#118089 = AXIS2_PLACEMENT_3D ( 'NONE', #96367, #80082, #191686 ) ;
#118090 = CARTESIAN_POINT ( 'NONE',  ( 3.683011284406639607, 7.448596931783069586, 0.7998128361456321445 ) ) ;
#118091 = CARTESIAN_POINT ( 'NONE',  ( -5.130090819275266334, 7.806487709571898748, 1.156910012491520590 ) ) ;
#118092 = CARTESIAN_POINT ( 'NONE',  ( 5.338878628731272613, 9.450718510153643948, -0.7998128361456481317 ) ) ;
#118093 = CIRCLE ( 'NONE', #7450, 11.92000000000000171 ) ;
#118094 = CARTESIAN_POINT ( 'NONE',  ( 0.1480828224388863745, -6.655928102866957907, 10.87712779691740117 ) ) ;
#118095 = CARTESIAN_POINT ( 'NONE',  ( 4.159596813995052322, 7.384974941181836172, -0.7733407813514819873 ) ) ;
#118096 = CARTESIAN_POINT ( 'NONE',  ( 8.703971430293332645, 12.13808852110884118, -1.082531754730543083 ) ) ;
#118097 = ORIENTED_EDGE ( 'NONE', *, *, #51127, .F. ) ;
#118098 = EDGE_CURVE ( 'NONE', #69637, #110438, #120120, .T. ) ;
#118099 = CARTESIAN_POINT ( 'NONE',  ( 5.835564593388589572, 0.5826401998472263699, -1.930423629703325927 ) ) ;
#118100 = CARTESIAN_POINT ( 'NONE',  ( 11.48243876534946217, 12.29999999999998295, 3.199999999999997957 ) ) ;
#118101 = DIRECTION ( 'NONE',  ( -0.000000000000000000, -1.000000000000000000, -0.000000000000000000 ) ) ;
#118102 = CARTESIAN_POINT ( 'NONE',  ( 1.807185592549606312, 2.518115318451403795, 2.499999999999998668 ) ) ;
#118103 = CARTESIAN_POINT ( 'NONE',  ( -3.294268138440636928, 6.787137228248626641, 1.040834085586084257E-14 ) ) ;
#118104 = CARTESIAN_POINT ( 'NONE',  ( 9.436111725431318931, 10.11114455586577776, -0.7216878364870257245 ) ) ;
#118105 = CARTESIAN_POINT ( 'NONE',  ( 3.643367292660666390, 1.782436080146361013, -0.8378801856493125477 ) ) ;
#118106 = CARTESIAN_POINT ( 'NONE',  ( 0.9793288802587530872, -1.918618388578940737, -0.9032494106611320683 ) ) ;
#118107 = CARTESIAN_POINT ( 'NONE',  ( -5.473741331615264549, 7.409117525016355010, -1.599625672291256295 ) ) ;
#118108 = CARTESIAN_POINT ( 'NONE',  ( 1.387358672533593129, 7.315968950352074174, -4.254625267140469624 ) ) ;
#118109 = CARTESIAN_POINT ( 'NONE',  ( 6.727182134110194056, 3.682851444631680682, 2.702965647100654234 ) ) ;
#118110 = CARTESIAN_POINT ( 'NONE',  ( 6.439412520197737244, 0.8424478218750917069, -2.023249321508275855 ) ) ;
#118111 = CARTESIAN_POINT ( 'NONE',  ( 3.939296163839981713, 2.811845806437661466, 0.7749999999965996311 ) ) ;
#118112 = CARTESIAN_POINT ( 'NONE',  ( 4.366181854897908998, 0.9076448143166337967, 1.699152538019559788 ) ) ;
#118113 = CARTESIAN_POINT ( 'NONE',  ( -6.808165692356648258, 11.09461040772476714, 0.7998128361456481317 ) ) ;
#118114 = CARTESIAN_POINT ( 'NONE',  ( -0.02988540731099689068, 4.098597030192621560, -2.281328281275496916 ) ) ;
#118115 = CARTESIAN_POINT ( 'NONE',  ( 0.8036966383840878914, 1.806304194667744500, 1.267646993260997945 ) ) ;
#118116 = DIRECTION ( 'NONE',  ( -1.000000000000000000, 0.000000000000000000, 0.000000000000000000 ) ) ;
#118117 = ORIENTED_EDGE ( 'NONE', *, *, #66399, .T. ) ;
#118118 = CARTESIAN_POINT ( 'NONE',  ( 4.923019175537949543, 4.916146257648610352, 0.000000000000000000 ) ) ;
#118119 = CARTESIAN_POINT ( 'NONE',  ( 6.754754220498722539, -0.5220956727660872598, -1.898933868174660589 ) ) ;
#118120 = CARTESIAN_POINT ( 'NONE',  ( 0.5912263705248020917, -0.6977439394254668636, 1.812568619595144925 ) ) ;
#118121 = CARTESIAN_POINT ( 'NONE',  ( 6.292345239091892140, -2.167472901860421519, 0.7650227848022586041 ) ) ;
#118123 = CARTESIAN_POINT ( 'NONE',  ( 4.346440162718026912, -1.840208154270198015, -0.2762933559420696072 ) ) ;
#118122 = CARTESIAN_POINT ( 'NONE',  ( -7.456058132872594335, 7.663432341298296535, 0.000000000000000000 ) ) ;
#118124 = CARTESIAN_POINT ( 'NONE',  ( 5.688527969385528849, 8.794310509995222347, -1.199719254218452047 ) ) ;
#118125 = CARTESIAN_POINT ( 'NONE',  ( -0.7500000000000006661, 11.45833333333333393, -1.299038105676657340 ) ) ;
#118126 = CARTESIAN_POINT ( 'NONE',  ( -2.324088772396477673E-16, -2.887500000000000178, -3.475000000000000089 ) ) ;
#118127 = CARTESIAN_POINT ( 'NONE',  ( -5.368138756007025947, 8.350246751061767725, 1.199719254218452047 ) ) ;
#118128 = CARTESIAN_POINT ( 'NONE',  ( -3.363224415809069612, -0.9755303453303005856, 0.7941732810802911713 ) ) ;
#118129 = CARTESIAN_POINT ( 'NONE',  ( 6.603094310190187777, -0.4545541770063685760, 2.048106021177148683 ) ) ;
#118130 = CARTESIAN_POINT ( 'NONE',  ( 5.531363484695522637, 5.555604941673978558, -0.7216878364870207285 ) ) ;
#118131 = ORIENTED_EDGE ( 'NONE', *, *, #11443, .T. ) ;
#118132 = DIRECTION ( 'NONE',  ( 1.000000000000000000, 0.000000000000000000, -0.000000000000000000 ) ) ;
#118133 = DIRECTION ( 'NONE',  ( 0.7592566023652995710, -0.6507913734559650498, 0.000000000000000000 ) ) ;
#118134 = CARTESIAN_POINT ( 'NONE',  ( 0.7151340513122245168, -0.2707656271505008982, 1.805370379145049275 ) ) ;
#118135 = CARTESIAN_POINT ( 'NONE',  ( -4.569261463005423352, 5.289558780716470565, -1.199719254218446718 ) ) ;
#118136 = CARTESIAN_POINT ( 'NONE',  ( 3.111645937125429029, 0.04567828748044086562, 1.733733899787115229 ) ) ;
#118137 = FACE_OUTER_BOUND ( 'NONE', #138580, .T. ) ;
#118138 = CARTESIAN_POINT ( 'NONE',  ( 6.509000000000010999, 0.004788705324892603143, 2.000274819378269786 ) ) ;
#118139 = CARTESIAN_POINT ( 'NONE',  ( -1.225000000000016298, 0.2708333333333532988, 0.7072540797572717253 ) ) ;
#118140 = CARTESIAN_POINT ( 'NONE',  ( 6.481070005604858686, -0.09514881109910081070, -1.823337098959529001 ) ) ;
#118141 = CARTESIAN_POINT ( 'NONE',  ( 2.869914117416060062, -1.941089286637355693, 0.2830422620509198128 ) ) ;
#118142 = CARTESIAN_POINT ( 'NONE',  ( -0.6125000000000314637, -0.2291666659838820230, -1.060881119635976200 ) ) ;
#118143 = CARTESIAN_POINT ( 'NONE',  ( -9.154780037725563702, 11.70366268214508487, 1.599625672291281386 ) ) ;
#118144 = CARTESIAN_POINT ( 'NONE',  ( 6.368579470117202490, 8.453095353268645695, 1.599625672291281386 ) ) ;
#118145 = CARTESIAN_POINT ( 'NONE',  ( 5.303433364654348559, 1.869980213031800398, -0.9998494819224086338 ) ) ;
#118146 = CARTESIAN_POINT ( 'NONE',  ( 6.373214726875630731, 9.593111727067046957, 1.199719254218452047 ) ) ;
#118147 = CARTESIAN_POINT ( 'NONE',  ( -9.622536337397040285, 12.24937836509514710, 1.599625672291281386 ) ) ;
#118148 = CIRCLE ( 'NONE', #169871, 11.09999999999999964 ) ;
#118149 = CARTESIAN_POINT ( 'NONE',  ( 2.852461952307944415, -2.064405766265942521, -0.1567919417525542591 ) ) ;
#118151 = CARTESIAN_POINT ( 'NONE',  ( -1.402160292154681736E-14, 0.3843750003414230232, 1.575800808251672791 ) ) ;
#118150 = DIRECTION ( 'NONE',  ( 0.000000000000000000, 1.000000000000000000, 0.000000000000000000 ) ) ;
#118153 = ORIENTED_EDGE ( 'NONE', *, *, #135735, .F. ) ;
#118152 = CARTESIAN_POINT ( 'NONE',  ( 5.004621511133813705, -2.204373672735039147, -0.2730638322096557435 ) ) ;
#118154 = CARTESIAN_POINT ( 'NONE',  ( 3.077065830326791929, -0.9295426453954873658, 2.102514275539566935 ) ) ;
#118155 = CARTESIAN_POINT ( 'NONE',  ( 8.758204044748010730, 9.320252261735261001, 0.7216878364870438212 ) ) ;
#118157 = CARTESIAN_POINT ( 'NONE',  ( 0.000000000000000000, -2.296874999522042327, -3.793834371823813001 ) ) ;
#118156 = CARTESIAN_POINT ( 'NONE',  ( 2.905190055078214595, 6.611415174225076186, 0.7998128361456271485 ) ) ;
#118158 = CARTESIAN_POINT ( 'NONE',  ( 1.224999999999986988, 1.645833333333327486, -0.7072540797572998139 ) ) ;
#118159 = CARTESIAN_POINT ( 'NONE',  ( -10.91033920341459051, 4.885615726745599297, 4.996448585388897357 ) ) ;
#118160 = CARTESIAN_POINT ( 'NONE',  ( -5.204170427930421283E-15, -6.268611901546719878, 10.55819884875827519 ) ) ;
#118161 = CARTESIAN_POINT ( 'NONE',  ( 3.849791259674230748, -1.322437695595569673, -1.381667681676468140 ) ) ;
#118162 = CARTESIAN_POINT ( 'NONE',  ( -11.84668730067608244, 13.50636224908218885, -1.400000000000002132 ) ) ;
#118163 = CARTESIAN_POINT ( 'NONE',  ( 4.102375631063598149, -0.5418327121037533889, -1.637530703111476305 ) ) ;
#118164 = CARTESIAN_POINT ( 'NONE',  ( 3.872279980006509970, -1.995268062538615883, -0.2910826752766728642 ) ) ;
#118165 = CARTESIAN_POINT ( 'NONE',  ( 4.219567396149206395, 2.254377101126247229, 0.4485144814023647730 ) ) ;
#118166 = CARTESIAN_POINT ( 'NONE',  ( -11.44800751629991353, 12.30000000000000071, -3.302956944461114652 ) ) ;
#118167 = CARTESIAN_POINT ( 'NONE',  ( 6.358053323650514344, 2.100580423050825818, -0.1529390103112079069 ) ) ;
#118168 = CARTESIAN_POINT ( 'NONE',  ( -5.316205630334255972, 8.255971431148344308, -1.082531754730549967 ) ) ;
#118169 = ORIENTED_EDGE ( 'NONE', *, *, #9358, .T. ) ;
#118170 = CARTESIAN_POINT ( 'NONE',  ( 5.202326708214688900, -0.5966268589385533838, -1.666288158821194187 ) ) ;
#118172 = CARTESIAN_POINT ( 'NONE',  ( 0.4458144982435990888, 0.7132466706018144587, -2.178543642160748917 ) ) ;
#118171 = CARTESIAN_POINT ( 'NONE',  ( 5.875479466675786355, 7.948088359245467416, -1.599625672291283607 ) ) ;
#118173 = CARTESIAN_POINT ( 'NONE',  ( 6.527308116070499544, -1.206667617865687214, -1.390688675169844624 ) ) ;
#118174 = CARTESIAN_POINT ( 'NONE',  ( -4.308793891044708779, 3.921347715840572956, 1.214306433183764966E-14 ) ) ;
#118175 = VECTOR ( 'NONE', #88358, 1000.000000000000000 ) ;
#118176 = CARTESIAN_POINT ( 'NONE',  ( -7.587723245503481095, 8.881373870289390737, 1.199719254218452047 ) ) ;
#118177 = CARTESIAN_POINT ( 'NONE',  ( -1.360316468750013108, -0.3281249996585910989, -3.469446951953614189E-14 ) ) ;
#118178 = LINE ( 'NONE', #183107, #160304 ) ;
#118179 = CARTESIAN_POINT ( 'NONE',  ( 0.5378411956755309031, 2.025704276806821191, -0.7818309977141599809 ) ) ;
#118180 = CARTESIAN_POINT ( 'NONE',  ( 1.516814941429758701, 0.2024661778830244008, 2.006371303556075958 ) ) ;
#118181 = CARTESIAN_POINT ( 'NONE',  ( 0.7499999999999885647, 0.01458333401615358182, 1.299038105676657340 ) ) ;
#118182 = CARTESIAN_POINT ( 'NONE',  ( 4.969325399568108814, 0.1871947810346066554, -1.917384544105669386 ) ) ;
#118183 = CARTESIAN_POINT ( 'NONE',  ( 1.364683531249996529, 12.21354166700805877, 0.7879004041258405033 ) ) ;
#118184 = CARTESIAN_POINT ( 'NONE',  ( 2.004415182159818176, -0.9449143528836713157, 2.010537586115124231 ) ) ;
#118185 = ORIENTED_EDGE ( 'NONE', *, *, #72448, .T. ) ;
#118187 = DIRECTION ( 'NONE',  ( 0.000000000000000000, 0.000000000000000000, -1.000000000000000000 ) ) ;
#118186 = FILL_AREA_STYLE_COLOUR ( '', #171933 ) ;
#118188 = CARTESIAN_POINT ( 'NONE',  ( -0.4461645575834740640, 3.167858595401910282, -1.950569735685831807 ) ) ;
#118189 = CARTESIAN_POINT ( 'NONE',  ( 7.865701674222579598, 12.32840238656838139, -0.7998128361456352531 ) ) ;
#118190 = FILL_AREA_STYLE ('',( #35798 ) ) ;
#118191 = CYLINDRICAL_SURFACE ( 'NONE', #132126, 0.3999999999999996336 ) ;
#118192 = CARTESIAN_POINT ( 'NONE',  ( 3.931004251652202353, -1.203735069864294571, -1.257276804044287655 ) ) ;
#118193 = CARTESIAN_POINT ( 'NONE',  ( 2.119516022818414669, 0.3384452847540948550, -1.932298432780136244 ) ) ;
#118195 = CARTESIAN_POINT ( 'NONE',  ( -1.364683531250012516, 3.301041667008084879, -0.7879004041258289570 ) ) ;
#118194 = CARTESIAN_POINT ( 'NONE',  ( 4.334856428067313416, 6.080418470877079429, -1.599625672291256295 ) ) ;
#118196 = CARTESIAN_POINT ( 'NONE',  ( -5.882246656098474524, 6.017915526194586917, -0.2943127404537674296 ) ) ;
#118197 = DIRECTION ( 'NONE',  ( 2.031254238220912814E-34, -1.000000000000000000, 1.301042606982605475E-17 ) ) ;
#118198 = CARTESIAN_POINT ( 'NONE',  ( 1.451709319293143396, 1.560653109857246701, 1.348772525646862341 ) ) ;
#118199 = CARTESIAN_POINT ( 'NONE',  ( -6.832419346282942563, 10.05857410638369487, 1.199719254218453823 ) ) ;
#118200 = CARTESIAN_POINT ( 'NONE',  ( -3.728129053633589152, 7.293308295973741195, 0.7216878364870317197 ) ) ;
#118201 = CARTESIAN_POINT ( 'NONE',  ( 1.446537619816448572, 2.259995149683653448, 0.1094724083178944679 ) ) ;
#118202 = ORIENTED_EDGE ( 'NONE', *, *, #137857, .F. ) ;
#118203 = CARTESIAN_POINT ( 'NONE',  ( -0.7500000000000006661, -0.3604166659838467512, -1.299038105676652011 ) ) ;
#118204 = EDGE_CURVE ( 'NONE', #97371, #57833, #99330, .T. ) ;
#118205 = CARTESIAN_POINT ( 'NONE',  ( 2.477632765499269141, 1.147360842229189437, 1.477270975257204411 ) ) ;
#118206 = CARTESIAN_POINT ( 'NONE',  ( 1.019655691060247227, -1.568448733338474455, 0.7400992899176340734 ) ) ;
#118207 = CARTESIAN_POINT ( 'NONE',  ( 5.724229345562060089, 2.111793275502030554, 0.5857118945327836057 ) ) ;
#118208 = CARTESIAN_POINT ( 'NONE',  ( 5.175001447075725736, -2.170742607874641461, -0.7831926130325519431 ) ) ;
#118209 = CARTESIAN_POINT ( 'NONE',  ( 1.358354339613274675, 0.8343398477911911915, 1.884629720726511692 ) ) ;
#118210 = CARTESIAN_POINT ( 'NONE',  ( 3.556523421261322149, -1.712991659986836002, -0.9147756334835445147 ) ) ;
#118211 = CARTESIAN_POINT ( 'NONE',  ( -3.701012746406287413, 6.301303389907177532, 1.082531754730560403 ) ) ;
#118212 = CARTESIAN_POINT ( 'NONE',  ( 6.186763334926775215, -0.2743023915687745617, -1.850177433978140051 ) ) ;
#118213 = CARTESIAN_POINT ( 'NONE',  ( 4.037125735401803084, 7.543859425723234757, -0.4173421496808590869 ) ) ;
#118214 = CARTESIAN_POINT ( 'NONE',  ( 6.679064532090532857, -0.9478974852125362505, -1.779352858464311016 ) ) ;
#118215 = CARTESIAN_POINT ( 'NONE',  ( 5.587368702607580673, 5.691220705896524734, -0.7216878364870458196 ) ) ;
#118216 = CARTESIAN_POINT ( 'NONE',  ( 1.360316468749981578, 1.744791667008098290, 0.7853790794158680422 ) ) ;
#118217 = CARTESIAN_POINT ( 'NONE',  ( 4.869767617671093340, -0.2496050341583149201, -2.000857388266870984 ) ) ;
#118218 = CARTESIAN_POINT ( 'NONE',  ( -3.212919216314315207, 5.731860938133201522, 1.082531754730560403 ) ) ;
#118219 = CARTESIAN_POINT ( 'NONE',  ( 8.718056468787178659, 10.12981962079525289, 1.199719254218462483 ) ) ;
#118220 = CARTESIAN_POINT ( 'NONE',  ( 5.388439706788500594, 5.251210844200210559, 0.7998128361456352531 ) ) ;
#118222 = CARTESIAN_POINT ( 'NONE',  ( -6.999862025036994062, -6.532648833121176501, 6.392587740394330531 ) ) ;
#118221 = CARTESIAN_POINT ( 'NONE',  ( 2.139018802738294589, -1.631172329757241801, 0.8201644002571031322 ) ) ;
#118223 = CARTESIAN_POINT ( 'NONE',  ( -4.125423880308188629, 8.035021303660014880, -0.7998128361456481317 ) ) ;
#118224 = FACE_OUTER_BOUND ( 'NONE', #48988, .T. ) ;
#118225 = CARTESIAN_POINT ( 'NONE',  ( -10.50000000000000355, 10.09158320108480744, -3.600000000000000533 ) ) ;
#118226 = ORIENTED_EDGE ( 'NONE', *, *, #205304, .F. ) ;
#118227 = CARTESIAN_POINT ( 'NONE',  ( -5.980555156959541208, 7.110307450275150210, 1.082531754730549078 ) ) ;
#118228 = ADVANCED_FACE ( 'NONE', ( #42442 ), #53437, .T. ) ;
#118229 = UNCERTAINTY_MEASURE_WITH_UNIT (LENGTH_MEASURE( 1.000000000000000082E-05 ), #53637, 'distance_accuracy_value', 'NONE');
#118230 = CARTESIAN_POINT ( 'NONE',  ( -3.735435015764967837, 4.316761258935923884, -1.199719254218452047 ) ) ;
#118231 = CARTESIAN_POINT ( 'NONE',  ( -9.671043645249580933, 10.17730576241299900, 0.7998128361456462443 ) ) ;
#118232 = CARTESIAN_POINT ( 'NONE',  ( 5.637369771878480762, -0.04735730112789998669, 2.019284605405778255 ) ) ;
#118233 = CARTESIAN_POINT ( 'NONE',  ( 0.1004478525090373164, -0.9956121213324088393, 1.872212410442177344 ) ) ;
#118234 = CARTESIAN_POINT ( 'NONE',  ( -7.096767062110449942, 7.244259425409119046, -0.7998128361456362523 ) ) ;
#118235 = CARTESIAN_POINT ( 'NONE',  ( 3.683011284406639607, 7.448596931783069586, 0.7998128361456321445 ) ) ;
#118236 = CARTESIAN_POINT ( 'NONE',  ( 4.891509840769978190, 1.525608517091806782, 1.385742337522611223 ) ) ;
#118237 = CARTESIAN_POINT ( 'NONE',  ( 5.379529795981254914, -0.4926393568372189891, -1.955173248319847845 ) ) ;
#118238 = ORIENTED_EDGE ( 'NONE', *, *, #125681, .F. ) ;
#118239 = ORIENTED_EDGE ( 'NONE', *, *, #180841, .F. ) ;
#118240 =( BOUNDED_CURVE ( )  B_SPLINE_CURVE ( 2, ( #214297, #150435, #51862, #181830, #180781, #85414, #183976 ),
 .UNSPECIFIED., .F., .T. ) 
 B_SPLINE_CURVE_WITH_KNOTS ( ( 3, 2, 2, 3 ),
 ( 0.1500000000000002165, 0.1541666666666668684, 0.1583333333333334925, 0.1625000000000001443 ),
 .UNSPECIFIED. ) 
 CURVE ( )  GEOMETRIC_REPRESENTATION_ITEM ( )  RATIONAL_B_SPLINE_CURVE ( ( 0.9999999999999928946, 0.8660254037844458130, 1.000000000000000000, 0.8660254037844387076, 1.000000000000000000, 0.8660254037844342667, 1.000000000000004441 ) ) 
 REPRESENTATION_ITEM ( '' )  );
#118241 = CARTESIAN_POINT ( 'NONE',  ( 3.570880328030153539, 7.341005539872356600, 0.2896471194287209006 ) ) ;
#118242 = CARTESIAN_POINT ( 'NONE',  ( 2.530568227245037605, 6.104080031761181857, 0.000000000000000000 ) ) ;
#118243 = CIRCLE ( 'NONE', #201169, 0.04999999999999969746 ) ;
#118245 = VERTEX_POINT ( 'NONE', #109628 ) ;
#118244 = CARTESIAN_POINT ( 'NONE',  ( -5.336015975430226099, 8.383046517047350932, -1.199719254218453823 ) ) ;
#118246 = CARTESIAN_POINT ( 'NONE',  ( 4.597299534708283453, 8.487268731053720927, 0.09294953129799360392 ) ) ;
#118247 = CARTESIAN_POINT ( 'NONE',  ( 4.569685373303983944, 1.560260980002409870, -1.276848140101802365 ) ) ;
#118248 = CARTESIAN_POINT ( 'NONE',  ( 3.046634964419430158, -1.505538468004435027, -1.059505732788845966 ) ) ;
#118249 = STYLED_ITEM ( 'NONE', ( #166222 ), #47427 ) ;
#118250 = LINE ( 'NONE', #128, #212419 ) ;
#118251 = CARTESIAN_POINT ( 'NONE',  ( 2.684532350912737009, -1.185368471958246905, 1.979860261248457931 ) ) ;
#118252 = CARTESIAN_POINT ( 'NONE',  ( 5.671053392266061977, 9.838255734277600695, 0.7998128361456331437 ) ) ;
#118253 = CARTESIAN_POINT ( 'NONE',  ( 4.886082254767631916, -1.023713625618065004, 1.903838226609423590 ) ) ;
#118254 = CARTESIAN_POINT ( 'NONE',  ( 8.422639742587595180, 10.84949900448412130, -1.599625672291268286 ) ) ;
#118255 = CARTESIAN_POINT ( 'NONE',  ( 0.1166052997346351955, -0.09441621361710265947, 1.939868080593883048 ) ) ;
#118256 = CARTESIAN_POINT ( 'NONE',  ( -6.573005544526917099, 6.562927978236513304, -0.7998128361456291469 ) ) ;
#118257 = CARTESIAN_POINT ( 'NONE',  ( -5.387385936583832802, 7.378645907471495846, -1.599625672291271394 ) ) ;
#118258 = CARTESIAN_POINT ( 'NONE',  ( 4.012460596634464416, 1.323225596166040186, -1.322536486416127977 ) ) ;
#118259 = ADVANCED_FACE ( 'NONE', ( #78107 ), #115805, .F. ) ;
#118261 = CARTESIAN_POINT ( 'NONE',  ( -4.911796789900812144, 8.952456364851418158, 0.7998128361456291469 ) ) ;
#118260 = CARTESIAN_POINT ( 'NONE',  ( 0.7499999999999885647, -0.4854166659838468623, 1.299038105676657340 ) ) ;
#118262 = CARTESIAN_POINT ( 'NONE',  ( 1.506762622594171930, -0.7967928049063888185, -2.058199171410409978 ) ) ;
#118263 = DIRECTION ( 'NONE',  ( -0.000000000000000000, -0.000000000000000000, -1.000000000000000000 ) ) ;
#118264 = CARTESIAN_POINT ( 'NONE',  ( 3.493197133815315603, 7.227147089426516402, -0.7998128361456291469 ) ) ;
#118265 = CARTESIAN_POINT ( 'NONE',  ( -3.588104209110990706, 7.337872010604796991, 1.040834085586084257E-14 ) ) ;
#118266 = CARTESIAN_POINT ( 'NONE',  ( -8.068510813464099485, 8.585886501895810596, 0.7216878364870317197 ) ) ;
#118267 = CARTESIAN_POINT ( 'NONE',  ( 0.6847650648834556764, -0.2371060910116972453, -1.956967405937762639 ) ) ;
#118268 = CARTESIAN_POINT ( 'NONE',  ( 6.287736656369789401, 1.586309881779718323, 1.676255113901073512 ) ) ;
#118269 = CARTESIAN_POINT ( 'NONE',  ( 1.697631272820496307, -1.418720726069604865, -1.355276769646639901 ) ) ;
#118270 = CARTESIAN_POINT ( 'NONE',  ( 4.082923458916259740, 1.956979318386397715, 0.6515942777399350572 ) ) ;
#118271 = CARTESIAN_POINT ( 'NONE',  ( 6.656690234629796699, 6.868486149930637552, 1.040834085586084257E-14 ) ) ;
#118272 = CARTESIAN_POINT ( 'NONE',  ( 6.692885107001518286, 7.837396042037102717, -1.199719254218452047 ) ) ;
#118273 = VERTEX_POINT ( 'NONE', #26154 ) ;
#118274 = CARTESIAN_POINT ( 'NONE',  ( 6.575341312503417690, 10.61505593132193326, -0.7216878364870267237 ) ) ;
#118275 = CARTESIAN_POINT ( 'NONE',  ( 1.364683531249988535, 4.467708333674754506, -0.7879004041258300672 ) ) ;
#118276 = CARTESIAN_POINT ( 'NONE',  ( 11.84668730067608600, 12.69999999999999929, -1.400000000000001910 ) ) ;
#118277 = CARTESIAN_POINT ( 'NONE',  ( 4.080641047588898118, 5.783833860318930320, -1.443375672974051449 ) ) ;
#118278 = CARTESIAN_POINT ( 'NONE',  ( 6.725048307591657171, -1.982231927674932948, -0.8863045971672071088 ) ) ;
#118280 = CARTESIAN_POINT ( 'NONE',  ( 6.075717905342373548, -0.9791751913862613010, 1.559117742379905858 ) ) ;
#118279 = CARTESIAN_POINT ( 'NONE',  ( -15.75000000000000000, 9.799999999999982947, 3.199999999999997957 ) ) ;
#118281 = CARTESIAN_POINT ( 'NONE',  ( 10.50000000000000178, 10.19999999999998153, 3.599999999999999201 ) ) ;
#118282 = CARTESIAN_POINT ( 'NONE',  ( -11.91826849282518452, 12.69999999999999929, -1.400000000000001465 ) ) ;
#118283 = CARTESIAN_POINT ( 'NONE',  ( 1.071320448993583918, 1.804315561281001123, -0.4931735697189034151 ) ) ;
#118284 = CARTESIAN_POINT ( 'NONE',  ( -6.041716223103725802, 6.056113169402001617, -0.5645603026655892087 ) ) ;
#118285 = CARTESIAN_POINT ( 'NONE',  ( -0.3999999999999003797, 3.087878369845980853, -2.023857702507796397 ) ) ;
#118286 = CARTESIAN_POINT ( 'NONE',  ( 6.562153376633583335, 6.794832157118596783, -0.3727171428496069971 ) ) ;
#118287 = CARTESIAN_POINT ( 'NONE',  ( -1.001543065824772872E-14, 5.634375000341415252, 1.575800808251672791 ) ) ;
#118288 = CARTESIAN_POINT ( 'NONE',  ( 1.312987857083922627, 1.562780923097413677, -1.101767902142808175 ) ) ;
#118289 = CARTESIAN_POINT ( 'NONE',  ( 3.010364070732887143, 1.283045204736869671, -1.219329851163194922 ) ) ;
#118290 = CARTESIAN_POINT ( 'NONE',  ( 0.6449871831117168774, 0.1410837285014763798, 1.907147727228817757 ) ) ;
#118292 = CARTESIAN_POINT ( 'NONE',  ( 4.692942998425689183, 1.668811738553135804, 0.9403632788237480389 ) ) ;
#118291 = CARTESIAN_POINT ( 'NONE',  ( -10.65400978224035811, 11.32409958890225710, 1.040834085586084257E-14 ) ) ;
#118293 = PLANE ( 'NONE',  #140182 ) ;
#118294 = CARTESIAN_POINT ( 'NONE',  ( 4.861744415569490663, -0.5273948137594737240, 1.897533870164061831 ) ) ;
#118295 = CARTESIAN_POINT ( 'NONE',  ( 1.283610819548046011, 0.1505422781087061845, -2.115291873224629082 ) ) ;
#118296 = CARTESIAN_POINT ( 'NONE',  ( 0.000000000000000000, 3.000000000000002665, 0.000000000000000000 ) ) ;
#118297 = CARTESIAN_POINT ( 'NONE',  ( 4.416781281874038179, 1.710313510141375115, 0.7581657270378170388 ) ) ;
#118299 = ORIENTED_EDGE ( 'NONE', *, *, #169097, .F. ) ;
#118298 = CARTESIAN_POINT ( 'NONE',  ( 0.06470675514189982991, -1.629034059718449834, -0.8243793580787887043 ) ) ;
#118301 = CARTESIAN_POINT ( 'NONE',  ( 4.067082894419602468, 3.847277586352047862, -0.7216878364870188411 ) ) ;
#118300 = CARTESIAN_POINT ( 'NONE',  ( 3.774219598512587037, 1.225428716765289749, 1.835190637982798023 ) ) ;
#118302 = CARTESIAN_POINT ( 'NONE',  ( 1.364683531249988535, 4.467708333674754506, -0.7879004041258300672 ) ) ;
#118303 = CARTESIAN_POINT ( 'NONE',  ( 0.4321753131953905980, 1.186194839137414414, 1.687308244272892166 ) ) ;
#118304 = CARTESIAN_POINT ( 'NONE',  ( 5.425234023762710578, 9.481190127698507553, -0.7998128361456291469 ) ) ;
#118305 = CARTESIAN_POINT ( 'NONE',  ( -8.962103233833181193, 10.41454084668224489, -1.199719254218446718 ) ) ;
#118306 = CARTESIAN_POINT ( 'NONE',  ( -9.193915077888615173, 15.44694766967490551, -7.646183055905130921 ) ) ;
#118307 = CARTESIAN_POINT ( 'NONE',  ( -3.423586633568784787, -0.02128689224817647760, -0.4190252743465633922 ) ) ;
#118308 = VECTOR ( 'NONE', #70991, 1000.000000000000000 ) ;
#118309 = CARTESIAN_POINT ( 'NONE',  ( -4.610264723183647995, 8.173666352459294515, -0.5982188967808210744 ) ) ;
#118310 = ORIENTED_EDGE ( 'NONE', *, *, #112082, .T. ) ;
#118311 = CARTESIAN_POINT ( 'NONE',  ( 2.980987059868035693, 1.948563265827065960, 0.6999735360200682877 ) ) ;
#118312 = CARTESIAN_POINT ( 'NONE',  ( 0.7499999999999902300, 4.316666666666691299, -1.299038105676658228 ) ) ;
#118313 = CARTESIAN_POINT ( 'NONE',  ( 1.616726252867954683, 1.452999108549270169, -1.600537328674697779 ) ) ;
#118314 = CARTESIAN_POINT ( 'NONE',  ( -6.419454189569741231, 6.887487763818779918, 0.7628848663763813098 ) ) ;
#118315 = CARTESIAN_POINT ( 'NONE',  ( 0.4518267731568551548, -1.429874679360541023, -1.426642250087527541 ) ) ;
#118316 = PRESENTATION_STYLE_ASSIGNMENT (( #85752 ) ) ;
#118317 = EDGE_LOOP ( 'NONE', ( #183282, #31489, #65879, #17482 ) ) ;
#118319 = CARTESIAN_POINT ( 'NONE',  ( 8.758204044748010730, 9.320252261735261001, 0.7216878364870438212 ) ) ;
#118318 = CARTESIAN_POINT ( 'NONE',  ( 0.1749903794560566661, 7.629137130509112907, -2.555305779167945435 ) ) ;
#118320 = CARTESIAN_POINT ( 'NONE',  ( 6.661482485103542572, -0.5350097378542042481, -1.943772860543022230 ) ) ;
#118321 = CARTESIAN_POINT ( 'NONE',  ( 5.630082600720735186, 1.913861949906026538, 0.08686293782892740012 ) ) ;
#118322 = CARTESIAN_POINT ( 'NONE',  ( 6.539320575229294441, -0.001643797937642132567, 2.203502507913539521 ) ) ;
#118323 = CARTESIAN_POINT ( 'NONE',  ( 3.632539538618652752, 0.3231117836275977373, 2.167502126216628522 ) ) ;
#118324 = CARTESIAN_POINT ( 'NONE',  ( 1.499999999999989120, 2.806250000682818158, 1.214306433183764966E-14 ) ) ;
#118325 = CARTESIAN_POINT ( 'NONE',  ( 3.181800181368432678, 1.864768544494728175, -0.4233684943922080834 ) ) ;
#118326 = CARTESIAN_POINT ( 'NONE',  ( -3.879604511804807032, 7.677955697080923514, 0.7998128361456341429 ) ) ;
#118328 = CARTESIAN_POINT ( 'NONE',  ( 3.836594282542909795, 6.459481848733281240, 1.082531754730558626 ) ) ;
#118327 = B_SPLINE_CURVE_WITH_KNOTS ( 'NONE', 3,
 ( #187423, #4377, #101916, #85660 ),
 .UNSPECIFIED., .F., .F.,
 ( 4, 4 ),
 ( 0.0006956056399114353287, 0.0009226328642097691209 ),
 .UNSPECIFIED. ) ;
#118330 = CARTESIAN_POINT ( 'NONE',  ( 1.054314798682391530, -1.277026470193865171, 1.560515422851154854 ) ) ;
#118329 = CARTESIAN_POINT ( 'NONE',  ( -8.907343734053998929, 12.37535620882957588, 1.082531754730558626 ) ) ;
#118331 = CARTESIAN_POINT ( 'NONE',  ( 1.364683531249997417, 11.04687500034139802, 2.602085213965210642E-15 ) ) ;
#118333 = CARTESIAN_POINT ( 'NONE',  ( -4.197131071882288289, 7.054347462908075350, -1.199719254218455378 ) ) ;
#118332 = CARTESIAN_POINT ( 'NONE',  ( -0.04093971525966337566, -2.051586291785143512, -1.022954789973041123 ) ) ;
#118335 = ORIENTED_EDGE ( 'NONE', *, *, #59714, .F. ) ;
#118334 = CARTESIAN_POINT ( 'NONE',  ( 3.873808679987042147, 0.9582704680195216485, 1.433834079761304281 ) ) ;
#118336 = CARTESIAN_POINT ( 'NONE',  ( -0.1399997263889612154, 1.357298622859518078, -2.254419820505838334 ) ) ;
#118337 = CARTESIAN_POINT ( 'NONE',  ( 8.067265095331215718, 9.370563018429956870, 1.199719254218462483 ) ) ;
#118338 = CARTESIAN_POINT ( 'NONE',  ( 5.359550796103802028, 5.147230771742885125, -0.7998128361456231517 ) ) ;
#118339 = VECTOR ( 'NONE', #189782, 1000.000000000000000 ) ;
#118340 = DIRECTION ( 'NONE',  ( 1.000000000000000000, 0.000000000000000000, 0.000000000000000000 ) ) ;
#118341 = CARTESIAN_POINT ( 'NONE',  ( 1.609737659951641309, 0.5726723138891121057, -1.876404140693301414 ) ) ;
#118342 = FACE_OUTER_BOUND ( 'NONE', #100430, .T. ) ;
#118343 = CARTESIAN_POINT ( 'NONE',  ( 4.493637847925535667, 7.329995691633395261, -1.199719254218452047 ) ) ;
#118344 = CARTESIAN_POINT ( 'NONE',  ( 0.07536363704235825300, -0.001874865094115065866, -2.144269471569634433 ) ) ;
#118345 = ORIENTED_EDGE ( 'NONE', *, *, #93378, .F. ) ;
#118346 = ORIENTED_EDGE ( 'NONE', *, *, #145457, .T. ) ;
#118347 = CARTESIAN_POINT ( 'NONE',  ( 4.143061475816012695, 0.09292765117045087564, 1.809223169447377710 ) ) ;
#118348 = VERTEX_POINT ( 'NONE', #108546 ) ;
#118349 = CARTESIAN_POINT ( 'NONE',  ( 4.830447868218803897, 8.857549289555754157, -0.7998128361456481317 ) ) ;
#118350 = CARTESIAN_POINT ( 'NONE',  ( 3.627688620108284745, 6.389997935838436227, 1.199719254218452047 ) ) ;
#118351 = CARTESIAN_POINT ( 'NONE',  ( 5.479120714502029976, -1.640381486070506156, -0.7687909062009666838 ) ) ;
#118352 = CARTESIAN_POINT ( 'NONE',  ( 4.841670253411575864, 8.662716039039905169, -0.7216878364870458196 ) ) ;
#118353 = CARTESIAN_POINT ( 'NONE',  ( -11.92051736251532112, 9.948197562073211486, -1.381800029228967386 ) ) ;
#118354 = CARTESIAN_POINT ( 'NONE',  ( 5.587453275722374713, 6.167276584799368244, -0.8733612469495740660 ) ) ;
#118355 = EDGE_CURVE ( 'NONE', #194084, #79317, #144234, .T. ) ;
#118357 = CARTESIAN_POINT ( 'NONE',  ( 8.703444544968814256, 12.24143683818393313, -1.199719254218446718 ) ) ;
#118356 = CARTESIAN_POINT ( 'NONE',  ( 5.705462897529653965, -1.467230705000615032, -1.144726319735862585 ) ) ;
#118358 = CARTESIAN_POINT ( 'NONE',  ( 3.251485182540703622, 1.868192404686802810, -0.4227579483004426653 ) ) ;
#118359 = FACE_OUTER_BOUND ( 'NONE', #112486, .T. ) ;
#118360 = CARTESIAN_POINT ( 'NONE',  ( -12.04410816989902955, 7.377574010548016759, -3.959763750030863783 ) ) ;
#118361 = CARTESIAN_POINT ( 'NONE',  ( -10.99949329275129450, -9.914220445327725173, 0.1055954338740902887 ) ) ;
#118362 = CARTESIAN_POINT ( 'NONE',  ( 5.341549334104176872, 9.175631956522799726, 0.7216878364870438212 ) ) ;
#118363 = CARTESIAN_POINT ( 'NONE',  ( -3.898132859128961236, 4.506575409527250997, -1.199719254218452047 ) ) ;
#118364 = CARTESIAN_POINT ( 'NONE',  ( 1.077287230265553175, -0.05381693868444263618, -2.161191418701657430 ) ) ;
#118365 = CARTESIAN_POINT ( 'NONE',  ( -6.622231685632140596, 6.690634819517756959, 0.000000000000000000 ) ) ;
#118366 = ADVANCED_FACE ( 'NONE', ( #92268 ), #146857, .T. ) ;
#118367 = CARTESIAN_POINT ( 'NONE',  ( 6.229045230835819069, 6.231917288922055320, -0.7998128361456481317 ) ) ;
#118368 = CARTESIAN_POINT ( 'NONE',  ( 0.6920833903016985200, -1.811158644599793810, -0.2285449354127722099 ) ) ;
#118369 = CARTESIAN_POINT ( 'NONE',  ( -4.985647801523292344, 6.839675073242382553, -1.599625672291256295 ) ) ;
#118370 = CARTESIAN_POINT ( 'NONE',  ( 3.223480179809079971, -1.759765543241718966, 0.4855387900214308550 ) ) ;
#118371 = CARTESIAN_POINT ( 'NONE',  ( 9.906083622534509914, -9.418601272609043562, -0.1729113328156559048 ) ) ;
#118372 = CARTESIAN_POINT ( 'NONE',  ( 2.144650067465687648, 1.855875215511919363, 0.4610605321611755958 ) ) ;
#118373 = CARTESIAN_POINT ( 'NONE',  ( 3.262113425008953183, -1.967426182293503079, 0.09390151542597660606 ) ) ;
#118374 = CARTESIAN_POINT ( 'NONE',  ( 3.456523497251274168, -1.714022962016878759, -0.9130526778427237033 ) ) ;
#118375 = CARTESIAN_POINT ( 'NONE',  ( -5.178288325776719603, 5.006034233019745372, 0.000000000000000000 ) ) ;
#118377 = CARTESIAN_POINT ( 'NONE',  ( 4.148766697842418694, 2.080301416381886703, 0.4105806053946169376 ) ) ;
#118376 = CARTESIAN_POINT ( 'NONE',  ( 5.833751235630055376, 10.02806988486892514, 0.7998128361456331437 ) ) ;
#118378 = CARTESIAN_POINT ( 'NONE',  ( 0.04234008746931722245, -7.776896528353615778, 9.555169238417180466 ) ) ;
#118379 = CARTESIAN_POINT ( 'NONE',  ( 9.423080456697809026, 10.95234760669099749, -1.199719254218446718 ) ) ;
#118380 = CARTESIAN_POINT ( 'NONE',  ( 6.082781304119575516, 6.035783188292461077, -0.3281998023207943760 ) ) ;
#118381 = CARTESIAN_POINT ( 'NONE',  ( -2.788906526875773208E-15, 11.71875000068279604, -1.499999999999998446 ) ) ;
#118382 = EDGE_LOOP ( 'NONE', ( #91908, #17183, #115572, #2336, #171811, #160481, #108230, #87915 ) ) ;
#118383 = CARTESIAN_POINT ( 'NONE',  ( 5.118366684358879759, 5.930181538962194132, 1.199719254218462483 ) ) ;
#118384 = CARTESIAN_POINT ( 'NONE',  ( 4.227110032410640095, 8.153655147779589996, 0.7998128361456271485 ) ) ;
#118385 = CARTESIAN_POINT ( 'NONE',  ( 11.97297122925974122, 12.30125079326911575, -0.8121202983519294483 ) ) ;
#118386 = CARTESIAN_POINT ( 'NONE',  ( 3.879382553896340013, 1.718498013671100777, -0.6167319420108534622 ) ) ;
#118387 = CARTESIAN_POINT ( 'NONE',  ( 0.2534910766302467255, 3.934660213246443661, -11.56267633880226775 ) ) ;
#118388 = CARTESIAN_POINT ( 'NONE',  ( -9.490344339885981029, 10.17441593939621924, -0.7216878364870267237 ) ) ;
#118389 =( GEOMETRIC_REPRESENTATION_CONTEXT ( 3 ) GLOBAL_UNCERTAINTY_ASSIGNED_CONTEXT ( ( #60868 ) ) GLOBAL_UNIT_ASSIGNED_CONTEXT ( ( #184179, #99743, #150644 ) ) REPRESENTATION_CONTEXT ( 'NONE', 'WORKASPACE' ) );
#118390 = CARTESIAN_POINT ( 'NONE',  ( -5.569768141569340969, 7.516503378918355516, 1.348759926630802131 ) ) ;
#118391 = DIRECTION ( 'NONE',  ( -0.000000000000000000, 1.000000000000000000, -0.000000000000000000 ) ) ;
#118392 = CARTESIAN_POINT ( 'NONE',  ( 4.803500792215161574, -0.4985019455652460740, 1.802925825644098534 ) ) ;
#118393 = CARTESIAN_POINT ( 'NONE',  ( 7.019370843573166319, 9.212351955633947043, 1.599625672291281386 ) ) ;
#118394 = AXIS2_PLACEMENT_3D ( 'NONE', #71649, #203783, #188622 ) ;
#118396 = EDGE_CURVE ( 'NONE', #53788, #59826, #36110, .T. ) ;
#118395 = CARTESIAN_POINT ( 'NONE',  ( 3.457566480858861091, 0.4672022665876771619, -1.868877010067309330 ) ) ;
#118397 = CARTESIAN_POINT ( 'NONE',  ( 2.886471042457359637, 6.589576326167374098, -0.3044456787500351980 ) ) ;
#118398 = CARTESIAN_POINT ( 'NONE',  ( 5.217190183160311356, 4.981143389975473568, -0.7998128361456211532 ) ) ;
#118399 = CARTESIAN_POINT ( 'NONE',  ( -0.6823417656250039265, 8.880208333674733723, -1.181850606188755259 ) ) ;
#118400 = CARTESIAN_POINT ( 'NONE',  ( -5.391338639728555648, 9.441645512991978961, -0.7998128361456231517 ) ) ;
#118401 = CARTESIAN_POINT ( 'NONE',  ( 3.277320446201373638, 4.846626492033466072, 1.599625672291267398 ) ) ;
#118402 = CARTESIAN_POINT ( 'NONE',  ( -5.908321080505254841, 10.11506803722328129, 0.7998128361456291469 ) ) ;
#118403 = CARTESIAN_POINT ( 'NONE',  ( 1.019337291899083064, -1.912195925978699140, 0.9092529662874779817 ) ) ;
#118404 = CARTESIAN_POINT ( 'NONE',  ( 9.023114925094663619, 10.48572115315399245, 1.199719254218453823 ) ) ;
#118406 = EDGE_CURVE ( 'NONE', #54210, #159016, #160742, .T. ) ;
#118405 = CARTESIAN_POINT ( 'NONE',  ( -1.499999999999997780, 3.650000000000021227, 1.214306433183764966E-14 ) ) ;
#118407 = CARTESIAN_POINT ( 'NONE',  ( 6.702015291077846548, 0.7979701500827086624, -1.910492173269620508 ) ) ;
#118410 = B_SPLINE_CURVE_WITH_KNOTS ( 'NONE', 3,
 ( #138219, #58018, #88394, #91619, #125241, #55884, #154461, #9267, #56956, #6039 ),
 .UNSPECIFIED., .F., .F.,
 ( 4, 3, 3, 4 ),
 ( 0.000000000000000000, 3.125302649357442460E-05, 8.414501133366901735E-05, 0.0001371975721651944632 ),
 .UNSPECIFIED. ) ;
#118409 = CARTESIAN_POINT ( 'NONE',  ( 4.260617097460324132, 7.265790484119571957, -0.9368387426427534637 ) ) ;
#118408 = CARTESIAN_POINT ( 'NONE',  ( 1.575478407343299692, -0.9843019613302635973, 1.555867251595323353 ) ) ;
#118411 = CARTESIAN_POINT ( 'NONE',  ( 0.1464030204712711281, -0.1495716826577230818, -2.263613701224455710 ) ) ;
#118412 = CARTESIAN_POINT ( 'NONE',  ( 5.504247177468179153, 7.444707678511436555, 1.443375672974062551 ) ) ;
#118414 = CARTESIAN_POINT ( 'NONE',  ( -1.115562610750309283E-14, 9.593750000682799595, 1.500000000000001554 ) ) ;
#118413 = CARTESIAN_POINT ( 'NONE',  ( 3.119784744920330422, 6.653849612466795627, 0.7216878364870257245 ) ) ;
#118415 = CARTESIAN_POINT ( 'NONE',  ( 1.060933235008169051, -2.074266264760935563, -0.9759354127518887756 ) ) ;
#118416 = EDGE_CURVE ( 'NONE', #167392, #103946, #73617, .T. ) ;
#118417 = CARTESIAN_POINT ( 'NONE',  ( 5.841732304440537149, 1.939831336911639781, 0.09320031894976579800 ) ) ;
#118418 = EDGE_LOOP ( 'NONE', ( #63682, #77050, #48762, #62865 ) ) ;
#118419 = CARTESIAN_POINT ( 'NONE',  ( 9.232739420781973294, 9.873876867108206667, -0.7216878364870257245 ) ) ;
#118420 =( BOUNDED_CURVE ( )  B_SPLINE_CURVE ( 2, ( #162067, #79729, #81861, #212917, #145845, #211852, #63488 ),
 .UNSPECIFIED., .F., .T. ) 
 B_SPLINE_CURVE_WITH_KNOTS ( ( 3, 2, 2, 3 ),
 ( 0.1874999999999999167, 0.1916666666666665964, 0.1958333333333332760, 0.1999999999999999556 ),
 .UNSPECIFIED. ) 
 CURVE ( )  GEOMETRIC_REPRESENTATION_ITEM ( )  RATIONAL_B_SPLINE_CURVE ( ( 1.000000000000002665, 0.8660254037844360431, 1.000000000000000000, 0.8660254037844387076, 1.000000000000000000, 0.8660254037844404840, 0.9999999999999982236 ) ) 
 REPRESENTATION_ITEM ( '' )  );
#118421 = CARTESIAN_POINT ( 'NONE',  ( 0.6506401683969212923, 1.984111478139438667, 0.3401018483101604928 ) ) ;
#118422 = CARTESIAN_POINT ( 'NONE',  ( -0.08058608058608696112, -5.907420853759267843, 10.99970480893081870 ) ) ;
#118424 = LINE ( 'NONE', #168178, #157362 ) ;
#118423 = CARTESIAN_POINT ( 'NONE',  ( -9.040589502214116280, 9.441775928871617651, 0.7998128361456462443 ) ) ;
#118425 = CARTESIAN_POINT ( 'NONE',  ( -10.10575425844435138, 4.358269247758318699, 5.859476710806498900 ) ) ;
#118427 = CARTESIAN_POINT ( 'NONE',  ( 2.746659024021454787, -1.472625519509669134, 0.9813492100937453166 ) ) ;
#118426 = CARTESIAN_POINT ( 'NONE',  ( 4.382818795122591204, 1.867623683829922054, -0.9396962251831328938 ) ) ;
#118428 = CARTESIAN_POINT ( 'NONE',  ( -11.10517813317449054, 1.720726420432414860, 4.015189785735357120 ) ) ;
#118430 = CARTESIAN_POINT ( 'NONE',  ( 4.892671604017262865, 1.907728271999886704, -1.270570218630202808 ) ) ;
#118429 = CARTESIAN_POINT ( 'NONE',  ( -11.39025776735688211, 6.535114720142842337, -3.782060309780574947 ) ) ;
#118431 = CARTESIAN_POINT ( 'NONE',  ( 3.855166295008194410, 1.726882014201753801, -0.2153026951989250037 ) ) ;
#118432 = CARTESIAN_POINT ( 'NONE',  ( 9.378489572351044856, 11.96465713920816043, -1.599625672291262513 ) ) ;
#118433 =( GEOMETRIC_REPRESENTATION_CONTEXT ( 3 ) GLOBAL_UNCERTAINTY_ASSIGNED_CONTEXT ( ( #47300 ) ) GLOBAL_UNIT_ASSIGNED_CONTEXT ( ( #129018, #88723, #6365 ) ) REPRESENTATION_CONTEXT ( 'NONE', 'WORKASPACE' ) );
#118434 = CARTESIAN_POINT ( 'NONE',  ( 6.235824307642648279, 6.239826211863360506, 0.000000000000000000 ) ) ;
#118435 = CARTESIAN_POINT ( 'NONE',  ( 3.180671111220879865, -0.8518272437034493105, -1.510038686645834183 ) ) ;
#118436 = CARTESIAN_POINT ( 'NONE',  ( 3.824824921856139870, -1.460638251479762229, 1.606552252625459420 ) ) ;
#118437 = CARTESIAN_POINT ( 'NONE',  ( 5.443762371086860341, 6.309809840144842141, 1.199719254218462483 ) ) ;
#118438 = CARTESIAN_POINT ( 'NONE',  ( 4.241422899474024177, 0.4370803545316758743, -1.968444674787086512 ) ) ;
#118439 = CARTESIAN_POINT ( 'NONE',  ( 1.343750000000001110, 1.895863743164117654, 0.7852924748299160429 ) ) ;
#118440 = CARTESIAN_POINT ( 'NONE',  ( -1.201851678989727383E-14, 3.743750000682817269, 1.732050807568877637 ) ) ;
#118441 = CARTESIAN_POINT ( 'NONE',  ( 1.940333228260374021, 1.905070304733847752, 0.2851023952017122665 ) ) ;
#118442 = CARTESIAN_POINT ( 'NONE',  ( 1.500000000000001332, 8.906250000682797818, 0.000000000000000000 ) ) ;
#118443 = CARTESIAN_POINT ( 'NONE',  ( 6.029551324705815674, -0.2728526602329122142, 2.204496564233568989 ) ) ;
#118444 = ORIENTED_EDGE ( 'NONE', *, *, #63237, .T. ) ;
#118445 = CARTESIAN_POINT ( 'NONE',  ( -0.2106854629475244378, 7.629137130509075604, -2.597154134060948749 ) ) ;
#118446 = CARTESIAN_POINT ( 'NONE',  ( 1.499999999999989120, 2.254166666666685970, 0.8660254037844524744 ) ) ;
#118447 = CARTESIAN_POINT ( 'NONE',  ( 5.601490020740366838, 9.686822124172440596, 1.040834085586084257E-14 ) ) ;
#118448 = CARTESIAN_POINT ( 'NONE',  ( 3.836594282542909795, 6.459481848733281240, 1.082531754730558626 ) ) ;
#118449 = CARTESIAN_POINT ( 'NONE',  ( 1.642778471875000035, -2.326041666188709112, -2.845375778867859751 ) ) ;
#118450 = CARTESIAN_POINT ( 'NONE',  ( 1.137687779795238052, -0.04954009815814026940, 2.220905934856795216 ) ) ;
#118451 = CARTESIAN_POINT ( 'NONE',  ( 5.898874287966751950, 0.3812104124719677412, 1.924297140916144455 ) ) ;
#118452 = CARTESIAN_POINT ( 'NONE',  ( 7.863365906246055914, 10.19701286208565705, -1.443375672974057666 ) ) ;
#118453 = CARTESIAN_POINT ( 'NONE',  ( -0.2822871844487425119, 3.300644403538278038, 1.982554686319321302 ) ) ;
#118454 = CARTESIAN_POINT ( 'NONE',  ( 6.468092748254181679, 1.154776641680499205, 1.945382213218769252 ) ) ;
#118455 = COLOUR_RGB ( '', 0.08235294, 0.09019608, 0.10196078) ;
#118456 = CARTESIAN_POINT ( 'NONE',  ( 5.876533236880477240, 5.820653295974182129, 0.7998128361456352531 ) ) ;
#118457 = CARTESIAN_POINT ( 'NONE',  ( -4.014622883422322985, 7.697827440719083647, -0.7216878364870458196 ) ) ;
#118458 = CARTESIAN_POINT ( 'NONE',  ( 4.510253362402360189, 2.062282729996979924, -0.04753222776765659435 ) ) ;
#118459 = CARTESIAN_POINT ( 'NONE',  ( -5.148345644887285744, 7.029489223833707001, -1.599625672291256295 ) ) ;
#118460 = CARTESIAN_POINT ( 'NONE',  ( -1.001543065824772872E-14, 4.243750000682819490, 1.732050807568877637 ) ) ;
#118461 = CARTESIAN_POINT ( 'NONE',  ( 0.6823417656249899377, 5.238541667008086655, -1.181850606188754593 ) ) ;
#118462 = CARTESIAN_POINT ( 'NONE',  ( 5.817618194842751222, -1.825074353437942554, 0.4092329068215995180 ) ) ;
#118463 = CARTESIAN_POINT ( 'NONE',  ( 5.010307813345768579, -1.644221866518974728, 0.5513857468827707553 ) ) ;
#118464 = CARTESIAN_POINT ( 'NONE',  ( 3.315673178333057969, 1.101538733106369072, -1.347505558334564535 ) ) ;
#118465 = CARTESIAN_POINT ( 'NONE',  ( 9.747949258101261449, 11.43532422494874368, -1.082531754730537088 ) ) ;
#118466 = CARTESIAN_POINT ( 'NONE',  ( 1.611265326866499148, -0.2753845699034764838, 2.275703152891339176 ) ) ;
#118467 = CARTESIAN_POINT ( 'NONE',  ( 0.6823417656249899377, 3.738541667008085767, -1.181850606188754593 ) ) ;
#118468 = CARTESIAN_POINT ( 'NONE',  ( 6.181206942494069878, 1.442326931096184151, 1.513799708994074900 ) ) ;
#118469 = CARTESIAN_POINT ( 'NONE',  ( 0.5679803739370090643, -1.732728882149033645, -0.6228371021387222317 ) ) ;
#118470 = CARTESIAN_POINT ( 'NONE',  ( -0.01979919457417661857, -6.863887352872468206, 9.496663240426189034 ) ) ;
#118471 = FILL_AREA_STYLE_COLOUR ( '', #204094 ) ;
#118472 = CARTESIAN_POINT ( 'NONE',  ( 2.145157927413956944, 0.8647252629472859109, 1.821741647932619390 ) ) ;
#118473 = CARTESIAN_POINT ( 'NONE',  ( 0.006183538434290089709, -0.9405624870862171472, -1.977291442860461768 ) ) ;
#118474 = CARTESIAN_POINT ( 'NONE',  ( 9.167499922608561391, 13.31163428502020452, -9.058864735568997517 ) ) ;
#118475 = CARTESIAN_POINT ( 'NONE',  ( -6.906989191158078079, 10.14557225873805812, -1.199719254218440723 ) ) ;
#118476 = CARTESIAN_POINT ( 'NONE',  ( 5.524057522564145728, 8.532151978711786100, 1.199719254218462483 ) ) ;
#118477 = CARTESIAN_POINT ( 'NONE',  ( 2.860144583491229131, 0.7611018733697445526, -1.979373954265637892 ) ) ;
#118478 = CARTESIAN_POINT ( 'NONE',  ( 1.364683531249986537, -0.6364583329919177856, 0.7879004041258500513 ) ) ;
#118479 = CARTESIAN_POINT ( 'NONE',  ( 5.320859459983126705, 1.688362619374352613, 0.6951667914897319278 ) ) ;
#118480 = ORIENTED_EDGE ( 'NONE', *, *, #191207, .F. ) ;
#118481 = CARTESIAN_POINT ( 'NONE',  ( -6.363572996767778100, 8.517530811019446091, -1.599625672291271394 ) ) ;
#118482 = EDGE_CURVE ( 'NONE', #187007, #153475, #123760, .T. ) ;
#118483 = DIRECTION ( 'NONE',  ( -1.000000000000000000, 0.000000000000000000, -8.638326563840826660E-31 ) ) ;
#118484 = CARTESIAN_POINT ( 'NONE',  ( -3.285556943750000514, -0.9260416661887070910, -1.896917185911906500 ) ) ;
#118485 = CARTESIAN_POINT ( 'NONE',  ( -5.636439174979254396, 7.598931675607687453, -1.599625672291256295 ) ) ;
#118486 = CARTESIAN_POINT ( 'NONE',  ( 2.004171506046021012, -0.8596719693435939114, 1.827822491074476918 ) ) ;
#118487 = CARTESIAN_POINT ( 'NONE',  ( 0.2531349071235571846, -1.691105571228457505, 1.254881668439677966 ) ) ;
#118488 = VECTOR ( 'NONE', #114990, 1000.000000000000000 ) ;
#118489 = CARTESIAN_POINT ( 'NONE',  ( -3.902768115887413014, 5.646591783325653147, -1.599625672291283607 ) ) ;
#118490 = CARTESIAN_POINT ( 'NONE',  ( 4.012436097835626825, 0.6663421089948203813, 1.737758261286206807 ) ) ;
#118491 = CARTESIAN_POINT ( 'NONE',  ( 8.890396042259068210, 11.39521468743417998, -1.599625672291257406 ) ) ;
#118492 = CARTESIAN_POINT ( 'NONE',  ( 2.970157261343746580, 6.585292010301047938, 0.4235207732182846851 ) ) ;
#118493 = ORIENTED_EDGE ( 'NONE', *, *, #178012, .T. ) ;
#118494 = B_SPLINE_CURVE_WITH_KNOTS ( 'NONE', 3,
 ( #133261, #199268, #50912, #117040, #63965, #80212, #119165, #39998, #56241, #154809 ),
 .UNSPECIFIED., .F., .F.,
 ( 4, 3, 3, 4 ),
 ( 7.467508872541053688E-17, 3.125178967435692016E-05, 6.527220184319362914E-05, 9.930990297292533473E-05 ),
 .UNSPECIFIED. ) ;
#118495 = CARTESIAN_POINT ( 'NONE',  ( -4.627410500965859264, 4.293067094081919777, 0.7998128361456341429 ) ) ;
#118496 = CARTESIAN_POINT ( 'NONE',  ( -7.914208982075130905, 10.25632978388623684, -1.599625672291263179 ) ) ;
#118498 = CARTESIAN_POINT ( 'NONE',  ( -4.095724654357025152, 7.689947244493171574, 0.7385042830605083042 ) ) ;
#118497 = CARTESIAN_POINT ( 'NONE',  ( -7.273023059088104425, 7.449891421883056530, 0.000000000000000000 ) ) ;
#118499 = CARTESIAN_POINT ( 'NONE',  ( -1.364683531250014514, -0.7614583329919104582, -0.7879004041258359514 ) ) ;
#118500 = CARTESIAN_POINT ( 'NONE',  ( 2.196291916443537939, -1.129096229514385819, -1.315908775350557169 ) ) ;
#118501 = CARTESIAN_POINT ( 'NONE',  ( 1.622608716997505418, -1.639457832600412113, 0.5842430463761526527 ) ) ;
#118503 = CARTESIAN_POINT ( 'NONE',  ( 7.293923454472069245, 11.45340176361870199, 0.7216878364870438212 ) ) ;
#118502 = CARTESIAN_POINT ( 'NONE',  ( 5.848310222665911162, 2.304730150483401463, 0.1192407711079427196 ) ) ;
#118504 = CARTESIAN_POINT ( 'NONE',  ( 4.740510986633625024, 5.559626234941203116, -1.199719254218450271 ) ) ;
#118505 = CARTESIAN_POINT ( 'NONE',  ( 1.546242023939500276, 2.058303352229321703, 0.1039559743286587457 ) ) ;
#118506 = CARTESIAN_POINT ( 'NONE',  ( 6.819654193105592732, -1.783474119298094296, 1.449237643660877151 ) ) ;
#118507 = CARTESIAN_POINT ( 'NONE',  ( 3.475000000000000533, -1.604166666666667629, 2.006292185433948827 ) ) ;
#118508 = CARTESIAN_POINT ( 'NONE',  ( -4.450819567036169211, 8.414649604842665553, -0.7998128361456362523 ) ) ;
#118509 = CARTESIAN_POINT ( 'NONE',  ( 0.5671783758751040017, 0.1957704533250003986, -1.961731083161978306 ) ) ;
#118511 = CARTESIAN_POINT ( 'NONE',  ( -5.953438850176548947, 9.959779401932374654, 0.000000000000000000 ) ) ;
#118510 = CARTESIAN_POINT ( 'NONE',  ( 3.691585721427274258, 1.799035686688513325, -0.6489376663148455071 ) ) ;
#118512 = CARTESIAN_POINT ( 'NONE',  ( 6.709632191794143274, -0.4886956906769434061, 2.160084693451309601 ) ) ;
#118513 = CARTESIAN_POINT ( 'NONE',  ( -1.225000000000035172, 1.562500000682809365, -4.510281037539698445E-14 ) ) ;
#118514 = CARTESIAN_POINT ( 'NONE',  ( 0.4019237886466847653, 10.57366454968463110, 1.499999999999997113 ) ) ;
#118515 = CARTESIAN_POINT ( 'NONE',  ( 5.370438244344566847, 5.438135171256338829, 0.000000000000000000 ) ) ;
#118516 = CARTESIAN_POINT ( 'NONE',  ( -5.465345319640241506, 5.548860092434608760, 0.7216878364870257245 ) ) ;
#118517 = CARTESIAN_POINT ( 'NONE',  ( 6.340501840829311675, 1.221348521443364366, -1.733245716811770309 ) ) ;
#118518 = EDGE_CURVE ( 'NONE', #35390, #130778, #10959, .T. ) ;
#118519 = CARTESIAN_POINT ( 'NONE',  ( 3.610674682972123684, -0.9327887667434494601, -2.110822472020437601 ) ) ;
#118520 = CARTESIAN_POINT ( 'NONE',  ( 4.351973852746993110, -0.7528527933186466292, 1.811862133468461922 ) ) ;
#118521 = CARTESIAN_POINT ( 'NONE',  ( 1.129655866247070595, 1.892139549451707037, -0.5178372573612434193 ) ) ;
#118522 = LINE ( 'NONE', #67540, #78167 ) ;
#118523 = ORIENTED_EDGE ( 'NONE', *, *, #122827, .F. ) ;
#118524 = CARTESIAN_POINT ( 'NONE',  ( 6.403528931544730796, -1.954801056786956259, 0.4946215565981848528 ) ) ;
#118526 = CARTESIAN_POINT ( 'NONE',  ( -7.645908563102897126, 11.00764485934031889, 1.199719254218453823 ) ) ;
#118525 = CARTESIAN_POINT ( 'NONE',  ( -6.437424008390261854, 6.404749519410410485, 0.7998128361456341429 ) ) ;
#118527 = CARTESIAN_POINT ( 'NONE',  ( 0.2339851986729903077, 0.3116528534230639247, 1.814411239467295101 ) ) ;
#118528 = CARTESIAN_POINT ( 'NONE',  ( 2.624086282063769815, 2.129961278301984784, -0.4196836606994054364 ) ) ;
#118529 = CARTESIAN_POINT ( 'NONE',  ( 10.40128792240049194, 10.48955026364925835, -5.993062759042677712 ) ) ;
#118530 = CARTESIAN_POINT ( 'NONE',  ( 1.107859837811319581, 1.609452232531217275, 1.380942675281403353 ) ) ;
#118531 = CARTESIAN_POINT ( 'NONE',  ( -1.500000000000001332, 1.431250000682816825, 0.000000000000000000 ) ) ;
#118532 = CARTESIAN_POINT ( 'NONE',  ( 8.594979316059474073, 12.11489407112305372, 1.199719254218450271 ) ) ;
#118533 = CARTESIAN_POINT ( 'NONE',  ( 11.88237264505823987, 13.75677038468308844, -0.9087825512663076921 ) ) ;
#118534 = CARTESIAN_POINT ( 'NONE',  ( 6.328358748234019338, 6.951510624437585939, -0.8854765018257749754 ) ) ;
#118535 = CARTESIAN_POINT ( 'NONE',  ( 2.073578556082512403, 1.972924284924733929, -0.5953725496260859895 ) ) ;
#118537 = DIRECTION ( 'NONE',  ( -5.578564026256490882E-16, -1.000000000000000000, -9.066213480720158442E-32 ) ) ;
#118536 = CARTESIAN_POINT ( 'NONE',  ( -9.938290294017125603, 11.55342575023019691, -1.199719254218441611 ) ) ;
#118538 = CARTESIAN_POINT ( 'NONE',  ( -1.364683531250012516, 1.780208333674757615, 0.7879004041258379498 ) ) ;
#118539 = CARTESIAN_POINT ( 'NONE',  ( -0.7500000000000215383, 5.441666666666685082, 1.299038105676671107 ) ) ;
#118540 = DIRECTION ( 'NONE',  ( 0.000000000000000000, 0.4363663406439433068, -0.8997690907966409135 ) ) ;
#118541 = ORIENTED_EDGE ( 'NONE', *, *, #90321, .T. ) ;
#118542 = CARTESIAN_POINT ( 'NONE',  ( 4.617770051018644573, -0.5065499601877522240, 1.843912185298258066 ) ) ;
#118543 = CIRCLE ( 'NONE', #63135, 11.09999999999999964 ) ;
#118544 = CARTESIAN_POINT ( 'NONE',  ( -0.02968770228139894218, 7.629137130509075604, -2.426318643530885222 ) ) ;
#118545 = CARTESIAN_POINT ( 'NONE',  ( 1.019259390987249603, 2.090591978351970859, 0.8652678750288608223 ) ) ;
#118546 = CARTESIAN_POINT ( 'NONE',  ( -8.514157279702017078, 12.87700789305364069, -0.7216878364870267237 ) ) ;
#118547 = CARTESIAN_POINT ( 'NONE',  ( 1.863241329703895888, -1.456548260382009685, -1.076974786960547048 ) ) ;
#118548 = CARTESIAN_POINT ( 'NONE',  ( 0.3388992355649001476, -1.619940322034026270, -1.022281207937189684 ) ) ;
#118549 = CARTESIAN_POINT ( 'NONE',  ( 1.469279758060073160, 1.824989553406907383, 0.9776941847434923449 ) ) ;
#118550 = CARTESIAN_POINT ( 'NONE',  ( -0.6823417656250003738, 0.2802083336747515641, -1.181850606188749264 ) ) ;
#118551 = CARTESIAN_POINT ( 'NONE',  ( 0.1628737759792201201, -1.759808232078699630, -0.8888803535714930870 ) ) ;
#118552 = CARTESIAN_POINT ( 'NONE',  ( 5.566998737003931552, -1.742544991934717125, -0.8218319283359241112 ) ) ;
#118553 = EDGE_CURVE ( 'NONE', #93109, #195316, #136479, .T. ) ;
#118555 = CARTESIAN_POINT ( 'NONE',  ( 6.119462805442048570, 6.996221746119736018, -0.9567421715909133484 ) ) ;
#118554 = CARTESIAN_POINT ( 'NONE',  ( 0.4523713176287887383, 0.7179250195528188438, -2.193251166140824715 ) ) ;
#118556 = CARTESIAN_POINT ( 'NONE',  ( 1.364683531249988535, 1.613541667008084879, 0.7879004041258500513 ) ) ;
#118557 = CARTESIAN_POINT ( 'NONE',  ( 3.930177659428602865, 1.143423634368987196, 1.716560605327678513 ) ) ;
#118558 = CARTESIAN_POINT ( 'NONE',  ( -5.554036483092550824, 9.631459663583308739, -0.7998128361456231517 ) ) ;
#118559 = CARTESIAN_POINT ( 'NONE',  ( 6.577677080924314801, 10.82570702772039262, 1.040834085586084257E-14 ) ) ;
#118560 = CARTESIAN_POINT ( 'NONE',  ( 3.680148631105580215, 6.380924938676771241, -1.199719254218446718 ) ) ;
#118561 = CARTESIAN_POINT ( 'NONE',  ( 6.342516933094585418, 6.294024598232139667, 1.040834085586084257E-14 ) ) ;
#118563 = CARTESIAN_POINT ( 'NONE',  ( 0.7499999999999902300, 4.316666666666691299, -1.299038105676658228 ) ) ;
#118562 = CARTESIAN_POINT ( 'NONE',  ( 5.667048493276758414, -1.902512422570214357, -0.9033719842039839021 ) ) ;
#118564 = CARTESIAN_POINT ( 'NONE',  ( 6.057099581687969803, 1.694805161836069107, -1.188877858866774107 ) ) ;
#118565 = CARTESIAN_POINT ( 'NONE',  ( 0.6823417656249882723, 1.488541667008083547, -1.181850606188749264 ) ) ;
#118566 = CARTESIAN_POINT ( 'NONE',  ( 4.745497693432328745, -1.667575968047749546, -1.375352955852253922 ) ) ;
#118567 = CARTESIAN_POINT ( 'NONE',  ( 4.231121231147261241, 1.847467856137770204, 0.8164654241873505747 ) ) ;
#118568 = CARTESIAN_POINT ( 'NONE',  ( -5.761852096127856981, 5.824508321678349532, 0.000000000000000000 ) ) ;
#118571 = CARTESIAN_POINT ( 'NONE',  ( 5.910991785878156435, 7.919243054989755670, -1.443375672974057666 ) ) ;
#118570 = CARTESIAN_POINT ( 'NONE',  ( 0.000000000000000000, -1.246874999522042948, -3.793834371823813001 ) ) ;
#118569 = CARTESIAN_POINT ( 'NONE',  ( 6.393551957296131683, 9.616838495890963401, 1.199719254218452047 ) ) ;
#118572 = CARTESIAN_POINT ( 'NONE',  ( -4.620296487206990932, 8.612372678375294299, 0.000000000000000000 ) ) ;
#118573 = CARTESIAN_POINT ( 'NONE',  ( 4.048064755690682581, 0.9548552675892291175, 1.776167154503265566 ) ) ;
#118574 = CARTESIAN_POINT ( 'NONE',  ( -9.501566725078754772, 9.979582688880366703, -0.7998128361456291469 ) ) ;
#118575 = CARTESIAN_POINT ( 'NONE',  ( -4.334856428067329404, 6.080418470877079429, -1.599625672291256295 ) ) ;
#118576 = CARTESIAN_POINT ( 'NONE',  ( -1.326716514427061987E-15, 2.999999999999988454, -1.225000000000003864 ) ) ;
#118577 = CARTESIAN_POINT ( 'NONE',  ( 6.396834479292349052, -8.176568542494905500, 7.055228938194280985 ) ) ;
#118579 = CARTESIAN_POINT ( 'NONE',  ( 4.095327490859664188, -0.3419149367107060522, 1.987051255384481463 ) ) ;
#118578 = CARTESIAN_POINT ( 'NONE',  ( -7.009202228140744673, 10.16085778526412042, -1.082531754730537088 ) ) ;
#118580 = CARTESIAN_POINT ( 'NONE',  ( 0.7499999999999920064, 5.483333333333353821, 1.299038105676669330 ) ) ;
#118581 = CARTESIAN_POINT ( 'NONE',  ( 0.6094340267816320544, -1.717071606940338446, 0.1640370458491739458 ) ) ;
#118582 = CARTESIAN_POINT ( 'NONE',  ( 6.412080304620304538, 6.445458208337293549, -0.7998128361456481317 ) ) ;
#118583 = AXIS2_PLACEMENT_3D ( 'NONE', #115699, #62618, #99402 ) ;
#118585 = CARTESIAN_POINT ( 'NONE',  ( -4.202664430556263042, 5.926194473780837413, 1.443375672974064550 ) ) ;
#118584 = CARTESIAN_POINT ( 'NONE',  ( 8.595506201384013778, 10.09080732544527592, 1.082531754730558626 ) ) ;
#118586 = CARTESIAN_POINT ( 'NONE',  ( -10.52211811376582062, 5.354010262649190111, 5.769489279399181214 ) ) ;
#118587 = CARTESIAN_POINT ( 'NONE',  ( 4.991395955090764502, 1.385047395102714685, 1.257364466828891914 ) ) ;
#118588 = CARTESIAN_POINT ( 'NONE',  ( 6.258070432960613161, 0.7665029349510013024, -1.861766797742714585 ) ) ;
#118589 = CYLINDRICAL_SURFACE ( 'NONE', #29910, 0.4000000000000001332 ) ;
#118590 = CARTESIAN_POINT ( 'NONE',  ( -5.261973015435229328, 9.153069261400824885, 0.000000000000000000 ) ) ;
#118591 = ORIENTED_EDGE ( 'NONE', *, *, #34900, .F. ) ;
#118592 = CARTESIAN_POINT ( 'NONE',  ( 1.159780049612362030, 1.203373692603469935, 1.617804775344060308 ) ) ;
#118593 = CARTESIAN_POINT ( 'NONE',  ( 1.335881098409009704, -1.007921504507871102, -1.505067075931452392 ) ) ;
#118594 = EDGE_CURVE ( 'NONE', #176125, #41277, #157206, .T. ) ;
#118595 = CARTESIAN_POINT ( 'NONE',  ( 3.512971199272317602, 6.152197928242737923, -1.082531754730549967 ) ) ;
#118596 = CARTESIAN_POINT ( 'NONE',  ( 5.946190753372003535, 2.158995856162956084, 0.1107517376499680406 ) ) ;
#118597 = CARTESIAN_POINT ( 'NONE',  ( 7.772902139336337335, 7.962807338847539107, 0.7998128361456341429 ) ) ;
#118598 = MECHANICAL_DESIGN_GEOMETRIC_PRESENTATION_REPRESENTATION (  '', ( #108249 ), #156595 ) ;
#118600 = CARTESIAN_POINT ( 'NONE',  ( -0.1532965272393977951, -1.712378426511364404, -0.8589627718659180733 ) ) ;
#118599 = CARTESIAN_POINT ( 'NONE',  ( -3.730464822054482710, 7.503959392372201442, 1.040834085586084257E-14 ) ) ;
#118601 = AXIS2_PLACEMENT_3D ( 'NONE', #59060, #158704, #30586 ) ;
#118602 = CARTESIAN_POINT ( 'NONE',  ( 1.855128211190495202, 8.960462962215050453, 0.7750000000000004663 ) ) ;
#118603 = PLANE ( 'NONE',  #187222 ) ;
#118604 = CARTESIAN_POINT ( 'NONE',  ( 0.6823417656249882723, -0.5947916663252492686, 1.181850606188755259 ) ) ;
#118606 = ORIENTED_EDGE ( 'NONE', *, *, #167207, .F. ) ;
#118605 = LINE ( 'NONE', #165162, #36175 ) ;
#118607 = CARTESIAN_POINT ( 'NONE',  ( -4.295235737431041478, 3.905529869957963029, -0.7998128361456221525 ) ) ;
#118608 = CARTESIAN_POINT ( 'NONE',  ( 3.713887418366210724, -2.130098009959373151, 0.3673708613747132534 ) ) ;
#118609 = CARTESIAN_POINT ( 'NONE',  ( -6.780486220610195680, 7.083191143566240910, -0.7216878364870338292 ) ) ;
#118610 = ADVANCED_FACE ( 'NONE', ( #94391 ), #188402, .T. ) ;
#118611 = CARTESIAN_POINT ( 'NONE',  ( 5.641601317062233001, 7.675230518029648508, -1.443375672974078761 ) ) ;
#118612 = CARTESIAN_POINT ( 'NONE',  ( 1.037531286769650452, -0.04638328994046451298, 2.120250110247793085 ) ) ;
#118613 = FACE_OUTER_BOUND ( 'NONE', #177859, .T. ) ;
#118614 = CIRCLE ( 'NONE', #84073, 11.00000000000000000 ) ;
#118615 = CARTESIAN_POINT ( 'NONE',  ( 1.739464312186237871, -1.425129977898047740, -1.362296117697106013 ) ) ;
#118616 = CARTESIAN_POINT ( 'NONE',  ( 4.623256175466385010, 1.666654777633369555, 0.9376445158523971646 ) ) ;
#118617 = EDGE_LOOP ( 'NONE', ( #97503, #95022, #191894, #42905 ) ) ;
#118618 = DIRECTION ( 'NONE',  ( 0.000000000000000000, 0.000000000000000000, -1.000000000000000000 ) ) ;
#118619 = CARTESIAN_POINT ( 'NONE',  ( 5.986760398725940568, 1.897641426698594813, 0.5270043353632068994 ) ) ;
#118620 = CARTESIAN_POINT ( 'NONE',  ( 0.1462902992968219407, -1.560392365369901668, 1.155808223090015963 ) ) ;
#118621 = ORIENTED_EDGE ( 'NONE', *, *, #61890, .F. ) ;
#118622 = CARTESIAN_POINT ( 'NONE',  ( -5.659602779061863487, 5.567567761852417085, 0.7998128361456281477 ) ) ;
#118624 = CARTESIAN_POINT ( 'NONE',  ( 6.940534579974978691, -6.675176078274695612, -6.653311379900283207 ) ) ;
#118623 = CARTESIAN_POINT ( 'NONE',  ( -4.496464221587651799, 5.274905009054215554, 1.199719254218452935 ) ) ;
#118626 = CARTESIAN_POINT ( 'NONE',  ( 5.004368096775565711, 8.852530189631227842, -0.7216878364870458196 ) ) ;
#118625 = CARTESIAN_POINT ( 'NONE',  ( 7.633404179693907388, 8.864391950186421454, -1.199719254218441611 ) ) ;
#118628 = VERTEX_POINT ( 'NONE', #57601 ) ;
#118627 = CARTESIAN_POINT ( 'NONE',  ( 5.180287844241702189, 0.9460499258955605839, 1.661804969971327761 ) ) ;
#118629 = B_SPLINE_CURVE_WITH_KNOTS ( 'NONE', 3,
 ( #149195, #165440, #82051, #34369, #198982, #83114 ),
 .UNSPECIFIED., .F., .F.,
 ( 4, 2, 4 ),
 ( 0.000000000000000000, 0.002406312826513422667, 0.004812625653026847070 ),
 .UNSPECIFIED. ) ;
#118630 = CARTESIAN_POINT ( 'NONE',  ( 3.352369063006555905, 2.207063162671081713, 4.936380160885933677E-05 ) ) ;
#118631 = AXIS2_PLACEMENT_3D ( 'NONE', #109638, #207045, #9916 ) ;
#118632 = CARTESIAN_POINT ( 'NONE',  ( 2.327434156339613924, -0.0004056629378437063877, 2.206952907597827362 ) ) ;
#118633 = CARTESIAN_POINT ( 'NONE',  ( 1.558944071570338652, 8.694263516233171174, 2.499999999999954259 ) ) ;
#118634 = CARTESIAN_POINT ( 'NONE',  ( 0.5746843702075511429, -1.384840223850939855, 1.318951758179337741 ) ) ;
#118635 = CARTESIAN_POINT ( 'NONE',  ( -1.790313668900411992, 0.4735605917218872474, 0.7140520948302793158 ) ) ;
#118636 = CARTESIAN_POINT ( 'NONE',  ( -2.359468172627429805, 5.347229341561620330, 0.7252027155559838123 ) ) ;
#118637 = CARTESIAN_POINT ( 'NONE',  ( -0.4092393038957372053, 6.441162235065689856, 3.221549646754199525 ) ) ;
#118638 = CARTESIAN_POINT ( 'NONE',  ( 3.578635096964689843, 1.315621898185691974, -1.598582974826658010 ) ) ;
#118639 = CARTESIAN_POINT ( 'NONE',  ( -5.935772324684618795, 5.819489221753827657, 0.000000000000000000 ) ) ;
#118640 = CARTESIAN_POINT ( 'NONE',  ( -4.752344554418619360, 8.202642464201909789, 0.7248784622895955154 ) ) ;
#118642 = CARTESIAN_POINT ( 'NONE',  ( 0.4269344243218140544, 2.069031678568326704, 0.6260965431626740463 ) ) ;
#118641 = CARTESIAN_POINT ( 'NONE',  ( -4.711622075948912247, 5.455646162483875017, -1.199719254218446718 ) ) ;
#118643 = CARTESIAN_POINT ( 'NONE',  ( 2.718528139169604341, 2.064530135181973591, 0.7356957861901700646 ) ) ;
#118644 = DIRECTION ( 'NONE',  ( 2.949029909160572061E-17, 1.000000000000000000, -8.673600428462391266E-15 ) ) ;
#118645 = CARTESIAN_POINT ( 'NONE',  ( 4.421367491832282504, 5.291255174293369556, 1.082531754730549078 ) ) ;
#118646 = CARTESIAN_POINT ( 'NONE',  ( 1.435115314734433989, 7.268684689231783125, 4.324912918975653220 ) ) ;
#118647 = CARTESIAN_POINT ( 'NONE',  ( -0.6823417656250039265, 12.88020833367473017, -1.181850606188755259 ) ) ;
#118648 = CARTESIAN_POINT ( 'NONE',  ( -5.631432701629818460, 7.663367133358481631, 1.599625672291263179 ) ) ;
#118649 = CARTESIAN_POINT ( 'NONE',  ( 6.258463337875916466, 1.656396116010181219, -0.5134576769376431038 ) ) ;
#118650 = CARTESIAN_POINT ( 'NONE',  ( -3.898132859128961236, 4.506575409527250997, -1.199719254218452047 ) ) ;
#118651 = CARTESIAN_POINT ( 'NONE',  ( 3.344645782512998267, -2.038826501179476391, -0.3585456059004287765 ) ) ;
#118652 = CARTESIAN_POINT ( 'NONE',  ( 4.903976463145187203, -1.133744943205544642, -1.787932202283550875 ) ) ;
#118653 = CARTESIAN_POINT ( 'NONE',  ( 4.801558957534076022, 8.753569217098425170, 0.7998128361456462443 ) ) ;
#118655 = EDGE_CURVE ( 'NONE', #37843, #160336, #173510, .T. ) ;
#118654 = CARTESIAN_POINT ( 'NONE',  ( 1.364683531249990311, 4.884375000341417916, 1.214306433183764966E-14 ) ) ;
#118656 = CARTESIAN_POINT ( 'NONE',  ( 2.377736956781382638, -1.911501772163497481, 0.4737601246572603064 ) ) ;
#118657 = CARTESIAN_POINT ( 'NONE',  ( 0.9844543725016400293, -1.211084316286781037, 1.480072698922259455 ) ) ;
#118658 = B_SPLINE_CURVE_WITH_KNOTS ( 'NONE', 3,
 ( #157544, #71976, #58960, #5903, #6973, #188951, #88261, #40591, #90403, #155390, #174871, #104519 ),
 .UNSPECIFIED., .F., .F.,
 ( 4, 2, 2, 2, 2, 4 ),
 ( 0.003750395023277889282, 0.003985267534262568016, 0.004220140045247247618, 0.004689885067216603351, 0.005159630089185959952, 0.005629375111155316552 ),
 .UNSPECIFIED. ) ;
#118659 = CARTESIAN_POINT ( 'NONE',  ( 4.716876218882520178, -0.1156266834452194386, 2.289457304130739779 ) ) ;
#118660 = CARTESIAN_POINT ( 'NONE',  ( 2.543341688579534132, -1.352695106659363544, -1.226303905950577144 ) ) ;
#118661 = EDGE_CURVE ( 'NONE', #128332, #93282, #179886, .T. ) ;
#118662 = CARTESIAN_POINT ( 'NONE',  ( 5.564695703766185275, 5.456842840674144490, 0.000000000000000000 ) ) ;
#118663 = CARTESIAN_POINT ( 'NONE',  ( 4.473827502385202770, 8.163289819517311585, 1.040834085586084257E-14 ) ) ;
#118664 = CARTESIAN_POINT ( 'NONE',  ( -5.533699252672048985, 9.607732894759390518, -0.7998128361456231517 ) ) ;
#118665 = CARTESIAN_POINT ( 'NONE',  ( 4.043230579294037952, 0.1031557717955585846, 2.010702285795034072 ) ) ;
#118666 = CARTESIAN_POINT ( 'NONE',  ( 4.364078322825436729, -1.956782558839207375, 0.1401112987177987601 ) ) ;
#118667 = CARTESIAN_POINT ( 'NONE',  ( -6.995117189646935962, 10.24838825697502109, 1.199719254218453823 ) ) ;
#118668 = CARTESIAN_POINT ( 'NONE',  ( -4.252453736180621391, 8.112946458852704268, -0.7998128361456281477 ) ) ;
#118669 = DIRECTION ( 'NONE',  ( 0.7592566023653005702, -0.6507913734559639396, 0.000000000000000000 ) ) ;
#118671 = CARTESIAN_POINT ( 'NONE',  ( 5.365971031753679732, 0.8746336007162245352, 1.538519630229380875 ) ) ;
#118670 = CARTESIAN_POINT ( 'NONE',  ( 0.1168898295945815374, -0.09829507837614966104, 2.088553102151818219 ) ) ;
#118672 = FACE_OUTER_BOUND ( 'NONE', #198481, .T. ) ;
#118673 = CARTESIAN_POINT ( 'NONE',  ( 2.326364362698669641, 2.126017103801054464, 0.5310240739047759062 ) ) ;
#118674 = CARTESIAN_POINT ( 'NONE',  ( 6.228409164912255491, 0.1778687648950585953, 1.731214608917114317 ) ) ;
#118675 = CARTESIAN_POINT ( 'NONE',  ( 5.587931867126699537, 9.671004278289832001, -0.7998128361456291469 ) ) ;
#118676 = SURFACE_STYLE_USAGE ( .BOTH. , #52543 ) ;
#118677 = CARTESIAN_POINT ( 'NONE',  ( 0.1699431646460221601, -1.131269863993559222, 1.302202208916112269 ) ) ;
#118678 = CARTESIAN_POINT ( 'NONE',  ( 0.2049558871960316941, 1.909868400323280424, 1.074723926240577221 ) ) ;
#118679 = CARTESIAN_POINT ( 'NONE',  ( 2.438337523484556790, 1.039148161723329578, -1.946916322307743474 ) ) ;
#118680 = PRESENTATION_LAYER_ASSIGNMENT (  '', '', ( #211995 ) ) ;
#118681 = CARTESIAN_POINT ( 'NONE',  ( 6.865710891575433905, -0.4862813381408522817, 2.124062634707358566 ) ) ;
#118682 = DIRECTION ( 'NONE',  ( -1.000000000000000000, 0.000000000000000000, 3.491481338843133355E-15 ) ) ;
#118683 = CARTESIAN_POINT ( 'NONE',  ( 0.7259617406208430657, 0.8522569803141609723, -1.938411259892757421 ) ) ;
#118684 = CIRCLE ( 'NONE', #104732, 12.00000000000000178 ) ;
#118685 = CARTESIAN_POINT ( 'NONE',  ( 6.777910281175842044, -7.189645481333912791, -6.776323679500925401 ) ) ;
#118686 = CARTESIAN_POINT ( 'NONE',  ( 5.948256396973989446, 1.924214498663083139, 0.09423418586224258098 ) ) ;
#118687 = ORIENTED_EDGE ( 'NONE', *, *, #134985, .T. ) ;
#118689 = CARTESIAN_POINT ( 'NONE',  ( -1.364683531250014514, -0.6989583329919100141, -0.7879004041258359514 ) ) ;
#118688 = CARTESIAN_POINT ( 'NONE',  ( 1.927642574099263983, -1.500803908722462499, -1.732858182149794812 ) ) ;
#118690 = CARTESIAN_POINT ( 'NONE',  ( 4.521807925357579805, 5.234196320127330715, -1.199719254218452047 ) ) ;
#118691 = CARTESIAN_POINT ( 'NONE',  ( 4.984594031318565932, 8.967110136513669616, 0.7998128361456462443 ) ) ;
#118692 = CARTESIAN_POINT ( 'NONE',  ( 3.580930751873512285, -1.490882799914891033, 1.646821992171596971 ) ) ;
#118693 = CARTESIAN_POINT ( 'NONE',  ( -7.537970219518083326, 9.817384560903001045, -1.443375672974059665 ) ) ;
#118694 = CARTESIAN_POINT ( 'NONE',  ( 4.826339496784873617, 8.574553812983598533, -0.7216878364870257245 ) ) ;
#118695 = CARTESIAN_POINT ( 'NONE',  ( -7.931156673870055407, 11.23647130528163096, 1.082531754730549967 ) ) ;
#118696 = CARTESIAN_POINT ( 'NONE',  ( 5.478903473698239601, 7.485416367438324059, -1.443375672974078761 ) ) ;
#118697 = VERTEX_POINT ( 'NONE', #165762 ) ;
#118698 = CARTESIAN_POINT ( 'NONE',  ( 1.705704151892040832, 1.882474636155605507, 0.7231385473688843879 ) ) ;
#118700 = CARTESIAN_POINT ( 'NONE',  ( 1.534110023759263308, 1.225272132802219360, 1.659075958507538973 ) ) ;
#118699 = CARTESIAN_POINT ( 'NONE',  ( 8.046927864910717432, 9.346836249606042202, 1.199719254218462483 ) ) ;
#118701 = CARTESIAN_POINT ( 'NONE',  ( 4.678972410047582464, 8.472901888448573615, -0.7216878364870357165 ) ) ;
#118702 = CARTESIAN_POINT ( 'NONE',  ( 0.6823417656249899377, 3.676041667008085767, -1.181850606188754593 ) ) ;
#118703 = CARTESIAN_POINT ( 'NONE',  ( 4.505938053128990539, -0.9357023767473917619, -1.981784127816770935 ) ) ;
#118704 = CARTESIAN_POINT ( 'NONE',  ( 0.7564826839323666174, 1.942540863013635821, -0.5404934282097761944 ) ) ;
#118705 = CARTESIAN_POINT ( 'NONE',  ( 1.083273795380396143, -0.8277460070302902206, 1.644747122058511035 ) ) ;
#118706 = CARTESIAN_POINT ( 'NONE',  ( 5.232074500395570205, 2.258064205686944437, 0.3942454582816708464 ) ) ;
#118707 = CARTESIAN_POINT ( 'NONE',  ( 2.958754162918544761, 0.2696264243384552950, -1.821159755858774654 ) ) ;
#118708 = CARTESIAN_POINT ( 'NONE',  ( 9.433775957010412938, 9.900493459467314850, 0.000000000000000000 ) ) ;
#118709 = CARTESIAN_POINT ( 'NONE',  ( 4.207882836062684540, -1.820678405428953095, 0.1343838851760314757 ) ) ;
#118710 = CARTESIAN_POINT ( 'NONE',  ( 4.764296165657141202, 1.880435471729305030, -0.7283773170061805802 ) ) ;
#118711 = CARTESIAN_POINT ( 'NONE',  ( -9.352427035328430449, 9.805586384171650849, 1.040834085586084257E-14 ) ) ;
#118713 = CARTESIAN_POINT ( 'NONE',  ( -5.596483547390937119, 9.751257581923240991, 0.000000000000000000 ) ) ;
#118712 = CARTESIAN_POINT ( 'NONE',  ( 4.188523121243816760, -2.237390873258153778, -0.3355513299154490592 ) ) ;
#118714 = CARTESIAN_POINT ( 'NONE',  ( 6.633818197422741925, -1.372689285068533271, -1.597217228543364564 ) ) ;
#118715 =( NAMED_UNIT ( * ) PLANE_ANGLE_UNIT ( ) SI_UNIT ( $, .RADIAN. ) );
#118716 = CARTESIAN_POINT ( 'NONE',  ( 3.227070907399377298, -1.911900318415656441, -0.7948586591664741352 ) ) ;
#118717 = CARTESIAN_POINT ( 'NONE',  ( 2.218730694130720771, 5.740269576461138890, 0.7998128361456462443 ) ) ;
#118718 = CARTESIAN_POINT ( 'NONE',  ( -1.360316468750038643, 1.651041667008089853, -0.7853790794159041244 ) ) ;
#118719 = APPLICATION_PROTOCOL_DEFINITION ( 'draft international standard', 'automotive_design', 1998, #38036 ) ;
#118721 = CARTESIAN_POINT ( 'NONE',  ( 2.139170349095420143, -1.720849962885454110, 0.8662218532024426043 ) ) ;
#118720 = CARTESIAN_POINT ( 'NONE',  ( -8.829384350997580455, 11.32403438096243775, 1.599625672291269396 ) ) ;
#118722 = UNCERTAINTY_MEASURE_WITH_UNIT (LENGTH_MEASURE( 1.000000000000000082E-05 ), #2030, 'distance_accuracy_value', 'NONE');
#118723 = DIRECTION ( 'NONE',  ( -1.000000000000000000, 0.000000000000000000, 0.000000000000000000 ) ) ;
#118724 = CARTESIAN_POINT ( 'NONE',  ( 6.965690641875434075, -0.4316760948062084990, 1.928339623932231239 ) ) ;
#118725 = CARTESIAN_POINT ( 'NONE',  ( 3.377389663135653031, 6.954388683717978026, -0.7216878364870338292 ) ) ;
#118726 = CARTESIAN_POINT ( 'NONE',  ( 5.849510849484250485, 6.002983934024645585, 0.3487602046992159810 ) ) ;
#118727 = CARTESIAN_POINT ( 'NONE',  ( -1.500000000000015099, 11.01041666734946389, -0.8660254037844309360 ) ) ;
#118728 = CARTESIAN_POINT ( 'NONE',  ( -2.819205876637805641, 5.376491725131008259, -1.199719254218446718 ) ) ;
#118729 = CARTESIAN_POINT ( 'NONE',  ( 2.127449211838834398, 1.986592753075850037, 0.9941332784057993477 ) ) ;
#118730 = AXIS2_PLACEMENT_3D ( 'NONE', #200801, #137979, #38332 ) ;
#118731 = CARTESIAN_POINT ( 'NONE',  ( 3.540152450731326450, 0.9484212380423739930, -1.880392733946538719 ) ) ;
#118732 = CARTESIAN_POINT ( 'NONE',  ( -7.598418745816086783, 7.829519723065708092, 0.000000000000000000 ) ) ;
#118733 = CARTESIAN_POINT ( 'NONE',  ( 6.076025397218672630, 10.24044673006381245, -0.7998128361456291469 ) ) ;
#118734 = CARTESIAN_POINT ( 'NONE',  ( 0.6954782174160825114, -1.312119466559122927, -1.320074052667360665 ) ) ;
#118735 = CARTESIAN_POINT ( 'NONE',  ( 7.149227073107712549, 7.235186428247455837, -0.7998128361456281477 ) ) ;
#118736 = CARTESIAN_POINT ( 'NONE',  ( 4.527533231959700366, 7.369540306339926516, 1.199719254218462483 ) ) ;
#118737 = CARTESIAN_POINT ( 'NONE',  ( -5.587368702607575344, 8.572328348800551723, 1.082531754730550855 ) ) ;
#118738 = CARTESIAN_POINT ( 'NONE',  ( -8.853111120043687166, 9.430977182913531820, 1.040834085586084257E-14 ) ) ;
#118739 = CARTESIAN_POINT ( 'NONE',  ( 1.406653384705614629, -2.110883996484512970, -0.2024971186788473154 ) ) ;
#118740 = CARTESIAN_POINT ( 'NONE',  ( -7.422162748838431412, 7.623887726591770608, -0.7998128361456362523 ) ) ;
#118742 = CARTESIAN_POINT ( 'NONE',  ( 4.527759979645433752, 1.903474890065796732, -0.4746247275292309609 ) ) ;
#118741 = CARTESIAN_POINT ( 'NONE',  ( 1.224999999999963896, 1.374999999999987343, -4.857225732735059864E-14 ) ) ;
#118743 = CARTESIAN_POINT ( 'NONE',  ( 3.063507763784904192, 0.3185916186679502715, -2.137983152197140413 ) ) ;
#118744 = CARTESIAN_POINT ( 'NONE',  ( 1.382094229771430705, -0.2707140722739818650, -1.821126350552772832 ) ) ;
#118745 = CARTESIAN_POINT ( 'NONE',  ( -4.059107376188687333, 7.562469429224047524, 0.4300614504739261879 ) ) ;
#118746 = DIRECTION ( 'NONE',  ( -3.451266460341926649E-31, -5.200010849845536803E-32, 1.000000000000000000 ) ) ;
#118747 = CARTESIAN_POINT ( 'NONE',  ( 4.997892061590047952, -0.5910035050068825901, -1.637047790839076589 ) ) ;
#118748 = CARTESIAN_POINT ( 'NONE',  ( -1.878313713277967700, 15.99999999999538858, -12.68000002627077905 ) ) ;
#118749 = CARTESIAN_POINT ( 'NONE',  ( 4.528060117284222308, 8.226561203566173930, 0.7216878364870438212 ) ) ;
#118750 = CARTESIAN_POINT ( 'NONE',  ( -10.28816806463375144, 6.680837282875757843, -5.326249955113787848 ) ) ;
#118751 = CARTESIAN_POINT ( 'NONE',  ( 2.202237438260604030, -2.161223104231101644, 0.05255616829508147347 ) ) ;
#118752 = CARTESIAN_POINT ( 'NONE',  ( 3.690779688840303496, -1.198677090843719872, -1.620934038430859703 ) ) ;
#118753 = CARTESIAN_POINT ( 'NONE',  ( 3.834746474454188013E-15, 12.84375000068279782, 1.500000000000001554 ) ) ;
#118754 = CARTESIAN_POINT ( 'NONE',  ( 1.217891636700708435, -2.108894920778502602, 0.4742063263511315796 ) ) ;
#118755 = CARTESIAN_POINT ( 'NONE',  ( 2.922686454756417085, 1.855838157306726632, 0.6655703372969791198 ) ) ;
#118756 = CARTESIAN_POINT ( 'NONE',  ( 6.509000000000010111, 3.701365531483376881, 2.414445852726577080 ) ) ;
#118757 = CARTESIAN_POINT ( 'NONE',  ( 3.895986966309549882, -0.6120611862858457153, -1.843141947886927978 ) ) ;
#118760 = VERTEX_POINT ( 'NONE', #29371 ) ;
#118759 = CARTESIAN_POINT ( 'NONE',  ( -5.180624094197616714, 5.216685329418210948, 0.7216878364870257245 ) ) ;
#118758 = CARTESIAN_POINT ( 'NONE',  ( -10.61567108937589765, 11.48729714713446803, 0.7216878364870438212 ) ) ;
#118761 = CARTESIAN_POINT ( 'NONE',  ( -3.973948422136968084, 7.650373902552835226, -0.7216878364870458196 ) ) ;
#118762 = CARTESIAN_POINT ( 'NONE',  ( -0.1106856583840878927, 5.722746153615347886, -2.590994828783958592 ) ) ;
#118763 = CARTESIAN_POINT ( 'NONE',  ( 5.061990249855835344, 6.999017606288844284, -1.599625672291273171 ) ) ;
#118764 = CARTESIAN_POINT ( 'NONE',  ( -6.140917232347002042, 6.129101290685087911, -0.7998128361456362523 ) ) ;
#118765 = CARTESIAN_POINT ( 'NONE',  ( -7.618755976236585958, 7.853246491889623648, 0.000000000000000000 ) ) ;
#118766 = CARTESIAN_POINT ( 'NONE',  ( -10.12757755928392456, 10.91785469536048758, 0.7216878364870438212 ) ) ;
#118767 = EDGE_CURVE ( 'NONE', #52075, #103536, #169141, .T. ) ;
#118768 = CARTESIAN_POINT ( 'NONE',  ( 0.2181801407958559869, -2.163675782650812618, 0.4331315337846516900 ) ) ;
#118769 = CARTESIAN_POINT ( 'NONE',  ( -3.285556943750000514, -3.638541666188706891, -1.896917185911906500 ) ) ;
#118770 = AXIS2_PLACEMENT_3D ( 'NONE', #69927, #136038, #53711 ) ;
#118771 = CARTESIAN_POINT ( 'NONE',  ( 4.522284091987982535, 0.9210895807079204634, 1.732038000912524689 ) ) ;
#118772 = CARTESIAN_POINT ( 'NONE',  ( 7.422199028477372451, 10.74665040227725044, -1.199719254218441611 ) ) ;
#118773 = CARTESIAN_POINT ( 'NONE',  ( 2.250625165576759290, 1.976955744075848065, -0.3961026872240576702 ) ) ;
#118774 = ORIENTED_EDGE ( 'NONE', *, *, #122755, .T. ) ;
#118775 = CARTESIAN_POINT ( 'NONE',  ( 3.169268314845040901, 1.912196763353574358, -0.9095376832224701946 ) ) ;
#118776 = CARTESIAN_POINT ( 'NONE',  ( 0.7499999999999885647, 2.097916667349486453, -1.299038105676652899 ) ) ;
#118777 = CARTESIAN_POINT ( 'NONE',  ( -6.878064000834399394, 6.918829510595249310, -0.7998128361456291469 ) ) ;
#118778 = CARTESIAN_POINT ( 'NONE',  ( 2.835703941817575124, 1.827261480098177460, 0.2250241719141122809 ) ) ;
#118779 = VERTEX_POINT ( 'NONE', #149511 ) ;
#118780 = CARTESIAN_POINT ( 'NONE',  ( -8.076906825439122528, 10.44614393447756129, -1.599625672291263179 ) ) ;
#118781 = CARTESIAN_POINT ( 'NONE',  ( 4.796824973295459316, 8.251456047330133714, 0.8599625132450954279 ) ) ;
#118782 = CARTESIAN_POINT ( 'NONE',  ( 4.043311264919998038, 0.1072909356813686182, 2.118029240109862155 ) ) ;
#118783 = DIRECTION ( 'NONE',  ( 0.000000000000000000, -1.000000000000000000, 0.000000000000000000 ) ) ;
#118784 = CARTESIAN_POINT ( 'NONE',  ( 7.637320603199683866, 7.804628880021436288, -0.7998128361456281477 ) ) ;
#118785 = CONICAL_SURFACE ( 'NONE', #191373, 8.368490868537556082, 0.7853981633974479459 ) ;
#118786 = CARTESIAN_POINT ( 'NONE',  ( 5.870404149471736943, -1.310866377807779593, 1.590078559457400287 ) ) ;
#118788 = CARTESIAN_POINT ( 'NONE',  ( 2.190726087351921425, 1.424366561657765207, 1.166803476217087576 ) ) ;
#118787 = CARTESIAN_POINT ( 'NONE',  ( 0.8536796107712171233, -0.6749765833247187707, 1.734523287792593571 ) ) ;
#118789 = CARTESIAN_POINT ( 'NONE',  ( 8.259941899223605333, 10.65968485389279508, -1.599625672291268286 ) ) ;
#118790 = CARTESIAN_POINT ( 'NONE',  ( 0.8281745818101267087, -6.790584702349180379E-15, 1.093811874046688892 ) ) ;
#118791 = LINE ( 'NONE', #50532, #70133 ) ;
#118792 = FACE_OUTER_BOUND ( 'NONE', #47004, .T. ) ;
#118793 = CARTESIAN_POINT ( 'NONE',  ( 1.981372325807278623, -0.1102420082176903682, -2.204251428397439483 ) ) ;
#118794 = CARTESIAN_POINT ( 'NONE',  ( 4.780719109985231974, -2.192918799143634079, -0.5559354454096259168 ) ) ;
#118795 = CARTESIAN_POINT ( 'NONE',  ( -6.209271165378811297, 10.18797409300986878, 0.7216878364870458196 ) ) ;
#118796 = CARTESIAN_POINT ( 'NONE',  ( 5.168131652730963310, 1.809155975298855523, -0.09671077906142805380 ) ) ;
#118797 = CARTESIAN_POINT ( 'NONE',  ( 4.311684426593565433, -1.183387839401760511, -1.506387502079686191 ) ) ;
#118798 = ADVANCED_FACE ( 'NONE', ( #114937 ), #1072, .F. ) ;
#118799 = CARTESIAN_POINT ( 'NONE',  ( -1.364683531249997417, 4.321875000341417028, 1.214306433183764966E-14 ) ) ;
#118800 = CARTESIAN_POINT ( 'NONE',  ( 3.854335392261270421, 0.7083531993744094368, 1.839989435513892380 ) ) ;
#118801 = CARTESIAN_POINT ( 'NONE',  ( 4.961713530105988923, 1.850188064717460223, -0.2750520410098392654 ) ) ;
#118802 = EDGE_CURVE ( 'NONE', #56229, #45216, #208570, .T. ) ;
#118803 = CARTESIAN_POINT ( 'NONE',  ( 4.791365544089026152, -1.701862485369805000, 0.7535167838805619800 ) ) ;
#118804 = CARTESIAN_POINT ( 'NONE',  ( 1.364683531249992088, 5.384375000341417916, 1.214306433183764966E-14 ) ) ;
#118805 = CARTESIAN_POINT ( 'NONE',  ( 0.5851731681005939434, 1.651346252830317551, 1.157095189655330314 ) ) ;
#118806 =( BOUNDED_CURVE ( )  B_SPLINE_CURVE ( 3, ( #30570, #98762, #180012, #80371 ),
 .UNSPECIFIED., .F., .T. ) 
 B_SPLINE_CURVE_WITH_KNOTS ( ( 4, 4 ),
 ( 0.000000000000000000, 0.5000000000000018874 ),
 .UNSPECIFIED. ) 
 CURVE ( )  GEOMETRIC_REPRESENTATION_ITEM ( )  RATIONAL_B_SPLINE_CURVE ( ( 1.000000000000000000, 0.3333333333333308723, 0.3333333333333333703, 1.000000000000002442 ) ) 
 REPRESENTATION_ITEM ( '' )  );
#118808 = CARTESIAN_POINT ( 'NONE',  ( 1.858176280533967661, 2.100347624109857758, -0.1560452747076390423 ) ) ;
#118807 = CARTESIAN_POINT ( 'NONE',  ( -4.134873662043608178, 4.886736029548026217, 1.082531754730558626 ) ) ;
#118809 = CARTESIAN_POINT ( 'NONE',  ( 9.480175724453529185, 12.08329098332774265, 1.599625672291279388 ) ) ;
#118811 = CARTESIAN_POINT ( 'NONE',  ( -10.15522075183580419, 11.80651128435196462, 1.199719254218462483 ) ) ;
#118810 = CARTESIAN_POINT ( 'NONE',  ( 0.6823417656249899377, 5.488541667008087543, -1.181850606188754593 ) ) ;
#118812 = CARTESIAN_POINT ( 'NONE',  ( -9.622669940282571943, -9.063128755109497448, 0.5283818209470610983 ) ) ;
#118813 = CARTESIAN_POINT ( 'NONE',  ( 2.338154391725711267, -1.166417678377267064, -1.648725491961404055 ) ) ;
#118814 = CARTESIAN_POINT ( 'NONE',  ( 1.364683531249988757, 1.634375000341421691, 0.000000000000000000 ) ) ;
#118815 = CARTESIAN_POINT ( 'NONE',  ( -4.636525346193588248, 4.511627113421689650, 0.7216878364870317197 ) ) ;
#118816 = CARTESIAN_POINT ( 'NONE',  ( 3.486418057008484617, 7.219238166485217434, 1.040834085586084257E-14 ) ) ;
#118817 = CARTESIAN_POINT ( 'NONE',  ( 2.618638089201937635, 1.414096770131420877, -1.634928933042498755 ) ) ;
#118818 = CARTESIAN_POINT ( 'NONE',  ( 6.610000000000026965, 7.052677709320480659, 2.598153670447616470 ) ) ;
#118821 = CARTESIAN_POINT ( 'NONE',  ( 2.250290310188348464, 5.569163095287620990, 0.7216878364870438212 ) ) ;
#118820 = CARTESIAN_POINT ( 'NONE',  ( 11.89942855770813956, 9.799999999999998934, -0.7000000000000009548 ) ) ;
#118819 = CARTESIAN_POINT ( 'NONE',  ( 4.167152111353856547, 5.955039778036558040, 1.599625672291262513 ) ) ;
#118822 = CARTESIAN_POINT ( 'NONE',  ( 11.97929049433705373, 9.719999999999998863, 0.7046979865771783036 ) ) ;
#118823 = CARTESIAN_POINT ( 'NONE',  ( 6.421112215724263272, -1.799107166270615732, 0.9110519380226205222 ) ) ;
#118824 =( BOUNDED_SURFACE ( )  B_SPLINE_SURFACE ( 3, 2, ( 
 ( #2741, #50462, #116581 ),
 ( #167414, #182576, #117659 ),
 ( #35256, #19005, #85086 ),
 ( #140280, #39539, #40628 ) ),
 .UNSPECIFIED., .F., .F., .F. ) 
 B_SPLINE_SURFACE_WITH_KNOTS ( ( 4, 4 ),
 ( 3, 3 ),
 ( 0.0002736160683302315730, 0.001000278046670501726 ),
 ( 0.000000000000000000, 1.000000000000000000 ),
 .UNSPECIFIED. ) 
 GEOMETRIC_REPRESENTATION_ITEM ( )  RATIONAL_B_SPLINE_SURFACE ( (
 ( 1.000000000000000000, 0.6273451206645928035, 1.000000000000000000),
 ( 1.000000000000000000, 0.6198151287834093859, 1.000000000000000000),
 ( 1.000000000000000000, 0.6183718462548107864, 1.000000000000000000),
 ( 1.000000000000000000, 0.6222643257228465119, 1.000000000000000000) ) ) 
 REPRESENTATION_ITEM ( '' )  SURFACE ( )  );
#118825 = CARTESIAN_POINT ( 'NONE',  ( -8.690413276679693766, 9.241163032322203819, 1.040834085586084257E-14 ) ) ;
#118826 = CARTESIAN_POINT ( 'NONE',  ( 1.347511689332027807, 0.6317163119916607839, -2.098556723903362009 ) ) ;
#118827 = CARTESIAN_POINT ( 'NONE',  ( 0.000000000000000000, 0.000000000000000000, 0.000000000000000000 ) ) ;
#118829 = CARTESIAN_POINT ( 'NONE',  ( -1.402160292154681736E-14, 12.42187500034139802, 1.575800808251682339 ) ) ;
#118828 = CARTESIAN_POINT ( 'NONE',  ( 1.270828881381684150, -1.433710284283566949, 1.750253757905173124 ) ) ;
#118830 = CARTESIAN_POINT ( 'NONE',  ( -7.648771216403934758, 12.07531685244661723, -0.7998128361456291469 ) ) ;
#118831 = CARTESIAN_POINT ( 'NONE',  ( -5.883875478206491927, 5.966868934103426447, 0.000000000000000000 ) ) ;
#118832 = CARTESIAN_POINT ( 'NONE',  ( -1.201851678989727383E-14, 2.634375000341417916, 1.575800808251672791 ) ) ;
#118833 = CARTESIAN_POINT ( 'NONE',  ( 4.635702676548680401, 8.322458603728597026, -0.3981331281527732968 ) ) ;
#118834 = CARTESIAN_POINT ( 'NONE',  ( 0.7500000000000006661, 9.833333333333332149, 1.299038105676657340 ) ) ;
#118835 = CARTESIAN_POINT ( 'NONE',  ( 3.562884411436726850, -1.522066076379503974, -0.8114761229951471533 ) ) ;
#118836 = CARTESIAN_POINT ( 'NONE',  ( 3.542423274920540432, 7.354853930707762721, -1.734723475976807094E-15 ) ) ;
#118837 =( BOUNDED_CURVE ( )  B_SPLINE_CURVE ( 2, ( #121306, #187282, #179573, #159054, #176378, #79920, #43197, #10648, #175321 ),
 .UNSPECIFIED., .F., .T. ) 
 B_SPLINE_CURVE_WITH_KNOTS ( ( 3, 2, 2, 2, 3 ),
 ( 0.7946428571428572063, 0.7976190476190476719, 0.8035714285714286031, 0.8095238095238095344, 0.8125000000000000000 ),
 .UNSPECIFIED. ) 
 CURVE ( )  GEOMETRIC_REPRESENTATION_ITEM ( )  RATIONAL_B_SPLINE_CURVE ( ( 0.9330127018922194093, 0.9330127018922206306, 1.000000000000000000, 0.8660254037844387076, 1.000000000000000000, 0.8660254037844387076, 1.000000000000000000, 0.9330127018922194093, 0.9330127018922194093 ) ) 
 REPRESENTATION_ITEM ( '' )  );
#118838 = CARTESIAN_POINT ( 'NONE',  ( 2.196244507144041513, -0.4668761045134894871, -1.706985182271273382 ) ) ;
#118839 = AXIS2_PLACEMENT_3D ( 'NONE', #28921, #110237, #95006 ) ;
#118840 = CARTESIAN_POINT ( 'NONE',  ( 2.789700014133191797, 1.910882804325767070, -0.6334545493084097201 ) ) ;
#118841 = CARTESIAN_POINT ( 'NONE',  ( 10.72180055030867329, 11.40318881831530540, 0.7998128361456341429 ) ) ;
#118842 = CARTESIAN_POINT ( 'NONE',  ( 5.473716482686670659, 2.128106746890707335, -0.5837492795209007213 ) ) ;
#118843 = STYLED_ITEM ( 'NONE', ( #159280 ), #54459 ) ;
#118844 = ORIENTED_EDGE ( 'NONE', *, *, #89525, .T. ) ;
#118845 = CARTESIAN_POINT ( 'NONE',  ( 4.500263427444707531, -0.9482861330638262531, 1.783302102689677371 ) ) ;
#118846 = CARTESIAN_POINT ( 'NONE',  ( -5.912237504011027767, 9.055304967058290799, 1.199719254218454489 ) ) ;
#118847 = CARTESIAN_POINT ( 'NONE',  ( 3.515250061227533696, -1.862011288300661871, 0.7743320027404425598 ) ) ;
#118849 = VERTEX_POINT ( 'NONE', #87700 ) ;
#118848 = CARTESIAN_POINT ( 'NONE',  ( 4.289189881116685754, -0.006549295265783834294, -1.811767228872669389 ) ) ;
#118850 = CARTESIAN_POINT ( 'NONE',  ( 3.045614982896325262, 0.6747646648952825288, -1.744891315567910439 ) ) ;
#118851 = DIRECTION ( 'NONE',  ( 0.000000000000000000, 1.000000000000000000, 0.000000000000000000 ) ) ;
#118852 = CARTESIAN_POINT ( 'NONE',  ( 2.179812656587180264, 1.874749209517186710, -0.3766967574026017229 ) ) ;
#118853 = LINE ( 'NONE', #86293, #167739 ) ;
#118854 = CARTESIAN_POINT ( 'NONE',  ( -10.65086514279933994, 4.118349190211191058, -6.883315229069521202 ) ) ;
#118855 = DIRECTION ( 'NONE',  ( 1.000000000000000000, 0.000000000000000000, -3.491481338843133355E-15 ) ) ;
#118856 = CARTESIAN_POINT ( 'NONE',  ( -1.364683531250012516, 3.592708333674750509, 0.7879004041258379498 ) ) ;
#118857 = CARTESIAN_POINT ( 'NONE',  ( 0.1934256698341470238, 1.783621342183003389, -0.6902995980747894667 ) ) ;
#118858 = CARTESIAN_POINT ( 'NONE',  ( 5.058600711674583472, 8.915801573680086634, 0.000000000000000000 ) ) ;
#118859 = CARTESIAN_POINT ( 'NONE',  ( 1.451531895509536874, 1.483362660712842063, 1.284035263222626844 ) ) ;
#118860 = CARTESIAN_POINT ( 'NONE',  ( 1.812013678032661668, -0.3846686717400226163, 0.6718421233638880441 ) ) ;
#118861 = EDGE_CURVE ( 'NONE', #154420, #213687, #187170, .T. ) ;
#118862 = CARTESIAN_POINT ( 'NONE',  ( -4.776215253764153346, 8.794277906025310898, -0.7998128361456362523 ) ) ;
#118863 = CARTESIAN_POINT ( 'NONE',  ( 5.431924468521282634, -2.068440459917933794, 0.4666711972392265650 ) ) ;
#118865 = CARTESIAN_POINT ( 'NONE',  ( -10.60630082101195804, 5.715768461961713953, -4.896526734066639186 ) ) ;
#118864 = CARTESIAN_POINT ( 'NONE',  ( 9.531545685607134999, 11.07889037375188401, 1.199719254218450271 ) ) ;
#118866 = CARTESIAN_POINT ( 'NONE',  ( 5.729747329291909885, -1.248464225167019714, -1.525673545143470200 ) ) ;
#118867 = CARTESIAN_POINT ( 'NONE',  ( -0.6823417656250212460, 1.051041667008083325, 1.181850606188755259 ) ) ;
#118868 = CARTESIAN_POINT ( 'NONE',  ( 0.9670423206251937964, -1.584547017232017518, 1.241716394148101088 ) ) ;
#118869 = VERTEX_POINT ( 'NONE', #88785 ) ;
#118870 = CARTESIAN_POINT ( 'NONE',  ( 1.089646232962078853, -0.5102306600231114597, 2.054730298310704750 ) ) ;
#118871 = CARTESIAN_POINT ( 'NONE',  ( 11.80022143584854710, 6.865729006526965605, 1.951202288423556919 ) ) ;
#118872 = CARTESIAN_POINT ( 'NONE',  ( 2.594261239525695206, 0.9781076984213372683, -1.824767828009652426 ) ) ;
#118873 = CARTESIAN_POINT ( 'NONE',  ( 3.691562964670865199, 7.528850235416478576, -0.7998128361456362523 ) ) ;
#118874 = CARTESIAN_POINT ( 'NONE',  ( 6.710359684120930091, 6.793450817754725257, 0.7998128361456352531 ) ) ;
#118875 = ORIENTED_EDGE ( 'NONE', *, *, #158609, .F. ) ;
#118877 = CARTESIAN_POINT ( 'NONE',  ( 5.027376032568989572, 4.759693547618927489, 0.7998128361456341429 ) ) ;
#118876 = CARTESIAN_POINT ( 'NONE',  ( 4.417973705048302335, 1.286473518301757712, -1.647865739169761978 ) ) ;
#118880 = EDGE_LOOP ( 'NONE', ( #92765, #13336, #72150, #104611 ) ) ;
#118879 = CARTESIAN_POINT ( 'NONE',  ( 1.892921280605066370, -0.08938092231483388272, -1.809401395368259280 ) ) ;
#118878 = CARTESIAN_POINT ( 'NONE',  ( 3.293790705515726280, -0.7410340593078695859, 1.668602820345471027 ) ) ;
#118881 = CARTESIAN_POINT ( 'NONE',  ( 6.445939570963195031, 0.8488519614954294079, -2.037301952897092594 ) ) ;
#118882 = DIRECTION ( 'NONE',  ( 0.000000000000000000, 0.000000000000000000, 1.000000000000000000 ) ) ;
#118883 = CARTESIAN_POINT ( 'NONE',  ( 10.13617411650462330, 13.69189752474445321, 7.314094131634138130 ) ) ;
#118884 = CARTESIAN_POINT ( 'NONE',  ( 5.333140672905051893, 0.1575165696711364749, 2.201206011701982934 ) ) ;
#118885 = CARTESIAN_POINT ( 'NONE',  ( -1.364683531250010740, 9.192708333674731946, 0.7879004041258445001 ) ) ;
#118886 = EDGE_CURVE ( 'NONE', #53408, #61933, #43116, .T. ) ;
#118887 = ORIENTED_EDGE ( 'NONE', *, *, #68041, .F. ) ;
#118888 = CARTESIAN_POINT ( 'NONE',  ( 4.494721087910216184, -1.855708629272670773, -0.4612273479895279138 ) ) ;
#118889 = CARTESIAN_POINT ( 'NONE',  ( -3.379006598303881059, 4.965260336153046516, -1.599625672291256295 ) ) ;
#118890 =( BOUNDED_CURVE ( )  B_SPLINE_CURVE ( 1, ( #148284, #99525 ),
 .UNSPECIFIED., .F., .T. ) 
 B_SPLINE_CURVE_WITH_KNOTS ( ( 2, 2 ),
 ( 0.000000000000000000, 6.249999999999788711E-05 ),
 .UNSPECIFIED. ) 
 CURVE ( )  GEOMETRIC_REPRESENTATION_ITEM ( )  RATIONAL_B_SPLINE_CURVE ( ( 0.9345202395942819873, 0.9345202395942819873 ) ) 
 REPRESENTATION_ITEM ( '' )  );
#118891 = CARTESIAN_POINT ( 'NONE',  ( 8.229962938695207342, 9.560377169021284871, 1.199719254218462483 ) ) ;
#118892 = CARTESIAN_POINT ( 'NONE',  ( 6.707487347292075519, -1.660346423639452951, -1.236579608897829363 ) ) ;
#118893 = CARTESIAN_POINT ( 'NONE',  ( -0.6801582343750438575, 0.7135416670080579893, 1.178068619123810334 ) ) ;
#118894 = CARTESIAN_POINT ( 'NONE',  ( 5.165293336682183600, 5.128523102325077687, -0.7216878364870197293 ) ) ;
#118895 = CARTESIAN_POINT ( 'NONE',  ( -5.587017333170084754, 5.816630895727369577, 0.4567169512200538461 ) ) ;
#118896 = CARTESIAN_POINT ( 'NONE',  ( 5.253852870291571442, 7.792406146126436006, -1.285611862062207011 ) ) ;
#118897 = CARTESIAN_POINT ( 'NONE',  ( -7.090402625748199128, 15.44810097730825760, -9.636366487198095854 ) ) ;
#118898 = FACE_OUTER_BOUND ( 'NONE', #163880, .T. ) ;
#118899 = CARTESIAN_POINT ( 'NONE',  ( 3.303821147848403861, -1.868562489643767144, 0.08839296284299941187 ) ) ;
#118900 = CARTESIAN_POINT ( 'NONE',  ( 3.791513125430877373, 7.352524219418101303, -0.3677586026353037996 ) ) ;
#118901 = CARTESIAN_POINT ( 'NONE',  ( -0.2409995289980245703, 0.2355275985303668385, -2.034371242098035548 ) ) ;
#118902 = AXIS2_PLACEMENT_3D ( 'NONE', #46993, #96819, #28595 ) ;
#118903 = CARTESIAN_POINT ( 'NONE',  ( -6.019457014787517046, 9.006155036351978893, 1.082531754730548412 ) ) ;
#118904 = CARTESIAN_POINT ( 'NONE',  ( 3.061108821635398769, 6.793320401875094561, -0.7998128361456362523 ) ) ;
#118905 = CARTESIAN_POINT ( 'NONE',  ( 5.392392409933256303, 7.314210449720692786, 1.599625672291267398 ) ) ;
#118906 = CARTESIAN_POINT ( 'NONE',  ( 6.526242037438201749, 1.059062773735760521, 1.778703558766213000 ) ) ;
#118907 = CARTESIAN_POINT ( 'NONE',  ( 0.8257962581623284892, 0.8146080751335778025, -1.844719337431327544 ) ) ;
#118908 = VECTOR ( 'NONE', #76055, 1000.000000000000000 ) ;
#118909 = CARTESIAN_POINT ( 'NONE',  ( -9.267161690140662600, 10.77044237904097734, -1.199719254218441611 ) ) ;
#118910 = CARTESIAN_POINT ( 'NONE',  ( 5.332099551924443404, 9.442809587212341427, 0.000000000000000000 ) ) ;
#118912 = EDGE_CURVE ( 'NONE', #184258, #74569, #30200, .T. ) ;
#118911 = DIRECTION ( 'NONE',  ( 0.6507913734559658270, -0.7592566023652989049, 0.000000000000000000 ) ) ;
#118913 = CARTESIAN_POINT ( 'NONE',  ( 0.9025786099917804117, 1.657183926254527595, -1.434042119274607563 ) ) ;
#118914 = CARTESIAN_POINT ( 'NONE',  ( 6.252569598636129378, 0.5776572744066663656, 1.731972519516040032 ) ) ;
#118915 = CARTESIAN_POINT ( 'NONE',  ( -3.379006598303881059, 4.965260336153046516, -1.599625672291256295 ) ) ;
#118916 = EDGE_CURVE ( 'NONE', #9078, #161735, #152702, .T. ) ;
#118917 = CARTESIAN_POINT ( 'NONE',  ( 4.245111494854632461, 7.966730820723463502, 0.000000000000000000 ) ) ;
#118918 = CARTESIAN_POINT ( 'NONE',  ( 8.536830278099042602, 13.11138575775759563, -0.7998128361456352531 ) ) ;
#118919 = MECHANICAL_DESIGN_GEOMETRIC_PRESENTATION_REPRESENTATION (  '', ( #191040 ), #63047 ) ;
#118920 = CARTESIAN_POINT ( 'NONE',  ( 4.650610384687404952, 5.384465856012134566, 1.199719254218462483 ) ) ;
#118921 = CARTESIAN_POINT ( 'NONE',  ( 3.553118775233146120, 6.302999783484076524, -1.199719254218453823 ) ) ;
#118922 = EDGE_LOOP ( 'NONE', ( #126546, #2972, #44508 ) ) ;
#118924 = CARTESIAN_POINT ( 'NONE',  ( 0.8209481077818219230, 1.523044454047136176, -1.316462280350006342 ) ) ;
#118923 = CARTESIAN_POINT ( 'NONE',  ( 4.300242120186610784, 1.420457692841030850, -1.171515996850613694 ) ) ;
#118925 = CARTESIAN_POINT ( 'NONE',  ( 2.337686028923485537, -1.414513361329417851, 1.811461888080208027 ) ) ;
#118927 = CARTESIAN_POINT ( 'NONE',  ( 0.4439182389155779673, -0.8842316343482552465, 1.637490449460777153 ) ) ;
#118926 = CARTESIAN_POINT ( 'NONE',  ( 5.029711800989886683, 4.970344644017389513, 1.040834085586084257E-14 ) ) ;
#118928 = CARTESIAN_POINT ( 'NONE',  ( -1.642778471874998480, -3.551041666188709645, 2.845375778867863303 ) ) ;
#118929 = CARTESIAN_POINT ( 'NONE',  ( -3.554208825076827782, 7.298327395898266623, 0.7998128361456341429 ) ) ;
#118930 = CARTESIAN_POINT ( 'NONE',  ( -9.439063867296153987, 14.51206345749796256, -7.409881739176208626 ) ) ;
#118931 = CARTESIAN_POINT ( 'NONE',  ( 4.711142613322857109, 1.586760866459841379, -1.067142987418716604 ) ) ;
#118932 = CARTESIAN_POINT ( 'NONE',  ( -9.755255220232635693, 11.33988483081495957, -1.199719254218441611 ) ) ;
#118933 = CARTESIAN_POINT ( 'NONE',  ( 6.373787108001086388, 6.824503602047865769, -0.5760177672454840359 ) ) ;
#118934 = CARTESIAN_POINT ( 'NONE',  ( -5.478903473698247595, 8.445785581739666981, -1.082531754730549967 ) ) ;
#118936 = CARTESIAN_POINT ( 'NONE',  ( 1.867826558377215118, 0.9591755677602131769, 1.605880698980370225 ) ) ;
#118935 = CARTESIAN_POINT ( 'NONE',  ( 4.089459622424143070, -0.7983975988373869237, 1.932503512935821011 ) ) ;
#118937 = CARTESIAN_POINT ( 'NONE',  ( 8.934460041725669655, 9.525884258209195821, 1.040834085586084257E-14 ) ) ;
#118938 = CARTESIAN_POINT ( 'NONE',  ( 1.364683531249990311, 5.196875000341417916, 1.214306433183764966E-14 ) ) ;
#118939 = CARTESIAN_POINT ( 'NONE',  ( 3.175097308692858444, 1.106666961078702771, 1.343256515094106041 ) ) ;
#118940 = CARTESIAN_POINT ( 'NONE',  ( 4.792970997630896512, 5.550553237779539018, 1.199719254218464037 ) ) ;
#118942 = CARTESIAN_POINT ( 'NONE',  ( -15.75000000000000000, 10.90000000000000036, 0.6999999999999992895 ) ) ;
#118941 = CARTESIAN_POINT ( 'NONE',  ( -5.561176828107109671, 5.894252131381872317, 0.6462735908731042089 ) ) ;
#118943 = CARTESIAN_POINT ( 'NONE',  ( 3.703458238649427692, -0.4988927697323896071, 1.651148375757867326 ) ) ;
#118944 = CARTESIAN_POINT ( 'NONE',  ( -5.391338639728555648, 9.441645512991978961, -0.7998128361456231517 ) ) ;
#118945 = CARTESIAN_POINT ( 'NONE',  ( 3.896163805485418852, -0.6886730243073329039, -2.080591098665984795 ) ) ;
#118946 = CARTESIAN_POINT ( 'NONE',  ( 6.727182134110200273, -0.004969159814478123736, 2.189081792362323586 ) ) ;
#118947 = DIRECTION ( 'NONE',  ( 5.551115123125765446E-17, 0.000000000000000000, -1.000000000000000000 ) ) ;
#118948 = CARTESIAN_POINT ( 'NONE',  ( 3.415042003188377251, -1.647272610417279015, 1.414370313860166872 ) ) ;
#118949 = CARTESIAN_POINT ( 'NONE',  ( 2.086296903703276140, -1.790263230197926436, -0.3570169370194844483 ) ) ;
#118950 = CARTESIAN_POINT ( 'NONE',  ( 0.000000000000000000, 19.00000000000000000, 11.92000000000000171 ) ) ;
#118951 = CARTESIAN_POINT ( 'NONE',  ( 4.294233728257051297, -0.9087460953031538669, -1.912572187454407047 ) ) ;
#118952 = ORIENTED_EDGE ( 'NONE', *, *, #37494, .F. ) ;
#118954 = CARTESIAN_POINT ( 'NONE',  ( 1.364683531249986537, 2.717708333674754062, -0.7879004041258239610 ) ) ;
#118953 = CARTESIAN_POINT ( 'NONE',  ( 4.335649905164426166, 0.9806507323757740480, -2.072138663387664614 ) ) ;
#118955 = CARTESIAN_POINT ( 'NONE',  ( 6.720655732516657821, 4.700665033810172311, 2.388972926809574737 ) ) ;
#118956 = CARTESIAN_POINT ( 'NONE',  ( 3.837121167867449945, 4.435395103055503441, 1.199719254218464037 ) ) ;
#118957 = CARTESIAN_POINT ( 'NONE',  ( 0.9617728337494994006, -1.673954878106189703, -1.301583125534570673 ) ) ;
#118958 = CARTESIAN_POINT ( 'NONE',  ( -4.690757960648240577, 6.495636925554817864, 1.443375672974064550 ) ) ;
#118959 = DIRECTION ( 'NONE',  ( 0.000000000000000000, 1.000000000000000000, 0.000000000000000000 ) ) ;
#118960 = CARTESIAN_POINT ( 'NONE',  ( -4.053524740361572398, 7.672936597156388316, 0.7216878364870317197 ) ) ;
#118962 = CARTESIAN_POINT ( 'NONE',  ( -1.500000000000001110, 12.05208333401613352, 0.8660254037844419273 ) ) ;
#118961 = CARTESIAN_POINT ( 'NONE',  ( -10.91804383151493241, -9.900000000000074962, 0.1905751639682748966 ) ) ;
#118963 = ORIENTED_EDGE ( 'NONE', *, *, #182421, .F. ) ;
#118964 = CARTESIAN_POINT ( 'NONE',  ( 6.381482430641396419, -0.5404875331735843336, -1.942542459342583294 ) ) ;
#118966 = CARTESIAN_POINT ( 'NONE',  ( 4.504768599022889397, 0.5450402360923761735, 1.989220403428487938 ) ) ;
#118965 = CARTESIAN_POINT ( 'NONE',  ( 2.835626683552519012, 6.459981564119914310, 0.000000000000000000 ) ) ;
#118968 = CARTESIAN_POINT ( 'NONE',  ( -0.2409995289980246813, 5.721856934700204178, -2.594540323675114113 ) ) ;
#118967 = CARTESIAN_POINT ( 'NONE',  ( 5.494797395288433250, 9.632623737803665875, 0.000000000000000000 ) ) ;
#118969 = CARTESIAN_POINT ( 'NONE',  ( 7.225569521440261767, 7.394528961293920233, -0.7998128361456341429 ) ) ;
#118970 = CARTESIAN_POINT ( 'NONE',  ( 1.642778471875001811, -0.6927083328553753638, 2.845375778867859751 ) ) ;
#118971 = CARTESIAN_POINT ( 'NONE',  ( 0.1331565106231363538, 7.629137130509071163, -2.545925718843544239 ) ) ;
#118972 = CARTESIAN_POINT ( 'NONE',  ( 0.5332922803617061724, -1.479851573012560761, -1.477019686621689143 ) ) ;
#118973 = CARTESIAN_POINT ( 'NONE',  ( 4.711564657724523819, 1.930417226389494090, 0.5826574956761670920 ) ) ;
#118974 = CARTESIAN_POINT ( 'NONE',  ( 4.722110844128335039, 1.763445737372179689, 0.5296355584529164329 ) ) ;
#118975 = CARTESIAN_POINT ( 'NONE',  ( 5.035963992472171746, 7.962709526937818083, 1.199719254218462483 ) ) ;
#118976 = CARTESIAN_POINT ( 'NONE',  ( 1.131409910074301806, -1.089654060068695252, -1.336973495911207843 ) ) ;
#118977 = CARTESIAN_POINT ( 'NONE',  ( 0.3390778084843976137, -1.706115258973059490, -1.074657883261991076 ) ) ;
#118978 = CARTESIAN_POINT ( 'NONE',  ( 1.161203735943004300, 1.374334461307982425, 1.842484299438088557 ) ) ;
#118979 = CARTESIAN_POINT ( 'NONE',  ( -4.903245109636583443, 8.872203061218007392, -0.7998128361456281477 ) ) ;
#118980 = CARTESIAN_POINT ( 'NONE',  ( 0.8435138722653515719, -1.939887490614403687, 1.163926157780611925 ) ) ;
#118981 = CARTESIAN_POINT ( 'NONE',  ( 3.492891347888595455, -0.4109570828031941514, -2.065403110348571492 ) ) ;
#118982 = CARTESIAN_POINT ( 'NONE',  ( -5.635349125135588721, 6.603604063193491136, 1.199719254218452935 ) ) ;
#118983 = CARTESIAN_POINT ( 'NONE',  ( 8.613507663383630941, 8.943513783569379427, -0.7998128361456221525 ) ) ;
#118985 = EDGE_CURVE ( 'NONE', #122503, #132208, #176825, .T. ) ;
#118984 = CARTESIAN_POINT ( 'NONE',  ( 6.875393295461478260, 8.154285278527437342, -1.082531754730548412 ) ) ;
#118986 = CARTESIAN_POINT ( 'NONE',  ( 6.062500000000003553, -1.451031289061355478, -1.451031289060867868 ) ) ;
#118987 = CARTESIAN_POINT ( 'NONE',  ( -6.735703387890906946, 6.752742128827836865, -0.7998128361456291469 ) ) ;
#118988 = CARTESIAN_POINT ( 'NONE',  ( 6.439759776366775768, 7.575769829591800786, 1.082531754730558626 ) ) ;
#118989 = CARTESIAN_POINT ( 'NONE',  ( 4.401803827585060169, 7.348580664174646060, 1.190671039528957253 ) ) ;
#118990 = CARTESIAN_POINT ( 'NONE',  ( -4.959585264500673496, 4.680604318205876524, 1.214306433183764966E-14 ) ) ;
#118991 = CARTESIAN_POINT ( 'NONE',  ( 4.728890529236228879, 1.530954898644999451, -1.609847601234422276 ) ) ;
#118992 = CARTESIAN_POINT ( 'NONE',  ( 2.677880624963273171, -1.125664371729949265, 1.880105217535378959 ) ) ;
#118993 = CARTESIAN_POINT ( 'NONE',  ( -6.087774667736030487, 7.061157519568837415, 1.199719254218450271 ) ) ;
#118994 = CARTESIAN_POINT ( 'NONE',  ( -5.157951095356222204, 4.982307464195829816, 0.000000000000000000 ) ) ;
#118995 = CARTESIAN_POINT ( 'NONE',  ( 5.881297811770386907, -0.04968318840743202180, 1.961410508136133712 ) ) ;
#118996 = CIRCLE ( 'NONE', #18578, 0.07999999999999997391 ) ;
#118997 = CARTESIAN_POINT ( 'NONE',  ( 1.364683531249988757, 1.384375000341421469, 0.000000000000000000 ) ) ;
#118998 = CARTESIAN_POINT ( 'NONE',  ( -3.469446951953614189E-15, 8.999999999999998224, -2.420000000000000373 ) ) ;
#119000 = ORIENTED_EDGE ( 'NONE', *, *, #39457, .F. ) ;
#118999 = CARTESIAN_POINT ( 'NONE',  ( -5.748293942514189681, 5.808690475795744490, -0.7216878364870207285 ) ) ;
#119001 = CARTESIAN_POINT ( 'NONE',  ( 4.676102344489991403, 2.097148071331572439, -0.3138259731317455392 ) ) ;
#119002 = CARTESIAN_POINT ( 'NONE',  ( -5.804299160426224624, 9.785783097223662352, -0.7216878364870338292 ) ) ;
#119003 = VERTEX_POINT ( 'NONE', #69290 ) ;
#119005 = CARTESIAN_POINT ( 'NONE',  ( 6.508665849870632236, 1.605377118863276387, -1.447859449074364591 ) ) ;
#119004 = CARTESIAN_POINT ( 'NONE',  ( -5.885648082108231982, 7.959951743916638733, 1.443375672974058777 ) ) ;
#119006 = CARTESIAN_POINT ( 'NONE',  ( 5.982172092127724383, 8.002286745614243912, -1.599625672291262513 ) ) ;
#119007 = CARTESIAN_POINT ( 'NONE',  ( 5.601068772352080671, -0.4412860211496574814, 1.787476196608045464 ) ) ;
#119008 = SURFACE_SIDE_STYLE ('',( #133092 ) ) ;
#119009 = CARTESIAN_POINT ( 'NONE',  ( -1.364683531250000748, 2.321875000341422357, 1.214306433183764966E-14 ) ) ;
#119010 = CARTESIAN_POINT ( 'NONE',  ( 1.241335265265028687, 1.738410175110545852, 0.08621907427421551806 ) ) ;
#119011 = CARTESIAN_POINT ( 'NONE',  ( 11.44779964734710909, 12.60189529870400804, 3.599999963171362616 ) ) ;
#119012 = CARTESIAN_POINT ( 'NONE',  ( -1.402160292154681736E-14, -0.9906249996585834161, -1.575800808251665908 ) ) ;
#119013 = CARTESIAN_POINT ( 'NONE',  ( 11.39743721391019626, 7.463254518212971256, -3.780308495066197594 ) ) ;
#119014 = CARTESIAN_POINT ( 'NONE',  ( 5.787991602622606813, -0.9759734195362681497, 1.928925553883020338 ) ) ;
#119015 = CARTESIAN_POINT ( 'NONE',  ( -4.460796234096120472, 5.163016013655583158, 1.199719254218462483 ) ) ;
#119016 = CARTESIAN_POINT ( 'NONE',  ( -5.856759170979136897, 9.776710099543576504, 0.000000000000000000 ) ) ;
#119017 = CARTESIAN_POINT ( 'NONE',  ( 4.715790015261832835, -2.120648752638915724, 0.4184459369844309440 ) ) ;
#119018 = CARTESIAN_POINT ( 'NONE',  ( 1.364683531249988535, 3.363541667008084879, 0.7879004041258500513 ) ) ;
#119019 = CARTESIAN_POINT ( 'NONE',  ( 4.692626201678701925, -0.4289087433139714411, -1.923991814828669433 ) ) ;
#119020 = CARTESIAN_POINT ( 'NONE',  ( 3.813592814792550190, -1.418126570600848124, 0.9972168832048341480 ) ) ;
#119021 = CARTESIAN_POINT ( 'NONE',  ( 0.7322823680011962821, 2.160084099745246178, 0.3691886501416344335 ) ) ;
#119022 = CARTESIAN_POINT ( 'NONE',  ( 2.028779783278670035, 1.327905328797769569, -1.887045328260747112 ) ) ;
#119023 = CARTESIAN_POINT ( 'NONE',  ( 5.114554592455347048, 1.424167462454002608, -1.489711086068323587 ) ) ;
#119024 = CARTESIAN_POINT ( 'NONE',  ( 6.286669113786358842, 1.687405947569386999, -0.9612952809280647104 ) ) ;
#119025 = CARTESIAN_POINT ( 'NONE',  ( -7.497295758232731089, 8.809561808435409702, -1.082531754730543083 ) ) ;
#119026 = CARTESIAN_POINT ( 'NONE',  ( -5.438755897737433287, 6.374245297895642537, -1.199719254218453823 ) ) ;
#119027 = CARTESIAN_POINT ( 'NONE',  ( 0.8795299900376440938, -0.4926441280813895762, -1.955172062459666904 ) ) ;
#119028 = CARTESIAN_POINT ( 'NONE',  ( -5.219525951136837705, 9.033271343060892633, -0.7216878364870207285 ) ) ;
#119029 = CARTESIAN_POINT ( 'NONE',  ( 3.153566124713353513, -1.803153744294363481, -1.271922660818012973 ) ) ;
#119030 = CARTESIAN_POINT ( 'NONE',  ( 3.285556943750000514, -1.451041666188708890, 1.896917185911906500 ) ) ;
#119031 = CARTESIAN_POINT ( 'NONE',  ( 1.164654898877310885, 1.413799132238046985, -1.210232755764220069 ) ) ;
#119032 = CARTESIAN_POINT ( 'NONE',  ( 1.737499999999999378, -1.822916665710751172, -3.009438278150925683 ) ) ;
#119033 = CARTESIAN_POINT ( 'NONE',  ( -7.720982897393577460, -6.307829212974239042, 7.834948825496934610 ) ) ;
#119034 = CARTESIAN_POINT ( 'NONE',  ( -9.499668754586236830, -7.643695121331953501, -0.07933191752404977759 ) ) ;
#119036 = CARTESIAN_POINT ( 'NONE',  ( 6.925078400183513949, 3.679108800414055302, 2.758152782261179325 ) ) ;
#119035 = CARTESIAN_POINT ( 'NONE',  ( -4.638114411034067963, 8.432649648999159808, -0.4721908680582111995 ) ) ;
#119037 = CARTESIAN_POINT ( 'NONE',  ( 6.017501326166345699, -1.026660802952833240, -1.528114487065170390 ) ) ;
#119038 = VERTEX_POINT ( 'NONE', #6427 ) ;
#119039 = CARTESIAN_POINT ( 'NONE',  ( 2.940362659251498645, 2.045167860313545916, 0.2535661900368457733 ) ) ;
#119040 = CARTESIAN_POINT ( 'NONE',  ( 1.360316468749955598, 1.536458333674721288, -0.7853790794159342115 ) ) ;
#119041 = CARTESIAN_POINT ( 'NONE',  ( -5.636439174979254396, 7.598931675607687453, -1.599625672291256295 ) ) ;
#119042 = CARTESIAN_POINT ( 'NONE',  ( 2.033858944562048965, -1.958440182618191416, 0.4929867953931149627 ) ) ;
#119043 = CARTESIAN_POINT ( 'NONE',  ( -1.402160292154681736E-14, -0.4124999999999747202, -1.732050807568870754 ) ) ;
#119044 = CARTESIAN_POINT ( 'NONE',  ( 4.695201269034174452, 4.372156323494968966, 1.214306433183764966E-14 ) ) ;
#119045 = CARTESIAN_POINT ( 'NONE',  ( 2.079048039887823052, -0.09986672515850322784, -2.058587512739398662 ) ) ;
#119047 = CARTESIAN_POINT ( 'NONE',  ( -1.364683531250000748, 12.85937500034139980, 0.000000000000000000 ) ) ;
#119046 = CARTESIAN_POINT ( 'NONE',  ( -1.451998047845039830, 7.315968950354585942, -4.301760722576429607 ) ) ;
#119048 = CARTESIAN_POINT ( 'NONE',  ( 6.928380191783277908, 8.041863964290678624, 1.199719254218462483 ) ) ;
#119049 = CARTESIAN_POINT ( 'NONE',  ( -0.2409995289980246258, 1.355929887833319469, -2.254219809973062816 ) ) ;
#119050 = CARTESIAN_POINT ( 'NONE',  ( 5.074942902252104204, -2.077123540546990110, -0.7459609299403434646 ) ) ;
#119051 = CARTESIAN_POINT ( 'NONE',  ( 1.739762150092131643, -1.564342989677082629, -1.491970722459233345 ) ) ;
#119052 = CARTESIAN_POINT ( 'NONE',  ( -4.392478581147607031, 7.108013530438723748, 1.082531754730560403 ) ) ;
#119053 = CARTESIAN_POINT ( 'NONE',  ( 0.4972802279516430612, -0.2910764605805628014, 1.995268990643041640 ) ) ;
#119054 = EDGE_CURVE ( 'NONE', #171893, #123409, #171271, .T. ) ;
#119055 = CARTESIAN_POINT ( 'NONE',  ( 2.021309514094786763, 2.292189817666248075, -0.1691314976695507954 ) ) ;
#119056 = CYLINDRICAL_SURFACE ( 'NONE', #115061, 1.224999999999996980 ) ;
#119057 = EDGE_CURVE ( 'NONE', #172976, #186393, #88983, .T. ) ;
#119058 = CARTESIAN_POINT ( 'NONE',  ( -1.806654366501805775, 0.000000000000000000, 2.500000000000000444 ) ) ;
#119059 = CARTESIAN_POINT ( 'NONE',  ( 1.858560999665780145, 8.965769984707671725, -0.7749999999999996891 ) ) ;
#119060 = STYLED_ITEM ( 'NONE', ( #154898 ), #115976 ) ;
#119061 = CARTESIAN_POINT ( 'NONE',  ( 2.254581950620972997, -1.447608085528677480, 1.184820545849271767 ) ) ;
#119062 = CARTESIAN_POINT ( 'NONE',  ( 3.661342437515973547, 1.897110692972364454, -0.6839366698164971448 ) ) ;
#119064 = CARTESIAN_POINT ( 'NONE',  ( 11.52469724861193612, 13.87999993351185068, 3.346365485506901827 ) ) ;
#119063 = CARTESIAN_POINT ( 'NONE',  ( -1.402160292154681736E-14, 1.446875000341420137, -1.575800808251659024 ) ) ;
#119066 = CARTESIAN_POINT ( 'NONE',  ( 5.391282926306558032, 1.858022621660906371, -0.9916069233004040084 ) ) ;
#119065 = CARTESIAN_POINT ( 'NONE',  ( -5.879432169820529630, 10.01108796476595764, -0.7998128361456221525 ) ) ;
#119067 = PRESENTATION_LAYER_ASSIGNMENT (  '', '', ( #150089 ) ) ;
#119068 = CARTESIAN_POINT ( 'NONE',  ( 8.118635056484817980, 8.366162408854107113, 0.7998128361456481317 ) ) ;
#119070 = CARTESIAN_POINT ( 'NONE',  ( -6.527360889975461156, 9.702672574024962415, 1.199719254218452047 ) ) ;
#119069 = CARTESIAN_POINT ( 'NONE',  ( 5.761288931164342486, 5.686201605971993978, -0.7998128361456481317 ) ) ;
#119071 = LINE ( 'NONE', #139551, #106593 ) ;
#119072 = CARTESIAN_POINT ( 'NONE',  ( 4.904559663377827228, -2.005024252762297898, -0.2429568683046164634 ) ) ;
#119073 = CARTESIAN_POINT ( 'NONE',  ( 1.364683531249990311, 5.613541667008087543, 0.7879004041258500513 ) ) ;
#119074 = CARTESIAN_POINT ( 'NONE',  ( 0.6376417299419987472, 1.925892387546113582, -0.7388170802648945656 ) ) ;
#119075 = CARTESIAN_POINT ( 'NONE',  ( 8.161645285746708112, 9.584636257201740506, -1.082531754730543083 ) ) ;
#119076 = ADVANCED_FACE ( 'NONE', ( #189466, #173241 ), #158055, .T. ) ;
#119077 = CARTESIAN_POINT ( 'NONE',  ( 6.086684617892325733, 6.065829907154645539, -0.7998128361456481317 ) ) ;
#119078 = CARTESIAN_POINT ( 'NONE',  ( -1.364683531250000748, -0.1781249996585798634, 0.000000000000000000 ) ) ;
#119080 = CARTESIAN_POINT ( 'NONE',  ( 8.787802685836132000, 3.956598013261175772, 7.485281629513396595 ) ) ;
#119079 = CARTESIAN_POINT ( 'NONE',  ( 5.662465432362883355, 6.635239754958710989, 1.199719254218451159 ) ) ;
#119081 =( BOUNDED_CURVE ( )  B_SPLINE_CURVE ( 2, ( #23032, #40393, #106497, #92364, #5703, #172524, #58760 ),
 .UNSPECIFIED., .F., .T. ) 
 B_SPLINE_CURVE_WITH_KNOTS ( ( 3, 2, 2, 3 ),
 ( 0.4750000000000001998, 0.4833333333333335036, 0.4916666666666666963, 0.5000000000000000000 ),
 .UNSPECIFIED. ) 
 CURVE ( )  GEOMETRIC_REPRESENTATION_ITEM ( )  RATIONAL_B_SPLINE_CURVE ( ( 0.9999999999999964473, 0.8660254037844422603, 1.000000000000000000, 0.8660254037844387076, 1.000000000000000000, 0.8660254037844387076, 1.000000000000000000 ) ) 
 REPRESENTATION_ITEM ( '' )  );
#119082 = CARTESIAN_POINT ( 'NONE',  ( 6.751597309481075726, 10.82068792779586985, 1.040834085586084257E-14 ) ) ;
#119084 = SURFACE_STYLE_USAGE ( .BOTH. , #149388 ) ;
#119083 = CARTESIAN_POINT ( 'NONE',  ( 3.244746832269917558, -2.138594630188391132, -0.3739374351436116073 ) ) ;
#119086 = CARTESIAN_POINT ( 'NONE',  ( 1.505144418776669601, -1.827259764946763454, 0.2261131901925839127 ) ) ;
#119085 = CARTESIAN_POINT ( 'NONE',  ( -3.307826292054304673, 6.802955074131234348, -0.7216878364870267237 ) ) ;
#119087 = CARTESIAN_POINT ( 'NONE',  ( -1.201851678989727383E-14, 3.196875000341420137, -1.575800808251660134 ) ) ;
#119088 = CARTESIAN_POINT ( 'NONE',  ( 4.388337494309430653, -0.4807229498768311182, -2.138019847805587403 ) ) ;
#119089 = LINE ( 'NONE', #201311, #102012 ) ;
#119090 = CARTESIAN_POINT ( 'NONE',  ( 4.698257824713211406, -2.261882422057570619, -0.06011341499151043322 ) ) ;
#119091 = CARTESIAN_POINT ( 'NONE',  ( -6.663996196316808174, 7.733415969579778171, -1.199719254218446718 ) ) ;
#119092 = SPHERICAL_SURFACE ( 'NONE', #208240, 9.500000000000001776 ) ;
#119093 = CARTESIAN_POINT ( 'NONE',  ( 5.061762083669725243, 7.855803969722688684, -1.119403510469544782 ) ) ;
#119094 = CARTESIAN_POINT ( 'NONE',  ( 0.7500000000000006661, 13.83333333333333570, 1.299038105676657340 ) ) ;
#119095 = CARTESIAN_POINT ( 'NONE',  ( -6.305950843687521790, 7.489935751457798219, 1.082531754730548412 ) ) ;
#119096 = CARTESIAN_POINT ( 'NONE',  ( 5.899206235721897507, 6.055031161196562373, 0.000000000000000000 ) ) ;
#119097 = CARTESIAN_POINT ( 'NONE',  ( 5.342920941031360726, -1.517576202870707380, 0.9101455627106845858 ) ) ;
#119098 = CARTESIAN_POINT ( 'NONE',  ( 5.784525094524856748, 9.900363043587685041, 1.040834085586084257E-14 ) ) ;
#119099 = CARTESIAN_POINT ( 'NONE',  ( 1.747240475267642257, -1.779442529384717808, 1.126025380906693352 ) ) ;
#119101 = CARTESIAN_POINT ( 'NONE',  ( 0.7499999999999885647, 2.316666666666689078, -1.299038105676652899 ) ) ;
#119100 = CARTESIAN_POINT ( 'NONE',  ( 1.364683531249997417, 11.73437500034139802, 2.602085213965210642E-15 ) ) ;
#119102 = CARTESIAN_POINT ( 'NONE',  ( 2.049204468142644231, 1.715183525312633517, -0.9679544390571446222 ) ) ;
#119103 = CARTESIAN_POINT ( 'NONE',  ( 0.1802491246630563426, -1.813337052076903877, -0.4591185353455888296 ) ) ;
#119104 = CARTESIAN_POINT ( 'NONE',  ( 0.6956633456795427994, -1.384754418207832405, -1.389998539416361423 ) ) ;
#119106 = ORIENTED_EDGE ( 'NONE', *, *, #170713, .T. ) ;
#119105 = CARTESIAN_POINT ( 'NONE',  ( 5.695527492674265169, 1.670499194714653468, -0.7014341174245084520 ) ) ;
#119107 = CARTESIAN_POINT ( 'NONE',  ( 6.236387472606139681, 8.298871356172400127, -1.443375672974057666 ) ) ;
#119108 = CARTESIAN_POINT ( 'NONE',  ( 1.364683531249988757, -0.05312499965857975237, 0.000000000000000000 ) ) ;
#119109 = CARTESIAN_POINT ( 'NONE',  ( 6.315307248462690204, -0.2269180964024133385, 1.856785020699961875 ) ) ;
#119110 = CARTESIAN_POINT ( 'NONE',  ( 4.403700966340357681, 4.032072637018845107, -0.7998128361456211532 ) ) ;
#119111 = CARTESIAN_POINT ( 'NONE',  ( 8.955454528940892445, 3.019799309333439652, 8.063527476383637094 ) ) ;
#119112 = CARTESIAN_POINT ( 'NONE',  ( 5.313363446356571984, -1.745981802610725442, -1.112170280247841703 ) ) ;
#119113 = CARTESIAN_POINT ( 'NONE',  ( -5.655159470231558849, 6.730679149092498648, 1.082531754730549078 ) ) ;
#119115 = PRESENTATION_STYLE_ASSIGNMENT (( #184039 ) ) ;
#119114 = AXIS2_PLACEMENT_3D ( 'NONE', #195942, #162381, #129954 ) ;
#119116 = CARTESIAN_POINT ( 'NONE',  ( 0.7499999999999885647, 0.9833333333333569293, 1.299038105676657340 ) ) ;
#119117 = CARTESIAN_POINT ( 'NONE',  ( 8.437251666405968464, 8.737881787095446384, 1.040834085586084257E-14 ) ) ;
#119118 = CARTESIAN_POINT ( 'NONE',  ( -7.883176251342026042, 11.28445716228600126, -1.199719254218446718 ) ) ;
#119119 = CARTESIAN_POINT ( 'NONE',  ( 5.020262018810099924, 9.078999131912302900, 0.7998128361456331437 ) ) ;
#119120 = CARTESIAN_POINT ( 'NONE',  ( -1.402160292154681736E-14, 0.1968750003414221628, -1.575800808251665908 ) ) ;
#119121 = CARTESIAN_POINT ( 'NONE',  ( -0.7500000000000006661, 0.6083333333333564852, -1.299038105676652011 ) ) ;
#119123 = CARTESIAN_POINT ( 'NONE',  ( 3.635557746758808495, 7.393234471193928847, -0.7998128361456291469 ) ) ;
#119122 = CARTESIAN_POINT ( 'NONE',  ( 4.949637131784443866, 1.452432516441283905, 1.319008059494260143 ) ) ;
#119124 = CARTESIAN_POINT ( 'NONE',  ( 3.638045922354939954, 0.05228986736816390590, -2.015604357568132166 ) ) ;
#119125 = EDGE_CURVE ( 'NONE', #49028, #136644, #167697, .T. ) ;
#119126 = CARTESIAN_POINT ( 'NONE',  ( 2.395587962911712498, -1.894220731477358921, 0.2854614921951497686 ) ) ;
#119127 = DIRECTION ( 'NONE',  ( 0.000000000000000000, 0.000000000000000000, -1.000000000000000000 ) ) ;
#119128 = CARTESIAN_POINT ( 'NONE',  ( 0.8729168595149154886, -0.05911722906676297740, -2.190938979806676734 ) ) ;
#119129 = CARTESIAN_POINT ( 'NONE',  ( 0.2335667940003021970, 4.085521407782252368, -2.708192491817535075 ) ) ;
#119130 = CARTESIAN_POINT ( 'NONE',  ( 1.598681293450100904, 1.532267803987485077, -1.072633048482305229 ) ) ;
#119131 = CARTESIAN_POINT ( 'NONE',  ( -1.500000000000001332, -1.068749999317178290, 0.000000000000000000 ) ) ;
#119132 = CARTESIAN_POINT ( 'NONE',  ( 4.289318580081720178, -0.004264002974461738975, -2.013376228308662252 ) ) ;
#119133 = CARTESIAN_POINT ( 'NONE',  ( -7.212047647465563038, 10.50147379109678880, -1.199719254218446718 ) ) ;
#119135 = CARTESIAN_POINT ( 'NONE',  ( 4.868830934094980911, -0.2605620880507720227, -2.101091820269097354 ) ) ;
#119134 = CARTESIAN_POINT ( 'NONE',  ( -4.595850885352567694, 8.305650432979225783, 1.040834085586084257E-14 ) ) ;
#119136 = CARTESIAN_POINT ( 'NONE',  ( 6.461392557816405535, 1.719054114842766268, 1.153505076091146053 ) ) ;
#119138 = CARTESIAN_POINT ( 'NONE',  ( 6.620655732516620873, 2.403464043289889496, 2.653833411862613012 ) ) ;
#119137 = CARTESIAN_POINT ( 'NONE',  ( 1.698888801382715252, 1.740066399362389271, 1.158727311120285819 ) ) ;
#119140 = ORIENTED_EDGE ( 'NONE', *, *, #48296, .F. ) ;
#119139 = CARTESIAN_POINT ( 'NONE',  ( 0.1996746939399509924, -1.724222465425511386, -0.05034706749046553159 ) ) ;
#119141 = CARTESIAN_POINT ( 'NONE',  ( 7.588813295347141441, 9.876701482703580837, -1.599625672291262513 ) ) ;
#119142 = CARTESIAN_POINT ( 'NONE',  ( -10.95308175811721085, 13.79999999999998295, 1.799999999999999600 ) ) ;
#119143 = DIRECTION ( 'NONE',  ( -1.000000000000000000, 7.771561172376097755E-16, 4.440892098500627148E-16 ) ) ;
#119145 = CARTESIAN_POINT ( 'NONE',  ( 5.450014562569148957, 9.302174723065263606, 1.040834085586084257E-14 ) ) ;
#119144 = CARTESIAN_POINT ( 'NONE',  ( 7.308008492965924141, 8.484763649003774333, -1.199719254218451159 ) ) ;
#119146 = CARTESIAN_POINT ( 'NONE',  ( 1.364683531249996529, 13.02604166700806410, 0.7879004041258403923 ) ) ;
#119148 = CARTESIAN_POINT ( 'NONE',  ( 0.8909134567714148689, -0.04341352697850982267, -1.811128585712480366 ) ) ;
#119147 = CARTESIAN_POINT ( 'NONE',  ( 5.833751235630055376, 10.02806988486892514, 0.7998128361456331437 ) ) ;
#119149 = CARTESIAN_POINT ( 'NONE',  ( -8.342344591110322227, 8.627156865917170236, -0.7998128361456291469 ) ) ;
#119150 = CARTESIAN_POINT ( 'NONE',  ( 6.830610463186557624, 6.863467050006115677, 1.040834085586084257E-14 ) ) ;
#119151 = CARTESIAN_POINT ( 'NONE',  ( 4.071134731106788252, 7.497899514862828241, -0.5496474101556632075 ) ) ;
#119152 = CARTESIAN_POINT ( 'NONE',  ( 4.383363735919856730, 4.008345868194933104, -0.7998128361456211532 ) ) ;
#119153 = ORIENTED_EDGE ( 'NONE', *, *, #87324, .T. ) ;
#119154 = CARTESIAN_POINT ( 'NONE',  ( 5.993767587909683670, -2.000856116866961187, 0.2496242821527286382 ) ) ;
#119155 = CARTESIAN_POINT ( 'NONE',  ( 0.5926325054007793858, -1.174586488569592690, 1.765252418913294319 ) ) ;
#119156 = FACE_OUTER_BOUND ( 'NONE', #174961, .T. ) ;
#119157 = CARTESIAN_POINT ( 'NONE',  ( -0.1394461523061351904, -0.009327122704730000241, -2.280146446826665230 ) ) ;
#119158 = CARTESIAN_POINT ( 'NONE',  ( 7.636191794455555737, -6.027819618361855092, 7.636191794455528203 ) ) ;
#119159 = CARTESIAN_POINT ( 'NONE',  ( -2.792616454734997866, 6.201876930592042925, 0.7216878364870317197 ) ) ;
#119160 = CARTESIAN_POINT ( 'NONE',  ( 9.083599731475983319, 11.62061899152058686, 1.443375672974076540 ) ) ;
#119161 = CARTESIAN_POINT ( 'NONE',  ( 3.871889627987592064, -1.941038753702705177, 0.3322218420921344562 ) ) ;
#119162 = CARTESIAN_POINT ( 'NONE',  ( 4.253529916566947122, 1.955168710539030075, -0.4926619687581067497 ) ) ;
#119163 = CARTESIAN_POINT ( 'NONE',  ( -7.555971681517696936, 7.709721804725773175, 0.7998128361456462443 ) ) ;
#119164 = CARTESIAN_POINT ( 'NONE',  ( -9.573337995800486055, -7.550885189219930460, 5.228734383400795993E-15 ) ) ;
#119166 = EDGE_CURVE ( 'NONE', #15288, #31452, #164301, .T. ) ;
#119165 = CARTESIAN_POINT ( 'NONE',  ( -3.090026840240785777, 6.449493289948600605, -0.7169942672678782936 ) ) ;
#119167 = CARTESIAN_POINT ( 'NONE',  ( 5.015667846030231303, -1.170523448010954315, -1.852474865436819274 ) ) ;
#119168 = CARTESIAN_POINT ( 'NONE',  ( 0.000000000000000000, -1.399999999999998579, 0.000000000000000000 ) ) ;
#119169 = CARTESIAN_POINT ( 'NONE',  ( 3.610301043878104021, -0.7796817500047310556, -1.761725471645478436 ) ) ;
#119170 = CARTESIAN_POINT ( 'NONE',  ( -6.835281999583978418, 11.12624609948998966, -0.7998128361456291469 ) ) ;
#119171 = CARTESIAN_POINT ( 'NONE',  ( -0.02968770228140016343, 0.2527710104786498047, -1.861515397111657144 ) ) ;
#119172 = CARTESIAN_POINT ( 'NONE',  ( 0.1333542156527660338, 0.2446709926765543996, -2.080993637364982884 ) ) ;
#119173 = CARTESIAN_POINT ( 'NONE',  ( -0.07727525906048532400, 7.079397053215386926, 2.120984693056199077 ) ) ;
#119174 = ORIENTED_EDGE ( 'NONE', *, *, #179202, .T. ) ;
#119175 = CARTESIAN_POINT ( 'NONE',  ( 5.072158865288245444, 5.090142562357324429, 0.7216878364870338292 ) ) ;
#119176 = CARTESIAN_POINT ( 'NONE',  ( 4.785976182654667177, -1.208483435658064487, -1.555025035033012148 ) ) ;
#119178 = CARTESIAN_POINT ( 'NONE',  ( 3.774091158939500978, 1.997611739970482692, -0.2487840229714877727 ) ) ;
#119177 = CARTESIAN_POINT ( 'NONE',  ( 0.2572359396431650458, 1.920763697077633614, -0.2861409625158922165 ) ) ;
#119179 = CARTESIAN_POINT ( 'NONE',  ( 5.589350027729360626, 1.375356176494828553, -1.841343765151080003 ) ) ;
#119181 = CARTESIAN_POINT ( 'NONE',  ( 4.574962676454192412, 1.700228875758927671, 0.7569903647998057483 ) ) ;
#119180 = CARTESIAN_POINT ( 'NONE',  ( 11.92619526913700057, 11.02781666661241644, 1.328859060402684644 ) ) ;
#119182 = CARTESIAN_POINT ( 'NONE',  ( 7.862802741282558294, 8.137967717776607657, 0.000000000000000000 ) ) ;
#119184 = ADVANCED_FACE ( 'NONE', ( #204623 ), #122433, .F. ) ;
#119183 = FACE_OUTER_BOUND ( 'NONE', #180784, .T. ) ;
#119185 = SURFACE_SIDE_STYLE ('',( #134346 ) ) ;
#119186 = CARTESIAN_POINT ( 'NONE',  ( -6.718228810771495141, 7.796687353110217877, 1.199719254218450271 ) ) ;
#119187 = CARTESIAN_POINT ( 'NONE',  ( 6.720655732516650716, 2.467238681591706673, 2.210725262702870175 ) ) ;
#119188 = CARTESIAN_POINT ( 'NONE',  ( 0.6795420635867071013, 1.475991390215245058, 1.620154534501851096 ) ) ;
#119189 = CARTESIAN_POINT ( 'NONE',  ( 5.992340707560160240, 7.053780915984068756, 1.082531754730558626 ) ) ;
#119190 = ORIENTED_EDGE ( 'NONE', *, *, #162356, .F. ) ;
#119191 =( LENGTH_UNIT ( ) NAMED_UNIT ( * ) SI_UNIT ( .MILLI., .METRE. ) );
#119192 = CARTESIAN_POINT ( 'NONE',  ( 11.97929049433705373, 9.719999999999998863, -0.7046979865771834106 ) ) ;
#119193 = CARTESIAN_POINT ( 'NONE',  ( 0.3986991128735201673, 1.519733473351183362, -1.011397189243423700 ) ) ;
#119194 = CARTESIAN_POINT ( 'NONE',  ( -4.406563619641430840, 5.099744630125142564, -1.199719254218446718 ) ) ;
#119195 = CARTESIAN_POINT ( 'NONE',  ( 2.443678673881148011, -1.509841515647825094, -0.8527992262679043867 ) ) ;
#119196 = SURFACE_SIDE_STYLE ('',( #137535 ) ) ;
#119197 = CARTESIAN_POINT ( 'NONE',  ( -6.050059093290697021, 6.050762344992199004, -0.5500513593517241118 ) ) ;
#119198 = CARTESIAN_POINT ( 'NONE',  ( 10.16199982864259788, 11.81442020729326536, 1.199719254218452047 ) ) ;
#119199 = CARTESIAN_POINT ( 'NONE',  ( 6.024025069106937913, -1.018266858664597763, -1.515143308444939274 ) ) ;
#119200 = CARTESIAN_POINT ( 'NONE',  ( 3.783995958019512607, -1.164969938643352299, -1.578273546942794647 ) ) ;
#119201 = CARTESIAN_POINT ( 'NONE',  ( 0.6124999999999932720, -0.6041666659838615949, 1.060881119635929348 ) ) ;
#119202 = CARTESIAN_POINT ( 'NONE',  ( -9.450196763925152510, 10.98398329845622001, -1.199719254218441611 ) ) ;
#119203 = CARTESIAN_POINT ( 'NONE',  ( 6.693975156845185737, 8.832723654451292816, 1.599625672291281386 ) ) ;
#119204 = CARTESIAN_POINT ( 'NONE',  ( 4.530007735025624704, -2.079396993832134388, 0.4145621898983055109 ) ) ;
#119205 = CARTESIAN_POINT ( 'NONE',  ( 5.332099551924443404, 9.442809587212341427, 0.000000000000000000 ) ) ;
#119206 = CIRCLE ( 'NONE', #153784, 0.05000000000000056483 ) ;
#119207 = CARTESIAN_POINT ( 'NONE',  ( -9.459838494033043332, 12.05956421450382088, 1.599625672291281386 ) ) ;
#119208 = ADVANCED_FACE ( 'NONE', ( #106139 ), #25885, .T. ) ;
#119209 = CARTESIAN_POINT ( 'NONE',  ( 2.536061329345109971, 1.270221119870031057, 1.634730569901183150 ) ) ;
#119211 = CARTESIAN_POINT ( 'NONE',  ( 0.6823417656249882723, -0.09479166632524876901, 1.181850606188755259 ) ) ;
#119210 = CARTESIAN_POINT ( 'NONE',  ( -11.94651559118242368, 11.15130655878970956, 1.135242698369626435 ) ) ;
#119214 = EDGE_LOOP ( 'NONE', ( #101658, #208553, #25316, #66132 ) ) ;
#119213 = CARTESIAN_POINT ( 'NONE',  ( 4.266425542637849233, 2.220793247050854902, -0.05466516159106404871 ) ) ;
#119212 = AXIS2_PLACEMENT_3D ( 'NONE', #31730, #95678, #130365 ) ;
#119215 = CARTESIAN_POINT ( 'NONE',  ( 3.252836000005991046, 2.242300829042419785, -0.5054477054214584486 ) ) ;
#119216 = CARTESIAN_POINT ( 'NONE',  ( 6.805829924380097040, 10.88395931184472154, 0.7216878364870438212 ) ) ;
#119218 = CARTESIAN_POINT ( 'NONE',  ( 1.642778471875001811, -2.092708332855373943, 2.845375778867859751 ) ) ;
#119217 = CARTESIAN_POINT ( 'NONE',  ( 7.024532985656136930, 8.328281583754568729, 1.082531754730549967 ) ) ;
#119219 = CARTESIAN_POINT ( 'NONE',  ( 0.3282377607281223852, 1.573664549684625769, 1.224999999999981659 ) ) ;
#119220 = ORIENTED_EDGE ( 'NONE', *, *, #137732, .T. ) ;
#119221 = CARTESIAN_POINT ( 'NONE',  ( -5.529805931533524621, 6.238042758285092582, -0.9566377225056829081 ) ) ;
#119222 = CARTESIAN_POINT ( 'NONE',  ( 2.847809051801777791, -1.287500320553297994, -1.414207669007704116 ) ) ;
#119223 = CARTESIAN_POINT ( 'NONE',  ( -0.3963168366282447952, 6.583269796083455638, -3.242944579665297145 ) ) ;
#119224 = CARTESIAN_POINT ( 'NONE',  ( 4.260587326446613865, -1.277293937326873019, 1.159233799866489889 ) ) ;
#119225 = CARTESIAN_POINT ( 'NONE',  ( 3.485564796978508184, -0.5807542032013839339, 1.931124776463407189 ) ) ;
#119226 = CARTESIAN_POINT ( 'NONE',  ( 3.938341551375645011, -1.911473949098478897, -1.276577049080502624 ) ) ;
#119227 = VECTOR ( 'NONE', #165756, 1000.000000000000000 ) ;
#119228 = DIRECTION ( 'NONE',  ( 0.000000000000000000, 1.000000000000000000, 0.000000000000000000 ) ) ;
#119229 = CARTESIAN_POINT ( 'NONE',  ( 6.024072228909682636, -1.168613738950954550, -1.751890494488865357 ) ) ;
#119230 = CARTESIAN_POINT ( 'NONE',  ( -5.885648082108231982, 7.959951743916638733, 1.443375672974058777 ) ) ;
#119231 = ORIENTED_EDGE ( 'NONE', *, *, #131603, .F. ) ;
#119232 = CARTESIAN_POINT ( 'NONE',  ( 4.569463179464338332, 1.716784003608927467, -0.4291735618162701438 ) ) ;
#119234 = CARTESIAN_POINT ( 'NONE',  ( 0.8675860333910101474, 2.207824459889203172, -0.6162223019612712571 ) ) ;
#119233 = CARTESIAN_POINT ( 'NONE',  ( 7.849244587668864348, 8.122149871893999062, 0.7998128361456291469 ) ) ;
#119235 = CARTESIAN_POINT ( 'NONE',  ( 0.3744471653823171486, 1.625640304646416734, -0.6218004557168725910 ) ) ;
#119236 = CARTESIAN_POINT ( 'NONE',  ( 0.4153311931459133799, 3.919693508839672713, 0.5000000000000067724 ) ) ;
#119237 = CARTESIAN_POINT ( 'NONE',  ( 6.351546390744761794, 2.185874319550953793, -0.1572705277706408222 ) ) ;
#119238 = CARTESIAN_POINT ( 'NONE',  ( -3.467853430045390706, 7.267855778353407459, 0.7998128361456352531 ) ) ;
#119239 = CARTESIAN_POINT ( 'NONE',  ( -5.398914348987512213, 6.259949555863199677, 2.500000000000001332 ) ) ;
#119240 = CARTESIAN_POINT ( 'NONE',  ( 3.973272364828547509, 7.311925558592853314, -0.9262215144194854144 ) ) ;
#119241 = CARTESIAN_POINT ( 'NONE',  ( 6.742638474511262636, -2.029596885996234334, -0.4079607620106340260 ) ) ;
#119242 = CARTESIAN_POINT ( 'NONE',  ( 0.8664231474371618669, -1.968446048378743152, -0.4370742218882398000 ) ) ;
#119243 = CARTESIAN_POINT ( 'NONE',  ( 0.7499999999999885647, -1.235416665983847473, 1.299038105676657340 ) ) ;
#119244 = CARTESIAN_POINT ( 'NONE',  ( 5.971306315489836258, 0.1393824199819072851, -1.921517340817725961 ) ) ;
#119245 = CARTESIAN_POINT ( 'NONE',  ( 0.6823417656249969321, 11.27604166700806765, -1.181850606188757036 ) ) ;
#119246 = CARTESIAN_POINT ( 'NONE',  ( 1.125557598851456786, 1.962289056045916524, 1.041162070263027761 ) ) ;
#119248 = ORIENTED_EDGE ( 'NONE', *, *, #151435, .F. ) ;
#119247 = CARTESIAN_POINT ( 'NONE',  ( 9.215791728987056786, 11.77484298861683598, -1.599625672291262513 ) ) ;
#119250 = CARTESIAN_POINT ( 'NONE',  ( -0.08000000000000714873, -5.907420853759267843, 10.91970695577494865 ) ) ;
#119249 = SURFACE_STYLE_FILL_AREA ( #35794 ) ;
#119251 = CARTESIAN_POINT ( 'NONE',  ( 7.065207446497155708, 9.336104335703744539, 0.000000000000000000 ) ) ;
#119252 = CARTESIAN_POINT ( 'NONE',  ( 7.553864141108259211, 11.96459193126834464, 1.040834085586084257E-14 ) ) ;
#119253 = FACE_OUTER_BOUND ( 'NONE', #45202, .T. ) ;
#119254 = DIRECTION ( 'NONE',  ( -0.9992060137953822085, 0.000000000000000000, 0.03984146075563027578 ) ) ;
#119255 = CARTESIAN_POINT ( 'NONE',  ( 4.089206054525551970, -0.6613740077951230090, 1.610090703890323605 ) ) ;
#119256 = CARTESIAN_POINT ( 'NONE',  ( 2.365611650783586040, -0.4327418640146082907, 1.913375882425945917 ) ) ;
#119258 = CARTESIAN_POINT ( 'NONE',  ( -1.201851678989727383E-14, 2.759375000341417916, -1.575800808251660134 ) ) ;
#119257 = CARTESIAN_POINT ( 'NONE',  ( 4.147904930777053245, 6.926640621626830807, -1.199719254218452047 ) ) ;
#119259 = CARTESIAN_POINT ( 'NONE',  ( 10.41272866534396435, -5.796408561409281290, 1.485228241937698088E-12 ) ) ;
#119260 = CARTESIAN_POINT ( 'NONE',  ( 6.232861002365865488, -1.862453515449840724, -0.6167318247369477646 ) ) ;
#119261 = CARTESIAN_POINT ( 'NONE',  ( -6.645467848992654858, 10.90479625713344625, 0.7998128361456481317 ) ) ;
#119262 = CARTESIAN_POINT ( 'NONE',  ( -4.243338890952904841, 5.973648010910253880, -1.443375672974051449 ) ) ;
#119263 = AXIS2_PLACEMENT_3D ( 'NONE', #138686, #122516, #24900 ) ;
#119264 = CARTESIAN_POINT ( 'NONE',  ( 5.436732529336289588, -1.586671906620169104, 1.244382051841623538 ) ) ;
#119265 = CARTESIAN_POINT ( 'NONE',  ( 1.218052960884225433, -2.206959832567402469, 0.4976822367108637013 ) ) ;
#119267 = ORIENTED_EDGE ( 'NONE', *, *, #90754, .T. ) ;
#119266 = CARTESIAN_POINT ( 'NONE',  ( -5.636439174979254396, 7.598931675607687453, -1.599625672291256295 ) ) ;
#119268 = CARTESIAN_POINT ( 'NONE',  ( 1.499999999999987121, 0.2854166673494805684, 0.8660254037844524744 ) ) ;
#119269 = CARTESIAN_POINT ( 'NONE',  ( 1.827212670807505379, -1.763035892288829620, 0.6254473451912796467 ) ) ;
#119270 = CARTESIAN_POINT ( 'NONE',  ( 0.1407077508718111714, 0.6607813331330723017, 1.603534759577706303 ) ) ;
#119271 = CARTESIAN_POINT ( 'NONE',  ( 4.652002595327206613, 0.8389548150543740812, 2.024815518666116088 ) ) ;
#119272 = CARTESIAN_POINT ( 'NONE',  ( 5.965930945686983122, 2.274828880937030728, -0.3866611637039600313 ) ) ;
#119273 = CARTESIAN_POINT ( 'NONE',  ( 0.8310182365124726411, 0.1507505247145359273, 2.055422933874837099 ) ) ;
#119274 = CARTESIAN_POINT ( 'NONE',  ( 3.363160477839432172, 1.894460165981373789, -0.4261612883773926441 ) ) ;
#119275 = CARTESIAN_POINT ( 'NONE',  ( -4.921246571636213929, 4.843801876438091902, 0.7216878364870317197 ) ) ;
#119276 = AXIS2_PLACEMENT_3D ( 'NONE', #154845, #41110, #186254 ) ;
#119277 = CARTESIAN_POINT ( 'NONE',  ( 5.360568611784803927, -1.355617963529401893, 1.289147430649554948 ) ) ;
#119278 = CARTESIAN_POINT ( 'NONE',  ( 4.008122245411202655, 7.584344604122328803, -0.2404964666735086298 ) ) ;
#119279 = CARTESIAN_POINT ( 'NONE',  ( 6.503279807981923177, 1.993766592317405051, 0.2985777636397292101 ) ) ;
#119280 = CARTESIAN_POINT ( 'NONE',  ( 1.360316468749983798, 0.9947916670081107249, 0.7853790794158600486 ) ) ;
#119281 = CARTESIAN_POINT ( 'NONE',  ( 4.412732527109735514, -1.242725882911545510, -1.587838301257207041 ) ) ;
#119282 = CARTESIAN_POINT ( 'NONE',  ( -4.622967192135580383, 5.456178481322002227, 1.082531754730558626 ) ) ;
#119283 = CARTESIAN_POINT ( 'NONE',  ( -4.620296487206990932, 8.612372678375294299, 0.000000000000000000 ) ) ;
#119284 = CARTESIAN_POINT ( 'NONE',  ( 9.935427640716063991, 10.48575375712389679, -0.7998128361456281477 ) ) ;
#119286 = CARTESIAN_POINT ( 'NONE',  ( -1.244150428499023908, 3.152476754118171964, 0.7750000000000100142 ) ) ;
#119285 = CARTESIAN_POINT ( 'NONE',  ( 1.629252094361890890, -1.719607636260962025, 0.6136192449261099746 ) ) ;
#119287 = CARTESIAN_POINT ( 'NONE',  ( -4.664887371553763096, 7.600063145858131364, -1.199719254218453823 ) ) ;
#119288 = CARTESIAN_POINT ( 'NONE',  ( -5.601453741101424022, 6.564059448486966986, -1.199719254218453823 ) ) ;
#119289 = CARTESIAN_POINT ( 'NONE',  ( -11.29165584589917870, 5.103824637450834700, 5.764786465619509137 ) ) ;
#119290 = ORIENTED_EDGE ( 'NONE', *, *, #194283, .F. ) ;
#119291 = CARTESIAN_POINT ( 'NONE',  ( -6.441532379824190357, 6.687744995982559892, 0.7216878364870257245 ) ) ;
#119292 = CARTESIAN_POINT ( 'NONE',  ( -4.600294193738529103, 4.261431402316699035, -0.7998128361456221525 ) ) ;
#119293 = CARTESIAN_POINT ( 'NONE',  ( 7.385065802799687162, -6.893137084989842123, 8.044078759455205230 ) ) ;
#119294 = CARTESIAN_POINT ( 'NONE',  ( 6.164714676696682716, 0.6357101859572679148, 1.917071687811313652 ) ) ;
#119296 = ORIENTED_EDGE ( 'NONE', *, *, #92379, .F. ) ;
#119295 = CARTESIAN_POINT ( 'NONE',  ( 0.2059360158346480729, 1.574223368660916611, 1.420867075595611650 ) ) ;
#119297 = CARTESIAN_POINT ( 'NONE',  ( -5.399890319992785237, 9.521898816625391504, 0.7998128361456291469 ) ) ;
#119298 = CARTESIAN_POINT ( 'NONE',  ( 5.840865249388943248, 5.708764300575555062, 0.7998128361456341429 ) ) ;
#119299 = CARTESIAN_POINT ( 'NONE',  ( 4.996976137430897857, 1.714615628211055398, -1.143075302399678472 ) ) ;
#119300 = CARTESIAN_POINT ( 'NONE',  ( 5.045546153961558922, -1.458558117013383892, 1.392544180963309230 ) ) ;
#119301 = ORIENTED_EDGE ( 'NONE', *, *, #50025, .T. ) ;
#119302 = VERTEX_POINT ( 'NONE', #10699 ) ;
#119303 = CARTESIAN_POINT ( 'NONE',  ( 4.760479229700392168, 4.886233537081844602, -0.7782378322892316014 ) ) ;
#119304 = CARTESIAN_POINT ( 'NONE',  ( -1.883777847254928028, 2.479999999999988880, 2.461990205983016100 ) ) ;
#119306 = ORIENTED_EDGE ( 'NONE', *, *, #65446, .F. ) ;
#119305 = CARTESIAN_POINT ( 'NONE',  ( -6.252245114557387851, 7.323316050852266557, -1.199719254218453823 ) ) ;
#119307 = CARTESIAN_POINT ( 'NONE',  ( 4.978670620768666844, 8.057607364700732688, 1.103355461389814662 ) ) ;
#119308 = CARTESIAN_POINT ( 'NONE',  ( 5.167342215279058237, -0.6766115767681828430, -1.899327316215810857 ) ) ;
#119309 = CARTESIAN_POINT ( 'NONE',  ( 3.661895226921571656, -1.235415792305821325, 1.365283978338522441 ) ) ;
#119310 = CARTESIAN_POINT ( 'NONE',  ( -1.608462485350629301, 8.735270501766756013, 2.463594439587650342 ) ) ;
#119311 = CARTESIAN_POINT ( 'NONE',  ( 2.368180137760375281, 2.262835426277497675, -0.4520343961368147312 ) ) ;
#119312 = CARTESIAN_POINT ( 'NONE',  ( 5.494797395288433250, 9.632623737803665875, 0.000000000000000000 ) ) ;
#119313 = CARTESIAN_POINT ( 'NONE',  ( 5.079442160427912967, 2.018932005888602887, -0.7727740077691500620 ) ) ;
#119314 = CARTESIAN_POINT ( 'NONE',  ( 7.639129486296027061, 10.99973593639901814, 1.199719254218460707 ) ) ;
#119316 = CARTESIAN_POINT ( 'NONE',  ( 2.659388954101277847, 1.913261587491304150, -0.6371546050257800298 ) ) ;
#119315 = CARTESIAN_POINT ( 'NONE',  ( -0.1119450412391852639, -0.4286113830911059130, -1.901434273657340412 ) ) ;
#119317 = CARTESIAN_POINT ( 'NONE',  ( -4.680589345215810049, 6.483773540883647435, -1.599625672291256295 ) ) ;
#119318 = EDGE_CURVE ( 'NONE', #121309, #67257, #136639, .T. ) ;
#119319 = CARTESIAN_POINT ( 'NONE',  ( 11.89942855770814312, 9.799999999999998934, 0.6999999999999992895 ) ) ;
#119320 = CARTESIAN_POINT ( 'NONE',  ( -5.544921637864844932, 5.571422787038162738, -0.7216878364870168427 ) ) ;
#119321 = AXIS2_PLACEMENT_3D ( 'NONE', #212064, #163349, #14925 ) ;
#119322 = CARTESIAN_POINT ( 'NONE',  ( 3.520239479114236403, 1.187513476551487424, -1.445374034619356207 ) ) ;
#119323 = VERTEX_POINT ( 'NONE', #23755 ) ;
#119324 = CARTESIAN_POINT ( 'NONE',  ( 0.2980362317399931626, -1.970818609879662953, -0.05296617050038961161 ) ) ;
#119326 = CARTESIAN_POINT ( 'NONE',  ( -6.912678218121246942, 9.158153569265168770, 1.599625672291269396 ) ) ;
#119325 = CARTESIAN_POINT ( 'NONE',  ( 0.7499999999999867883, -0.6520833326505159899, -1.299038105676652899 ) ) ;
#119327 = CARTESIAN_POINT ( 'NONE',  ( 1.243116305521356990, 0.4334984505205765060, 2.163720904216937857 ) ) ;
#119328 = ORIENTED_EDGE ( 'NONE', *, *, #28655, .F. ) ;
#119329 = CARTESIAN_POINT ( 'NONE',  ( 3.947104627881218963, 8.980740528189222971, -0.7749999999999996891 ) ) ;
#119330 = CARTESIAN_POINT ( 'NONE',  ( 2.693266070609028784, 6.293894182352508970, 0.000000000000000000 ) ) ;
#119331 = CARTESIAN_POINT ( 'NONE',  ( -4.355193658487827690, 6.104145239700998538, -1.599625672291256295 ) ) ;
#119332 = CARTESIAN_POINT ( 'NONE',  ( -7.882977371601947780, -5.341768514962232040, 7.624693973552358450 ) ) ;
#119333 = CARTESIAN_POINT ( 'NONE',  ( 0.1808907491311480820, -0.1332662104699660066, -1.940345832946618554 ) ) ;
#119334 = CARTESIAN_POINT ( 'NONE',  ( 0.2886476729930695373, -1.083662648423104891, 2.037333779670726930 ) ) ;
#119335 = CARTESIAN_POINT ( 'NONE',  ( 0.2386218892466463737, -1.902018210125755004, -0.4804332253167050149 ) ) ;
#119336 = CARTESIAN_POINT ( 'NONE',  ( 3.766515156912704665, -0.8315086482118605460, -1.887695802070661344 ) ) ;
#119337 = CARTESIAN_POINT ( 'NONE',  ( 5.178851490740196795, 7.065079377328788546, 1.443375672974062551 ) ) ;
#119338 = ADVANCED_FACE ( 'NONE', ( #208892 ), #89859, .T. ) ;
#119339 = CARTESIAN_POINT ( 'NONE',  ( 6.204791576909545192, 7.267953590263130259, -1.199719254218452047 ) ) ;
#119340 = ORIENTED_EDGE ( 'NONE', *, *, #195398, .F. ) ;
#119341 = CARTESIAN_POINT ( 'NONE',  ( 7.253248993186720561, 10.44557901115111065, 1.082531754730558626 ) ) ;
#119342 = CARTESIAN_POINT ( 'NONE',  ( -0.6823417656250212460, 5.113541667008086655, 1.181850606188767472 ) ) ;
#119343 = CARTESIAN_POINT ( 'NONE',  ( -10.35086068573297524, 3.817517357212610207, -6.072273895623982121 ) ) ;
#119344 = CARTESIAN_POINT ( 'NONE',  ( 5.138177029454841893, 7.017625839162543677, 1.443375672974062551 ) ) ;
#119345 = CARTESIAN_POINT ( 'NONE',  ( 6.883263157960365142, -0.007059606330772279746, 2.153658854459541416 ) ) ;
#119347 = CARTESIAN_POINT ( 'NONE',  ( 5.653808312887880660, 0.7519890275384639722, 1.680886247995525773 ) ) ;
#119346 = CARTESIAN_POINT ( 'NONE',  ( 6.972266317189433020E-16, 0.5000000006828014820, -1.225000000000012745 ) ) ;
#119348 = CARTESIAN_POINT ( 'NONE',  ( 11.92619525870748021, 12.57377703206318920, 1.328859154005125554 ) ) ;
#119349 = DIRECTION ( 'NONE',  ( 0.000000000000000000, 1.000000000000000000, 0.000000000000000000 ) ) ;
#119350 = DIRECTION ( 'NONE',  ( 1.040834085586084257E-15, 1.000000000000000000, -4.622230424712076367E-32 ) ) ;
#119351 = CARTESIAN_POINT ( 'NONE',  ( -4.313069242314466756, 7.435226253386592710, 1.131090909019900614 ) ) ;
#119352 = CARTESIAN_POINT ( 'NONE',  ( -0.2646952133101811433, 3.312294480054168933, -2.056620194547992053 ) ) ;
#119353 = CARTESIAN_POINT ( 'NONE',  ( 5.396826230253299883, 7.665096674459883630, -1.326205021280580265 ) ) ;
#119354 = CARTESIAN_POINT ( 'NONE',  ( 1.364683531249990311, 5.196875000341417916, 1.214306433183764966E-14 ) ) ;
#119355 = CARTESIAN_POINT ( 'NONE',  ( 1.594246750649646494, -1.022002606473694675, 1.616071880676916317 ) ) ;
#119356 = CARTESIAN_POINT ( 'NONE',  ( 2.113771285056417426, -0.8311870117129838142, -1.562508279020339064 ) ) ;
#119357 = CARTESIAN_POINT ( 'NONE',  ( 5.865890606937535168, 0.5820329372835297832, -1.927131433562751406 ) ) ;
#119359 = CARTESIAN_POINT ( 'NONE',  ( 4.024928501738918030, -1.664925135935046763, 0.9472863605698205181 ) ) ;
#119358 = CARTESIAN_POINT ( 'NONE',  ( -10.00321840878439339, 10.56484298653695397, 1.040834085586084257E-14 ) ) ;
#119360 = DIRECTION ( 'NONE',  ( 0.000000000000000000, 0.000000000000000000, 1.000000000000000000 ) ) ;
#119361 = CARTESIAN_POINT ( 'NONE',  ( 5.055114266443681004, 1.638575763527612583, -1.092465951337840524 ) ) ;
#119362 = CARTESIAN_POINT ( 'NONE',  ( 6.398695825915057256, -1.981597308308700844, -0.3899587018172407382 ) ) ;
#119363 = CARTESIAN_POINT ( 'NONE',  ( 2.540684401258877401, -0.3622604021566167010, -0.2586409171621159020 ) ) ;
#119364 = CARTESIAN_POINT ( 'NONE',  ( 4.012460596634464416, 1.323225596166040186, -1.322536486416127977 ) ) ;
#119366 = VERTEX_POINT ( 'NONE', #126684 ) ;
#119365 = CARTESIAN_POINT ( 'NONE',  ( 5.936138232048088881, 0.8439337091313244832, -1.504256470664022238 ) ) ;
#119368 = CARTESIAN_POINT ( 'NONE',  ( 3.931501358282940117, 4.649468341827285300, -1.082531754730543083 ) ) ;
#119367 = CARTESIAN_POINT ( 'NONE',  ( 3.282038605231399231, 1.400092287458438722, 1.705885466304429166 ) ) ;
#119369 = CARTESIAN_POINT ( 'NONE',  ( -1.364683531249997417, 4.071875000341417028, 1.214306433183764966E-14 ) ) ;
#119370 = CARTESIAN_POINT ( 'NONE',  ( 0.7485702846574161518, -2.046882729015482738, -0.2544144183350918742 ) ) ;
#119371 = CARTESIAN_POINT ( 'NONE',  ( 7.775764792637399836, 9.030479331953833011, -1.199719254218441611 ) ) ;
#119373 = CARTESIAN_POINT ( 'NONE',  ( -9.691380875670077444, 10.20103253123691189, 0.7998128361456462443 ) ) ;
#119372 = AXIS2_PLACEMENT_3D ( 'NONE', #54433, #170299, #134641 ) ;
#119374 = CARTESIAN_POINT ( 'NONE',  ( -9.048073855341844052, 15.44705409027664089, -7.818180454737184704 ) ) ;
#119375 = CARTESIAN_POINT ( 'NONE',  ( 0.1747926744264677867, 6.948552888299643904, -2.450368216405907962 ) ) ;
#119376 = CARTESIAN_POINT ( 'NONE',  ( -4.543700865150305468, 8.221430542475131276, -0.3925545784149546691 ) ) ;
#119377 = ORIENTED_EDGE ( 'NONE', *, *, #15073, .T. ) ;
#119378 = CARTESIAN_POINT ( 'NONE',  ( 2.910663983731573090, 0.6951178490613962868, 1.950330170896700022 ) ) ;
#119380 = CARTESIAN_POINT ( 'NONE',  ( -1.499999999999997780, 4.650000000000022560, 1.214306433183764966E-14 ) ) ;
#119379 = CIRCLE ( 'NONE', #25901, 10.97656854249491332 ) ;
#119381 = CARTESIAN_POINT ( 'NONE',  ( 5.996784015946103885, 5.890669528225568996, 1.040834085586084257E-14 ) ) ;
#119382 = CARTESIAN_POINT ( 'NONE',  ( -6.292453103784333202, 6.974073686386621951, 0.9489479220791104952 ) ) ;
#119383 = CARTESIAN_POINT ( 'NONE',  ( 0.6803390939152150763, 0.9973279206440927025, 1.756184504224398202 ) ) ;
#119384 = ORIENTED_EDGE ( 'NONE', *, *, #19510, .T. ) ;
#119386 = CARTESIAN_POINT ( 'NONE',  ( 6.792271770766432404, 10.86814146596211472, 1.040834085586084257E-14 ) ) ;
#119385 = CARTESIAN_POINT ( 'NONE',  ( 0.07499057489264347731, 1.360887136235461758, -2.209073988085366480 ) ) ;
#119387 = CARTESIAN_POINT ( 'NONE',  ( 6.696638777208028692, -1.314797947003863543, -1.528504179509587280 ) ) ;
#119388 = CARTESIAN_POINT ( 'NONE',  ( 5.559766488213514712, 1.146785110015311915, 1.534377285673252267 ) ) ;
#119389 = CARTESIAN_POINT ( 'NONE',  ( 6.539320575229251808, 2.414832891527439962, 2.584256253838035366 ) ) ;
#119390 = CARTESIAN_POINT ( 'NONE',  ( 3.755584314896889264, 2.174856280799509545, -0.2696606696684644700 ) ) ;
#119391 = CIRCLE ( 'NONE', #28877, 0.04999999999999930889 ) ;
#119392 = CARTESIAN_POINT ( 'NONE',  ( -1.201851678989727383E-14, 2.743750000682820378, 1.732050807568877637 ) ) ;
#119393 = CARTESIAN_POINT ( 'NONE',  ( 3.076317393561965208, 0.8638369986560844316, 1.706277067364106115 ) ) ;
#119394 = CARTESIAN_POINT ( 'NONE',  ( -5.427341564172148303, 5.226320001155936090, 0.000000000000000000 ) ) ;
#119395 = CARTESIAN_POINT ( 'NONE',  ( 4.989037339704528229, 4.922891105851139315, 1.040834085586084257E-14 ) ) ;
#119397 = CARTESIAN_POINT ( 'NONE',  ( 0.7554827284574801016, 1.942536278707338360, -0.5405140857882018146 ) ) ;
#119396 = CARTESIAN_POINT ( 'NONE',  ( 10.18461545817735470, 3.956598013261175772, -5.433575010662928584 ) ) ;
#119398 = CARTESIAN_POINT ( 'NONE',  ( 1.364683531249996529, 11.52604166700806410, 0.7879004041258405033 ) ) ;
#119400 = CARTESIAN_POINT ( 'NONE',  ( -5.143339171537843590, 7.093924681584509173, 1.599625672291263179 ) ) ;
#119399 = CARTESIAN_POINT ( 'NONE',  ( 6.181208317857348256, 1.509947553572440704, 1.588605474358975478 ) ) ;
#119402 = ORIENTED_EDGE ( 'NONE', *, *, #100779, .F. ) ;
#119401 = CARTESIAN_POINT ( 'NONE',  ( 3.487030103973333794, 1.559624344477263502, -0.7367539641185815169 ) ) ;
#119403 = SURFACE_STYLE_USAGE ( .BOTH. , #152904 ) ;
#119404 = CARTESIAN_POINT ( 'NONE',  ( 6.272618624616828953, 10.46980549536166016, 1.040834085586084257E-14 ) ) ;
#119405 = CARTESIAN_POINT ( 'NONE',  ( 4.123651276850781144, 7.962676922967908411, -0.7998128361456221525 ) ) ;
#119406 = CARTESIAN_POINT ( 'NONE',  ( 11.89197415570409611, 11.30000000000000604, 0.8055989572471813354 ) ) ;
#119407 = CARTESIAN_POINT ( 'NONE',  ( 1.328483007144948935, -1.247240240105648601, 1.514344512384787622 ) ) ;
#119408 = CARTESIAN_POINT ( 'NONE',  ( -9.367496997601300279, 15.00000000000599343, -7.499999999995378808 ) ) ;
#119409 = CARTESIAN_POINT ( 'NONE',  ( 4.867540842506059562, 5.637551390133895168, -1.199719254218452047 ) ) ;
#119410 = CARTESIAN_POINT ( 'NONE',  ( 0.07516593201277278757, 5.721767059778611220, -2.638283098249011971 ) ) ;
#119411 = ORIENTED_EDGE ( 'NONE', *, *, #115651, .T. ) ;
#119412 = CARTESIAN_POINT ( 'NONE',  ( 2.680963302754415079, 0.4788041664859938318, -0.1016165050511480955 ) ) ;
#119413 = ORIENTED_EDGE ( 'NONE', *, *, #153496, .T. ) ;
#119414 = CARTESIAN_POINT ( 'NONE',  ( 3.404753564208697014, -0.3562933990706117493, -1.775892323017129737 ) ) ;
#119415 = AXIS2_PLACEMENT_3D ( 'NONE', #85776, #18629, #4487 ) ;
#119416 = ORIENTED_EDGE ( 'NONE', *, *, #192598, .F. ) ;
#119417 = CARTESIAN_POINT ( 'NONE',  ( 8.204655514564224816, 12.72384853363364066, 1.040834085586084257E-14 ) ) ;
#119418 = FACE_OUTER_BOUND ( 'NONE', #190510, .T. ) ;
#119419 = CARTESIAN_POINT ( 'NONE',  ( 4.758376837038695406, 1.806999933331495445, 0.1280191873242030876 ) ) ;
#119420 = CARTESIAN_POINT ( 'NONE',  ( 0.003376046620571365731, -7.161464053357560644, 9.586610838029431036 ) ) ;
#119421 = CARTESIAN_POINT ( 'NONE',  ( -6.392587740394328755, -6.532648833121157850, -6.999862025036979851 ) ) ;
#119422 = CARTESIAN_POINT ( 'NONE',  ( 4.778452461313970723, 6.762070782353614362, -1.245597109521460633 ) ) ;
#119424 = CARTESIAN_POINT ( 'NONE',  ( 8.367353357928214663, 12.91366268422496688, 1.040834085586084257E-14 ) ) ;
#119423 = CARTESIAN_POINT ( 'NONE',  ( 5.476954007041204164, 1.719599228052148154, 0.7121796456092708283 ) ) ;
#119425 = CARTESIAN_POINT ( 'NONE',  ( 2.636237813805066388, 0.6479696587880221514, 1.802806680411846774 ) ) ;
#119426 = CARTESIAN_POINT ( 'NONE',  ( 5.750066545971570520, 5.881034856487848295, -0.7216878364870458196 ) ) ;
#119427 = CARTESIAN_POINT ( 'NONE',  ( -10.45911201557330195, 5.175391108250987138, -5.201428006079835242 ) ) ;
#119428 = STYLED_ITEM ( 'NONE', ( #130855 ), #87643 ) ;
#119429 = CARTESIAN_POINT ( 'NONE',  ( 9.499623061593991835, -9.908700546396012498, -0.08463495275094053139 ) ) ;
#119430 = CARTESIAN_POINT ( 'NONE',  ( 5.356880090730862243, 7.343055753976412525, 1.443375672974064550 ) ) ;
#119431 = CARTESIAN_POINT ( 'NONE',  ( 5.504247177468168495, 9.365446107114122398, 0.7216878364870438212 ) ) ;
#119432 = CARTESIAN_POINT ( 'NONE',  ( -8.948018195339354719, 12.42280974699582607, 1.082531754730560403 ) ) ;
#119433 = DIRECTION ( 'NONE',  ( 1.000000000000000000, 0.000000000000000000, -3.491481338843133355E-15 ) ) ;
#119434 = CARTESIAN_POINT ( 'NONE',  ( -5.936491157937300756, 8.019268665717216749, 1.599625672291263179 ) ) ;
#119435 = CARTESIAN_POINT ( 'NONE',  ( 1.921934154048171584, 1.202774473455773041, -1.709796194579858319 ) ) ;
#119436 = CARTESIAN_POINT ( 'NONE',  ( 6.042093733545556233, 7.078139439671806699, -1.199719254218452047 ) ) ;
#119437 = CARTESIAN_POINT ( 'NONE',  ( 0.3580656308817787292, 0.6935259069400134813, 1.688922952486398454 ) ) ;
#119438 = CARTESIAN_POINT ( 'NONE',  ( -4.578903193113314174, 6.365139696764064325, 1.599625672291267398 ) ) ;
#119439 = CARTESIAN_POINT ( 'NONE',  ( 2.239018641000252607, -1.631965468365924377, 0.8183158014263000046 ) ) ;
#119440 = CARTESIAN_POINT ( 'NONE',  ( 0.000000000000000000, 7.849261790823902629, 0.000000000000000000 ) ) ;
#119441 = CARTESIAN_POINT ( 'NONE',  ( 1.968876373762207255, -1.476028252698018628, 1.215921256797661609 ) ) ;
#119442 = CARTESIAN_POINT ( 'NONE',  ( 2.189847533163618465, -1.284324338361255258, -1.493307823759764341 ) ) ;
#119443 = CARTESIAN_POINT ( 'NONE',  ( 3.228005407155889461, 1.895358990768666096, 0.4226955006484037214 ) ) ;
#119444 = CARTESIAN_POINT ( 'NONE',  ( -5.015590482412729756, 4.816220082428420923, 0.000000000000000000 ) ) ;
#119446 = CARTESIAN_POINT ( 'NONE',  ( 4.060867369437678676, 0.5686956411946364476, 2.042824496258560441 ) ) ;
#119445 = CARTESIAN_POINT ( 'NONE',  ( 8.154303043976348420, 8.478051404252736845, 0.7998128361456281477 ) ) ;
#119448 = EDGE_CURVE ( 'NONE', #16465, #129112, #153949, .T. ) ;
#119447 = CARTESIAN_POINT ( 'NONE',  ( 6.710127771514622808, -7.162053774861990796, 6.725445687907760650 ) ) ;
#119449 = CARTESIAN_POINT ( 'NONE',  ( 8.072990401933337168, 11.50590700464255356, -1.199719254218446718 ) ) ;
#119450 = CARTESIAN_POINT ( 'NONE',  ( 6.064713176501767222, 6.047104440226040545, 0.4075101515045934097 ) ) ;
#119451 = CARTESIAN_POINT ( 'NONE',  ( -1.123270288250315163, 2.985197346350006331, -0.7749999999993613109 ) ) ;
#119452 = ORIENTED_EDGE ( 'NONE', *, *, #195535, .T. ) ;
#119453 = CARTESIAN_POINT ( 'NONE',  ( 7.713663051532233972, 7.963971413067895355, -0.7998128361456341429 ) ) ;
#119454 = CARTESIAN_POINT ( 'NONE',  ( 11.97929049433705373, 12.22000000000000064, -0.7046979865771821894 ) ) ;
#119455 = CARTESIAN_POINT ( 'NONE',  ( 3.844227010333609584, 1.817057058749595777, 0.1772887374331885701 ) ) ;
#119456 = CARTESIAN_POINT ( 'NONE',  ( 0.1509401653462701109, -0.4529219869476922011, -2.027634260368789576 ) ) ;
#119457 = CARTESIAN_POINT ( 'NONE',  ( -9.354762803749327560, 10.01623748057011376, 0.7216878364870438212 ) ) ;
#119458 = CARTESIAN_POINT ( 'NONE',  ( -5.638125304375204649, 7.460809226315815224, 1.342380602066863160 ) ) ;
#119459 = DIRECTION ( 'NONE',  ( 1.776356839400250465E-15, 0.000000000000000000, -1.000000000000000000 ) ) ;
#119460 = CARTESIAN_POINT ( 'NONE',  ( 4.522238337509359773, 1.150754656758418593, -1.474723989322044959 ) ) ;
#119461 = CARTESIAN_POINT ( 'NONE',  ( 7.884230021546724920, 9.157022099014721306, 1.199719254218462483 ) ) ;
#119462 = CARTESIAN_POINT ( 'NONE',  ( 2.279798536657418495, 1.185040197188882871, 1.518827336823719953 ) ) ;
#119463 = CARTESIAN_POINT ( 'NONE',  ( -0.3859971386777985569, 2.800000000000025580, 1.330683448905541022 ) ) ;
#119464 = CARTESIAN_POINT ( 'NONE',  ( 3.192055101013606233, 5.811482486902795230, -1.199719254218446718 ) ) ;
#119465 = CARTESIAN_POINT ( 'NONE',  ( -1.364683531250000748, 9.171875000341403350, 0.000000000000000000 ) ) ;
#119466 = CARTESIAN_POINT ( 'NONE',  ( -6.307567778855718288, 8.381915046796901692, -1.599625672291263179 ) ) ;
#119467 = CARTESIAN_POINT ( 'NONE',  ( 3.876741858503734761, 6.610283703974623393, 1.199719254218462483 ) ) ;
#119468 = CARTESIAN_POINT ( 'NONE',  ( -5.438229012412911345, 5.517224400669388018, -0.7216878364870338292 ) ) ;
#119469 = AXIS2_PLACEMENT_3D ( 'NONE', #72367, #153644, #170946 ) ;
#119470 = EDGE_CURVE ( 'NONE', #170502, #138277, #209266, .T. ) ;
#119471 = CARTESIAN_POINT ( 'NONE',  ( 1.001738948178192645, -2.064706785862341132, 0.4679990497924620407 ) ) ;
#119472 = CARTESIAN_POINT ( 'NONE',  ( -1.872228381520322449, 3.300000000000011369, -0.3999999999999993006 ) ) ;
#119473 = CARTESIAN_POINT ( 'NONE',  ( 0.000000000000000000, 13.20000000000000284, 0.000000000000000000 ) ) ;
#119474 = CARTESIAN_POINT ( 'NONE',  ( 6.455931442665615805, -0.7031469350025701948, 1.947301169641938223 ) ) ;
#119476 = CARTESIAN_POINT ( 'NONE',  ( 4.230803266364135951, 7.299989629454814555, -0.8951707687023923166 ) ) ;
#119475 = CARTESIAN_POINT ( 'NONE',  ( 0.8020088176248600931, 1.394402496181508466, -1.202495849378336423 ) ) ;
#119477 = CARTESIAN_POINT ( 'NONE',  ( 0.3163000706473735879, -1.844146670390820475, 1.371622413452098233 ) ) ;
#119478 = CARTESIAN_POINT ( 'NONE',  ( 4.853455804012212660, 7.645820290447483458, 1.082531754730558626 ) ) ;
#119480 = SURFACE_SIDE_STYLE ('',( #170288 ) ) ;
#119479 = CARTESIAN_POINT ( 'NONE',  ( 5.072158865288243668, 6.050511776658669127, 1.082531754730549078 ) ) ;
#119481 = CARTESIAN_POINT ( 'NONE',  ( 1.236728449817244835, 0.4514257060114800213, 2.247219992417306411 ) ) ;
#119482 = CARTESIAN_POINT ( 'NONE',  ( 7.721398836998367265, -6.134628647623499909, -7.721398836998390358 ) ) ;
#119483 = CARTESIAN_POINT ( 'NONE',  ( -4.990283058281743678, 7.979691447040783814, -1.199719254218453823 ) ) ;
#119484 = CARTESIAN_POINT ( 'NONE',  ( 5.542900022196344700, -1.532237948119744342, -1.192973588722973100 ) ) ;
#119485 = ORIENTED_EDGE ( 'NONE', *, *, #23022, .F. ) ;
#119486 = CARTESIAN_POINT ( 'NONE',  ( 9.381879110532285182, 10.04787317181692075, 0.000000000000000000 ) ) ;
#119487 = CARTESIAN_POINT ( 'NONE',  ( 0.2814942100668381131, 0.1933317163467423994, -2.003872996790170724 ) ) ;
#119488 = CARTESIAN_POINT ( 'NONE',  ( 6.368375356916068597, -1.978549699825098429, -0.3886382054163611821 ) ) ;
#119489 = CARTESIAN_POINT ( 'NONE',  ( -6.665805079413154921, 10.92852302595736447, 0.7998128361456481317 ) ) ;
#119490 = DIRECTION ( 'NONE',  ( 0.9998476951563912696, 0.000000000000000000, -0.01745240643728004568 ) ) ;
#119492 = CARTESIAN_POINT ( 'NONE',  ( 0.9008075156715513732, 1.443549170786810443, 1.023676300919857507 ) ) ;
#119491 = CARTESIAN_POINT ( 'NONE',  ( 2.361375956566538648, 2.050102581710811389, -0.4087646360023765024 ) ) ;
#119493 = CARTESIAN_POINT ( 'NONE',  ( 4.121797130385867369, 7.239738145266779945, 1.078207043259531872 ) ) ;
#119494 = TOROIDAL_SURFACE ( 'NONE', #91784, 11.92000000000000171, 0.08000000000000000167 ) ;
#119496 = CARTESIAN_POINT ( 'NONE',  ( 4.664210274407590617, -1.499448637150493813, 1.733910808658318814 ) ) ;
#119495 = CARTESIAN_POINT ( 'NONE',  ( 5.408776937209000657, 5.274937613024121674, 0.7998128361456352531 ) ) ;
#119497 = CARTESIAN_POINT ( 'NONE',  ( 3.521201755802486844, -1.038059167858174092, -1.396672450663126508 ) ) ;
#119498 = CARTESIAN_POINT ( 'NONE',  ( 4.390142812726693045, 4.016254791136236513, 1.214306433183764966E-14 ) ) ;
#119499 = CARTESIAN_POINT ( 'NONE',  ( 6.073126464278658432, 6.050012061272033392, 0.000000000000000000 ) ) ;
#119500 = CARTESIAN_POINT ( 'NONE',  ( 3.409274926616968404, 0.4192967605245543905, 1.682228440661166502 ) ) ;
#119501 =( BOUNDED_CURVE ( )  B_SPLINE_CURVE ( 2, ( #43884, #46015, #42823, #208469, #142461, #47081, #145675 ),
 .UNSPECIFIED., .F., .T. ) 
 B_SPLINE_CURVE_WITH_KNOTS ( ( 3, 2, 2, 3 ),
 ( 0.1500000000000002165, 0.1541666666666668961, 0.1583333333333335480, 0.1625000000000002276 ),
 .UNSPECIFIED. ) 
 CURVE ( )  GEOMETRIC_REPRESENTATION_ITEM ( )  RATIONAL_B_SPLINE_CURVE ( ( 0.9999999999999928946, 0.8660254037844458130, 1.000000000000000000, 0.8660254037844387076, 1.000000000000000000, 0.8660254037844316022, 1.000000000000007105 ) ) 
 REPRESENTATION_ITEM ( '' )  );
#119502 = CARTESIAN_POINT ( 'NONE',  ( 3.895131827238162536, 0.3151296210822142063, 2.148063795774640461 ) ) ;
#119503 = CARTESIAN_POINT ( 'NONE',  ( 4.310602774141044868, 7.116454772218158809, -1.199719254218452047 ) ) ;
#119504 = CARTESIAN_POINT ( 'NONE',  ( 4.733611406029458735, 0.6279933214467496860, -1.916352419866963697 ) ) ;
#119505 = CARTESIAN_POINT ( 'NONE',  ( 3.093750000000001776, -1.895863743164152071, -0.7852924748298234503 ) ) ;
#119506 = CARTESIAN_POINT ( 'NONE',  ( -1.201851678989727383E-14, 4.368750000682820378, -1.732050807568863648 ) ) ;
#119507 = CARTESIAN_POINT ( 'NONE',  ( 2.625899107431714175, -1.107553820047700199, -1.575994028688005644 ) ) ;
#119508 = CARTESIAN_POINT ( 'NONE',  ( -1.500000000000001110, 8.552083334016131744, 0.8660254037844419273 ) ) ;
#119509 = CARTESIAN_POINT ( 'NONE',  ( 4.799211390369230834, -0.2731021391014861188, -2.204526388291703221 ) ) ;
#119510 = VERTEX_POINT ( 'NONE', #141831 ) ;
#119511 = CARTESIAN_POINT ( 'NONE',  ( -0.2108831679770924727, 4.091978752061476321, -2.452067053820900622 ) ) ;
#119512 = CARTESIAN_POINT ( 'NONE',  ( -1.402160292154681736E-14, 1.587500000000018785, -1.732050807568863648 ) ) ;
#119513 = CARTESIAN_POINT ( 'NONE',  ( 7.298366762858032430, 7.409182732956175244, 1.040834085586084257E-14 ) ) ;
#119514 = CARTESIAN_POINT ( 'NONE',  ( 4.161989969270892153, 6.839110149915929249, 1.082531754730558626 ) ) ;
#119515 = CARTESIAN_POINT ( 'NONE',  ( -3.285556943750000070, -2.559374999522041172, 0.000000000000000000 ) ) ;
#119516 = CARTESIAN_POINT ( 'NONE',  ( 0.7686061912218185022, 2.218469807834182017, -0.1147041126551024554 ) ) ;
#119517 = CARTESIAN_POINT ( 'NONE',  ( 5.529730448059603454, 1.891198321494348633, -0.5216162335564683561 ) ) ;
#119518 = CARTESIAN_POINT ( 'NONE',  ( 8.324343129110697959, 9.774450407793066731, -1.082531754730543083 ) ) ;
#119519 = CARTESIAN_POINT ( 'NONE',  ( 6.714178486276241919, -1.057601618853749148, -1.999996817866441123 ) ) ;
#119520 = AXIS2_PLACEMENT_3D ( 'NONE', #201714, #37101, #20829 ) ;
#119521 = CARTESIAN_POINT ( 'NONE',  ( 5.662465432362883355, 6.635239754958710989, 1.199719254218451159 ) ) ;
#119522 = CARTESIAN_POINT ( 'NONE',  ( -5.804299160426249493, 5.944306240018289778, -0.7216878364870338292 ) ) ;
#119523 = CARTESIAN_POINT ( 'NONE',  ( 3.789554774376595159, -1.906935327315992579, 0.7867413014382127479 ) ) ;
#119524 = CARTESIAN_POINT ( 'NONE',  ( -3.554208825076827782, 7.298327395898266623, 0.7998128361456341429 ) ) ;
#119525 = AXIS2_PLACEMENT_3D ( 'NONE', #172130, #106109, #23725 ) ;
#119526 = CARTESIAN_POINT ( 'NONE',  ( 0.7499999999999885647, 3.347916667349487341, -1.299038105676658228 ) ) ;
#119527 = CARTESIAN_POINT ( 'NONE',  ( 1.364683531249988535, 5.217708333674750065, -0.7879004041258300672 ) ) ;
#119528 = CARTESIAN_POINT ( 'NONE',  ( 5.325416506339426981, -1.776575524504429016, 0.5857008802128694791 ) ) ;
#119529 = CARTESIAN_POINT ( 'NONE',  ( 5.291581958225426874, 1.307657812419236176, -1.139094164941084841 ) ) ;
#119530 = CARTESIAN_POINT ( 'NONE',  ( 3.087183437724149826, -0.7025620359558025774, 1.592517242405028233 ) ) ;
#119531 = CARTESIAN_POINT ( 'NONE',  ( 1.910137617552462030, -1.084854587848137708, -2.019442561568355110 ) ) ;
#119532 = CARTESIAN_POINT ( 'NONE',  ( -1.364683531249997417, 3.821875000341416584, 1.214306433183764966E-14 ) ) ;
#119534 = CARTESIAN_POINT ( 'NONE',  ( 5.249593148720715696, 2.088313038247250120, -0.1037309089504182269 ) ) ;
#119533 = B_SPLINE_CURVE_WITH_KNOTS ( 'NONE', 3,
 ( #23924, #90029, #156085, #107394, #179796, #128991, #15131, #143068, #159269, #30351 ),
 .UNSPECIFIED., .F., .F.,
 ( 4, 2, 2, 2, 4 ),
 ( 3.274218758650651739E-18, 0.0002021113321160316874, 0.0004042226642320600680, 0.0006063339963480846809, 0.0008084453284641086434 ),
 .UNSPECIFIED. ) ;
#119535 = CARTESIAN_POINT ( 'NONE',  ( 6.650339433524894872, -1.499410535642144549, 1.233700977392115705 ) ) ;
#119536 = CARTESIAN_POINT ( 'NONE',  ( 7.714278451735655587E-14, -9.900000000000003908, 11.00029519899101160 ) ) ;
#119537 =( NAMED_UNIT ( * ) SI_UNIT ( $, .STERADIAN. ) SOLID_ANGLE_UNIT ( ) );
#119538 = CARTESIAN_POINT ( 'NONE',  ( 1.389296306420295224, -0.7283806465635984662, -1.880434191983325398 ) ) ;
#119539 = CARTESIAN_POINT ( 'NONE',  ( 0.4807640440005827576, -0.2721776580492247799, -2.174417363000572756 ) ) ;
#119540 = CARTESIAN_POINT ( 'NONE',  ( 9.634427881463707877, 13.63015724552533037, -8.222364378050974310 ) ) ;
#119541 = CARTESIAN_POINT ( 'NONE',  ( -9.203287345578106127, 9.631590079462940324, 0.7998128361456462443 ) ) ;
#119542 = CARTESIAN_POINT ( 'NONE',  ( 7.006866460164219212, 7.069099046480051385, -0.7998128361456281477 ) ) ;
#119543 = CARTESIAN_POINT ( 'NONE',  ( 2.684367718930933844, 1.136400967617630986, 1.790090880730066392 ) ) ;
#119544 = CARTESIAN_POINT ( 'NONE',  ( -2.788906526875773208E-15, 10.46875000068279604, -1.499999999999998446 ) ) ;
#119545 = CARTESIAN_POINT ( 'NONE',  ( 5.004447790439923160, -0.6182884515001166870, -1.717943145347331502 ) ) ;
#119546 = ORIENTED_EDGE ( 'NONE', *, *, #195328, .T. ) ;
#119547 = CARTESIAN_POINT ( 'NONE',  ( -7.618755976236585958, 7.853246491889623648, 0.000000000000000000 ) ) ;
#119548 = DIRECTION ( 'NONE',  ( 0.000000000000000000, 0.000000000000000000, 1.000000000000000000 ) ) ;
#119549 = CARTESIAN_POINT ( 'NONE',  ( -1.642778471874998480, -0.8385416661887100664, 2.845375778867863303 ) ) ;
#119550 = CARTESIAN_POINT ( 'NONE',  ( -6.170932472514347289, 10.35117165124207972, 0.000000000000000000 ) ) ;
#119551 = CARTESIAN_POINT ( 'NONE',  ( 2.355728564803623915, -1.499445635549499389, -1.353443481924651470 ) ) ;
#119552 = CARTESIAN_POINT ( 'NONE',  ( 0.4816451290811329389, 1.964891932219949844, -0.7582931990086133611 ) ) ;
#119553 = CARTESIAN_POINT ( 'NONE',  ( -2.959422669532919326, 6.674686557755516780, 0.7998128361456352531 ) ) ;
#119554 = CARTESIAN_POINT ( 'NONE',  ( 3.836619860451701669, -1.792334419201064399, -0.5002748670543122333 ) ) ;
#119555 = CARTESIAN_POINT ( 'NONE',  ( 9.402743226277308963, 10.92862083786708816, -1.199719254218446718 ) ) ;
#119556 = CARTESIAN_POINT ( 'NONE',  ( 11.94105721237522921, 13.52740784401788687, -1.187919463087249605 ) ) ;
#119557 = CARTESIAN_POINT ( 'NONE',  ( -2.252626078164912560, 5.779814191167667481, 0.7998128361456341429 ) ) ;
#119558 = CARTESIAN_POINT ( 'NONE',  ( -8.993135964566285168, 9.386413468282476913, -0.7998128361456291469 ) ) ;
#119559 = CARTESIAN_POINT ( 'NONE',  ( 5.566980414702134894, -1.652319403193935887, -0.7768266693391965294 ) ) ;
#119560 = VECTOR ( 'NONE', #45880, 1000.000000000000000 ) ;
#119562 = CARTESIAN_POINT ( 'NONE',  ( -4.153809255294044434, 7.618134729639562508, -0.8777755718400248597 ) ) ;
#119561 = CARTESIAN_POINT ( 'NONE',  ( -5.088052786878465739, 9.158088361325352977, 0.000000000000000000 ) ) ;
#119563 = CARTESIAN_POINT ( 'NONE',  ( 4.960800185296459830, 8.075801985472857325, -1.085925974634168290 ) ) ;
#119564 = CARTESIAN_POINT ( 'NONE',  ( 1.686441086386183619, -0.9581320880991549549, -1.444804011637023322 ) ) ;
#119565 = CARTESIAN_POINT ( 'NONE',  ( 6.386648935047418263, 1.599332519906123462, -0.9119682274050244786 ) ) ;
#119567 = CARTESIAN_POINT ( 'NONE',  ( 7.998947442382716488, 9.394822106610419610, -1.082531754730543083 ) ) ;
#119566 = CARTESIAN_POINT ( 'NONE',  ( 5.162836451262333703, -1.674513216643868985, 1.588141549981958001 ) ) ;
#119568 = CARTESIAN_POINT ( 'NONE',  ( -10.44369633504468631, 5.112959841837462882, -5.232137017608344820 ) ) ;
#119569 = CARTESIAN_POINT ( 'NONE',  ( 1.757177114327221901, -1.766000478700447074, -1.061884917490847791 ) ) ;
#119570 = CARTESIAN_POINT ( 'NONE',  ( 4.645640190976921602, 8.571663989448405019, 1.040834085586084257E-14 ) ) ;
#119571 = ADVANCED_FACE ( 'NONE', ( #207835 ), #60523, .F. ) ;
#119572 = CARTESIAN_POINT ( 'NONE',  ( 6.643951024375948755, -0.1027215121673381443, -2.296211363497886460 ) ) ;
#119573 = CARTESIAN_POINT ( 'NONE',  ( 8.220249535482631487, 15.16568599130686223, -8.682936656944493237 ) ) ;
#119574 = CARTESIAN_POINT ( 'NONE',  ( -5.803772275101700906, 8.928762199997411386, -1.199719254218452047 ) ) ;
#119575 = CARTESIAN_POINT ( 'NONE',  ( 6.561405567229332547, 0.3174558530528898692, -1.843364171016811603 ) ) ;
#119576 = AXIS2_PLACEMENT_3D ( 'NONE', #175593, #111714, #112781 ) ;
#119577 = EDGE_CURVE ( 'NONE', #188383, #160603, #194830, .T. ) ;
#119579 = CARTESIAN_POINT ( 'NONE',  ( -3.471769853551161411, 6.208092708188416076, 1.199719254218452935 ) ) ;
#119578 = CARTESIAN_POINT ( 'NONE',  ( 3.937688585161042809, -1.828529804631402023, 0.5600222464785462595 ) ) ;
#119580 = CARTESIAN_POINT ( 'NONE',  ( 4.723365791888975096, -0.1103408873950258995, 2.204240794804641190 ) ) ;
#119581 = CARTESIAN_POINT ( 'NONE',  ( 0.6124999999999776179, 1.479166667349464337, -1.060881119635962211 ) ) ;
#119582 = CARTESIAN_POINT ( 'NONE',  ( -7.607533590599451223, 9.008448956188397361, 1.082531754730549078 ) ) ;
#119583 = CARTESIAN_POINT ( 'NONE',  ( 5.194182247366878613, 6.192872389083746043, 1.082531754730549078 ) ) ;
#119584 = TOROIDAL_SURFACE ( 'NONE', #26125, 3.971937515251341644, 0.08000000000000000167 ) ;
#119585 = CARTESIAN_POINT ( 'NONE',  ( -5.004368096775595021, 5.971422546727199077, 1.082531754730549078 ) ) ;
#119586 = CARTESIAN_POINT ( 'NONE',  ( 5.830757645730302308, 1.424217953154560012, -1.571192434731554677 ) ) ;
#119587 = VERTEX_POINT ( 'NONE', #110421 ) ;
#119588 = CARTESIAN_POINT ( 'NONE',  ( 3.927071981709300719, 2.190135382617847792, 0.7269923479944776501 ) ) ;
#119589 = CARTESIAN_POINT ( 'NONE',  ( 3.912515228517557286, 0.7039278570535618673, 1.831416474553926310 ) ) ;
#119590 = CARTESIAN_POINT ( 'NONE',  ( -3.786470039966538970, 7.639575156594750283, 0.000000000000000000 ) ) ;
#119591 = CARTESIAN_POINT ( 'NONE',  ( 1.076917802502619592, 1.810449747239597951, 0.7559744942375111743 ) ) ;
#119592 = FACE_OUTER_BOUND ( 'NONE', #194742, .T. ) ;
#119593 = CYLINDRICAL_SURFACE ( 'NONE', #60855, 0.09999999999999971412 ) ;
#119594 = ORIENTED_EDGE ( 'NONE', *, *, #106096, .F. ) ;
#119595 = CARTESIAN_POINT ( 'NONE',  ( 5.999232488047272049, -0.2420365156972601739, 2.001857322483958423 ) ) ;
#119596 = CARTESIAN_POINT ( 'NONE',  ( -7.486073373039941359, 11.88550270185529278, -0.7998128361456291469 ) ) ;
#119597 = CARTESIAN_POINT ( 'NONE',  ( -0.01213283819992416745, -0.3988646234997471618, -1.803908381610368261 ) ) ;
#119598 = CARTESIAN_POINT ( 'NONE',  ( 3.151421466623941292, 1.864366918651944927, -1.112252681494025897 ) ) ;
#119599 = CARTESIAN_POINT ( 'NONE',  ( 9.955160869828317161, 11.52437543985780266, -6.705892285181387358 ) ) ;
#119600 = CARTESIAN_POINT ( 'NONE',  ( 0.4750491441844888474, -1.531729482103380224, 1.466773057065169361 ) ) ;
#119601 = CARTESIAN_POINT ( 'NONE',  ( 1.499999999999987121, 2.077083334016153415, -0.8660254037844262731 ) ) ;
#119602 = CARTESIAN_POINT ( 'NONE',  ( 8.191097360950562845, 12.70803068775103739, -0.7998128361456352531 ) ) ;
#119603 = CARTESIAN_POINT ( 'NONE',  ( -1.833504494307588661, 2.521637134586328877, -2.499652564413211042 ) ) ;
#119604 = CARTESIAN_POINT ( 'NONE',  ( 6.592372495380235620, 6.775069446727209233, 0.2122460957004346782 ) ) ;
#119605 = CARTESIAN_POINT ( 'NONE',  ( 1.616555492630408875, 1.386288697630438715, -1.524948804171057493 ) ) ;
#119607 = CARTESIAN_POINT ( 'NONE',  ( 3.125598124496329360E-16, 2.519999999999999130, 2.000000000000000000 ) ) ;
#119606 = CARTESIAN_POINT ( 'NONE',  ( -10.49131193887636826, 11.13428543831092909, 1.040834085586084257E-14 ) ) ;
#119608 = CARTESIAN_POINT ( 'NONE',  ( -1.402160292154681736E-14, 2.196875000341423689, -1.575800808251660134 ) ) ;
#119609 = DIRECTION ( 'NONE',  ( 0.000000000000000000, 0.000000000000000000, 1.000000000000000000 ) ) ;
#119610 = ORIENTED_EDGE ( 'NONE', *, *, #137765, .F. ) ;
#119611 = CARTESIAN_POINT ( 'NONE',  ( 4.740819843082155316, 1.831016553098392619, 0.5515768964349797576 ) ) ;
#119612 = CARTESIAN_POINT ( 'NONE',  ( 1.499999999999993117, 9.385416667349463893, 0.8660254037844408170 ) ) ;
#119613 = CARTESIAN_POINT ( 'NONE',  ( 5.203297092594585393, 9.292540051327542017, 0.7998128361456341429 ) ) ;
#119614 = CARTESIAN_POINT ( 'NONE',  ( -3.144601563365788444, 5.756120026313656268, -1.199719254218452935 ) ) ;
#119616 = EDGE_CURVE ( 'NONE', #194102, #184826, #107056, .T. ) ;
#119615 = CARTESIAN_POINT ( 'NONE',  ( 0.7733460811225587594, 0.3524055278083237930, -1.776778109436588204 ) ) ;
#119618 = CARTESIAN_POINT ( 'NONE',  ( 0.4971116367980681350, -0.2779505141972256066, 1.895288638825567862 ) ) ;
#119617 = CARTESIAN_POINT ( 'NONE',  ( 7.404765023120892131, -6.836271202499960786, 7.949604103952387035 ) ) ;
#119619 = CARTESIAN_POINT ( 'NONE',  ( 2.488806849732328796, 2.007603858877416769, 0.5053560088097220904 ) ) ;
#119620 = CARTESIAN_POINT ( 'NONE',  ( 0.6823417656249882723, -0.2614583329919109578, -1.181850606188749264 ) ) ;
#119621 = CARTESIAN_POINT ( 'NONE',  ( 0.4617158845385913590, 1.950347379310466422, -0.2869839225536646166 ) ) ;
#119622 = CARTESIAN_POINT ( 'NONE',  ( 2.613660848560446226, -1.805822647967849193, 0.2677728182119283318 ) ) ;
#119624 = CARTESIAN_POINT ( 'NONE',  ( 6.174897528274166270, 6.957956273452501783, 0.8961316764096085574 ) ) ;
#119623 = CARTESIAN_POINT ( 'NONE',  ( 0.1007806894988797913, -2.307328790448114120, -0.04970016441883937791 ) ) ;
#119625 = CARTESIAN_POINT ( 'NONE',  ( -1.364683531250000748, 2.009375000341421913, 1.214306433183764966E-14 ) ) ;
#119626 = CARTESIAN_POINT ( 'NONE',  ( 4.492669715648281326, 2.022274968565600517, 0.4054665169595774721 ) ) ;
#119627 = CARTESIAN_POINT ( 'NONE',  ( -7.711890448074853133, 7.891627032375787998, -0.7998128361456291469 ) ) ;
#119628 = CARTESIAN_POINT ( 'NONE',  ( 8.450809820019639318, 8.753699632978056755, -0.7998128361456291469 ) ) ;
#119629 = CARTESIAN_POINT ( 'NONE',  ( 4.867540842506059562, 5.637551390133895168, -1.199719254218452047 ) ) ;
#119630 = CARTESIAN_POINT ( 'NONE',  ( 5.087333953625774008, 6.958308917361963886, 1.599625672291267398 ) ) ;
#119632 = CARTESIAN_POINT ( 'NONE',  ( 0.7499999999999902300, 4.066666666666690411, -1.299038105676658228 ) ) ;
#119631 = CARTESIAN_POINT ( 'NONE',  ( 5.825249245718299385, -0.05505390245461554838, 2.105416907300653673 ) ) ;
#119633 = EDGE_CURVE ( 'NONE', #182678, #116046, #91662, .T. ) ;
#119634 = CARTESIAN_POINT ( 'NONE',  ( 0.2390591215055883068, -2.106223889411312999, -0.5266447289704286883 ) ) ;
#119635 = CARTESIAN_POINT ( 'NONE',  ( -1.402160292154681736E-14, 1.759375000341421469, -1.575800808251659024 ) ) ;
#119636 = CARTESIAN_POINT ( 'NONE',  ( 3.708425082824120533, -0.8722964037291662809, -1.977944213000272455 ) ) ;
#119637 = CARTESIAN_POINT ( 'NONE',  ( 3.932289538495234549, -1.040048408385336964, -1.731156807262229425 ) ) ;
#119638 = CARTESIAN_POINT ( 'NONE',  ( 6.620655732516647518, 3.684600858287550906, 2.687722323901103660 ) ) ;
#119641 = CARTESIAN_POINT ( 'NONE',  ( 6.480434237652135998, 6.662854153456708950, 0.7216878364870317197 ) ) ;
#119640 = CARTESIAN_POINT ( 'NONE',  ( -3.475000000000000533, 0.000000000000000000, 0.000000000000000000 ) ) ;
#119639 = DIRECTION ( 'NONE',  ( 0.000000000000000000, 0.000000000000000000, -1.000000000000000000 ) ) ;
#119642 = CARTESIAN_POINT ( 'NONE',  ( -6.805266759416629618, 6.904175738932996964, 0.000000000000000000 ) ) ;
#119643 = CARTESIAN_POINT ( 'NONE',  ( 2.887907956677421506, -2.014008092954455265, 0.1037802451031161477 ) ) ;
#119644 = CARTESIAN_POINT ( 'NONE',  ( -9.287498920561160887, 10.79416914786490089, -1.199719254218441611 ) ) ;
#119646 = SURFACE_STYLE_FILL_AREA ( #172612 ) ;
#119645 = CARTESIAN_POINT ( 'NONE',  ( -5.101945877444165944, 4.846691699973280976, 0.000000000000000000 ) ) ;
#119647 = CARTESIAN_POINT ( 'NONE',  ( -1.402160292154681736E-14, 8.671875000341403350, 1.575800808251682339 ) ) ;
#119648 = DIRECTION ( 'NONE',  ( -0.000000000000000000, 1.000000000000000000, -0.000000000000000000 ) ) ;
#119650 = CARTESIAN_POINT ( 'NONE',  ( 4.974232547167513729, -2.001514726140873890, -0.2440111082952014510 ) ) ;
#119649 = CARTESIAN_POINT ( 'NONE',  ( -7.009202228140739344, 11.12122699956546334, -0.7216878364870267237 ) ) ;
#119651 = CARTESIAN_POINT ( 'NONE',  ( -0.7499999999999972244, 5.108333333333353821, -1.299038105676652011 ) ) ;
#119652 = CARTESIAN_POINT ( 'NONE',  ( 0.1524156081505250449, -1.388816673012055025, 1.022707173280016368 ) ) ;
#119653 = CARTESIAN_POINT ( 'NONE',  ( 4.712340909201580885, 7.655425606447271214, -1.199719254218452047 ) ) ;
#119655 = CARTESIAN_POINT ( 'NONE',  ( 0.1025498324992813182, -6.714092063936424992, 10.99981089498244380 ) ) ;
#119654 = CARTESIAN_POINT ( 'NONE',  ( 8.107412671292031803, 11.44210330227398487, 1.082531754730557072 ) ) ;
#119656 = CARTESIAN_POINT ( 'NONE',  ( 0.000000000000000000, 4.000000000000003553, 0.000000000000000000 ) ) ;
#119657 = CARTESIAN_POINT ( 'NONE',  ( 5.905500869136258046, -0.4549164269060863020, 1.814235589242949587 ) ) ;
#119658 = CARTESIAN_POINT ( 'NONE',  ( 6.187749739576326569, 1.925281575520617849, -0.5883678985393098193 ) ) ;
#119659 = FACE_OUTER_BOUND ( 'NONE', #154331, .T. ) ;
#119660 = CARTESIAN_POINT ( 'NONE',  ( -7.390603132780795725, 8.755363422066633206, -1.082531754730549967 ) ) ;
#119661 = ORIENTED_EDGE ( 'NONE', *, *, #200299, .F. ) ;
#119662 = CARTESIAN_POINT ( 'NONE',  ( 10.68346185744421462, 11.56638637654751989, 0.000000000000000000 ) ) ;
#119663 = CARTESIAN_POINT ( 'NONE',  ( 1.212517793387542842, 1.944078472882956987, 0.5350667013180390175 ) ) ;
#119664 = CARTESIAN_POINT ( 'NONE',  ( 4.001064729364292916, 6.721640380016713934, -1.082531754730548412 ) ) ;
#119665 = LINE ( 'NONE', #154244, #79923 ) ;
#119666 = CARTESIAN_POINT ( 'NONE',  ( 7.239690839573049708, 11.39013037956983965, 1.040834085586084257E-14 ) ) ;
#119667 = CARTESIAN_POINT ( 'NONE',  ( 8.098297826064319693, 8.342435640030188893, 0.7998128361456481317 ) ) ;
#119669 = CARTESIAN_POINT ( 'NONE',  ( 6.292599812010432281, 1.415705964336026357, -1.290654269910092911 ) ) ;
#119668 = CARTESIAN_POINT ( 'NONE',  ( -4.232116505760120440, 8.089219690028791376, -0.7998128361456281477 ) ) ;
#119670 = CARTESIAN_POINT ( 'NONE',  ( 0.000000000000000000, 13.79999999999998295, 0.000000000000000000 ) ) ;
#119671 = DIRECTION ( 'NONE',  ( -3.497202527569253358E-15, 0.000000000000000000, -1.000000000000000000 ) ) ;
#119672 = VECTOR ( 'NONE', #33961, 1000.000000000000000 ) ;
#119673 = CARTESIAN_POINT ( 'NONE',  ( 5.111060722227499298, 8.906728576000002562, -0.7216878364870267237 ) ) ;
#119674 = CARTESIAN_POINT ( 'NONE',  ( 1.387358672525639269, 7.251968950354889643, 4.302625267139791987 ) ) ;
#119676 = ORIENTED_EDGE ( 'NONE', *, *, #124581, .F. ) ;
#119675 = CARTESIAN_POINT ( 'NONE',  ( 4.704316114261903436, 4.590716342834741504, 1.214306433183764966E-14 ) ) ;
#119677 = CARTESIAN_POINT ( 'NONE',  ( -10.62011439820619429, 11.28455497419572318, -0.7998128361456221525 ) ) ;
#119678 = CARTESIAN_POINT ( 'NONE',  ( 3.819328725847204620, -0.1613130240520690706, 2.155748724213396361 ) ) ;
#119679 = CARTESIAN_POINT ( 'NONE',  ( -7.268579750702160780, 8.613002809641560731, -1.082531754730549967 ) ) ;
#119680 = CARTESIAN_POINT ( 'NONE',  ( 6.875393295905841917, 7.193916064744513506, 0.000000000000000000 ) ) ;
#119681 = CARTESIAN_POINT ( 'NONE',  ( 1.213308285724056690, 1.730450836393576886, -1.225479750871574680 ) ) ;
#119682 = CARTESIAN_POINT ( 'NONE',  ( 5.649374308873757577, -1.440485763676568443, -1.121356984487072328 ) ) ;
#119683 =( BOUNDED_SURFACE ( )  B_SPLINE_SURFACE ( 3, 2, ( 
 ( #75672, #156937, #124509 ),
 ( #176376, #158007, #59414 ),
 ( #73529, #42128, #27982 ),
 ( #91945, #177437, #139631 ),
 ( #44249, #111434, #207786 ),
 ( #107167, #205654, #29054 ) ),
 .UNSPECIFIED., .F., .F., .T. ) 
 B_SPLINE_SURFACE_WITH_KNOTS ( ( 4, 2, 4 ),
 ( 3, 3 ),
 ( 0.000000000000000000, 0.0003766405729503173702, 0.0007532811459006347405 ),
 ( 0.000000000000000000, 1.000000000000000000 ),
 .UNSPECIFIED. ) 
 GEOMETRIC_REPRESENTATION_ITEM ( )  RATIONAL_B_SPLINE_SURFACE ( (
 ( 1.000000000000000000, 0.7071067811865551223, 1.000000000000000000),
 ( 1.000000000000000000, 0.7211294902955875941, 1.000000000000000000),
 ( 1.000000000000000000, 0.7311181975227702967, 1.000000000000000000),
 ( 1.000000000000000000, 0.7429553055063979894, 1.000000000000000000),
 ( 1.000000000000000000, 0.7451698531056455410, 1.000000000000000000),
 ( 1.000000000000000000, 0.7452309222762957264, 1.000000000000000000) ) ) 
 REPRESENTATION_ITEM ( '' )  SURFACE ( )  );
#119684 = CARTESIAN_POINT ( 'NONE',  ( 2.214082964306641532, -0.9260232682030484774, -1.740301080291997149 ) ) ;
#119685 = CARTESIAN_POINT ( 'NONE',  ( 4.148624843374196125, 1.876505540506741010, 0.3678670841067502861 ) ) ;
#119686 = VERTEX_POINT ( 'NONE', #64786 ) ;
#119687 = APPLICATION_CONTEXT ( 'automotive_design' ) ;
#119688 = CARTESIAN_POINT ( 'NONE',  ( -5.000000000000013323, 8.499999999999996447, 0.7750000000000004663 ) ) ;
#119689 = CARTESIAN_POINT ( 'NONE',  ( 6.127403468923573904, 0.1463605449630276667, -1.964188589371117954 ) ) ;
#119690 = CARTESIAN_POINT ( 'NONE',  ( 0.3748122768056568743, 1.812325467826606085, -0.6980362920307162655 ) ) ;
#119691 = ORIENTED_EDGE ( 'NONE', *, *, #148050, .F. ) ;
#119692 = CARTESIAN_POINT ( 'NONE',  ( -5.147255595043616516, 6.034161611419515125, 1.199719254218452935 ) ) ;
#119694 = CARTESIAN_POINT ( 'NONE',  ( 6.895452369244176261, -6.747656629766812131, -6.524021554744646956 ) ) ;
#119693 = CARTESIAN_POINT ( 'NONE',  ( -4.146814880933400005, 5.931313009212638931, 1.599625672291270506 ) ) ;
#119697 = EDGE_CURVE ( 'NONE', #2109, #132973, #171249, .T. ) ;
#119696 = CARTESIAN_POINT ( 'NONE',  ( 5.329763783503544516, 9.232158490813878515, -0.7216878364870458196 ) ) ;
#119695 = CARTESIAN_POINT ( 'NONE',  ( 7.151035956204054855, 10.43029348462504124, 1.199719254218460707 ) ) ;
#119699 = EDGE_LOOP ( 'NONE', ( #66579, #202620, #44058, #153061 ) ) ;
#119698 = CARTESIAN_POINT ( 'NONE',  ( 5.373660369522260005, 0.3689257714810100786, -1.876182517032434216 ) ) ;
#119700 = CARTESIAN_POINT ( 'NONE',  ( 0.3587983166186413109, 0.8468606107991830667, 2.038007455039527294 ) ) ;
#119701 = CARTESIAN_POINT ( 'NONE',  ( -5.634755928360857702, 5.776502004022960435, -0.2774256996143938947 ) ) ;
#119702 = CARTESIAN_POINT ( 'NONE',  ( 6.375645430456404306, 0.3419251235410331602, -1.983688181122665650 ) ) ;
#119703 = CARTESIAN_POINT ( 'NONE',  ( -1.500000000000008216, 8.750000000000000000, 3.469446951953614189E-15 ) ) ;
#119704 = CARTESIAN_POINT ( 'NONE',  ( -5.431221679128885427, 7.631776636990481144, 1.349246548148795632 ) ) ;
#119705 = CARTESIAN_POINT ( 'NONE',  ( -8.673617379884035472E-15, 3.487142912321097299, -11.99525683304594281 ) ) ;
#119706 = CARTESIAN_POINT ( 'NONE',  ( 2.752462066230080495, -2.064650614848703825, -0.1547973748374023295 ) ) ;
#119707 = CARTESIAN_POINT ( 'NONE',  ( -4.629219384062206011, 7.488174150459498968, -1.199719254218452047 ) ) ;
#119708 = VECTOR ( 'NONE', #180086, 1000.000000000000000 ) ;
#119709 = CARTESIAN_POINT ( 'NONE',  ( -4.907053429147543611, 8.030730943182621928, 0.9696864716568325271 ) ) ;
#119711 = CARTESIAN_POINT ( 'NONE',  ( 0.8487565004985967443, 0.6285140637429244004, 2.068326486519965979 ) ) ;
#119710 = CARTESIAN_POINT ( 'NONE',  ( -5.251085567194491155, 5.020688004682002159, -0.7998128361456221525 ) ) ;
#119712 = CARTESIAN_POINT ( 'NONE',  ( -11.98811477081661536, 9.050839079014156852, 0.6170501206370091474 ) ) ;
#119713 = CARTESIAN_POINT ( 'NONE',  ( -3.602337597214539753E-15, 12.81249999999999822, 1.500000000000001554 ) ) ;
#119714 = CARTESIAN_POINT ( 'NONE',  ( -0.6823417656250003738, 13.71354166700806942, 1.181850606188754593 ) ) ;
#119715 = ADVANCED_FACE ( 'NONE', ( #13891 ), #131968, .T. ) ;
#119717 = CARTESIAN_POINT ( 'NONE',  ( -4.132202957115018727, 8.042930226601317401, 0.000000000000000000 ) ) ;
#119716 = CARTESIAN_POINT ( 'NONE',  ( 6.825078400183550720, 7.629137130509051623, 2.555651831298339616 ) ) ;
#119718 = CARTESIAN_POINT ( 'NONE',  ( 5.520041967268690897, -1.564255855279505836, 0.7489400339724672229 ) ) ;
#119719 = CIRCLE ( 'NONE', #171597, 0.05000000000000007910 ) ;
#119721 = CARTESIAN_POINT ( 'NONE',  ( -2.930533758848195447, 6.570706485298192234, -0.7998128361456281477 ) ) ;
#119720 = VECTOR ( 'NONE', #150288, 1000.000000000000000 ) ;
#119722 = CARTESIAN_POINT ( 'NONE',  ( 4.065334711822697678, 1.773058433220272789, 1.068561072119569522 ) ) ;
#119723 = CARTESIAN_POINT ( 'NONE',  ( 4.939118062403117904, -1.789252976562827779, -1.131630611658622332 ) ) ;
#119724 = CARTESIAN_POINT ( 'NONE',  ( 6.479907352327590964, 9.647310113435821677, 1.199719254218462483 ) ) ;
#119725 = CARTESIAN_POINT ( 'NONE',  ( -1.364683531250010740, 4.530208333674754506, 0.7879004041258379498 ) ) ;
#119726 = CARTESIAN_POINT ( 'NONE',  ( 2.641402650619076198, 1.802640082279869382, -0.7936183362749064107 ) ) ;
#119727 = CARTESIAN_POINT ( 'NONE',  ( 1.107505169401588274, 1.450017293480215352, 1.247013401884336403 ) ) ;
#119728 = CARTESIAN_POINT ( 'NONE',  ( 4.629038687585553369, -2.096899809942855075, 0.9264041093646653291 ) ) ;
#119729 = CARTESIAN_POINT ( 'NONE',  ( 3.017977635683791071, -0.9002817137206723386, -1.588204215665294461 ) ) ;
#119730 = CIRCLE ( 'NONE', #53965, 0.08000000000000080658 ) ;
#119731 = CARTESIAN_POINT ( 'NONE',  ( 5.499767588998890844, 6.445425604367387429, 1.199719254218451159 ) ) ;
#119732 = CARTESIAN_POINT ( 'NONE',  ( 4.921246571636183731, 7.724909519342112674, -1.082531754730549078 ) ) ;
#119733 = CARTESIAN_POINT ( 'NONE',  ( -5.506582945444718824, 9.576097202994168001, 0.7998128361456481317 ) ) ;
#119734 = CARTESIAN_POINT ( 'NONE',  ( 4.377201702235844927, -1.800125857882298508, -0.9014936589236545172 ) ) ;
#119735 = CARTESIAN_POINT ( 'NONE',  ( 3.168751141962049545, 1.424179589570490512, -1.349414796185027576 ) ) ;
#119736 = CARTESIAN_POINT ( 'NONE',  ( -7.670162217029145246, 9.971608557999250166, 1.599625672291295375 ) ) ;
#119737 = CARTESIAN_POINT ( 'NONE',  ( -6.600121851754250812, 6.594563670001734046, 0.7998128361456341429 ) ) ;
#119738 = CARTESIAN_POINT ( 'NONE',  ( 0.1753634416057497647, 2.004068818557998011, -2.558292918872175914 ) ) ;
#119740 = CARTESIAN_POINT ( 'NONE',  ( 4.188192146485575584, -1.750654529572701179, -0.2590412592250490587 ) ) ;
#119739 = CARTESIAN_POINT ( 'NONE',  ( 6.052696072153842977, -1.792546385985850810, -1.075631278504029620 ) ) ;
#119741 = CARTESIAN_POINT ( 'NONE',  ( 4.903184595771473475, 4.840886387581087469, 0.6212912700429285007 ) ) ;
#119742 = CARTESIAN_POINT ( 'NONE',  ( 0.7268461993804631316, 0.1648446022758827123, 2.185306563462440899 ) ) ;
#119743 = CARTESIAN_POINT ( 'NONE',  ( 6.509682854689390119, -0.8273637111445523162, -1.531083434488962780 ) ) ;
#119744 = CARTESIAN_POINT ( 'NONE',  ( 6.805303039055573322, 10.02693841461847057, 1.199719254218460707 ) ) ;
#119745 = CARTESIAN_POINT ( 'NONE',  ( 0.1333692844072801587, 4.087911462428309051, -2.608372271572469092 ) ) ;
#119746 = CARTESIAN_POINT ( 'NONE',  ( 0.01170749999939314084, -0.7329999334961794233, -1.560365621481168086 ) ) ;
#119747 = CARTESIAN_POINT ( 'NONE',  ( 0.4042330683431404892, 0.3962127685512468744, 2.263842283499896801 ) ) ;
#119748 = CARTESIAN_POINT ( 'NONE',  ( 0.9432342461353732110, -1.730868645791438842, -1.344178957308760802 ) ) ;
#119749 = CARTESIAN_POINT ( 'NONE',  ( 3.475398437264758833, 0.05438942809191970457, -2.206374867412825402 ) ) ;
#119750 = CARTESIAN_POINT ( 'NONE',  ( 6.566846207931698487, 1.613421326539933531, -1.453093050198107861 ) ) ;
#119751 = FACE_OUTER_BOUND ( 'NONE', #130949, .T. ) ;
#119752 = CARTESIAN_POINT ( 'NONE',  ( 1.288444443960437225, -0.7676182150243222591, -1.973457848717992569 ) ) ;
#119753 = CARTESIAN_POINT ( 'NONE',  ( 3.656250000000002665, -1.895863743164003523, 0.7852924748301777225 ) ) ;
#119754 = CARTESIAN_POINT ( 'NONE',  ( 6.727182134110194944, 2.413774403037728167, 2.569658639860139093 ) ) ;
#119755 = CARTESIAN_POINT ( 'NONE',  ( 5.157218254430565807, -1.627291586725558181, -1.030705938667796140 ) ) ;
#119756 = VERTEX_POINT ( 'NONE', #79970 ) ;
#119758 = CARTESIAN_POINT ( 'NONE',  ( 1.499999999999989120, 5.545833333333350268, -0.8660254037844323793 ) ) ;
#119757 = CARTESIAN_POINT ( 'NONE',  ( 1.523386150502318737, -2.156637510313658801, 0.7774349738483375960 ) ) ;
#119759 = CARTESIAN_POINT ( 'NONE',  ( 4.009460741339333723, 5.700790169694431420, -1.599625672291256295 ) ) ;
#119760 = CARTESIAN_POINT ( 'NONE',  ( 5.412729640353754590, 7.337937218544611895, 1.599625672291267398 ) ) ;
#119761 = CARTESIAN_POINT ( 'NONE',  ( 3.229344874888330441, 2.008827177783510720, 0.9482931344305007837 ) ) ;
#119762 = CARTESIAN_POINT ( 'NONE',  ( -6.860062538834774237, 10.94723069537516302, 0.7216878364870458196 ) ) ;
#119763 = DIRECTION ( 'NONE',  ( -0.8660254037844399289, 0.000000000000000000, -0.4999999999999978351 ) ) ;
#119764 = CARTESIAN_POINT ( 'NONE',  ( 6.182154858151487353, 6.314861544039274577, -0.7216878364870257245 ) ) ;
#119765 = CARTESIAN_POINT ( 'NONE',  ( -6.846504384776750385, 10.93141284897413890, -0.7216878364870267237 ) ) ;
#119766 = CARTESIAN_POINT ( 'NONE',  ( 5.641601317062233001, 7.675230518029648508, -1.443375672974078761 ) ) ;
#119767 = CARTESIAN_POINT ( 'NONE',  ( 2.320935597664942396, 0.9480396085976348086, -1.779626998253575509 ) ) ;
#119769 = CARTESIAN_POINT ( 'NONE',  ( 1.375913251025398409, -2.013209319166248346, 0.4479213407221314669 ) ) ;
#119768 = CARTESIAN_POINT ( 'NONE',  ( 8.938903350111612411, 9.323142084752035430, -0.7998128361456221525 ) ) ;
#119770 = DIRECTION ( 'NONE',  ( 0.000000000000000000, -1.000000000000000000, 0.000000000000000000 ) ) ;
#119771 = CARTESIAN_POINT ( 'NONE',  ( 5.180624093753221970, 9.058162186105164437, 0.000000000000000000 ) ) ;
#119772 = CARTESIAN_POINT ( 'NONE',  ( 6.339394973347380002, 0.6569538336487945607, -1.611921592020611582 ) ) ;
#119773 = CARTESIAN_POINT ( 'NONE',  ( 9.905860218026550257, -6.920331743278818948, 9.269928574751062911E-15 ) ) ;
#119774 = CARTESIAN_POINT ( 'NONE',  ( 0.6823417656249882723, 2.676041667008084879, -1.181850606188749264 ) ) ;
#119775 = CARTESIAN_POINT ( 'NONE',  ( 2.917004591651660927, -0.1773711190117404635, 1.760840049638369154 ) ) ;
#119776 = CARTESIAN_POINT ( 'NONE',  ( 1.301407962653992501, 1.352153127569672098, -1.496052916918483522 ) ) ;
#119777 = CARTESIAN_POINT ( 'NONE',  ( 0.1164230846485321547, -0.09151219166612066525, 1.839079034809627755 ) ) ;
#119778 = CARTESIAN_POINT ( 'NONE',  ( 5.003627799853592073, -2.281530862488420297, 0.2229171871234881530 ) ) ;
#119779 = CARTESIAN_POINT ( 'NONE',  ( 3.064218985076866630, -1.701416833343888824, -0.7040189834505713451 ) ) ;
#119780 = CARTESIAN_POINT ( 'NONE',  ( 8.718056468787178659, 10.12981962079525289, 1.199719254218462483 ) ) ;
#119781 = CARTESIAN_POINT ( 'NONE',  ( 3.627796970749700201, -1.086779551322129445, -1.466705181690882709 ) ) ;
#119782 = CARTESIAN_POINT ( 'NONE',  ( 5.080704010962952211, -0.7231418808758652839, 1.882473355234378865 ) ) ;
#119783 = CARTESIAN_POINT ( 'NONE',  ( -7.669108446824431269, 12.09904362127053545, -0.7998128361456291469 ) ) ;
#119785 = CARTESIAN_POINT ( 'NONE',  ( -7.456058132872594335, 7.663432341298296535, 0.000000000000000000 ) ) ;
#119784 = CARTESIAN_POINT ( 'NONE',  ( 3.415140116862291908, 2.044469143995849780, 0.9693780919050251077 ) ) ;
#119786 = CARTESIAN_POINT ( 'NONE',  ( -0.005051300619423290325, -0.4623140147347043483, -2.061856797492032545 ) ) ;
#119787 = CARTESIAN_POINT ( 'NONE',  ( -0.4169036860910567133, 3.145283463680806246, 0.4342470185719313203 ) ) ;
#119788 = CARTESIAN_POINT ( 'NONE',  ( 3.209495720308676248, -1.691010085789945716, -1.194244797349801157 ) ) ;
#119789 = CARTESIAN_POINT ( 'NONE',  ( 2.517010073631369860, 6.088262185878572375, -0.7998128361456281477 ) ) ;
#119790 = CARTESIAN_POINT ( 'NONE',  ( 1.360316468749971808, 2.567708333674758148, -0.7853790794159301036 ) ) ;
#119791 = CARTESIAN_POINT ( 'NONE',  ( 5.883467998083113493, 0.1561420574479575052, -2.114776682634044391 ) ) ;
#119793 = STYLED_ITEM ( 'NONE', ( #180337 ), #15900 ) ;
#119792 = PRODUCT_CONTEXT ( 'NONE', #119687, 'mechanical' ) ;
#119795 = CARTESIAN_POINT ( 'NONE',  ( 1.945805723040757051, 0.7375614711745586138, -1.779911670397672951 ) ) ;
#119794 = CARTESIAN_POINT ( 'NONE',  ( -8.319899820280397762, 12.85830022363583147, -0.7998128361456281477 ) ) ;
#119796 = CARTESIAN_POINT ( 'NONE',  ( -6.781144757626059061, -7.161464053357560644, 6.776370306708066948 ) ) ;
#119797 = CARTESIAN_POINT ( 'NONE',  ( 6.438338856661699694, -1.056498591242978957, 1.661895973567611540 ) ) ;
#119798 = CARTESIAN_POINT ( 'NONE',  ( 3.838366886000300404, 6.531826229425389485, -1.082531754730548412 ) ) ;
#119799 = CARTESIAN_POINT ( 'NONE',  ( 5.824368567101982030, 6.018301469053008113, 0.4368841385695241275 ) ) ;
#119800 = CARTESIAN_POINT ( 'NONE',  ( -1.500000000000008216, 9.531250000682799595, 3.469446951953614189E-15 ) ) ;
#119801 = CARTESIAN_POINT ( 'NONE',  ( -3.952365473583647315, 4.569846793057691592, 1.199719254218462483 ) ) ;
#119802 = CARTESIAN_POINT ( 'NONE',  ( 0.4400545237335662940, -2.106857831338632359, 0.7043091553551988904 ) ) ;
#119803 = CARTESIAN_POINT ( 'NONE',  ( 3.891714145839750838, 1.523869777361567479, 1.453819373739003051 ) ) ;
#119804 = CARTESIAN_POINT ( 'NONE',  ( -3.709037541790315640, 6.484905011134099340, -1.199719254218450271 ) ) ;
#119805 = CARTESIAN_POINT ( 'NONE',  ( 7.884230021546724920, 9.157022099014721306, 1.199719254218462483 ) ) ;
#119806 = CARTESIAN_POINT ( 'NONE',  ( 0.8009387066525032184, -1.599029608822761128, 0.9519043452789009985 ) ) ;
#119807 = CARTESIAN_POINT ( 'NONE',  ( 5.449487677688982679, 8.445153826357429949, -1.199719254218446718 ) ) ;
#119808 = CARTESIAN_POINT ( 'NONE',  ( 5.281064527722868718, 6.119995689553514140, 1.199719254218462483 ) ) ;
#119809 = CARTESIAN_POINT ( 'NONE',  ( -5.614485009834902840, 9.564333254867113610, 0.7216878364870267237 ) ) ;
#119810 = CARTESIAN_POINT ( 'NONE',  ( -6.561783159334121152, 10.59923808595773664, -0.7216878364870278340 ) ) ;
#119811 = CARTESIAN_POINT ( 'NONE',  ( 1.248456593208754795, 1.040400552670465162, -1.847740296886036582 ) ) ;
#119812 = CARTESIAN_POINT ( 'NONE',  ( -6.400331034103001748, 9.624747418832267698, 1.199719254218452935 ) ) ;
#119814 = CARTESIAN_POINT ( 'NONE',  ( 4.035565188342554954, 1.848088059160474694, -0.6588067414724924076 ) ) ;
#119813 = CARTESIAN_POINT ( 'NONE',  ( -0.6125000000000331291, 0.7916666666666558605, 1.060881119635891157 ) ) ;
#119815 = CARTESIAN_POINT ( 'NONE',  ( 1.920999885407469243, 2.016935458891587096, 0.7782144962657986387 ) ) ;
#119816 = CARTESIAN_POINT ( 'NONE',  ( 1.276629239279066574, 1.701104413791530767, -0.7050613402737049284 ) ) ;
#119818 = CARTESIAN_POINT ( 'NONE',  ( -5.662059632048889846, 6.153064387560178261, -0.8011038117717106388 ) ) ;
#119817 = CARTESIAN_POINT ( 'NONE',  ( -4.659162064951642535, 5.464719159645540003, 1.199719254218452935 ) ) ;
#119819 = EDGE_CURVE ( 'NONE', #142570, #191858, #99563, .T. ) ;
#119820 = CARTESIAN_POINT ( 'NONE',  ( 3.626658729539467441, -1.607292185769314097, 0.6678421186538037180 ) ) ;
#119821 = CARTESIAN_POINT ( 'NONE',  ( 0.7124089920921192753, 16.00000000000000711, -12.66466791154696914 ) ) ;
#119822 = CARTESIAN_POINT ( 'NONE',  ( 4.365362273920230685, 8.036747052974847705, 0.7216878364870298324 ) ) ;
#119823 = CARTESIAN_POINT ( 'NONE',  ( -10.45911201557330195, 5.175391108250987138, -5.201428006079835242 ) ) ;
#119824 = CARTESIAN_POINT ( 'NONE',  ( 0.8487565004985967443, 0.6285140637429244004, 2.068326486519965979 ) ) ;
#119825 =( GEOMETRIC_REPRESENTATION_CONTEXT ( 3 ) GLOBAL_UNCERTAINTY_ASSIGNED_CONTEXT ( ( #191672 ) ) GLOBAL_UNIT_ASSIGNED_CONTEXT ( ( #196303, #178999, #47949 ) ) REPRESENTATION_CONTEXT ( 'NONE', 'WORKASPACE' ) );
#119826 = CARTESIAN_POINT ( 'NONE',  ( 3.708361104356564297, -1.524809962200252444, -1.319026932540816599 ) ) ;
#119827 = CARTESIAN_POINT ( 'NONE',  ( -9.449669878600616357, 12.04770082983265844, -1.443375672974058777 ) ) ;
#119828 = CARTESIAN_POINT ( 'NONE',  ( 0.3741789627117291239, 1.245922373857488274, 1.766349570875298758 ) ) ;
#119829 = CARTESIAN_POINT ( 'NONE',  ( 3.379716691394366368, 1.249474069150168454, 1.524969178572218809 ) ) ;
#119830 = AXIS2_PLACEMENT_3D ( 'NONE', #158585, #43791, #90387 ) ;
#119831 = CARTESIAN_POINT ( 'NONE',  ( -1.416786528094066577, 7.999640415717689912, -11.00953083556809453 ) ) ;
#119832 = CARTESIAN_POINT ( 'NONE',  ( 2.102980028956519476, -0.4233231936755370572, 1.895218400837359818 ) ) ;
#119835 = ORIENTED_EDGE ( 'NONE', *, *, #205156, .T. ) ;
#119834 = CARTESIAN_POINT ( 'NONE',  ( -3.363831509966360489, 6.938570838353784076, -0.7216878364870458196 ) ) ;
#119833 = CARTESIAN_POINT ( 'NONE',  ( 6.486579876843341808, -1.171037552013409089, 1.512559164390047783 ) ) ;
#119836 = CARTESIAN_POINT ( 'NONE',  ( -4.868786560638931782, 6.773613302202437403, 1.443375672974058777 ) ) ;
#119837 = CARTESIAN_POINT ( 'NONE',  ( 4.980641328173811999, 6.904110530993182948, 1.599625672291269396 ) ) ;
#119838 = EDGE_CURVE ( 'NONE', #177712, #63704, #161235, .T. ) ;
#119839 = CARTESIAN_POINT ( 'NONE',  ( -4.145761110728687804, 8.058748072483927771, -0.7998128361456481317 ) ) ;
#119841 = ORIENTED_EDGE ( 'NONE', *, *, #60250, .T. ) ;
#119840 = CARTESIAN_POINT ( 'NONE',  ( -7.279802135894939852, 7.457800344824362604, -0.7998128361456362523 ) ) ;
#119842 = CARTESIAN_POINT ( 'NONE',  ( -7.985389288324685531, 12.26011190311341537, -0.7216878364870267237 ) ) ;
#119843 = CARTESIAN_POINT ( 'NONE',  ( 0.5697015142280477118, 0.2141057807664332180, -2.196374807094509496 ) ) ;
#119844 = CARTESIAN_POINT ( 'NONE',  ( -9.569358774149646862, 4.446947634372958369, 7.167287524840457280 ) ) ;
#119845 = CARTESIAN_POINT ( 'NONE',  ( 4.047668389856577065, 1.417901948909123799, 1.355967163993692992 ) ) ;
#119846 = CARTESIAN_POINT ( 'NONE',  ( 7.259501185113382604, 10.55683625168592243, -1.199719254218441611 ) ) ;
#119847 = CARTESIAN_POINT ( 'NONE',  ( 1.916638904718031000, -1.319229391439219246, -1.525043083973671498 ) ) ;
#119848 = ORIENTED_EDGE ( 'NONE', *, *, #182569, .F. ) ;
#119849 = CARTESIAN_POINT ( 'NONE',  ( 2.044302899665669138, 0.9103292306275132528, 1.911821358334654608 ) ) ;
#119850 = CARTESIAN_POINT ( 'NONE',  ( -0.7500000000000215383, 1.972916667349486453, 1.299038105676659116 ) ) ;
#119852 = CARTESIAN_POINT ( 'NONE',  ( -4.934277840369690971, 7.844075682818238526, -1.199719254218452047 ) ) ;
#119851 = CARTESIAN_POINT ( 'NONE',  ( -10.49201538390856037, 0.9691415390508770766, 5.610609371109086752 ) ) ;
#119853 = CARTESIAN_POINT ( 'NONE',  ( 3.521284115754549582, -1.097709940230184200, -1.477957507169822104 ) ) ;
#119854 = ORIENTED_EDGE ( 'NONE', *, *, #207633, .F. ) ;
#119855 = CARTESIAN_POINT ( 'NONE',  ( -9.332089804907933939, 9.781859615347734405, 1.040834085586084257E-14 ) ) ;
#119856 = SURFACE_SIDE_STYLE ('',( #65673 ) ) ;
#119857 = CARTESIAN_POINT ( 'NONE',  ( 3.515986968957810266, -0.6120941298391362473, 2.030368431519948391 ) ) ;
#119858 = DIRECTION ( 'NONE',  ( -0.9632918427306595976, 0.000000000000000000, -0.2684563758389253985 ) ) ;
#119859 = CARTESIAN_POINT ( 'NONE',  ( 6.693975156845185737, 8.832723654451292816, 1.599625672291281386 ) ) ;
#119860 = CARTESIAN_POINT ( 'NONE',  ( 4.973930670403752252, 1.183205397963146499, 1.687068388967316368 ) ) ;
#119862 = CARTESIAN_POINT ( 'NONE',  ( 2.120424178990498731, 0.001545453418709194504, 1.841430844159386293 ) ) ;
#119861 = CARTESIAN_POINT ( 'NONE',  ( -5.865874016206865882, 9.995270118883347266, 0.000000000000000000 ) ) ;
#119863 = CARTESIAN_POINT ( 'NONE',  ( 7.235247531187115833, 11.59287255302699648, -0.7998128361456291469 ) ) ;
#119864 = FILL_AREA_STYLE_COLOUR ( '', #115447 ) ;
#119865 = DIRECTION ( 'NONE',  ( 0.000000000000000000, -1.000000000000000000, 0.000000000000000000 ) ) ;
#119866 = CARTESIAN_POINT ( 'NONE',  ( 1.737500000000001155, -1.589583332377419334, 3.009438278150922130 ) ) ;
#119867 = AXIS2_PLACEMENT_3D ( 'NONE', #210430, #161714, #144428 ) ;
#119868 = CARTESIAN_POINT ( 'NONE',  ( 2.209865124170300898, -0.4819264253047173541, 2.153463223375853719 ) ) ;
#119869 = CARTESIAN_POINT ( 'NONE',  ( 3.954570948191834745, 0.8096313216635497856, 2.112761250790657908 ) ) ;
#119870 = CARTESIAN_POINT ( 'NONE',  ( -8.514157279702036618, 9.035531035848267223, -0.7216878364870278340 ) ) ;
#119871 = CARTESIAN_POINT ( 'NONE',  ( 4.517698195727691157, -0.4766141805869225645, 1.747713001785702325 ) ) ;
#119872 = CARTESIAN_POINT ( 'NONE',  ( 4.135878506090823414, 1.915180532728939289, -0.05283342432932899152 ) ) ;
#119873 = CARTESIAN_POINT ( 'NONE',  ( 0.6823417656249899377, 4.738541667008086655, -1.181850606188754593 ) ) ;
#119874 = VECTOR ( 'NONE', #6196, 1000.000000000000000 ) ;
#119875 = CARTESIAN_POINT ( 'NONE',  ( 3.573081558413326864, 0.04979752193529430465, -1.971001165494235652 ) ) ;
#119876 = CARTESIAN_POINT ( 'NONE',  ( 0.5516240470409677910, 0.6072917441693607143, -1.828224634575502883 ) ) ;
#119877 = CARTESIAN_POINT ( 'NONE',  ( 4.557402362779487959, 0.4096945884842878582, -1.825068887194372991 ) ) ;
#119878 = CARTESIAN_POINT ( 'NONE',  ( 3.633692980683305152, -2.132556294031516142, 0.8823059210255141949 ) ) ;
#119879 = CARTESIAN_POINT ( 'NONE',  ( 4.756226040108163744, -1.860656195911802646, -0.04637829637440040592 ) ) ;
#119880 = CARTESIAN_POINT ( 'NONE',  ( 1.364683531249990311, 5.113541667008084879, 0.7879004041258500513 ) ) ;
#119881 = DIRECTION ( 'NONE',  ( 1.000000000000000000, 0.000000000000000000, 0.000000000000000000 ) ) ;
#119883 = CARTESIAN_POINT ( 'NONE',  ( 1.699976503534783356, -0.7083771898081425711, 1.983499743616623956 ) ) ;
#119882 = CARTESIAN_POINT ( 'NONE',  ( -4.460269348771590536, 5.266364330730674226, 1.082531754730558626 ) ) ;
#119884 = EDGE_CURVE ( 'NONE', #6089, #30915, #74494, .T. ) ;
#119885 = CARTESIAN_POINT ( 'NONE',  ( 8.062294901620731480, 12.55776115186623620, 1.040834085586084257E-14 ) ) ;
#119887 = LINE ( 'NONE', #99316, #132271 ) ;
#119886 = CARTESIAN_POINT ( 'NONE',  ( -1.201851678989727383E-14, 4.759375000341419693, -1.575800808251660134 ) ) ;
#119888 = CARTESIAN_POINT ( 'NONE',  ( 3.305043459179863419, -0.4174351347619070229, -2.078937965663613774 ) ) ;
#119889 = CARTESIAN_POINT ( 'NONE',  ( -4.994822026498660250, 4.892179926465111350, 0.1397116456474693513 ) ) ;
#119890 = CARTESIAN_POINT ( 'NONE',  ( 0.7209703750307445702, 1.526537956607315172, -1.322641891180293516 ) ) ;
#119891 = CARTESIAN_POINT ( 'NONE',  ( 1.364683531249986537, 1.405208333674755838, -0.7879004041258239610 ) ) ;
#119892 = AXIS2_PLACEMENT_3D ( 'NONE', #51737, #14931, #149223 ) ;
#119893 = CARTESIAN_POINT ( 'NONE',  ( -2.928197990871687306, 5.399686175116803710, 1.082531754730560403 ) ) ;
#119894 = EDGE_CURVE ( 'NONE', #73830, #114534, #81273, .T. ) ;
#119895 = CARTESIAN_POINT ( 'NONE',  ( 4.961394147597008697, 7.875711374583454827, -1.199719254218452047 ) ) ;
#119896 = ORIENTED_EDGE ( 'NONE', *, *, #42077, .F. ) ;
#119897 = CARTESIAN_POINT ( 'NONE',  ( 1.862795570070171713, -1.530026953448139659, 1.527182012981804560 ) ) ;
#119898 = CARTESIAN_POINT ( 'NONE',  ( 5.233084105194869551, 6.167981546557892436, -1.082531754730548412 ) ) ;
#119901 = PLANE ( 'NONE',  #117675 ) ;
#119900 = CARTESIAN_POINT ( 'NONE',  ( 6.825078400183570260, 4.696493799637426747, 2.518305144748238966 ) ) ;
#119899 = CARTESIAN_POINT ( 'NONE',  ( 4.441177836928239309, 7.339068688795062911, 1.199719254218452047 ) ) ;
#119902 = CARTESIAN_POINT ( 'NONE',  ( -11.78331023100045627, 12.29999999999998295, 1.799999999999999600 ) ) ;
#119903 = CARTESIAN_POINT ( 'NONE',  ( 5.753138727196851043, 0.1435251449807967150, -2.011451301405759118 ) ) ;
#119904 = CARTESIAN_POINT ( 'NONE',  ( -8.351459436338037889, 10.76645531385962862, -1.443375672974059665 ) ) ;
#119905 = CARTESIAN_POINT ( 'NONE',  ( 0.2225716830646235489, 2.098996182288978218, 0.6302611576235671587 ) ) ;
#119906 = DIRECTION ( 'NONE',  ( -0.000000000000000000, 1.000000000000000000, -0.000000000000000000 ) ) ;
#119908 = CARTESIAN_POINT ( 'NONE',  ( -1.364683531250010740, 11.38020833367473728, 0.7879004041258445001 ) ) ;
#119907 = CARTESIAN_POINT ( 'NONE',  ( 1.552057811931725428, 0.6552935188219483065, -2.165526471026494537 ) ) ;
#119909 = CARTESIAN_POINT ( 'NONE',  ( -8.402302512167102222, 10.82577223566020841, -1.599625672291263179 ) ) ;
#119910 = CARTESIAN_POINT ( 'NONE',  ( -3.728129053633589152, 7.293308295973741195, 0.7216878364870317197 ) ) ;
#119911 = CARTESIAN_POINT ( 'NONE',  ( 1.364683531249988757, 1.696875000341414808, 0.000000000000000000 ) ) ;
#119912 = CARTESIAN_POINT ( 'NONE',  ( -1.115562610750309283E-14, 9.312500000000001776, 1.500000000000001554 ) ) ;
#119913 = CARTESIAN_POINT ( 'NONE',  ( 1.499999999999997113, 9.645833333333333925, -0.8660254037844378194 ) ) ;
#119914 = CARTESIAN_POINT ( 'NONE',  ( 4.266008093515370803, 0.8158808812368329999, 1.519711535667643609 ) ) ;
#119915 = CARTESIAN_POINT ( 'NONE',  ( 6.201928923608456046, 6.200281597156833691, 0.7998128361456352531 ) ) ;
#119916 = CARTESIAN_POINT ( 'NONE',  ( 1.914973420724352726, -0.2224279105748054597, 1.755648307094020311 ) ) ;
#119917 = CARTESIAN_POINT ( 'NONE',  ( 2.877592485514004039, 0.2932790309252801819, -1.991490711024199944 ) ) ;
#119918 = CARTESIAN_POINT ( 'NONE',  ( 4.805825877545530922, -0.5924843665619135002, 2.125676689404366826 ) ) ;
#119919 = ORIENTED_EDGE ( 'NONE', *, *, #114516, .T. ) ;
#119920 = CARTESIAN_POINT ( 'NONE',  ( 3.867448311701796371, -1.681569574351711838, -1.118542113429069396 ) ) ;
#119921 = CARTESIAN_POINT ( 'NONE',  ( -7.259464905474441565, 7.434073576000447048, -0.7998128361456362523 ) ) ;
#119923 = CARTESIAN_POINT ( 'NONE',  ( 3.691029940746898053, 1.730877988113326493, 1.034147909374658170 ) ) ;
#119922 = CARTESIAN_POINT ( 'NONE',  ( 5.883467998083113493, 0.1561420574479575329, -2.114776682634044391 ) ) ;
#119925 = EDGE_LOOP ( 'NONE', ( #80712, #86307, #129156, #75459, #43259, #107429, #188065 ) ) ;
#119924 = CARTESIAN_POINT ( 'NONE',  ( 4.148556159002002808, 1.777816924242316299, 0.3471830323657533746 ) ) ;
#119926 = ORIENTED_EDGE ( 'NONE', *, *, #199528, .T. ) ;
#119927 = CARTESIAN_POINT ( 'NONE',  ( 1.059204734455133412, 0.3686402435371800568, -1.833797362824276078 ) ) ;
#119928 = DIRECTION ( 'NONE',  ( 0.6507913734559640506, -0.7592566023653004592, 0.000000000000000000 ) ) ;
#119929 = CARTESIAN_POINT ( 'NONE',  ( 5.971335983229998590, -1.557292021941504734, -0.9250951156042800383 ) ) ;
#119930 = CARTESIAN_POINT ( 'NONE',  ( 1.673838217086946587E-16, 4.000000000000003553, 2.500000000000007994 ) ) ;
#119931 = CARTESIAN_POINT ( 'NONE',  ( -9.510997388311002609, 3.006837337344905325, -6.782141846552069531 ) ) ;
#119932 = CARTESIAN_POINT ( 'NONE',  ( 5.858531774436539052, 6.007577623030311287, 0.000000000000000000 ) ) ;
#119933 = CARTESIAN_POINT ( 'NONE',  ( -1.364683531250012516, 2.592708333674753174, 0.7879004041258379498 ) ) ;
#119934 = CARTESIAN_POINT ( 'NONE',  ( 0.2637284958507991606, 0.5978344860198721022, -1.816641584731902626 ) ) ;
#119935 = ORIENTED_EDGE ( 'NONE', *, *, #26279, .F. ) ;
#119936 = CARTESIAN_POINT ( 'NONE',  ( 5.045042558060919724, 8.899983727797476263, -0.7216878364870458196 ) ) ;
#119937 = CARTESIAN_POINT ( 'NONE',  ( 1.943732651021431224, 1.350599318427040840, 1.423195245143428433 ) ) ;
#119938 = PLANE ( 'NONE',  #78773 ) ;
#119939 = CARTESIAN_POINT ( 'NONE',  ( -4.261005416444848315, 8.193199762486115034, 0.7998128361456352531 ) ) ;
#119940 = CARTESIAN_POINT ( 'NONE',  ( 4.078469121099765005, 1.002472831208834680, 1.868716877859360137 ) ) ;
#119941 = CARTESIAN_POINT ( 'NONE',  ( 10.40996301719436090, 11.03937836301526687, 0.000000000000000000 ) ) ;
#119942 = CARTESIAN_POINT ( 'NONE',  ( 5.430923302262330665, 0.1424395525144121211, 1.966244542718327715 ) ) ;
#119943 = CARTESIAN_POINT ( 'NONE',  ( 1.364683531249988535, 1.363541667008083769, 0.7879004041258500513 ) ) ;
#119944 = CARTESIAN_POINT ( 'NONE',  ( 1.265886429849511163, 0.5802531365422005649, -1.927800331509860632 ) ) ;
#119945 = ORIENTED_EDGE ( 'NONE', *, *, #100518, .F. ) ;
#119946 = AXIS2_PLACEMENT_3D ( 'NONE', #192040, #30647, #43703 ) ;
#119947 = CARTESIAN_POINT ( 'NONE',  ( 0.8962975493561256002, -0.9559892387472949116, -1.889204697816506240 ) ) ;
#119948 = CARTESIAN_POINT ( 'NONE',  ( 11.75312296564416847, 6.986206119746739773, -2.433357306325415692 ) ) ;
#119949 = CARTESIAN_POINT ( 'NONE',  ( 2.295452831283749440, -1.850383948470477602, 0.9288054807428181014 ) ) ;
#119950 = CARTESIAN_POINT ( 'NONE',  ( 3.528865121306874464, 7.339036084825155015, -0.7998128361456362523 ) ) ;
#119951 = CARTESIAN_POINT ( 'NONE',  ( 5.037736595929563244, 8.035053907629919223, -1.199719254218452047 ) ) ;
#119952 = ORIENTED_EDGE ( 'NONE', *, *, #18068, .T. ) ;
#119954 = CARTESIAN_POINT ( 'NONE',  ( 5.843727902690005749, 6.776436293681846301, -1.199719254218445830 ) ) ;
#119953 = CARTESIAN_POINT ( 'NONE',  ( 4.382818795122591204, 1.867623683829922054, -0.9396962251831328938 ) ) ;
#119957 = ORIENTED_EDGE ( 'NONE', *, *, #201940, .F. ) ;
#119956 = CARTESIAN_POINT ( 'NONE',  ( 1.840194262915356260, 1.042575051921472040, -1.481162322861505620 ) ) ;
#119955 = CARTESIAN_POINT ( 'NONE',  ( 3.276193339942961913, -1.088440757138483539, 1.465454812695582643 ) ) ;
#119958 = CARTESIAN_POINT ( 'NONE',  ( 6.375609195709820654, 2.113139023092651225, -0.6363509056886568205 ) ) ;
#119959 = DIRECTION ( 'NONE',  ( 1.276756478318932585E-15, -1.000000000000000000, 1.665334536937738262E-16 ) ) ;
#119960 = CARTESIAN_POINT ( 'NONE',  ( 8.486526397101934904, 12.59978548610894578, -8.445610199728610823 ) ) ;
#119961 = CARTESIAN_POINT ( 'NONE',  ( 5.877994779194309238, 1.310017027744770246, 1.775731318763192013 ) ) ;
#119962 = CARTESIAN_POINT ( 'NONE',  ( 8.294891053462476904, 8.571794405328034827, 1.040834085586084257E-14 ) ) ;
#119963 = CARTESIAN_POINT ( 'NONE',  ( 1.364683531249997417, 9.296875000341403350, 2.602085213965210642E-15 ) ) ;
#119964 = ORIENTED_EDGE ( 'NONE', *, *, #3232, .T. ) ;
#119965 = CARTESIAN_POINT ( 'NONE',  ( 3.563058999304801411, -1.561743426874351970, 1.103242700682869781 ) ) ;
#119966 = CARTESIAN_POINT ( 'NONE',  ( -4.243865776277440993, 4.909930479533815451, -1.199719254218446718 ) ) ;
#119967 = CARTESIAN_POINT ( 'NONE',  ( 6.936968151686458306, 11.24487994360957188, 0.7998128361456462443 ) ) ;
#119968 = CARTESIAN_POINT ( 'NONE',  ( 6.285608408418759119, -1.950803066209889636, 0.6937918898708081983 ) ) ;
#119969 = CARTESIAN_POINT ( 'NONE',  ( -9.333041836230016486, 15.44694763438214125, 7.472413793098208856 ) ) ;
#119970 = CARTESIAN_POINT ( 'NONE',  ( 6.497619750234602698, -2.191128968173004843, 0.05151875470104508997 ) ) ;
#119971 = CARTESIAN_POINT ( 'NONE',  ( 5.845834525830363226, 7.300097092180095615, -1.274846751706928849 ) ) ;
#119972 = CARTESIAN_POINT ( 'NONE',  ( -1.797499070710327107, 15.51994604999343608, -11.89808504883940543 ) ) ;
#119973 = ORIENTED_EDGE ( 'NONE', *, *, #117255, .F. ) ;
#119974 = CARTESIAN_POINT ( 'NONE',  ( 1.464175926609780964E-14, -2.187499999999999112, -3.475000000000000533 ) ) ;
#119975 = CARTESIAN_POINT ( 'NONE',  ( 3.567518508692040236, 1.825626599287116791, -0.4067673385957787380 ) ) ;
#119976 = CARTESIAN_POINT ( 'NONE',  ( -0.02319159430947542733, 0.7471999394491578572, -1.895068635927643630 ) ) ;
#119977 = AXIS2_PLACEMENT_3D ( 'NONE', #25951, #89921, #107280 ) ;
#119978 = ADVANCED_FACE ( 'NONE', ( #95186 ), #95197, .T. ) ;
#119979 = CARTESIAN_POINT ( 'NONE',  ( -9.367496997601300279, 15.00000000000599165, 7.679999999987998649 ) ) ;
#119980 = CARTESIAN_POINT ( 'NONE',  ( -8.026063749610056419, 10.38682701267698150, -1.443375672974059665 ) ) ;
#119982 = CARTESIAN_POINT ( 'NONE',  ( 3.074666975249065626, 6.809138247757705820, 0.000000000000000000 ) ) ;
#119981 = AXIS2_PLACEMENT_3D ( 'NONE', #68187, #136433, #117032 ) ;
#119983 = CARTESIAN_POINT ( 'NONE',  ( 6.561392567526037389, 1.717850402480676664, 1.155108059606273052 ) ) ;
#119984 = CARTESIAN_POINT ( 'NONE',  ( 1.476185646619165626, -2.006963189339417308, -0.1948195631672477446 ) ) ;
#119985 = CARTESIAN_POINT ( 'NONE',  ( -8.839026081105473054, 12.39961529701003684, -1.199719254218446718 ) ) ;
#119986 = CARTESIAN_POINT ( 'NONE',  ( 6.017840079619279692, 8.114175741012878973, -1.599625672291281386 ) ) ;
#119987 = LINE ( 'NONE', #19197, #87450 ) ;
#119988 = CARTESIAN_POINT ( 'NONE',  ( 1.148660753082946240, -1.725648174752218100, 1.350667304935410318 ) ) ;
#119989 = CARTESIAN_POINT ( 'NONE',  ( 6.358013415952256331, 1.820405254634300363, -0.1396899356524081148 ) ) ;
#119990 = CARTESIAN_POINT ( 'NONE',  ( -2.788173145904702555, 6.404619103530779789, -0.7998128361456281477 ) ) ;
#119991 = CARTESIAN_POINT ( 'NONE',  ( 5.451787166470912993, 6.493411461371761284, -1.082531754730548412 ) ) ;
#119992 = CARTESIAN_POINT ( 'NONE',  ( 9.103410076571945453, 12.70806329172093818, 1.199719254218450271 ) ) ;
#119993 = CARTESIAN_POINT ( 'NONE',  ( 3.460355519985863548, 5.060167411448709629, 1.599625672291267398 ) ) ;
#119994 = CARTESIAN_POINT ( 'NONE',  ( 2.878073747850912412, 6.579779482459851003, -0.7998128361456362523 ) ) ;
#119995 = ORIENTED_EDGE ( 'NONE', *, *, #209914, .T. ) ;
#119997 = CARTESIAN_POINT ( 'NONE',  ( 0.5221354380547962304, -2.003184638039813503, 0.1996226354380666868 ) ) ;
#119996 = CARTESIAN_POINT ( 'NONE',  ( 4.335397732480402055, 0.7831895168094182846, -1.666506522714307437 ) ) ;
#119998 = CARTESIAN_POINT ( 'NONE',  ( 2.073957380999270850, 1.703569143382680506, -1.543048383257297207 ) ) ;
#120000 = CARTESIAN_POINT ( 'NONE',  ( 6.157081138237819218, 1.605775322519078729, -1.126676614267435150 ) ) ;
#119999 = CARTESIAN_POINT ( 'NONE',  ( 3.551873057100283226, 6.127307085716883428, 1.082531754730558626 ) ) ;
#120001 = CARTESIAN_POINT ( 'NONE',  ( 3.285556943750000514, -3.463541666188707957, 1.896917185911906500 ) ) ;
#120002 = CARTESIAN_POINT ( 'NONE',  ( -5.037017762676898158, 5.835274463666530131, -1.199719254218446718 ) ) ;
#120003 = FILL_AREA_STYLE ('',( #69019 ) ) ;
#120004 = CARTESIAN_POINT ( 'NONE',  ( 4.886922752366290368, -1.802716094696995786, -0.6387714794457154399 ) ) ;
#120005 = CARTESIAN_POINT ( 'NONE',  ( -7.784352752540590004, 12.23349531127272094, 0.7998128361456481317 ) ) ;
#120006 = CARTESIAN_POINT ( 'NONE',  ( 6.484283628081795037, 6.752753718119230975, 0.1579380340677779548 ) ) ;
#120007 = CARTESIAN_POINT ( 'NONE',  ( -5.157951095356222204, 4.982307464195829816, 0.000000000000000000 ) ) ;
#120009 = CARTESIAN_POINT ( 'NONE',  ( 2.571000202304725590, 0.09389976206976291540, -1.868427151830873267 ) ) ;
#120008 = CARTESIAN_POINT ( 'NONE',  ( 2.788710525494293879, 1.791885054564039903, -1.076980376859866029 ) ) ;
#120010 = CARTESIAN_POINT ( 'NONE',  ( 7.565086526745395723, 10.80938946696957004, -1.082531754730543083 ) ) ;
#120011 = CARTESIAN_POINT ( 'NONE',  ( -6.506745451169519079, -8.202869699938538872, -6.922231005658564307 ) ) ;
#120012 = CARTESIAN_POINT ( 'NONE',  ( 3.210250486799534286, 1.574880741971116827, 0.7411356085459307463 ) ) ;
#120013 = CARTESIAN_POINT ( 'NONE',  ( 5.847644326195776010, 5.716673223516856694, -0.7998128361456281477 ) ) ;
#120015 = CARTESIAN_POINT ( 'NONE',  ( 11.88237951145550220, 13.75680652621284317, -0.9087114598430711121 ) ) ;
#120014 = CARTESIAN_POINT ( 'NONE',  ( -0.7500000000000179856, 11.57291666734946212, 1.299038105676658228 ) ) ;
#120016 = CARTESIAN_POINT ( 'NONE',  ( 4.389066697632080682, 1.539216480442310075, -0.7786167122535156970 ) ) ;
#120017 = CARTESIAN_POINT ( 'NONE',  ( 4.071962858106247474, -1.261020321617589479, 1.792237525612811355 ) ) ;
#120018 = CARTESIAN_POINT ( 'NONE',  ( 6.164705905600972535, -1.563586322211576674, 1.557672334054376773 ) ) ;
#120019 = CARTESIAN_POINT ( 'NONE',  ( -10.43233925736708301, 5.066585305077033752, -5.254699789447807134 ) ) ;
#120020 = AXIS2_PLACEMENT_3D ( 'NONE', #105818, #204306, #73255 ) ;
#120021 = CARTESIAN_POINT ( 'NONE',  ( 3.081114545232612301, 2.042771114613873173, 0.7355539269583191153 ) ) ;
#120022 = CARTESIAN_POINT ( 'NONE',  ( 1.752308680507021155, 0.5713779359179693706, 1.734036872924920702 ) ) ;
#120023 = LINE ( 'NONE', #37633, #117889 ) ;
#120024 = CARTESIAN_POINT ( 'NONE',  ( 4.223895228407223534, 0.9020499113536835090, -1.915681561053275139 ) ) ;
#120025 = EDGE_LOOP ( 'NONE', ( #87913, #2329, #77704, #125909 ) ) ;
#120027 = CARTESIAN_POINT ( 'NONE',  ( 0.6823417656249882723, 2.488541667008084435, -1.181850606188749264 ) ) ;
#120026 = CARTESIAN_POINT ( 'NONE',  ( 5.109026413134919231, -0.3384823820529453964, 2.267118282965301379 ) ) ;
#120028 = CARTESIAN_POINT ( 'NONE',  ( 6.620655732516656400, 2.994310854299454316, 2.180639477081049993 ) ) ;
#120029 = CARTESIAN_POINT ( 'NONE',  ( 4.403700966340357681, 4.032072637018845107, -0.7998128361456211532 ) ) ;
#120030 = AXIS2_PLACEMENT_3D ( 'NONE', #171988, #3047, #136295 ) ;
#120031 = CARTESIAN_POINT ( 'NONE',  ( 0.6277789859737945566, -0.3070864893036719945, 2.098006834332386994 ) ) ;
#120032 = CARTESIAN_POINT ( 'NONE',  ( -6.073689629242176480, 6.188318776978391611, -0.7216878364870278340 ) ) ;
#120033 = ADVANCED_FACE ( 'NONE', ( #136213 ), #53584, .T. ) ;
#120034 = CARTESIAN_POINT ( 'NONE',  ( -11.86145016429273191, 19.00000000000000000, 1.179999999999997051 ) ) ;
#120035 = CARTESIAN_POINT ( 'NONE',  ( -5.544921637864833386, 7.492161215640853023, -1.443375672974051449 ) ) ;
#120037 = CARTESIAN_POINT ( 'NONE',  ( -0.7500000000000179856, 11.82291666734946389, 1.299038105676658228 ) ) ;
#120036 = DIRECTION ( 'NONE',  ( 0.7806247498251047690, 0.000000000000000000, 0.6249999999683939489 ) ) ;
#120038 = EDGE_LOOP ( 'NONE', ( #9853, #213762, #11630, #69396, #103030, #131280 ) ) ;
#120039 = CARTESIAN_POINT ( 'NONE',  ( 5.168592345394213972, 1.356298078840772803, 1.492257005506092193 ) ) ;
#120041 = CARTESIAN_POINT ( 'NONE',  ( 4.205966187000295342, 0.6995128471476423915, -1.940432845919232374 ) ) ;
#120040 = CARTESIAN_POINT ( 'NONE',  ( 4.852928918687680948, 7.749168607522574526, 1.199719254218462483 ) ) ;
#120043 = CARTESIAN_POINT ( 'NONE',  ( -0.1411974294642332484, 2.879603353482541817, -2.388950311486548461 ) ) ;
#120042 = CARTESIAN_POINT ( 'NONE',  ( 7.191674137406095291, 7.354984346587396082, 0.000000000000000000 ) ) ;
#120044 = CARTESIAN_POINT ( 'NONE',  ( 7.309781096423290769, 8.557108029695882578, 1.199719254218452935 ) ) ;
#120045 = CARTESIAN_POINT ( 'NONE',  ( -3.285556943750000514, -1.188541666188710044, -1.896917185911906500 ) ) ;
#120046 = DIRECTION ( 'NONE',  ( 0.000000000000000000, 0.000000000000000000, -1.000000000000000000 ) ) ;
#120047 = CARTESIAN_POINT ( 'NONE',  ( 0.3750906047784249853, 1.949931092985623726, -0.7544815049443721611 ) ) ;
#120048 = CARTESIAN_POINT ( 'NONE',  ( 4.360000113718985659, -0.002809843368253156070, -2.016597020062675050 ) ) ;
#120049 = CARTESIAN_POINT ( 'NONE',  ( 3.456447201099471123, -1.625387274077850996, -0.8650149607793489182 ) ) ;
#120050 = AXIS2_PLACEMENT_3D ( 'NONE', #76290, #145611, #44889 ) ;
#120051 = CARTESIAN_POINT ( 'NONE',  ( 5.331380718671758778, 7.243030143248949670, -1.599625672291256295 ) ) ;
#120052 = SURFACE_SIDE_STYLE ('',( #117911 ) ) ;
#120053 = CARTESIAN_POINT ( 'NONE',  ( 0.6391468373067762387, -1.214715217071378195, -1.224744053251116904 ) ) ;
#120054 = CARTESIAN_POINT ( 'NONE',  ( -2.266184231778562541, 5.795632037050281404, 1.040834085586084257E-14 ) ) ;
#120055 = CARTESIAN_POINT ( 'NONE',  ( 0.6690544563107813092, 1.549219078230345215, 1.698357357312555660 ) ) ;
#120056 = CARTESIAN_POINT ( 'NONE',  ( -6.684333426737305572, 7.757142738403693727, -1.199719254218446718 ) ) ;
#120057 = CARTESIAN_POINT ( 'NONE',  ( 6.438354578037611908, 2.236760482230481184, 0.3397759937929164531 ) ) ;
#120058 = CARTESIAN_POINT ( 'NONE',  ( 3.387430394310109616, 1.903944824823229798, -0.9005924351132842398 ) ) ;
#120059 = CARTESIAN_POINT ( 'NONE',  ( -5.957882158562513908, 5.915560371269843465, -0.7998128361456362523 ) ) ;
#120060 = CARTESIAN_POINT ( 'NONE',  ( 6.775324078527185989, 8.927630729746953264, -1.599625672291262513 ) ) ;
#120061 = CARTESIAN_POINT ( 'NONE',  ( 5.194182247366861738, 9.073980031987776584, 0.7216878364870317197 ) ) ;
#120062 = CARTESIAN_POINT ( 'NONE',  ( 6.125000000000003553, -2.052068128417929849, 3.487440458529189440E-13 ) ) ;
#120063 = CARTESIAN_POINT ( 'NONE',  ( -5.703176172842872482, 9.805455968292021041, 0.000000000000000000 ) ) ;
#120064 = CARTESIAN_POINT ( 'NONE',  ( 6.819388077549422889, 8.018669514304889390, -1.082531754730543971 ) ) ;
#120065 = CARTESIAN_POINT ( 'NONE',  ( 4.441740843186996912, 7.307116142998927977, 1.228109861675081849 ) ) ;
#120066 = CARTESIAN_POINT ( 'NONE',  ( -5.108724954250998707, 4.854600622914589714, -0.7998128361456221525 ) ) ;
#120068 = CARTESIAN_POINT ( 'NONE',  ( 3.568779976319371272, 0.8023129380761647722, 2.071619486725768677 ) ) ;
#120067 = CARTESIAN_POINT ( 'NONE',  ( 2.478903650112133317, -1.459102030866548994, 1.539066919819010781 ) ) ;
#120069 = CARTESIAN_POINT ( 'NONE',  ( 2.519692321801832335, -1.262790281060278907, -1.790845962237663791 ) ) ;
#120070 = CARTESIAN_POINT ( 'NONE',  ( -4.954615070790188369, 7.867802451642154082, -1.199719254218452047 ) ) ;
#120071 = CARTESIAN_POINT ( 'NONE',  ( -4.659162064951642535, 5.464719159645540003, 1.199719254218452935 ) ) ;
#120072 = CARTESIAN_POINT ( 'NONE',  ( 5.846142468697441252, -0.8834969228576605715, 1.751761657833034613 ) ) ;
#120073 = CARTESIAN_POINT ( 'NONE',  ( 0.6823417656249899377, 1.842708333674752952, 1.181850606188755259 ) ) ;
#120074 = CARTESIAN_POINT ( 'NONE',  ( -4.177320726786328819, 5.966903162707725805, -1.443375672974066548 ) ) ;
#120076 = VERTEX_POINT ( 'NONE', #103709 ) ;
#120075 = CARTESIAN_POINT ( 'NONE',  ( -5.422898255786198440, 7.349800603215774331, -1.443375672974052559 ) ) ;
#120077 = CARTESIAN_POINT ( 'NONE',  ( 5.133110336712339183, 1.960249873928998410, 0.8093987030339530042 ) ) ;
#120078 = CARTESIAN_POINT ( 'NONE',  ( -3.984117037569407938, 5.741498858621315371, 1.599625672291270506 ) ) ;
#120079 = ORIENTED_EDGE ( 'NONE', *, *, #78821, .T. ) ;
#120081 = CARTESIAN_POINT ( 'NONE',  ( 6.473507614529132148, 2.070149491355821159, -0.6224772505839873959 ) ) ;
#120080 = CARTESIAN_POINT ( 'NONE',  ( -5.153507786970267013, 8.066157280557016307, -1.082531754730549967 ) ) ;
#120082 = CARTESIAN_POINT ( 'NONE',  ( 7.332262146892202459, 7.448727347662698506, -0.7998128361456281477 ) ) ;
#120083 = CARTESIAN_POINT ( 'NONE',  ( 5.179192671508887180, 1.240781939916297372, 1.360553736468192554 ) ) ;
#120084 = UNCERTAINTY_MEASURE_WITH_UNIT (LENGTH_MEASURE( 1.000000000000000082E-05 ), #114427, 'distance_accuracy_value', 'NONE');
#120085 = DIRECTION ( 'NONE',  ( -0.000000000000000000, -1.000000000000000000, -0.000000000000000000 ) ) ;
#120086 = CARTESIAN_POINT ( 'NONE',  ( -1.364683531250012516, 3.092708333674755838, 0.7879004041258379498 ) ) ;
#120087 = CARTESIAN_POINT ( 'NONE',  ( 1.258879523317941285, 1.714807473692409268, -0.2965960235774521836 ) ) ;
#120088 = CARTESIAN_POINT ( 'NONE',  ( 11.52901446936747298, 12.30574472532411434, 3.330874149801136053 ) ) ;
#120089 = CARTESIAN_POINT ( 'NONE',  ( 0.3999999999999758193, 3.000000000000047518, 2.023857702507768419 ) ) ;
#120090 = LINE ( 'NONE', #152514, #46054 ) ;
#120091 = CARTESIAN_POINT ( 'NONE',  ( 4.926735330553584369, 2.067573386176469796, 0.6309256262674377558 ) ) ;
#120092 = CARTESIAN_POINT ( 'NONE',  ( -3.978428010606240850, 6.728917548094202949, -1.199719254218452047 ) ) ;
#120093 = CARTESIAN_POINT ( 'NONE',  ( -7.415946836550729948, 9.675023947441092176, 1.443375672974090751 ) ) ;
#120094 = CARTESIAN_POINT ( 'NONE',  ( 5.155217493315787713, -1.824165352752779246, -1.159627250419709155 ) ) ;
#120095 = CARTESIAN_POINT ( 'NONE',  ( 4.780523264075623224, -1.911459794658072697, -0.4817293046612564633 ) ) ;
#120096 = CARTESIAN_POINT ( 'NONE',  ( 4.217908468276907463, -1.441162302510163640, -0.9635822893686758484 ) ) ;
#120097 = CARTESIAN_POINT ( 'NONE',  ( 0.7498831369015904746, 2.188782640433343474, -0.1130235578899463078 ) ) ;
#120098 = CARTESIAN_POINT ( 'NONE',  ( 1.835461723582560767, 0.2275736305563350881, 2.296322244814374081 ) ) ;
#120099 = CARTESIAN_POINT ( 'NONE',  ( 3.725900457647839392, -1.224662966953151688, -1.657274842633131851 ) ) ;
#120100 = CARTESIAN_POINT ( 'NONE',  ( 6.233930015136599501, 1.921560620327814606, 0.2806146417165931717 ) ) ;
#120101 = CARTESIAN_POINT ( 'NONE',  ( -8.975134502122321223, 9.573337795338607847, 1.040834085586084257E-14 ) ) ;
#120102 = CARTESIAN_POINT ( 'NONE',  ( -4.522526758610270647, 7.433975764090723359, -1.199719254218453823 ) ) ;
#120103 = DIRECTION ( 'NONE',  ( -5.551115123125765446E-17, 0.000000000000000000, 1.000000000000000000 ) ) ;
#120104 = ADVANCED_FACE ( 'NONE', ( #183871 ), #122955, .T. ) ;
#120105 = CARTESIAN_POINT ( 'NONE',  ( -3.654804927335652209, 6.421633627603656080, 1.199719254218452935 ) ) ;
#120106 = CARTESIAN_POINT ( 'NONE',  ( -5.843201017365469596, 9.760892253660966134, 0.7216878364870458196 ) ) ;
#120107 = CARTESIAN_POINT ( 'NONE',  ( 3.171135245091468491, -2.038329301889611589, -0.8460836234857532778 ) ) ;
#120108 = CARTESIAN_POINT ( 'NONE',  ( -3.285556943750000070, -2.646874999522041971, 0.000000000000000000 ) ) ;
#120109 = VERTEX_POINT ( 'NONE', #199028 ) ;
#120110 = CARTESIAN_POINT ( 'NONE',  ( 6.977413161700751765, -0.1449424838519241254, 1.929857014940839832 ) ) ;
#120111 =( BOUNDED_CURVE ( )  B_SPLINE_CURVE ( 2, ( #2201, #169000, #4334 ),
 .UNSPECIFIED., .F., .T. ) 
 B_SPLINE_CURVE_WITH_KNOTS ( ( 3, 3 ),
 ( 0.000000000000000000, 0.0002183499308599263643 ),
 .UNSPECIFIED. ) 
 CURVE ( )  GEOMETRIC_REPRESENTATION_ITEM ( )  RATIONAL_B_SPLINE_CURVE ( ( 1.000000000000000000, 0.9929791974830429746, 0.9866942310032822405 ) ) 
 REPRESENTATION_ITEM ( '' )  );
#120112 = CARTESIAN_POINT ( 'NONE',  ( 1.378728738066221871, 4.086408449757453099, -0.5908528300941785494 ) ) ;
#120114 = CARTESIAN_POINT ( 'NONE',  ( 6.825078400183510752, 2.433016701115862102, 2.426111979085682879 ) ) ;
#120113 = CARTESIAN_POINT ( 'NONE',  ( -6.555587544261016753, 6.796970737185429989, -0.4399619850315484859 ) ) ;
#120115 = DIRECTION ( 'NONE',  ( 1.000000000000000000, 0.000000000000000000, -0.000000000000000000 ) ) ;
#120116 = ORIENTED_EDGE ( 'NONE', *, *, #208162, .F. ) ;
#120117 = CARTESIAN_POINT ( 'NONE',  ( 2.905207415116388248, 1.740275362031361794, 1.103647167516639938 ) ) ;
#120118 = CARTESIAN_POINT ( 'NONE',  ( -1.360316468750008667, 0.1197916670080665519, -0.7853790794159001276 ) ) ;
#120120 = B_SPLINE_CURVE_WITH_KNOTS ( 'NONE', 3,
 ( #184379, #37067, #101000, #168147, #151906, #20800, #152963, #54403 ),
 .UNSPECIFIED., .F., .F.,
 ( 4, 2, 2, 4 ),
 ( 6.054694391546165775E-16, 0.0001985720215092564753, 0.0003971440430179074780, 0.0007942880860352082364 ),
 .UNSPECIFIED. ) ;
#120119 = UNCERTAINTY_MEASURE_WITH_UNIT (LENGTH_MEASURE( 1.000000000000000082E-05 ), #30165, 'distance_accuracy_value', 'NONE');
#120121 = CARTESIAN_POINT ( 'NONE',  ( -5.880485940025243607, 7.883652901494672349, 1.599625672291269396 ) ) ;
#120122 = DIRECTION ( 'NONE',  ( 1.000000000000000000, 0.000000000000000000, 0.000000000000000000 ) ) ;
#120123 = DIRECTION ( 'NONE',  ( 0.000000000000000000, 0.000000000000000000, -1.000000000000000000 ) ) ;
#120124 = CARTESIAN_POINT ( 'NONE',  ( 5.169736645512481132, 4.925780929386339935, 0.7998128361456341429 ) ) ;
#120125 = CARTESIAN_POINT ( 'NONE',  ( 2.043891306636512528, 0.7897949731258145922, -1.903750762553678921 ) ) ;
#120126 =( BOUNDED_SURFACE ( )  B_SPLINE_SURFACE ( 3, 2, ( 
 ( #89246, #155297, #139060 ),
 ( #205088, #162779, #110878 ),
 ( #65237, #43701, #80447 ),
 ( #45834, #114095, #93518 ) ),
 .UNSPECIFIED., .F., .F., .F. ) 
 B_SPLINE_SURFACE_WITH_KNOTS ( ( 4, 4 ),
 ( 3, 3 ),
 ( 0.000000000000000000, 9.170893476602526924E-05 ),
 ( 0.000000000000000000, 1.000000000000000000 ),
 .UNSPECIFIED. ) 
 GEOMETRIC_REPRESENTATION_ITEM ( )  RATIONAL_B_SPLINE_SURFACE ( (
 ( 1.000000000000000000, 0.7100530722026773267, 1.000000000000000000),
 ( 1.000000000000000000, 0.6998898451682588062, 1.000000000000000000),
 ( 1.000000000000000000, 0.6894756946157454269, 1.000000000000000000),
 ( 1.000000000000000000, 0.6787756258918318242, 1.000000000000000000) ) ) 
 REPRESENTATION_ITEM ( '' )  SURFACE ( )  );
#120127 = EDGE_CURVE ( 'NONE', #166004, #12101, #84366, .T. ) ;
#120129 = CARTESIAN_POINT ( 'NONE',  ( -1.402160292154681736E-14, 13.92187500034139624, 1.575800808251682339 ) ) ;
#120128 = FACE_OUTER_BOUND ( 'NONE', #45657, .T. ) ;
#120130 = CARTESIAN_POINT ( 'NONE',  ( 6.307567778855705853, 8.381915046796901692, -1.599625672291262513 ) ) ;
#120131 = CARTESIAN_POINT ( 'NONE',  ( 5.865903189996044098, 2.174886565178067777, -0.3735607071253948530 ) ) ;
#120132 = CARTESIAN_POINT ( 'NONE',  ( 0.6675187767142229944, 0.2125181155594977611, -2.151144519195991922 ) ) ;
#120133 = CARTESIAN_POINT ( 'NONE',  ( -4.609409038966234995, 7.361099064560491456, -1.082531754730549967 ) ) ;
#120134 = CARTESIAN_POINT ( 'NONE',  ( 0.6906390985809904848, 1.523792322931913468, -1.320830384837400118 ) ) ;
#120135 = CARTESIAN_POINT ( 'NONE',  ( 1.617049182541079544, 0.6662764605713987764, -2.199669867806148371 ) ) ;
#120136 = CARTESIAN_POINT ( 'NONE',  ( 1.813763795902412879, 3.950000000000016165, 0.3999999999999576672 ) ) ;
#120137 = CARTESIAN_POINT ( 'NONE',  ( -3.782361668532609134, 7.356579680022602652, 1.040834085586084257E-14 ) ) ;
#120138 = DIRECTION ( 'NONE',  ( 1.016547956922408957E-15, 1.000000000000000000, -4.622230424712075819E-32 ) ) ;
#120139 = CARTESIAN_POINT ( 'NONE',  ( 1.533845512228737551, 0.9248708299973290581, -1.625957014461040906 ) ) ;
#120140 = CARTESIAN_POINT ( 'NONE',  ( 3.626185617424378282, 2.007256095728218614, 0.1928357053486499662 ) ) ;
#120142 = CARTESIAN_POINT ( 'NONE',  ( 6.639320575229255894, 6.035237531390704291, 2.698156163645454964 ) ) ;
#120141 = CARTESIAN_POINT ( 'NONE',  ( 0.6823417656249899377, 1.092708333674752286, 1.181850606188755259 ) ) ;
#120144 = CARTESIAN_POINT ( 'NONE',  ( 4.582709122986449835, -2.042650070554121733, -0.5124292222106421324 ) ) ;
#120143 = CARTESIAN_POINT ( 'NONE',  ( -6.015013705957189316, 10.16926642359206134, 0.7998128361456481317 ) ) ;
#120145 = EDGE_CURVE ( 'NONE', #151085, #39437, #53600, .T. ) ;
#120146 = CARTESIAN_POINT ( 'NONE',  ( 5.459129407796876166, 9.520734742405036144, 1.040834085586084257E-14 ) ) ;
#120148 = CARTESIAN_POINT ( 'NONE',  ( -8.199983978166823562, 8.461069484149769337, -0.7998128361456291469 ) ) ;
#120147 = CARTESIAN_POINT ( 'NONE',  ( 4.115782150200256950, 6.959440387612411349, 1.199719254218452047 ) ) ;
#120149 = CARTESIAN_POINT ( 'NONE',  ( 4.098537063712264228, 7.253343185014818673, 1.055677455976588686 ) ) ;
#120150 = CARTESIAN_POINT ( 'NONE',  ( 4.570572472720978219, 0.7768735290680817140, 1.864611197846306911 ) ) ;
#120151 = CARTESIAN_POINT ( 'NONE',  ( 0.7499999999999885647, -0.7354166659838470288, 1.299038105676657340 ) ) ;
#120152 = EDGE_CURVE ( 'NONE', #44633, #195163, #84819, .T. ) ;
#120153 = CARTESIAN_POINT ( 'NONE',  ( 0.3036763228623740041, -1.592034637876770908, -1.310935287704196206 ) ) ;
#120154 = CARTESIAN_POINT ( 'NONE',  ( 8.432808358020016826, 10.86136238915529084, 1.443375672974076540 ) ) ;
#120155 = CARTESIAN_POINT ( 'NONE',  ( 6.081358973892867503, 1.999796440023202448, -0.8210498935554910727 ) ) ;
#120156 = CARTESIAN_POINT ( 'NONE',  ( 5.363132282657546490, 8.414682208812571673, -1.199719254218452047 ) ) ;
#120157 = CARTESIAN_POINT ( 'NONE',  ( -1.364683531250014514, -0.4489583329919089039, -0.7879004041258359514 ) ) ;
#120159 = CARTESIAN_POINT ( 'NONE',  ( -0.1106856583841061281, -0.002128758811529350356, -1.996853503091333693 ) ) ;
#120158 = CARTESIAN_POINT ( 'NONE',  ( 5.123001941117305336, 7.070197912760590064, 1.599625672291268286 ) ) ;
#120160 = CARTESIAN_POINT ( 'NONE',  ( 6.710922848640084482, 9.812865175846695820, -1.082531754730537976 ) ) ;
#120161 = CARTESIAN_POINT ( 'NONE',  ( 2.682273331476907607, -1.248350377418592672, -1.776241996044833238 ) ) ;
#120163 = CARTESIAN_POINT ( 'NONE',  ( 2.243484787601189634, 1.840893492186860492, 0.04347913094143729396 ) ) ;
#120162 = CARTESIAN_POINT ( 'NONE',  ( -4.284013352238250860, 7.941839977679187257, -0.7216878364870267237 ) ) ;
#120164 = CARTESIAN_POINT ( 'NONE',  ( -1.201851678989727383E-14, 3.696875000341422801, -1.575800808251660134 ) ) ;
#120165 = CARTESIAN_POINT ( 'NONE',  ( 3.667680160636753506, 1.218766932906123479, 1.821211977396507198 ) ) ;
#120166 = DIRECTION ( 'NONE',  ( -3.330669073875479482E-16, 3.330669073875479482E-16, 1.000000000000000000 ) ) ;
#120167 = CARTESIAN_POINT ( 'NONE',  ( 5.120128864776952504, -1.205885850527373293, -1.914207236704228654 ) ) ;
#120168 = CARTESIAN_POINT ( 'NONE',  ( -5.585069213825653023, 8.603332285183535433, -1.199719254218440723 ) ) ;
#120169 = CARTESIAN_POINT ( 'NONE',  ( -1.872228381520320672, 3.299999999999962519, 0.3999999999999628852 ) ) ;
#120170 = CARTESIAN_POINT ( 'NONE',  ( 6.435429789636040177, 6.784273175954743884, -0.4071148367965071735 ) ) ;
#120171 = CARTESIAN_POINT ( 'NONE',  ( -1.500000000000001110, 13.27083333333333748, 0.8660254037844419273 ) ) ;
#120172 = CARTESIAN_POINT ( 'NONE',  ( -4.936577328707246082, 8.773440960218172435, 0.000000000000000000 ) ) ;
#120173 = CARTESIAN_POINT ( 'NONE',  ( 5.397554552016212703, 8.350878506444006533, 1.082531754730547524 ) ) ;
#120174 = CARTESIAN_POINT ( 'NONE',  ( 4.903428802837151324, -0.4723676116331463892, 1.705421244663980263 ) ) ;
#120175 = AXIS2_PLACEMENT_3D ( 'NONE', #140455, #89179, #57729 ) ;
#120176 =( BOUNDED_SURFACE ( )  B_SPLINE_SURFACE ( 3, 3, ( 
 ( #100584, #183961, #52898, #86471, #152536, #17178, #4121, #66985, #34511, #70190 ),
 ( #136302, #169849, #53974, #186090, #37721, #103799, #49701, #134186, #182895, #166658 ),
 ( #18248, #35572, #101652, #88621, #73408, #39865, #139511, #58240, #90761, #124396 ),
 ( #72332, #156822, #141668, #138438, #105974, #154676, #87544, #71260, #155746, #6261 ),
 ( #137374, #109199, #171996, #104872, #107047, #204456, #56110, #23588, #153613, #74495 ),
 ( #122268, #55043, #205538, #188225, #89696, #190354, #7331, #38790, #25725, #57175 ),
 ( #203390, #121192, #123337, #207679, #157893, #5184, #140600, #189301, #40941, #22511 ) ),
 .UNSPECIFIED., .T., .F., .T. ) 
 B_SPLINE_SURFACE_WITH_KNOTS ( ( 4, 3, 4 ),
 ( 4, 1, 1, 1, 1, 1, 1, 4 ),
 ( 0.000000000000000000, 0.5000000000000000000, 1.000000000000000000 ),
 ( 0.000000000000000000, 0.09123828766142533242, 0.1830323254715014447, 0.2554767746403809325, 0.3605042187413262100, 0.5206858269973231312, 0.7335850107976985557, 1.000000000000000000 ),
 .UNSPECIFIED. ) 
 GEOMETRIC_REPRESENTATION_ITEM ( )  RATIONAL_B_SPLINE_SURFACE ( (
 ( 1.000000000000000000, 1.000000000000000000, 1.000000000000000000, 0.9999999999999997780, 1.000000000000000000, 1.000000000000000000, 1.000000000000000222, 1.000000000000000000, 1.000000000000000000, 1.000000000000000000),
 ( 0.3333333333333333703, 0.3333333333333333703, 0.3333333333333334259, 0.3333333333333332593, 0.3333333333333333703, 0.3333333333333333703, 0.3333333333333334814, 0.3333333333333333703, 0.3333333333333333703, 0.3333333333333333703),
 ( 0.3333333333333333703, 0.3333333333333333703, 0.3333333333333334259, 0.3333333333333332593, 0.3333333333333333703, 0.3333333333333333703, 0.3333333333333334814, 0.3333333333333333703, 0.3333333333333333703, 0.3333333333333333703),
 ( 1.000000000000000000, 1.000000000000000000, 1.000000000000000000, 0.9999999999999997780, 1.000000000000000000, 1.000000000000000000, 1.000000000000000222, 1.000000000000000000, 1.000000000000000000, 1.000000000000000000),
 ( 0.3333333333333333703, 0.3333333333333333703, 0.3333333333333334259, 0.3333333333333332593, 0.3333333333333333703, 0.3333333333333333703, 0.3333333333333334814, 0.3333333333333333703, 0.3333333333333333703, 0.3333333333333333703),
 ( 0.3333333333333333703, 0.3333333333333333703, 0.3333333333333334259, 0.3333333333333332593, 0.3333333333333333703, 0.3333333333333333703, 0.3333333333333334814, 0.3333333333333333703, 0.3333333333333333703, 0.3333333333333333703),
 ( 1.000000000000000000, 1.000000000000000000, 1.000000000000000000, 0.9999999999999997780, 1.000000000000000000, 1.000000000000000000, 1.000000000000000222, 1.000000000000000000, 1.000000000000000000, 1.000000000000000000) ) ) 
 REPRESENTATION_ITEM ( '' )  SURFACE ( )  );
#120177 = CARTESIAN_POINT ( 'NONE',  ( 7.235247531187115833, 11.59287255302699648, -0.7998128361456291469 ) ) ;
#120178 = CARTESIAN_POINT ( 'NONE',  ( 1.870285774507766119, 1.081916120455215902, 1.806640566525853808 ) ) ;
#120180 = CARTESIAN_POINT ( 'NONE',  ( -1.402160292154681736E-14, 2.587500000000023892, -1.732050807568863648 ) ) ;
#120179 = CARTESIAN_POINT ( 'NONE',  ( -1.364683531250014514, 12.58854166700806054, -0.7879004041258335089 ) ) ;
#120181 = CARTESIAN_POINT ( 'NONE',  ( 2.365619736264668038, -0.4344343780767513374, 1.920862584678226348 ) ) ;
#120182 = CARTESIAN_POINT ( 'NONE',  ( -5.171509248969888617, 4.998125310078441075, 0.7998128361456281477 ) ) ;
#120183 = CARTESIAN_POINT ( 'NONE',  ( 8.912450614902654777, 3.507114751586604129, 8.024806578262976942 ) ) ;
#120185 = ORIENTED_EDGE ( 'NONE', *, *, #170416, .F. ) ;
#120184 = CARTESIAN_POINT ( 'NONE',  ( 5.959207022242491547, -1.525490245149653701, 0.9768169865009832531 ) ) ;
#120186 = CARTESIAN_POINT ( 'NONE',  ( 5.314433026876846711, 9.143996264757578984, -0.7216878364870267237 ) ) ;
#120187 = STYLED_ITEM ( 'NONE', ( #22522 ), #149381 ) ;
#120188 = CARTESIAN_POINT ( 'NONE',  ( -1.364683531250014514, -0.1989583329919157317, -0.7879004041258359514 ) ) ;
#120189 = CARTESIAN_POINT ( 'NONE',  ( 4.979306205331720747, 1.745251617482036943, -0.6738592683939447214 ) ) ;
#120190 = CARTESIAN_POINT ( 'NONE',  ( 5.770397209236588942, -0.9257025293247715947, -1.851810055641222252 ) ) ;
#120191 =( LENGTH_UNIT ( ) NAMED_UNIT ( * ) SI_UNIT ( .MILLI., .METRE. ) );
#120192 = CARTESIAN_POINT ( 'NONE',  ( -3.797692425159308716, 7.444741906078900406, 0.000000000000000000 ) ) ;
#120193 = FACE_OUTER_BOUND ( 'NONE', #121844, .T. ) ;
#120194 = CARTESIAN_POINT ( 'NONE',  ( 1.499999999999987121, 0.004166666666691258049, 0.8660254037844524744 ) ) ;
#120195 = CARTESIAN_POINT ( 'NONE',  ( 7.507464373665139412, 9.781794407407920389, 1.599625672291281386 ) ) ;
#120196 = CARTESIAN_POINT ( 'NONE',  ( -8.371269781434001800, 11.85389961405997816, -1.199719254218446718 ) ) ;
#120197 = CARTESIAN_POINT ( 'NONE',  ( 6.475954649182838807, 7.584310507915338562, 1.199719254218452047 ) ) ;
#120198 = CARTESIAN_POINT ( 'NONE',  ( -1.364683531250000748, 0.5093750003414208027, 0.000000000000000000 ) ) ;
#120199 = AXIS2_PLACEMENT_3D ( 'NONE', #83449, #168968, #20571 ) ;
#120200 = CARTESIAN_POINT ( 'NONE',  ( -1.201851678989727383E-14, 1.212500000000025002, 1.732050807568877637 ) ) ;
#120202 = CARTESIAN_POINT ( 'NONE',  ( 5.996784015946103885, 5.890669528225568996, 1.040834085586084257E-14 ) ) ;
#120201 = CARTESIAN_POINT ( 'NONE',  ( 5.072687121480487171, 1.354251660176824856, -1.419695456575476689 ) ) ;
#120203 = CARTESIAN_POINT ( 'NONE',  ( 3.110703712691643918, 0.7282687159771012997, -1.880146464672841411 ) ) ;
#120204 = CARTESIAN_POINT ( 'NONE',  ( 3.081152777801674958, 1.513245778044673306, 1.174690267158661872 ) ) ;
#120205 = DIRECTION ( 'NONE',  ( 0.000000000000000000, -1.000000000000000000, -0.000000000000000000 ) ) ;
#120206 = CARTESIAN_POINT ( 'NONE',  ( 0.2401087780563165297, 2.186128513634697512, 0.1550312349237955856 ) ) ;
#120207 =( LENGTH_UNIT ( ) NAMED_UNIT ( * ) SI_UNIT ( .MILLI., .METRE. ) );
#120208 = CARTESIAN_POINT ( 'NONE',  ( 2.653401028632852654, 0.5028369177751991215, -1.801603059227441239 ) ) ;
#120209 = CARTESIAN_POINT ( 'NONE',  ( -1.364683531250010295, 5.738541667008088432, -0.7879004041258300672 ) ) ;
#120210 = CARTESIAN_POINT ( 'NONE',  ( 4.342045473679829293, -1.241779438462310203, -1.584497923379190931 ) ) ;
#120211 = CARTESIAN_POINT ( 'NONE',  ( -9.182950115157607840, 9.607863310639020327, 0.7998128361456462443 ) ) ;
#120212 = EDGE_CURVE ( 'NONE', #63949, #124240, #91511, .T. ) ;
#120214 = CARTESIAN_POINT ( 'NONE',  ( 4.640305734921336800, 0.8116497034467985427, 1.955664341570842790 ) ) ;
#120213 = CARTESIAN_POINT ( 'NONE',  ( -3.795919822146277767, 7.372397525905215687, -0.7216878364870267237 ) ) ;
#120215 = CARTESIAN_POINT ( 'NONE',  ( -2.352382916832147064, 2.704376054464897816, -2.456006149337788269 ) ) ;
#120216 = CARTESIAN_POINT ( 'NONE',  ( 6.057099581687969803, 1.694805161836069107, -1.188877858866774107 ) ) ;
#120218 = FACE_OUTER_BOUND ( 'NONE', #110126, .T. ) ;
#120217 = CARTESIAN_POINT ( 'NONE',  ( 1.224293845215556953, 2.015865829440838031, 0.5543246906533367824 ) ) ;
#120220 = EDGE_LOOP ( 'NONE', ( #35959, #208431, #206197, #158473 ) ) ;
#120219 = CARTESIAN_POINT ( 'NONE',  ( 6.668987789458199700, -1.670617902683011025, -0.7365018021969899076 ) ) ;
#120221 = CARTESIAN_POINT ( 'NONE',  ( 5.926885707468349196, 10.06645042535509660, 1.040834085586084257E-14 ) ) ;
#120222 = CARTESIAN_POINT ( 'NONE',  ( 8.042162931142705418, -6.699677480914211891, -7.505515594164287485 ) ) ;
#120223 = CARTESIAN_POINT ( 'NONE',  ( -0.08865135991733066878, -9.916958638733639475, -9.499586356067535320 ) ) ;
#120224 = CARTESIAN_POINT ( 'NONE',  ( -10.43230948805442893, 5.066484524551064794, 5.254757398418679060 ) ) ;
#120226 = CARTESIAN_POINT ( 'NONE',  ( 7.117667457050084856, 7.406292909420979953, -0.7216878364870257245 ) ) ;
#120225 = CARTESIAN_POINT ( 'NONE',  ( 6.283314124929436417, 9.417951348137970413, -1.199719254218440723 ) ) ;
#120227 = LINE ( 'NONE', #172110, #37373 ) ;
#120229 = CARTESIAN_POINT ( 'NONE',  ( 0.7327119416217167114, 1.673282569690562882, 0.6944263290599298477 ) ) ;
#120228 = CARTESIAN_POINT ( 'NONE',  ( 7.828907357248368726, 8.098423103070084395, 0.7998128361456281477 ) ) ;
#120230 = CARTESIAN_POINT ( 'NONE',  ( -6.821723845970312894, 11.11042825360738284, 0.000000000000000000 ) ) ;
#120231 = CARTESIAN_POINT ( 'NONE',  ( 6.342516933094585418, 6.294024598232139667, 1.040834085586084257E-14 ) ) ;
#120232 = CARTESIAN_POINT ( 'NONE',  ( -1.500000000000001332, -1.099999999999982991, 0.000000000000000000 ) ) ;
#120233 = CARTESIAN_POINT ( 'NONE',  ( 0.9999999999999833467, 9.200000000000018829, 0.4000000000000144551 ) ) ;
#120234 = CARTESIAN_POINT ( 'NONE',  ( 4.359110081993588182, 5.044382169536003602, -1.199719254218452047 ) ) ;
#120235 = ORIENTED_EDGE ( 'NONE', *, *, #187696, .T. ) ;
#120236 = CARTESIAN_POINT ( 'NONE',  ( 5.853138716089107518, 0.1455171034051294665, -2.011206573937059261 ) ) ;
#120237 = CARTESIAN_POINT ( 'NONE',  ( 0.1531979293848736434, 0.3668625560977051281, 2.088361607889513305 ) ) ;
#120238 = CARTESIAN_POINT ( 'NONE',  ( 0.7119062752653980697, -6.995223886616102449E-15, -1.051716123837681760 ) ) ;
#120239 = CARTESIAN_POINT ( 'NONE',  ( 7.465774003072967346, -6.268611901546719878, 7.465774003072962017 ) ) ;
#120240 = CARTESIAN_POINT ( 'NONE',  ( -5.097502569058221411, 6.009803087731781623, -1.082531754730544860 ) ) ;
#120241 = CARTESIAN_POINT ( 'NONE',  ( 10.05978679165993483, 11.79913468076720306, 1.082531754730548412 ) ) ;
#120242 = CARTESIAN_POINT ( 'NONE',  ( 3.414863416077691838, -1.494280747806640885, 1.283048038104795507 ) ) ;
#120243 = CARTESIAN_POINT ( 'NONE',  ( 4.605092316430917876, -0.09611821078869468848, 2.014234682242924457 ) ) ;
#120244 = CARTESIAN_POINT ( 'NONE',  ( -5.696397096036042385, 9.797547045350714967, -0.7998128361456231517 ) ) ;
#120245 = CARTESIAN_POINT ( 'NONE',  ( 0.4320269763654895345, 3.055387103097206847, -0.4199383792806877236 ) ) ;
#120246 = CARTESIAN_POINT ( 'NONE',  ( 6.727182134110200273, -0.004969159814478123736, 2.189081792362323586 ) ) ;
#120247 = CARTESIAN_POINT ( 'NONE',  ( 4.945371362016417471, 0.6893947036107104243, -2.080263006054481334 ) ) ;
#120248 = CARTESIAN_POINT ( 'NONE',  ( -3.147653791585731220, 8.920000000000001705, -2.419999999999998597 ) ) ;
#120249 = CARTESIAN_POINT ( 'NONE',  ( 3.381779240904962069, 1.220913077095790111, 1.490098802054098837 ) ) ;
#120250 = CARTESIAN_POINT ( 'NONE',  ( -7.588813295347149435, 9.876701482703580837, -1.599625672291263179 ) ) ;
#120251 = CARTESIAN_POINT ( 'NONE',  ( -0.02948999725180690215, 0.001137248348246927814, -1.926291057026579656 ) ) ;
#120252 = CARTESIAN_POINT ( 'NONE',  ( -0.004863692847738298151, -0.4900785244342681923, -2.159743284330918112 ) ) ;
#120253 =( NAMED_UNIT ( * ) PLANE_ANGLE_UNIT ( ) SI_UNIT ( $, .RADIAN. ) );
#120254 = ORIENTED_EDGE ( 'NONE', *, *, #193063, .F. ) ;
#120255 = CARTESIAN_POINT ( 'NONE',  ( 3.268924434670684498, 6.827845917175511481, -1.734723475976807094E-15 ) ) ;
#120256 = EDGE_LOOP ( 'NONE', ( #43442, #160994, #148447, #10789 ) ) ;
#120257 = CARTESIAN_POINT ( 'NONE',  ( 4.662928361469391270, 1.524974937183399160, -1.246301010749743199 ) ) ;
#120258 = ORIENTED_EDGE ( 'NONE', *, *, #125125, .T. ) ;
#120260 = CARTESIAN_POINT ( 'NONE',  ( 3.967443207080887380, -1.674941000623398457, -1.116458483097344301 ) ) ;
#120259 = CARTESIAN_POINT ( 'NONE',  ( 0.7142757748631656245, 1.794906310038762109, 0.7420174003010558961 ) ) ;
#120261 = AXIS2_PLACEMENT_3D ( 'NONE', #12884, #177551, #129942 ) ;
#120262 = CARTESIAN_POINT ( 'NONE',  ( 5.554211264220430877, 2.030576384096828502, -1.076727444025220803 ) ) ;
#120264 = CARTESIAN_POINT ( 'NONE',  ( 3.801460577334394575, -1.406423387113703960, -1.218697170607488944 ) ) ;
#120263 = SURFACE_STYLE_USAGE ( .BOTH. , #139664 ) ;
#120265 = CARTESIAN_POINT ( 'NONE',  ( 7.388267364804250725, 7.584343111885245570, -0.7998128361456341429 ) ) ;
#120266 = DIRECTION ( 'NONE',  ( 3.330669073875478989E-16, -3.540251991789410786E-16, -1.000000000000000000 ) ) ;
#120267 = CARTESIAN_POINT ( 'NONE',  ( -7.531718027591449705, 8.745758106066849891, 1.199719254218462483 ) ) ;
#120268 = CARTESIAN_POINT ( 'NONE',  ( -3.960390268967665328, 6.674186842887300131, 1.082531754730549967 ) ) ;
#120269 = CARTESIAN_POINT ( 'NONE',  ( 0.1170720436180875679, -0.1011795954627830590, 2.189343785608413917 ) ) ;
#120270 = CARTESIAN_POINT ( 'NONE',  ( 5.721177635286841756, 6.737423998331861341, -1.082531754730543083 ) ) ;
#120271 = EDGE_CURVE ( 'NONE', #39684, #12895, #3595, .T. ) ;
#120272 = CARTESIAN_POINT ( 'NONE',  ( 6.825078400183575589, 7.629137130509070275, 2.455651831298297338 ) ) ;
#120273 = CARTESIAN_POINT ( 'NONE',  ( 2.179728514415657799E-12, -5.796408561409501559, -10.41272866534444752 ) ) ;
#120274 = CARTESIAN_POINT ( 'NONE',  ( 1.031563979315492485, -1.156294252604734396, -1.412831148817683680 ) ) ;
#120275 = CARTESIAN_POINT ( 'NONE',  ( -5.461236948206312114, 5.265864615862458464, 0.7998128361456341429 ) ) ;
#120276 = CARTESIAN_POINT ( 'NONE',  ( 2.672175078814063909, 1.228020439816409848, 1.224710958539473094 ) ) ;
#120277 = CARTESIAN_POINT ( 'NONE',  ( 0.6124999999999707345, 1.895833334016133742, 1.060881119635880721 ) ) ;
#120278 = CARTESIAN_POINT ( 'NONE',  ( 6.509000000000053632, 6.037921079186737927, 2.494901127718162304 ) ) ;
#120279 = CARTESIAN_POINT ( 'NONE',  ( -4.880045225915050189, 7.780804299287790826, 1.199719254218464037 ) ) ;
#120280 = CARTESIAN_POINT ( 'NONE',  ( 1.123270288250309834, 2.971052654332832610, -0.7749999999993620881 ) ) ;
#120281 = CARTESIAN_POINT ( 'NONE',  ( 5.988856447087389512, -0.2726756491404982441, -1.805090154579996442 ) ) ;
#120282 = CARTESIAN_POINT ( 'NONE',  ( 3.485159065011545376, 0.04355839926390054490, 1.961427607708135179 ) ) ;
#120283 = EDGE_CURVE ( 'NONE', #102449, #112981, #205879, .T. ) ;
#120284 = CARTESIAN_POINT ( 'NONE',  ( -1.225000000000022293, -1.166666665983833617, 0.7072540797572477445 ) ) ;
#120285 = CARTESIAN_POINT ( 'NONE',  ( -10.00321840878439339, 10.56484298653695397, 1.040834085586084257E-14 ) ) ;
#120286 = CARTESIAN_POINT ( 'NONE',  ( 6.775324078527185989, 8.927630729746953264, -1.599625672291262513 ) ) ;
#120287 = CARTESIAN_POINT ( 'NONE',  ( 3.985108911058360182, -1.979049277059058864, -0.7619450576143712572 ) ) ;
#120288 = CARTESIAN_POINT ( 'NONE',  ( 6.827182134110199918, 7.629137130509069387, 2.789055895399249252 ) ) ;
#120289 = ADVANCED_FACE ( 'NONE', ( #137285 ), #106571, .T. ) ;
#120290 = CARTESIAN_POINT ( 'NONE',  ( -10.13202086811422475, 10.71511252242175161, -0.7998128361456291469 ) ) ;
#120291 = CIRCLE ( 'NONE', #85744, 0.08000000000000020983 ) ;
#120292 = CARTESIAN_POINT ( 'NONE',  ( 2.237250781069185734, -0.09733102107959036575, -2.068066387140480522 ) ) ;
#120294 = CARTESIAN_POINT ( 'NONE',  ( -6.009258394948636914E-15, 14.71875000068279427, -1.732050807568875195 ) ) ;
#120293 = CARTESIAN_POINT ( 'NONE',  ( 0.2999999999999669598, 4.050057683544661558, -0.8916696671246847616 ) ) ;
#120296 = ORIENTED_EDGE ( 'NONE', *, *, #173466, .F. ) ;
#120295 = CARTESIAN_POINT ( 'NONE',  ( 4.688250436721117964, 1.278455086129190121, 1.816331037743470933 ) ) ;
#120297 = CARTESIAN_POINT ( 'NONE',  ( 1.829147786997789016, 0.8750025983248543859, -2.125820487401499204 ) ) ;
#120298 = CARTESIAN_POINT ( 'NONE',  ( 9.761507412159302177, 10.49077285704843199, -0.7216878364870257245 ) ) ;
#120300 = CARTESIAN_POINT ( 'NONE',  ( -3.285556943749998737, -2.880208332855377584, 1.896917185911908499 ) ) ;
#120299 = CARTESIAN_POINT ( 'NONE',  ( 6.943184063974162434, 9.193743722760251202, -1.443375672974064550 ) ) ;
#120301 = CARTESIAN_POINT ( 'NONE',  ( 6.509000000000010999, 0.004788705324892603143, 2.000274819378269786 ) ) ;
#120302 = CARTESIAN_POINT ( 'NONE',  ( -5.446377490701157065, 6.293253950424717580, -1.032046567709556273 ) ) ;
#120303 = CARTESIAN_POINT ( 'NONE',  ( 3.287273477832891366, 0.04233216220104508987, -1.912079899511004433 ) ) ;
#120304 = CARTESIAN_POINT ( 'NONE',  ( -0.5146802535525265565, 6.793498207845753534, -3.562260005870215629 ) ) ;
#120305 = CARTESIAN_POINT ( 'NONE',  ( 4.155083606764530479, -1.434382041474260516, -0.9574503856549732017 ) ) ;
#120306 = CARTESIAN_POINT ( 'NONE',  ( 1.762908039156896978, -0.1037823317905466058, -2.014007988105172231 ) ) ;
#120307 = CARTESIAN_POINT ( 'NONE',  ( 3.674713919220749414, 1.665813291469726787, 1.584223201981638685 ) ) ;
#120308 = DIRECTION ( 'NONE',  ( 0.000000000000000000, 1.000000000000000000, 0.000000000000000000 ) ) ;
#120309 = CARTESIAN_POINT ( 'NONE',  ( 6.445935634123193481, 0.8078061350838610100, -1.945192272397469280 ) ) ;
#120310 = CARTESIAN_POINT ( 'NONE',  ( -5.804299160426242388, 6.904675454319632699, -1.082531754730549967 ) ) ;
#120311 = ORIENTED_EDGE ( 'NONE', *, *, #67524, .F. ) ;
#120312 = CARTESIAN_POINT ( 'NONE',  ( 5.008955365368598756, 1.539791945809299012, 0.8722439129504773181 ) ) ;
#120314 = CARTESIAN_POINT ( 'NONE',  ( 0.3227791477718846558, 2.195406398872503217, 0.6593016323864949735 ) ) ;
#120313 = CARTESIAN_POINT ( 'NONE',  ( 6.688968683495743583, 8.897159112202094988, -1.599625672291283607 ) ) ;
#120315 = CARTESIAN_POINT ( 'NONE',  ( 6.509700743154069436, -0.8726169035938921015, -1.621212818125779220 ) ) ;
#120316 = CARTESIAN_POINT ( 'NONE',  ( -4.569261463005423352, 5.289558780716470565, -1.199719254218446718 ) ) ;
#120317 = CARTESIAN_POINT ( 'NONE',  ( 5.824229312739954700, 2.111140916326431416, 0.5876101183235474812 ) ) ;
#120318 = CARTESIAN_POINT ( 'NONE',  ( -5.981082042284069367, 7.006959133200059142, 1.199719254218452935 ) ) ;
#120319 = LINE ( 'NONE', #151693, #7507 ) ;
#120320 = DIRECTION ( 'NONE',  ( -0.000000000000000000, -1.000000000000000000, -0.000000000000000000 ) ) ;
#120321 = CARTESIAN_POINT ( 'NONE',  ( 0.5026746641029911089, 2.165404592850531440, 0.1593437185135812284 ) ) ;
#120322 = CARTESIAN_POINT ( 'NONE',  ( 1.411342602523330214, -1.897109289313268166, 0.6839406069230756779 ) ) ;
#120323 = CARTESIAN_POINT ( 'NONE',  ( 1.364683531249992088, 5.634375000341417916, 1.214306433183764966E-14 ) ) ;
#120324 = CARTESIAN_POINT ( 'NONE',  ( 4.195867187722844172, -0.7361232629885716694, 1.780507395703424978 ) ) ;
#120325 = CARTESIAN_POINT ( 'NONE',  ( -1.364683531250010295, 11.88020833367473017, 0.7879004041258445001 ) ) ;
#120326 = CARTESIAN_POINT ( 'NONE',  ( 0.7389115964958146154, 1.317144317036992973, -1.788695212975628168 ) ) ;
#120328 = ORIENTED_EDGE ( 'NONE', *, *, #70447, .F. ) ;
#120327 = CARTESIAN_POINT ( 'NONE',  ( 9.028840231696797503, 12.62106513936658203, -1.199719254218446718 ) ) ;
#120330 = CARTESIAN_POINT ( 'NONE',  ( -6.189608320745405123, 5.317548586107503361, 2.438128985384274472 ) ) ;
#120329 = CARTESIAN_POINT ( 'NONE',  ( 1.270916165646588603, 3.040225491120026380, -0.7749999999999910294 ) ) ;
#120331 = CARTESIAN_POINT ( 'NONE',  ( 1.499999999999959810, 7.564371094685075292, -10.87018506808107965 ) ) ;
#120332 = CARTESIAN_POINT ( 'NONE',  ( 4.701980345841006326, 4.380065246436280368, 0.7998128361456341429 ) ) ;
#120333 = CARTESIAN_POINT ( 'NONE',  ( -1.115562610750309283E-14, 9.093750000682799595, 1.500000000000001554 ) ) ;
#120334 = PLANE ( 'NONE',  #159766 ) ;
#120335 = CARTESIAN_POINT ( 'NONE',  ( 3.790341827058436142, 1.467891733132551613, -0.9347920342070329403 ) ) ;
#120337 = CARTESIAN_POINT ( 'NONE',  ( 2.805073129645048624, -1.632656238785214597, 1.087510969322850629 ) ) ;
#120336 = AXIS2_PLACEMENT_3D ( 'NONE', #174488, #111662, #73759 ) ;
#120339 = CARTESIAN_POINT ( 'NONE',  ( 1.364683531249988535, 2.926041667008082658, 0.7879004041258500513 ) ) ;
#120338 = CARTESIAN_POINT ( 'NONE',  ( 5.834086172582112262, 5.700855377634248100, 1.040834085586084257E-14 ) ) ;
#120340 = CARTESIAN_POINT ( 'NONE',  ( -5.203466197636060997, 6.462176032175228180, 1.180525766716962410 ) ) ;
#120341 = CARTESIAN_POINT ( 'NONE',  ( 8.543609354905870035, 13.11929468069890525, 0.7998128361456462443 ) ) ;
#120342 = CARTESIAN_POINT ( 'NONE',  ( 0.3618804954101816906, -0.5516051106895186740, 1.987472385349927428 ) ) ;
#120343 = CARTESIAN_POINT ( 'NONE',  ( -8.694856585065634746, 9.038420858865048757, 0.7998128361456462443 ) ) ;
#120344 = CARTESIAN_POINT ( 'NONE',  ( -4.243338890952901288, 6.934017225211593249, -1.082531754730548412 ) ) ;
#120345 = CARTESIAN_POINT ( 'NONE',  ( 5.155482549980198392, 1.942097955248718533, -0.5424665614216088727 ) ) ;
#120346 = CARTESIAN_POINT ( 'NONE',  ( 0.7610528644104715967, -1.636749228899089470, 1.562301092707372607 ) ) ;
#120348 = ORIENTED_EDGE ( 'NONE', *, *, #46978, .T. ) ;
#120347 = CARTESIAN_POINT ( 'NONE',  ( -6.205881626753225966, 8.263281202677319470, 1.599625672291283607 ) ) ;
#120349 = CARTESIAN_POINT ( 'NONE',  ( 0.7499999999999885647, 0.01458333401615358182, 1.299038105676657340 ) ) ;
#120350 = CARTESIAN_POINT ( 'NONE',  ( 1.704156511045151978, -0.6684128243485131238, -1.747238085743174185 ) ) ;
#120351 = CARTESIAN_POINT ( 'NONE',  ( -0.08779760418278770295, -1.063538860511966444, -1.369745729481768759 ) ) ;
#120353 = CARTESIAN_POINT ( 'NONE',  ( 4.335597073515660149, 0.9364531651635084053, -1.981528385891350386 ) ) ;
#120352 = CARTESIAN_POINT ( 'NONE',  ( -3.956095110007852622E-14, 2.328125000341396689, -1.570758158831800255 ) ) ;
#120354 = CARTESIAN_POINT ( 'NONE',  ( 5.561655955723623812, 0.4570820274143985729, -2.261718950934066275 ) ) ;
#120355 = CARTESIAN_POINT ( 'NONE',  ( 0.4618819262211275034, 2.038552468250200533, -0.3016747405163843765 ) ) ;
#120356 = CARTESIAN_POINT ( 'NONE',  ( 3.328005318368632892, 1.894807597966931878, 0.4246257584521081485 ) ) ;
#120357 = CARTESIAN_POINT ( 'NONE',  ( -2.914639836813632812, 6.344237543017112735, 0.7216878364870317197 ) ) ;
#120358 = DIRECTION ( 'NONE',  ( 0.000000000000000000, 0.000000000000000000, 1.000000000000000000 ) ) ;
#120359 = ADVANCED_FACE ( 'NONE', ( #17629 ), #194540, .T. ) ;
#120360 = CARTESIAN_POINT ( 'NONE',  ( 4.746763178560261309, 5.670883475476017566, 1.082531754730549078 ) ) ;
#120361 =( LENGTH_UNIT ( ) NAMED_UNIT ( * ) SI_UNIT ( .MILLI., .METRE. ) );
#120362 = CARTESIAN_POINT ( 'NONE',  ( 4.201796189063250253, 1.844709454618495670, 0.8146275914719460776 ) ) ;
#120363 = CARTESIAN_POINT ( 'NONE',  ( -4.568734577680899633, 4.432537883490215158, -0.7216878364870207285 ) ) ;
#120364 = CARTESIAN_POINT ( 'NONE',  ( -6.954406449166956605, 7.078172043641714595, -0.7998128361456362523 ) ) ;
#120365 = CARTESIAN_POINT ( 'NONE',  ( 8.934986926605834157, 10.38290515491702770, -1.199719254218446718 ) ) ;
#120367 = CARTESIAN_POINT ( 'NONE',  ( 7.721398836998361048, -5.907420853759298041, -7.721398836998386805 ) ) ;
#120366 = CARTESIAN_POINT ( 'NONE',  ( 0.8908993799596062191, 1.611356928563783208, -0.8583080905386344384 ) ) ;
#120368 = CARTESIAN_POINT ( 'NONE',  ( -5.798046968499580345, 6.793418213784815585, 1.199719254218452935 ) ) ;
#120369 = CARTESIAN_POINT ( 'NONE',  ( -4.980641328173854632, 6.904110530993182948, 1.599625672291263401 ) ) ;
#120370 = CARTESIAN_POINT ( 'NONE',  ( -9.956232484441596142, 5.504245459870187318, 6.026037945409589369 ) ) ;
#120371 = ORIENTED_EDGE ( 'NONE', *, *, #83347, .F. ) ;
#120372 = CARTESIAN_POINT ( 'NONE',  ( 0.2159880523044250267, -2.119658899406823505, 0.4233941889316418239 ) ) ;
#120373 = CARTESIAN_POINT ( 'NONE',  ( -6.753369912938502750, 7.051555451282599307, 0.000000000000000000 ) ) ;
#120374 = CARTESIAN_POINT ( 'NONE',  ( -1.349890321011207206, 8.200329036966270024, 10.79298809153610961 ) ) ;
#120375 = CARTESIAN_POINT ( 'NONE',  ( -10.15913717534155047, 10.74674821418697057, 0.7998128361456462443 ) ) ;
#120376 = CARTESIAN_POINT ( 'NONE',  ( 5.496742197731416368, -1.970900515782060936, -0.4404336293717215356 ) ) ;
#120378 = ORIENTED_EDGE ( 'NONE', *, *, #179894, .F. ) ;
#120377 = CARTESIAN_POINT ( 'NONE',  ( 5.496814983966967993, -2.166796134289544984, -0.4884321829702345519 ) ) ;
#120379 = CARTESIAN_POINT ( 'NONE',  ( -8.100070429521727178, 8.414780020722290033, 0.7998128361456341429 ) ) ;
#120380 = CARTESIAN_POINT ( 'NONE',  ( 4.493637847925535667, 7.329995691633395261, -1.199719254218452047 ) ) ;
#120381 = CARTESIAN_POINT ( 'NONE',  ( 5.243067039532245843, -1.768777590322716309, 1.057421601032474623 ) ) ;
#120382 = CARTESIAN_POINT ( 'NONE',  ( 4.377577386359387646, -0.4445010797573499817, -1.966645064109616481 ) ) ;
#120383 = ORIENTED_EDGE ( 'NONE', *, *, #89670, .F. ) ;
#120384 = VERTEX_POINT ( 'NONE', #112303 ) ;
#120385 = CARTESIAN_POINT ( 'NONE',  ( 1.910130646976073043, 3.278792710263286114, -0.4195261609911307144 ) ) ;
#120386 = CARTESIAN_POINT ( 'NONE',  ( 2.693266070609028784, 6.293894182352508970, 0.000000000000000000 ) ) ;
#120388 = ORIENTED_EDGE ( 'NONE', *, *, #70198, .T. ) ;
#120387 = CARTESIAN_POINT ( 'NONE',  ( -7.608060475923978494, 8.905100639113307182, 1.199719254218452047 ) ) ;
#120389 = CARTESIAN_POINT ( 'NONE',  ( 4.812217717264355876, 8.234349973070900219, 0.8868998539744571419 ) ) ;
#120390 = CARTESIAN_POINT ( 'NONE',  ( 4.042342166264912606, 1.899327733865597168, -0.6766104081444989093 ) ) ;
#120391 = CARTESIAN_POINT ( 'NONE',  ( 3.820104440490858622, 1.748809976318686177, 0.5759312369505511509 ) ) ;
#120392 = DIRECTION ( 'NONE',  ( 0.000000000000000000, 1.000000000000000000, 0.000000000000000000 ) ) ;
#120393 = CARTESIAN_POINT ( 'NONE',  ( 2.438448314377542392, 1.086391669559241047, -2.035977865114136254 ) ) ;
#120394 = CARTESIAN_POINT ( 'NONE',  ( 4.934241560730721510, 4.721313007132757811, 0.000000000000000000 ) ) ;
#120395 = CARTESIAN_POINT ( 'NONE',  ( 4.710339443014814442, -0.9195336665917231977, -1.956380038831563972 ) ) ;
#120396 = CARTESIAN_POINT ( 'NONE',  ( 8.555358625423188812, 9.940005470203933768, 1.199719254218462483 ) ) ;
#120397 = CARTESIAN_POINT ( 'NONE',  ( 0.5736477084636192325, -1.077812090576779402, 1.615333711560530849 ) ) ;
#120398 = CARTESIAN_POINT ( 'NONE',  ( -5.773074481320628948, 5.629675071162500544, 0.000000000000000000 ) ) ;
#120399 = CARTESIAN_POINT ( 'NONE',  ( -3.594090741707730796, 15.51961551409570994, 11.45768715124896708 ) ) ;
#120400 = CARTESIAN_POINT ( 'NONE',  ( -1.499999999999997780, 4.181250000682819490, 1.214306433183764966E-14 ) ) ;
#120401 = CARTESIAN_POINT ( 'NONE',  ( 2.535844406030359544, 0.8837261853790435717, -1.648756255988912400 ) ) ;
#120402 = CARTESIAN_POINT ( 'NONE',  ( 0.4210825541404016326, -0.1013260788591107547, 1.968891031686560211 ) ) ;
#120404 = CARTESIAN_POINT ( 'NONE',  ( -7.587723245503481095, 8.881373870289390737, 1.199719254218452047 ) ) ;
#120403 = CARTESIAN_POINT ( 'NONE',  ( 1.364683531249992088, 5.634375000341417916, 1.214306433183764966E-14 ) ) ;
#120405 = CARTESIAN_POINT ( 'NONE',  ( 2.016531038934398445, -1.041976349804032420, -1.945408382319254503 ) ) ;
#120406 = ORIENTED_EDGE ( 'NONE', *, *, #113521, .F. ) ;
#120407 = EDGE_CURVE ( 'NONE', #108500, #79124, #36251, .T. ) ;
#120408 = CARTESIAN_POINT ( 'NONE',  ( 3.931903513251288285, 8.991426765939651844, -0.7749999999999996891 ) ) ;
#120409 = CARTESIAN_POINT ( 'NONE',  ( 3.246287715468270108, 5.874753870433235825, 1.199719254218450271 ) ) ;
#120410 = CARTESIAN_POINT ( 'NONE',  ( -5.057354993097396445, 5.859001232490445688, -1.199719254218446718 ) ) ;
#120411 = CARTESIAN_POINT ( 'NONE',  ( -7.847520364415487393, -5.402328468025377362, 7.653681110113387476 ) ) ;
#120412 = CARTESIAN_POINT ( 'NONE',  ( 6.174684870424203886, -1.871919000353940099, -0.6187097519457245287 ) ) ;
#120413 = CARTESIAN_POINT ( 'NONE',  ( 0.4468379896771547122, 2.301730118641607703, 0.1654463548556948105 ) ) ;
#120414 = CARTESIAN_POINT ( 'NONE',  ( 0.6780837441340243910, -1.046368970337024473, -1.659334490400856454 ) ) ;
#120415 = ADVANCED_FACE ( 'NONE', ( #28854 ), #77594, .T. ) ;
#120416 = CARTESIAN_POINT ( 'NONE',  ( 3.713784835328519218, 0.5057260441109856508, -1.999473844451674642 ) ) ;
#120417 = CARTESIAN_POINT ( 'NONE',  ( 5.341549334104188418, 7.254893527920112994, 1.443375672974062551 ) ) ;
#120418 = CARTESIAN_POINT ( 'NONE',  ( 7.856023664475727308, 8.130058794835305136, -0.7998128361456341429 ) ) ;
#120419 = VERTEX_POINT ( 'NONE', #210789 ) ;
#120420 = CARTESIAN_POINT ( 'NONE',  ( 9.042925270190638187, 9.652427024751663254, 0.7216878364870458196 ) ) ;
#120421 = CARTESIAN_POINT ( 'NONE',  ( -1.364683531249997417, 3.571875000341423245, 1.214306433183764966E-14 ) ) ;
#120422 = CARTESIAN_POINT ( 'NONE',  ( 10.24999999999999822, 1.255262969126037044E-15, 6.123233995736778362E-17 ) ) ;
#120423 = CARTESIAN_POINT ( 'NONE',  ( 5.056828107772846082, 6.922718763866881453, -1.443375672974051449 ) ) ;
#120424 = CARTESIAN_POINT ( 'NONE',  ( 6.250449712397290192, -2.160098187209258835, -0.2192636458223720386 ) ) ;
#120426 = CARTESIAN_POINT ( 'NONE',  ( 5.407694413872749628, -0.8332299576223768378, -1.642021276980778932 ) ) ;
#120425 = DIRECTION ( 'NONE',  ( 0.000000000000000000, -1.000000000000000000, 0.000000000000000000 ) ) ;
#120427 = DIRECTION ( 'NONE',  ( 1.000000000000000000, 0.000000000000000000, 0.000000000000000000 ) ) ;
#120428 = CARTESIAN_POINT ( 'NONE',  ( -11.87828357749937069, 12.29689747259577892, -1.708055325888869325 ) ) ;
#120429 = CARTESIAN_POINT ( 'NONE',  ( 0.2978465640060874997, -1.869987984933557890, -0.05268733258671080832 ) ) ;
#120430 = CARTESIAN_POINT ( 'NONE',  ( -4.762889583212370326, 6.995502248939536649, 1.426468515190159714 ) ) ;
#120431 = DIRECTION ( 'NONE',  ( -5.578564026256490882E-16, -1.000000000000000000, -9.066213480720158442E-32 ) ) ;
#120432 = EDGE_CURVE ( 'NONE', #154836, #214357, #32873, .T. ) ;
#120433 = CARTESIAN_POINT ( 'NONE',  ( 6.142241479726070708, 7.081583759122534794, -1.089790755372788800 ) ) ;
#120434 = CARTESIAN_POINT ( 'NONE',  ( -1.290813828370758864, 3.620001302969693580, 0.4579576469030058883 ) ) ;
#120435 = CARTESIAN_POINT ( 'NONE',  ( 2.395042364772178356, 1.366200922416866526, 1.125074557178520118 ) ) ;
#120437 = CARTESIAN_POINT ( 'NONE',  ( 6.076820132975093713, -1.421968828841757126, 1.425219213311772926 ) ) ;
#120436 = TOROIDAL_SURFACE ( 'NONE', #165347, -0.1799999999926198968, 0.5000000000000013323 ) ;
#120439 = CARTESIAN_POINT ( 'NONE',  ( 4.288635103545942684, 1.478190772419993415, -1.218367487985058339 ) ) ;
#120438 = CARTESIAN_POINT ( 'NONE',  ( -8.533967624797991647, 12.04371376465130439, -1.199719254218446718 ) ) ;
#120440 = DIRECTION ( 'NONE',  ( -0.6507913734559642727, 0.7592566023653003482, 2.775557561562893816E-17 ) ) ;
#120441 = CARTESIAN_POINT ( 'NONE',  ( 5.318794011649015552, -1.427836685786993742, 1.356881127696080158 ) ) ;
#120442 = CARTESIAN_POINT ( 'NONE',  ( 0.07077104593807002908, 0.8175350930016941353, 1.956879683024402183 ) ) ;
#120443 = CARTESIAN_POINT ( 'NONE',  ( -1.754679937794462408, -0.9610454613041046201, 1.302031786359981957 ) ) ;
#120444 = CARTESIAN_POINT ( 'NONE',  ( 2.957714569337116295, 1.861795396119047208, -0.1817069356538636715 ) ) ;
#120446 = ORIENTED_EDGE ( 'NONE', *, *, #38054, .F. ) ;
#120445 = CARTESIAN_POINT ( 'NONE',  ( 6.604117967919251875, -1.724316898024110811, 0.05080964468639861259 ) ) ;
#120448 = CARTESIAN_POINT ( 'NONE',  ( 4.528060117284244512, 4.385084346360807572, 0.7216878364870317197 ) ) ;
#120447 = CARTESIAN_POINT ( 'NONE',  ( 3.633602750639616019, -2.039237483250630589, 0.8441791899983088765 ) ) ;
#120449 = CARTESIAN_POINT ( 'NONE',  ( 0.6823417656249882723, 2.738541667008084879, -1.181850606188749264 ) ) ;
#120450 = CARTESIAN_POINT ( 'NONE',  ( 0.2563952634283462872, -2.062181505987520147, -0.05231737696831904177 ) ) ;
#120451 = CARTESIAN_POINT ( 'NONE',  ( 7.124973419181436007, 8.271222729588529887, -1.199719254218446718 ) ) ;
#120452 = CARTESIAN_POINT ( 'NONE',  ( -8.666686507633592385, 11.13422023037111330, 1.599625672291269396 ) ) ;
#120453 = FACE_OUTER_BOUND ( 'NONE', #21941, .T. ) ;
#120454 = CARTESIAN_POINT ( 'NONE',  ( -5.413783410558481890, 5.210502155273325720, -0.7998128361456221525 ) ) ;
#120455 = EDGE_CURVE ( 'NONE', #211530, #105777, #162063, .T. ) ;
#120456 = LINE ( 'NONE', #88963, #33670 ) ;
#120458 = AXIS2_PLACEMENT_3D ( 'NONE', #210785, #62408, #124306 ) ;
#120457 = AXIS2_PLACEMENT_3D ( 'NONE', #120293, #153787, #23768 ) ;
#120459 = VERTEX_POINT ( 'NONE', #167119 ) ;
#120460 = CARTESIAN_POINT ( 'NONE',  ( 2.717306809760032138, -1.800131872397674471, -1.022606600864908399 ) ) ;
#120461 = CARTESIAN_POINT ( 'NONE',  ( 1.499999999999990896, 4.025000000000021672, 1.214306433183764966E-14 ) ) ;
#120462 = CARTESIAN_POINT ( 'NONE',  ( 4.137209430464448445, 7.978494768850520558, 1.040834085586084257E-14 ) ) ;
#120463 = CARTESIAN_POINT ( 'NONE',  ( -6.126043159632901691, 7.090966632250176538, 1.117993467579528222 ) ) ;
#120464 = CARTESIAN_POINT ( 'NONE',  ( 1.014326189163064607, -2.019862491587170350, 0.002270882547714125031 ) ) ;
#120465 = DIRECTION ( 'NONE',  ( 0.000000000000000000, -1.000000000000000000, 0.000000000000000000 ) ) ;
#120466 = CARTESIAN_POINT ( 'NONE',  ( -1.364683531250010295, 4.280208333674753618, 0.7879004041258379498 ) ) ;
#120467 = ORIENTED_EDGE ( 'NONE', *, *, #44771, .F. ) ;
#120469 = CARTESIAN_POINT ( 'NONE',  ( 9.598809568795314107, 10.30095870645710754, -0.7216878364870257245 ) ) ;
#120468 = CARTESIAN_POINT ( 'NONE',  ( 0.1747926744264451659, 0.2546335194838904581, -1.890750172325323275 ) ) ;
#120470 = CARTESIAN_POINT ( 'NONE',  ( 6.081407632663145435, 1.356090666932512789, -1.492028312255622824 ) ) ;
#120471 = CARTESIAN_POINT ( 'NONE',  ( 5.682812683241409424, 1.562005318756795713, -1.108807820749290851 ) ) ;
#120472 = CYLINDRICAL_SURFACE ( 'NONE', #79440, 11.09999999999999964 ) ;
#120473 = CARTESIAN_POINT ( 'NONE',  ( 3.474349307649237328, -2.112600797985896950, -0.5827812199917583591 ) ) ;
#120474 = CARTESIAN_POINT ( 'NONE',  ( -1.201851678989727383E-14, 2.493750000682819046, 1.732050807568877637 ) ) ;
#120475 = CARTESIAN_POINT ( 'NONE',  ( 2.882959773793275726, -1.768624019741386277, -0.7279546805132871556 ) ) ;
#120476 = CARTESIAN_POINT ( 'NONE',  ( -6.091691091241777656, 6.001394449403842479, 0.7998128361456341429 ) ) ;
#120477 = CARTESIAN_POINT ( 'NONE',  ( 5.788968402910816380, 5.856144012925152076, 0.7216878364870317197 ) ) ;
#120479 = CARTESIAN_POINT ( 'NONE',  ( 1.247672978039487734, 1.986097573956084439, -0.3474914183895366215 ) ) ;
#120478 = DIRECTION ( 'NONE',  ( 5.578564026256491869E-16, 1.000000000000000000, 9.066213480720160632E-32 ) ) ;
#120480 = B_SPLINE_CURVE_WITH_KNOTS ( 'NONE', 3,
 ( #84944, #20982, #131622, #101186 ),
 .UNSPECIFIED., .F., .F.,
 ( 4, 4 ),
 ( 3.104682540415231782E-18, 5.209409853017606958E-06 ),
 .UNSPECIFIED. ) ;
#120481 = CARTESIAN_POINT ( 'NONE',  ( -1.364683531250010295, 11.19270833367473550, 0.7879004041258445001 ) ) ;
#120483 = CARTESIAN_POINT ( 'NONE',  ( -3.657667580636712934, 7.489305620709952649, -0.7998128361456481317 ) ) ;
#120482 = CARTESIAN_POINT ( 'NONE',  ( 6.339412547452306868, 0.8406370108028878851, -2.024118718474729128 ) ) ;
#120485 = ORIENTED_EDGE ( 'NONE', *, *, #145044, .F. ) ;
#120484 = CARTESIAN_POINT ( 'NONE',  ( 2.906937612971383089, 1.455985047528246090, 0.9243032718214757582 ) ) ;
#120486 = CARTESIAN_POINT ( 'NONE',  ( 0.1405533004714383249, 7.629137130509051623, -2.879722665736083709 ) ) ;
#120487 = CARTESIAN_POINT ( 'NONE',  ( 8.132193210098487057, 8.381980254736715708, 1.040834085586084257E-14 ) ) ;
#120488 = CARTESIAN_POINT ( 'NONE',  ( 4.310602774141044868, 7.116454772218158809, -1.199719254218452047 ) ) ;
#120489 = DIRECTION ( 'NONE',  ( -0.000000000000000000, 0.000000000000000000, -1.000000000000000000 ) ) ;
#120490 = CARTESIAN_POINT ( 'NONE',  ( 1.187862215860764126, -1.241893603568875903, -1.518774446641702580 ) ) ;
#120491 =( NAMED_UNIT ( * ) PLANE_ANGLE_UNIT ( ) SI_UNIT ( $, .RADIAN. ) );
#120492 = CARTESIAN_POINT ( 'NONE',  ( 3.683011284406639607, 7.448596931783069586, 0.7998128361456321445 ) ) ;
#120493 = CARTESIAN_POINT ( 'NONE',  ( -1.500000000000008216, 10.74999999999999645, 3.469446951953614189E-15 ) ) ;
#120494 = VERTEX_POINT ( 'NONE', #151933 ) ;
#120495 = CIRCLE ( 'NONE', #16637, 0.08000000000000032085 ) ;
#120496 = DIRECTION ( 'NONE',  ( 0.000000000000000000, 1.000000000000000000, 0.000000000000000000 ) ) ;
#120497 = EDGE_CURVE ( 'NONE', #116248, #49891, #118424, .T. ) ;
#120498 = ORIENTED_EDGE ( 'NONE', *, *, #14173, .T. ) ;
#120499 = CARTESIAN_POINT ( 'NONE',  ( 4.389189793862141364, -0.004542125399705549196, -1.811656973097997447 ) ) ;
#120500 = ORIENTED_EDGE ( 'NONE', *, *, #13528, .F. ) ;
#120501 = CARTESIAN_POINT ( 'NONE',  ( 8.594979316059474073, 12.11489407112305372, 1.199719254218450271 ) ) ;
#120502 = CARTESIAN_POINT ( 'NONE',  ( -5.425723655374722121, 6.121007837424875753, 1.095972955597510401 ) ) ;
#120503 = CARTESIAN_POINT ( 'NONE',  ( 4.529823624924778969, -1.775545877285337193, 0.3580350944670795399 ) ) ;
#120504 = CARTESIAN_POINT ( 'NONE',  ( 7.648208051440442468, 8.095533279534887328, 0.000000000000000000 ) ) ;
#120505 = CARTESIAN_POINT ( 'NONE',  ( 5.611280047485872835, 6.151892252731265387, -0.8436193503846599606 ) ) ;
#120507 = CARTESIAN_POINT ( 'NONE',  ( -0.6823417656250039265, 15.06770833367473195, -1.181850606188755259 ) ) ;
#120506 = CARTESIAN_POINT ( 'NONE',  ( 5.617585446245374037, 0.3627780356338809464, -1.825160902907280613 ) ) ;
#120508 = CARTESIAN_POINT ( 'NONE',  ( 2.442874106818424096, -1.667949397242382448, -0.9418811778915718858 ) ) ;
#120509 = CARTESIAN_POINT ( 'NONE',  ( -6.608557002163582439, -8.105676417795779187, -6.825099317097834017 ) ) ;
#120510 = CARTESIAN_POINT ( 'NONE',  ( -10.97400665845581536, 4.893988168282350948, 4.351071648605314479 ) ) ;
#120511 = DIRECTION ( 'NONE',  ( 1.000000000000000000, -7.387867266669436732E-31, 0.000000000000000000 ) ) ;
#120512 = CARTESIAN_POINT ( 'NONE',  ( 8.297226821883377568, 8.782445501726501291, -0.7216878364870267237 ) ) ;
#120513 = CARTESIAN_POINT ( 'NONE',  ( -3.521367211247373508, 5.131347717920458962, -1.599625672291256295 ) ) ;
#120514 = DIRECTION ( 'NONE',  ( 0.000000000000000000, 0.000000000000000000, -1.000000000000000000 ) ) ;
#120515 = CARTESIAN_POINT ( 'NONE',  ( 1.306708042577527262, 1.844576602789575137, 0.9840055123579400931 ) ) ;
#120516 = CARTESIAN_POINT ( 'NONE',  ( 4.369470645354133431, 8.319742529546998000, 0.7998128361456271485 ) ) ;
#120517 = CARTESIAN_POINT ( 'NONE',  ( 6.088885551643496541, -0.2832829338282101261, -1.905325039026314560 ) ) ;
#120518 = CARTESIAN_POINT ( 'NONE',  ( -3.730464822054482710, 7.503959392372201442, 1.040834085586084257E-14 ) ) ;
#120519 = CARTESIAN_POINT ( 'NONE',  ( 2.731258071184277103, -1.704167518380688140, 0.6551187846031494288 ) ) ;
#120520 = CARTESIAN_POINT ( 'NONE',  ( 9.780965096007749437, 12.99495041104594861, 8.039825270927440926 ) ) ;
#120521 = CARTESIAN_POINT ( 'NONE',  ( 2.109489925670060551, 1.480643174185194200, 1.210387159491378650 ) ) ;
#120522 = CARTESIAN_POINT ( 'NONE',  ( 2.101947443238092017, 0.7566099462053441638, -1.818632640566263614 ) ) ;
#120523 = CARTESIAN_POINT ( 'NONE',  ( 3.351055748958339908, 0.4689680007726776401, -1.884483806560928398 ) ) ;
#120524 = ORIENTED_EDGE ( 'NONE', *, *, #131051, .T. ) ;
#120525 = CARTESIAN_POINT ( 'NONE',  ( -0.1000000000000028644, -9.919999999999998153, -9.579478065113972818 ) ) ;
#120526 = CARTESIAN_POINT ( 'NONE',  ( -5.517242166118370150, 5.401480380085008193, 0.7998128361456281477 ) ) ;
#120528 = CARTESIAN_POINT ( 'NONE',  ( 3.832379111121624327, -1.093062754469842579, -1.817066923117337751 ) ) ;
#120527 = CARTESIAN_POINT ( 'NONE',  ( 4.248501033035879004, 6.049946853332221153, -1.599625672291273171 ) ) ;
#120529 = CARTESIAN_POINT ( 'NONE',  ( -10.51582573219070227, 13.61290858478269605, 3.554376768052134317 ) ) ;
#120530 = CARTESIAN_POINT ( 'NONE',  ( 9.935427640716063991, 10.48575375712389679, -0.7998128361456281477 ) ) ;
#120531 = B_SPLINE_CURVE_WITH_KNOTS ( 'NONE', 3,
 ( #72558, #74709, #71479, #22727, #171134, #75773, #106193 ),
 .UNSPECIFIED., .F., .F.,
 ( 4, 3, 4 ),
 ( 0.0001932293135873497478, 0.0009000000018422023643, 0.002089330742406760120 ),
 .UNSPECIFIED. ) ;
#120532 = CARTESIAN_POINT ( 'NONE',  ( 5.670051627282618689, 6.304626411287498122, 1.111461560052000586 ) ) ;
#120533 = CARTESIAN_POINT ( 'NONE',  ( 3.006787879153326681, 6.373552747333731006, -0.4818892653130519843 ) ) ;
#120534 = ORIENTED_EDGE ( 'NONE', *, *, #52153, .F. ) ;
#120535 = VECTOR ( 'NONE', #12704, 1000.000000000000000 ) ;
#120536 = CARTESIAN_POINT ( 'NONE',  ( 5.664274315459256748, 9.830346811336296398, -0.7998128361456481317 ) ) ;
#120537 = CARTESIAN_POINT ( 'NONE',  ( 0.000000000000000000, 0.000000000000000000, 0.000000000000000000 ) ) ;
#120538 = CARTESIAN_POINT ( 'NONE',  ( 3.756323439517950558, 0.6585720284536450420, 1.702948436616057881 ) ) ;
#120539 = CARTESIAN_POINT ( 'NONE',  ( 10.99960280095051779, -9.919999999999998153, -0.09350563796401789585 ) ) ;
#120540 = CARTESIAN_POINT ( 'NONE',  ( -8.948018195339354719, 12.42280974699582607, 1.082531754730560403 ) ) ;
#120541 = CARTESIAN_POINT ( 'NONE',  ( -4.651396499164954790, 8.416516698401213858, 0.5247324002638984464 ) ) ;
#120542 = DIRECTION ( 'NONE',  ( -1.000000000000000000, 0.000000000000000000, 0.000000000000000000 ) ) ;
#120543 = CARTESIAN_POINT ( 'NONE',  ( 4.715616592392388284, -1.834479983729628616, 0.3652084810651031743 ) ) ;
#120544 = CARTESIAN_POINT ( 'NONE',  ( 6.726816770674637347, 10.99970333242910669, -0.7998128361456291469 ) ) ;
#120545 = CARTESIAN_POINT ( 'NONE',  ( 1.822755070894378271, 1.797457900398396813, 0.6936678961073846628 ) ) ;
#120546 = CARTESIAN_POINT ( 'NONE',  ( 6.561383603009730336, 1.629167342741120406, 1.092533971175007723 ) ) ;
#120547 = EDGE_CURVE ( 'NONE', #87461, #159016, #184995, .T. ) ;
#120548 = CARTESIAN_POINT ( 'NONE',  ( 1.364683531250000303, 8.817708333674731946, -0.7879004041258355073 ) ) ;
#120549 = CARTESIAN_POINT ( 'NONE',  ( -7.250913225210214641, 7.353820272367037170, 0.7998128361456341429 ) ) ;
#120550 = CARTESIAN_POINT ( 'NONE',  ( 3.323720213644492993, 7.029424015893889433, 1.040834085586084257E-14 ) ) ;
#120551 = CARTESIAN_POINT ( 'NONE',  ( -5.004368096775595021, 5.971422546727199077, 1.082531754730549078 ) ) ;
#120552 = CARTESIAN_POINT ( 'NONE',  ( 1.195080948601736859, 1.869106744463861158, 0.9945057017613133654 ) ) ;
#120553 = CARTESIAN_POINT ( 'NONE',  ( -3.099101127474140682, 6.559442382121059900, -0.4367601086740290350 ) ) ;
#120554 = CARTESIAN_POINT ( 'NONE',  ( 0.1144128442232072856, 7.018241394332943806, 3.990988525777207752 ) ) ;
#120555 = CARTESIAN_POINT ( 'NONE',  ( 4.856339096887199780, -2.069677458173447171, -0.05615216265978521804 ) ) ;
#120557 = CARTESIAN_POINT ( 'NONE',  ( 4.472818454536469090, 7.041451798021368447, -1.136577435397856384 ) ) ;
#120556 = CARTESIAN_POINT ( 'NONE',  ( 0.7316835000789992938, 1.813914744281470925, 0.3150931809976220133 ) ) ;
#120558 = EDGE_LOOP ( 'NONE', ( #199507, #86649, #37881, #185894 ) ) ;
#120559 = CARTESIAN_POINT ( 'NONE',  ( 5.678471694547736703, 1.738760799997655537, 1.503693327295371862 ) ) ;
#120560 = CARTESIAN_POINT ( 'NONE',  ( 6.805829924380108586, 8.963220883242035697, 1.443375672974076540 ) ) ;
#120562 =( NAMED_UNIT ( * ) PLANE_ANGLE_UNIT ( ) SI_UNIT ( $, .RADIAN. ) );
#120561 = CARTESIAN_POINT ( 'NONE',  ( 3.879041347285658414, 6.579279767591636130, -1.082531754730548412 ) ) ;
#120563 = B_SPLINE_CURVE_WITH_KNOTS ( 'NONE', 3,
 ( #182153, #197348, #147556, #183231, #84669, #33783, #98803, #213578 ),
 .UNSPECIFIED., .F., .F.,
 ( 4, 2, 2, 4 ),
 ( 4.982613841084584701E-18, 0.0002034531274099235997, 0.0004069062548198428084, 0.0008138125096396765096 ),
 .UNSPECIFIED. ) ;
#120564 = CARTESIAN_POINT ( 'NONE',  ( 1.447684683128658278, 0.6615928844308440748, -2.194714443420691552 ) ) ;
#120565 = LINE ( 'NONE', #204905, #202451 ) ;
#120566 = CARTESIAN_POINT ( 'NONE',  ( -6.934069218746458318, 7.054445274817795486, -0.7998128361456362523 ) ) ;
#120567 = CARTESIAN_POINT ( 'NONE',  ( 5.912047867262844925, 1.302452500554865722, -1.440575834569270519 ) ) ;
#120568 = ORIENTED_EDGE ( 'NONE', *, *, #112880, .F. ) ;
#120569 = CARTESIAN_POINT ( 'NONE',  ( 8.229436053370676518, 9.663725486096376827, 1.082531754730558626 ) ) ;
#120570 = EDGE_CURVE ( 'NONE', #143955, #50054, #25895, .T. ) ;
#120571 = ORIENTED_EDGE ( 'NONE', *, *, #181980, .T. ) ;
#120572 = CARTESIAN_POINT ( 'NONE',  ( 6.222915752822945734, 1.412394824171304908, -1.289504995239741714 ) ) ;
#120573 = CARTESIAN_POINT ( 'NONE',  ( -10.63367255181986160, 11.30037282007833532, 1.040834085586084257E-14 ) ) ;
#120575 = CARTESIAN_POINT ( 'NONE',  ( 7.084367489069545069E-14, 8.210952333604106812, 2.038660652713624177 ) ) ;
#120574 = CARTESIAN_POINT ( 'NONE',  ( -8.474009703741204547, 9.845098394908269768, -1.199719254218446718 ) ) ;
#120576 = CARTESIAN_POINT ( 'NONE',  ( -3.285556943750000514, -1.976041666188710577, -1.896917185911906500 ) ) ;
#120578 = CARTESIAN_POINT ( 'NONE',  ( 1.076598688339102772, -0.03801472141184288056, -1.769612961288852926 ) ) ;
#120577 = CARTESIAN_POINT ( 'NONE',  ( 2.537156728381038118, -1.549654062961543177, -1.403521045075975415 ) ) ;
#120579 = CARTESIAN_POINT ( 'NONE',  ( 6.486953984781112403, -2.015912550161761629, 0.05229459904129707404 ) ) ;
#120581 = CARTESIAN_POINT ( 'NONE',  ( 3.785359544849807190, 1.659571404495253866, 1.581462771572618609 ) ) ;
#120580 = DIRECTION ( 'NONE',  ( -0.000000000000000000, -1.000000000000000000, -0.000000000000000000 ) ) ;
#120582 = CARTESIAN_POINT ( 'NONE',  ( 2.958654558096874609, 0.2547609298257165200, -1.721438497358678932 ) ) ;
#120583 = CARTESIAN_POINT ( 'NONE',  ( 8.367353357928214663, 12.91366268422496688, 1.040834085586084257E-14 ) ) ;
#120584 = CARTESIAN_POINT ( 'NONE',  ( -4.896959554461132846, 4.880740138633571590, -0.5902973598261325172 ) ) ;
#120585 = CARTESIAN_POINT ( 'NONE',  ( 3.356526315702735186, -0.7047320765170405066, 1.584360681437890550 ) ) ;
#120586 = CARTESIAN_POINT ( 'NONE',  ( 3.367796644333774569, -0.4264072692300807099, 2.128736309618290079 ) ) ;
#120587 = CARTESIAN_POINT ( 'NONE',  ( 5.684946482831785275, 5.526859072925533134, -0.7998128361456231517 ) ) ;
#120588 = CARTESIAN_POINT ( 'NONE',  ( 4.294157853547872605, -0.8666056138363428252, -1.820986994602634024 ) ) ;
#120589 = CARTESIAN_POINT ( 'NONE',  ( 2.000000000000001332, -1.212302805901314492E-13, -2.052068128417949389 ) ) ;
#120590 = CIRCLE ( 'NONE', #82466, 2.000000000000000000 ) ;
#120591 = CARTESIAN_POINT ( 'NONE',  ( -1.402160292154681736E-14, 2.368750000682818602, -1.732050807568863648 ) ) ;
#120592 = CARTESIAN_POINT ( 'NONE',  ( 1.430555067506549483, 1.855864167146383581, 0.5162276523679990570 ) ) ;
#120593 = CARTESIAN_POINT ( 'NONE',  ( 0.7500000000000006661, 8.947916667349467446, -1.299038105676657340 ) ) ;
#120594 = CARTESIAN_POINT ( 'NONE',  ( 4.447658085050952614, -2.030299463072975819, 0.9018405843745944672 ) ) ;
#120595 = ORIENTED_EDGE ( 'NONE', *, *, #180391, .T. ) ;
#120596 = CARTESIAN_POINT ( 'NONE',  ( -0.2106854629475400364, 0.7093903261615883693, -2.078205123749873984 ) ) ;
#120597 = CARTESIAN_POINT ( 'NONE',  ( 0.7499999999999885647, 2.316666666666689078, -1.299038105676652899 ) ) ;
#120598 = CARTESIAN_POINT ( 'NONE',  ( 6.103141704446003679, 10.27208242182903142, 0.7998128361456462443 ) ) ;
#120599 = CARTESIAN_POINT ( 'NONE',  ( 3.945059511452237100, 6.586024615794168646, -1.082531754730548412 ) ) ;
#120600 = CARTESIAN_POINT ( 'NONE',  ( 3.285556943749998737, -1.305208332855376296, -1.896917185911906722 ) ) ;
#120601 = CARTESIAN_POINT ( 'NONE',  ( 0.4697634657386277612, -1.879787550458272394, -1.183196895768683365 ) ) ;
#120602 = CARTESIAN_POINT ( 'NONE',  ( 5.389097038490845648, 0.1425914310585977562, 1.956722230749982971 ) ) ;
#120603 = CARTESIAN_POINT ( 'NONE',  ( 8.595506201384004896, 12.01154575404795466, 1.082531754730546636 ) ) ;
#120604 = CARTESIAN_POINT ( 'NONE',  ( -11.41267819554183127, 3.447199233515635619, 3.708203932499423150 ) ) ;
#120605 = CARTESIAN_POINT ( 'NONE',  ( 0.5093243970649004027, 1.880507610096779025, 1.065828983023514809 ) ) ;
#120606 = CIRCLE ( 'NONE', #165505, 12.00000000000000178 ) ;
#120607 = CARTESIAN_POINT ( 'NONE',  ( -4.448483799059637533, 7.243629294661272588, 1.082531754730549967 ) ) ;
#120608 = CARTESIAN_POINT ( 'NONE',  ( 3.297386996040070795, -1.820318649397782318, 0.9700563119749375796 ) ) ;
#120609 = CARTESIAN_POINT ( 'NONE',  ( -5.199715606040888005, 6.025088614257851027, -1.199719254218446718 ) ) ;
#120610 = CARTESIAN_POINT ( 'NONE',  ( -0.7499999999999972244, 4.139583334016149863, -1.299038105676652899 ) ) ;
#120611 = CARTESIAN_POINT ( 'NONE',  ( -0.6823417656249969321, 4.780208333674755394, -1.181850606188749264 ) ) ;
#120612 = CARTESIAN_POINT ( 'NONE',  ( 4.956247902659736582, 0.7144662795386286236, 1.728917671469521800 ) ) ;
#120613 = CARTESIAN_POINT ( 'NONE',  ( 3.920349067101033036, -1.199671410015031192, -1.252466492151423694 ) ) ;
#120614 = CARTESIAN_POINT ( 'NONE',  ( 3.913389451132457619, -0.8987009378256786141, -1.490314472085547237 ) ) ;
#120615 = CARTESIAN_POINT ( 'NONE',  ( 1.066458480799619135, -1.449176446249898831, 1.776219484066744903 ) ) ;
#120616 = CARTESIAN_POINT ( 'NONE',  ( -1.001543065824772872E-14, 4.384375000341417916, 1.575800808251672791 ) ) ;
#120617 = CARTESIAN_POINT ( 'NONE',  ( 4.634370609685579900, 0.3589238887658425248, 2.059545865661859931 ) ) ;
#120618 = CARTESIAN_POINT ( 'NONE',  ( 0.2515690823673248921, 0.7017594223384625574, 1.702352774230586618 ) ) ;
#120619 = CARTESIAN_POINT ( 'NONE',  ( 4.207966135563078858, 7.175396087857926375, 7.500000000000000000 ) ) ;
#120620 = SURFACE_STYLE_FILL_AREA ( #40375 ) ;
#120621 = CARTESIAN_POINT ( 'NONE',  ( 2.180314765559120183, 1.560501322096979449, 1.277041908422072991 ) ) ;
#120622 = EDGE_CURVE ( 'NONE', #116561, #162002, #19777, .T. ) ;
#120623 = CARTESIAN_POINT ( 'NONE',  ( -4.731432421044877934, 6.543090462684225450, -1.443375672974051449 ) ) ;
#120624 = CARTESIAN_POINT ( 'NONE',  ( 9.664668247050562044, 13.51658191024029243, -8.185676666504042132 ) ) ;
#120625 = CARTESIAN_POINT ( 'NONE',  ( -6.852756576703439961, 10.08230087520760954, 1.199719254218453823 ) ) ;
#120626 = CARTESIAN_POINT ( 'NONE',  ( 7.318703993278529829, 7.432909501780090800, 1.040834085586084257E-14 ) ) ;
#120627 = CARTESIAN_POINT ( 'NONE',  ( 2.227333921462580246, 1.895369558270381338, 0.9509248740046101211 ) ) ;
#120628 = DIRECTION ( 'NONE',  ( 0.000000000000000000, 0.000000000000000000, 1.000000000000000000 ) ) ;
#120629 = CARTESIAN_POINT ( 'NONE',  ( 5.303274670167754223, 1.494737065598227943, 1.048009559513597866 ) ) ;
#120630 = EDGE_LOOP ( 'NONE', ( #54048, #68869, #197933, #110784 ) ) ;
#120631 = CARTESIAN_POINT ( 'NONE',  ( -6.903036488013351679, 8.082572653217566128, -1.199719254218452047 ) ) ;
#120632 = CARTESIAN_POINT ( 'NONE',  ( -4.907688418022547516, 4.827984030555475314, 1.214306433183764966E-14 ) ) ;
#120633 = CARTESIAN_POINT ( 'NONE',  ( 3.285556943750000070, -1.421874999522041660, 0.000000000000000000 ) ) ;
#120634 = CARTESIAN_POINT ( 'NONE',  ( -7.691553217654356622, 7.867900263551875994, -0.7998128361456291469 ) ) ;
#120635 = CARTESIAN_POINT ( 'NONE',  ( 2.056904690034748739, 0.4466968674397324701, 1.969590803855451933 ) ) ;
#120636 = CARTESIAN_POINT ( 'NONE',  ( 5.122202071631626552, -1.176711583861598243, -1.866687997650509079 ) ) ;
#120637 = CARTESIAN_POINT ( 'NONE',  ( -2.972980823146582186, 6.690504403638126263, 0.000000000000000000 ) ) ;
#120638 = CARTESIAN_POINT ( 'NONE',  ( 3.748742453178009360, -0.3589989779783793744, -1.825800159725386118 ) ) ;
#120639 = CARTESIAN_POINT ( 'NONE',  ( 8.028399517586572998, 12.51821653715971472, -0.7998128361456352531 ) ) ;
#120640 = PLANE ( 'NONE',  #140521 ) ;
#120641 = CARTESIAN_POINT ( 'NONE',  ( -5.264643720808155791, 5.036505850564608089, 0.000000000000000000 ) ) ;
#120642 = CARTESIAN_POINT ( 'NONE',  ( -7.320512876374914768, 10.62801655815766999, 1.199719254218453823 ) ) ;
#120643 = CARTESIAN_POINT ( 'NONE',  ( 5.443921307256319508, 0.7362202147598860824, -1.670853202368662860 ) ) ;
#120645 = CARTESIAN_POINT ( 'NONE',  ( -4.301340604499551468, 7.447936736316801642, -1.117465989868490883 ) ) ;
#120644 = CARTESIAN_POINT ( 'NONE',  ( -3.142457743317409680, 6.888227477170756785, 0.7998128361456352531 ) ) ;
#120646 = CARTESIAN_POINT ( 'NONE',  ( -0.6823417656250003738, -0.5322916663252491576, -1.181850606188749264 ) ) ;
#120647 = CARTESIAN_POINT ( 'NONE',  ( 0.6668559383766320403, -0.5766704339003425606, -1.635293367498649397 ) ) ;
#120648 = CARTESIAN_POINT ( 'NONE',  ( 0.3744471653823171486, 1.625640304646416734, -0.6218004557168725910 ) ) ;
#120649 = CARTESIAN_POINT ( 'NONE',  ( 6.059233210108489587, -1.975957287588899769, -1.191867793525339669 ) ) ;
#120650 = CARTESIAN_POINT ( 'NONE',  ( 2.878073747850912412, 6.579779482459851003, -0.7998128361456362523 ) ) ;
#120651 = CARTESIAN_POINT ( 'NONE',  ( 1.722021792205346902, -1.142311743720581196, -1.714993188781144928 ) ) ;
#120652 = CARTESIAN_POINT ( 'NONE',  ( 4.482942347612929979, 8.381849838857084123, 1.040834085586084257E-14 ) ) ;
#120653 = CIRCLE ( 'NONE', #151656, 0.2000000000000005107 ) ;
#120654 = CARTESIAN_POINT ( 'NONE',  ( 0.1751529202326657098, -0.8592662624449104447, -1.822031250676876768 ) ) ;
#120655 = CARTESIAN_POINT ( 'NONE',  ( 1.499999999999996891, 11.42708333401612997, -0.8660254037844378194 ) ) ;
#120656 = CARTESIAN_POINT ( 'NONE',  ( -6.343235766347277149, 8.493804042195527870, -1.599625672291271394 ) ) ;
#120657 = CARTESIAN_POINT ( 'NONE',  ( 5.576977133510579776, -0.04717937999037385977, -1.870219006134994588 ) ) ;
#120659 = CARTESIAN_POINT ( 'NONE',  ( -3.311934663488232733, 7.085950550703385531, -0.7998128361456481317 ) ) ;
#120658 = CARTESIAN_POINT ( 'NONE',  ( 4.043146078444789460, 0.09904687726844901841, 1.909973672635330910 ) ) ;
#120660 = CARTESIAN_POINT ( 'NONE',  ( 4.530015419921377351, -1.356323209173672106, -1.740806116466916409 ) ) ;
#120661 = CARTESIAN_POINT ( 'NONE',  ( 0.6124999999999707345, 1.395833334016133298, 1.060881119635904923 ) ) ;
#120662 = EDGE_CURVE ( 'NONE', #12413, #187007, #98593, .T. ) ;
#120663 = CARTESIAN_POINT ( 'NONE',  ( -6.522881301506166629, 9.663759714182251770, 1.082531754730549967 ) ) ;
#120664 = CARTESIAN_POINT ( 'NONE',  ( 4.163762572728282763, 6.911454530608037494, -1.082531754730548412 ) ) ;
#120665 = CARTESIAN_POINT ( 'NONE',  ( -4.136646265500958819, 7.840188053144158786, -0.7216878364870458196 ) ) ;
#120666 = CARTESIAN_POINT ( 'NONE',  ( 5.795592431653455279, 1.959276243578732091, -0.8114611383256833399 ) ) ;
#120667 = EDGE_LOOP ( 'NONE', ( #71666, #209868, #20945, #127419 ) ) ;
#120668 = CARTESIAN_POINT ( 'NONE',  ( 3.593080373992099119, -0.4475695053229776788, -2.263611109821815681 ) ) ;
#120669 = CARTESIAN_POINT ( 'NONE',  ( 3.596105239937871456, 0.8843387906064968940, -1.751336483779348585 ) ) ;
#120670 = CARTESIAN_POINT ( 'NONE',  ( -4.125423880308188629, 8.035021303660013103, -0.7998128361456481317 ) ) ;
#120671 = CARTESIAN_POINT ( 'NONE',  ( 1.164813196467245904, 1.489159823276710926, -1.277213275948145599 ) ) ;
#120672 = CARTESIAN_POINT ( 'NONE',  ( 8.665088397661675046, 14.86833811616255119, 8.238078554563339040 ) ) ;
#120673 = CARTESIAN_POINT ( 'NONE',  ( 4.927462483923885195, 4.713404084191450849, -0.7998128361456481317 ) ) ;
#120674 = VERTEX_POINT ( 'NONE', #104253 ) ;
#120675 = CARTESIAN_POINT ( 'NONE',  ( 5.964077395145578109, -1.074666730956087335, 1.706109649615504154 ) ) ;
#120676 = CARTESIAN_POINT ( 'NONE',  ( -8.272446282632566650, 12.80293776304669962, 0.7998128361456481317 ) ) ;
#120677 = PRESENTATION_STYLE_ASSIGNMENT (( #202884 ) ) ;
#120678 = CARTESIAN_POINT ( 'NONE',  ( 3.221698175004498399, 0.3232067185854271552, -2.146787281877101439 ) ) ;
#120679 = CARTESIAN_POINT ( 'NONE',  ( 4.529305835417093640, 7.441884687032027657, -1.199719254218450271 ) ) ;
#120681 = EDGE_CURVE ( 'NONE', #59570, #193391, #47797, .T. ) ;
#120680 = CARTESIAN_POINT ( 'NONE',  ( 0.7035762090183244055, 1.867434778015097940, -1.004864118554361863 ) ) ;
#120682 = CARTESIAN_POINT ( 'NONE',  ( 0.7499999999999885647, 1.347916667349485786, -1.299038105676652899 ) ) ;
#120683 = CARTESIAN_POINT ( 'NONE',  ( 8.920375002787457319, 12.49452237230570084, 1.199719254218450271 ) ) ;
#120684 = CARTESIAN_POINT ( 'NONE',  ( 1.863054968392299671, 2.484104531656126102, 2.477705830955055699 ) ) ;
#120685 = CARTESIAN_POINT ( 'NONE',  ( 4.831949485534527966, 8.212610664285437068, 0.9193987405316924599 ) ) ;
#120686 = CARTESIAN_POINT ( 'NONE',  ( 1.352885421680804834, -1.626251134426279332, 1.265669239494594311 ) ) ;
#120688 = DIRECTION ( 'NONE',  ( 0.000000000000000000, 0.000000000000000000, -1.000000000000000000 ) ) ;
#120687 = CARTESIAN_POINT ( 'NONE',  ( -8.469039510030723861, 13.03229652834454733, 1.040834085586084257E-14 ) ) ;
#120689 = CARTESIAN_POINT ( 'NONE',  ( -1.364683531250014514, 1.488541667008084435, -0.7879004041258289570 ) ) ;
#120690 = PRESENTATION_STYLE_ASSIGNMENT (( #55609 ) ) ;
#120691 = VERTEX_POINT ( 'NONE', #187615 ) ;
#120692 = CARTESIAN_POINT ( 'NONE',  ( 4.389254143344611947, -0.003399479254035177832, -1.912461472815998542 ) ) ;
#120693 = B_SPLINE_CURVE_WITH_KNOTS ( 'NONE', 3,
 ( #196236, #53176, #71533, #88894, #73688, #119304, #69398 ),
 .UNSPECIFIED., .F., .F.,
 ( 4, 3, 4 ),
 ( 0.000000000000000000, 3.004831683896754227E-05, 4.142468191938748892E-05 ),
 .UNSPECIFIED. ) ;
#120694 = CARTESIAN_POINT ( 'NONE',  ( 4.996827606291168955, 1.470251540571869020, -0.9849021259363596181 ) ) ;
#120695 = CARTESIAN_POINT ( 'NONE',  ( 6.200875153403774043, 8.327716660428123419, -1.599625672291283607 ) ) ;
#120696 = CARTESIAN_POINT ( 'NONE',  ( -2.740719608256871442, 6.349256642941639051, 0.7998128361456341429 ) ) ;
#120697 = CARTESIAN_POINT ( 'NONE',  ( 0.1580966392830873424, 1.806712829659435027, 0.1331060069221217668 ) ) ;
#120699 = CARTESIAN_POINT ( 'NONE',  ( 1.129944905810562839, 1.913687095308055808, 0.09034645858918381733 ) ) ;
#120698 = CARTESIAN_POINT ( 'NONE',  ( -0.5087312005655101332, 6.815231585927279845, -3.595452205664221079 ) ) ;
#120700 = CARTESIAN_POINT ( 'NONE',  ( 2.225130849662222410, -1.891980959128433781, -0.8411517639917851508 ) ) ;
#120701 = CARTESIAN_POINT ( 'NONE',  ( -1.364683531250014514, 0.3010416670080866552, -0.7879004041258359514 ) ) ;
#120702 = CARTESIAN_POINT ( 'NONE',  ( 0.8835904138565253696, 1.322268204680861814, 1.462458760404183433 ) ) ;
#120703 = CARTESIAN_POINT ( 'NONE',  ( 2.578497204056416692, -1.747032809129964503, -0.5301130021647950663 ) ) ;
#120705 = CARTESIAN_POINT ( 'NONE',  ( 5.355423173304108886, 7.585870477640591858, 1.239999553246450725 ) ) ;
#120704 = CARTESIAN_POINT ( 'NONE',  ( 0.08326089795122111614, -2.240168680488762387, -0.5538300120674977123 ) ) ;
#120706 = CARTESIAN_POINT ( 'NONE',  ( -1.201851678989727383E-14, 0.8218750003414171390, 1.575800808251672791 ) ) ;
#120707 = CARTESIAN_POINT ( 'NONE',  ( 4.018078825213769356, 2.047437054436978876, -0.2496575186523365686 ) ) ;
#120708 = CARTESIAN_POINT ( 'NONE',  ( -7.237355071596549116, 7.338002426484427687, 1.040834085586084257E-14 ) ) ;
#120709 = CARTESIAN_POINT ( 'NONE',  ( 6.889514614038635187, 11.18951748302043114, -0.7998128361456291469 ) ) ;
#120710 = CARTESIAN_POINT ( 'NONE',  ( 5.705283713252285338, 5.550585841749445137, -0.7998128361456211532 ) ) ;
#120712 = EDGE_CURVE ( 'NONE', #78732, #121840, #210412, .T. ) ;
#120711 =( BOUNDED_CURVE ( )  B_SPLINE_CURVE ( 2, ( #71966, #40581, #39494, #154320, #186801 ),
 .UNSPECIFIED., .F., .T. ) 
 B_SPLINE_CURVE_WITH_KNOTS ( ( 3, 2, 3 ),
 ( 0.2625000001274112038, 0.2666666666666666075, 0.2749999999999999112 ),
 .UNSPECIFIED. ) 
 CURVE ( )  GEOMETRIC_REPRESENTATION_ITEM ( )  RATIONAL_B_SPLINE_CURVE ( ( 0.9330127018922194093, 0.9330127039406028722, 1.000000000000000000, 0.8660254037844404840, 0.9999999999999982236 ) ) 
 REPRESENTATION_ITEM ( '' )  );
#120713 = CARTESIAN_POINT ( 'NONE',  ( 5.656776405399742025, 7.622658444431597680, -1.599625672291262513 ) ) ;
#120715 = CARTESIAN_POINT ( 'NONE',  ( -1.499999999999997780, 4.150000000000021672, 1.214306433183764966E-14 ) ) ;
#120714 = CARTESIAN_POINT ( 'NONE',  ( 5.192451847192011805, -2.089709803398311028, -0.2606072588380181076 ) ) ;
#120716 = CARTESIAN_POINT ( 'NONE',  ( 6.180147188013234150, -1.146869210499700920, -1.723488058659912392 ) ) ;
#120717 = CARTESIAN_POINT ( 'NONE',  ( -1.364683531250014514, 1.051041667008090208, -0.7879004041258289570 ) ) ;
#120718 = CARTESIAN_POINT ( 'NONE',  ( 3.743588348364734752, -1.634107004491680115, -1.415051943026650161 ) ) ;
#120719 = CARTESIAN_POINT ( 'NONE',  ( 4.828773858256512064, 1.391243881446821762, -1.464325142460545459 ) ) ;
#120720 = CARTESIAN_POINT ( 'NONE',  ( 6.620655732516648406, 3.679503859435423241, 2.787618683092321969 ) ) ;
#120723 = CARTESIAN_POINT ( 'NONE',  ( 5.016153647376196290, 8.796003655340152605, 0.7216878364870438212 ) ) ;
#120722 = CARTESIAN_POINT ( 'NONE',  ( 1.642778471875001811, -3.142708332855375986, 2.845375778867859751 ) ) ;
#120721 = CARTESIAN_POINT ( 'NONE',  ( 4.147109113946162218, 7.227559249243857842, -0.9911899289537524638 ) ) ;
#120724 = CARTESIAN_POINT ( 'NONE',  ( -4.769436176957319695, 8.786368983084006601, 0.7998128361456281477 ) ) ;
#120725 = CARTESIAN_POINT ( 'NONE',  ( 2.290250256651988892, -0.7762311197250795214, -1.861343989391924358 ) ) ;
#120726 = CARTESIAN_POINT ( 'NONE',  ( -6.028571859570855729, 10.18508426947466816, 0.000000000000000000 ) ) ;
#120728 = CARTESIAN_POINT ( 'NONE',  ( -4.261456902168970551, 7.437061921213615534, -1.019078666317332349 ) ) ;
#120727 = CARTESIAN_POINT ( 'NONE',  ( -4.386226389220933441, 5.076017861301227008, -1.199719254218446718 ) ) ;
#120729 = CARTESIAN_POINT ( 'NONE',  ( 0.05425791151749740499, -7.744511198441856870, -9.500000000000131450 ) ) ;
#120730 = CARTESIAN_POINT ( 'NONE',  ( 5.537344615273096515, -0.04053095765194079242, 1.912125305397804009 ) ) ;
#120731 = DIRECTION ( 'NONE',  ( 0.6716942845482062330, -1.762391939599642519E-12, 0.7408284471490506062 ) ) ;
#120733 = CARTESIAN_POINT ( 'NONE',  ( 4.130482583401101415, 0.5405105419177670401, 1.942537254285629400 ) ) ;
#120732 = CARTESIAN_POINT ( 'NONE',  ( -8.636180661780668899, 10.13826086257468795, -1.082531754730543083 ) ) ;
#120734 = CARTESIAN_POINT ( 'NONE',  ( 1.499999999999990896, 5.525000000000022560, 1.214306433183764966E-14 ) ) ;
#120735 = CARTESIAN_POINT ( 'NONE',  ( 1.364683531249997417, 8.484375000341396245, 2.602085213965210642E-15 ) ) ;
#120736 = CARTESIAN_POINT ( 'NONE',  ( 6.528329376709017140, 0.9880424216301281204, -1.413504571246849695 ) ) ;
#120737 = CARTESIAN_POINT ( 'NONE',  ( 6.062430963966053632, 7.101866208495718702, -1.199719254218452047 ) ) ;
#120739 = CARTESIAN_POINT ( 'NONE',  ( 8.167861197590044142, 8.493869250135347215, 0.000000000000000000 ) ) ;
#120738 = CARTESIAN_POINT ( 'NONE',  ( 8.351459436338029008, 10.76645531385962862, -1.443375672974063439 ) ) ;
#120740 = CARTESIAN_POINT ( 'NONE',  ( -5.233084104750526322, 5.207612331738130429, 0.000000000000000000 ) ) ;
#120741 = CARTESIAN_POINT ( 'NONE',  ( 5.518772846390051612, 1.727975122137341613, 0.7167417953098526029 ) ) ;
#120742 = CARTESIAN_POINT ( 'NONE',  ( 0.01235793338260140865, -2.012684344489227062, -0.04732037452980299846 ) ) ;
#120743 = SURFACE_STYLE_FILL_AREA ( #41569 ) ;
#120744 = CARTESIAN_POINT ( 'NONE',  ( 1.885682352965558861, -1.950755244972163904, 0.6936349442826782452 ) ) ;
#120745 = CARTESIAN_POINT ( 'NONE',  ( 8.596335327489152242E-14, -8.872104535001083647, -9.837524982414047159 ) ) ;
#120746 = ORIENTED_EDGE ( 'NONE', *, *, #167641, .T. ) ;
#120747 = CARTESIAN_POINT ( 'NONE',  ( 8.988692655735958326, 12.47026328412523988, -1.082531754730543083 ) ) ;
#120748 = CARTESIAN_POINT ( 'NONE',  ( 0.6851730022342136239, 1.650096953764205399, 1.158669022729153175 ) ) ;
#120749 = CARTESIAN_POINT ( 'NONE',  ( 3.729901657090948230, 6.405283462364505631, 1.082531754730549078 ) ) ;
#120750 = CARTESIAN_POINT ( 'NONE',  ( -10.39230484541323740, 4.000000000000003553, 6.000000000000048850 ) ) ;
#120751 = CARTESIAN_POINT ( 'NONE',  ( 8.717529583462649612, 10.23316793787035195, 1.082531754730558626 ) ) ;
#120752 = CARTESIAN_POINT ( 'NONE',  ( 7.721532178182734185, 8.967207948423393304, 1.199719254218462483 ) ) ;
#120754 = CARTESIAN_POINT ( 'NONE',  ( 5.730082575778132181, 1.913663781862886104, 0.08886097549761286241 ) ) ;
#120753 = CARTESIAN_POINT ( 'NONE',  ( -6.891622154448065807, 6.934647356477856128, 1.040834085586084257E-14 ) ) ;
#120755 = AXIS2_PLACEMENT_3D ( 'NONE', #104516, #121904, #57885 ) ;
#120756 = CARTESIAN_POINT ( 'NONE',  ( 1.913245249192530695, 8.998828458478531189, 0.7750000000000004663 ) ) ;
#120757 = DIRECTION ( 'NONE',  ( 5.578564026256490882E-16, 1.000000000000000000, 9.066213480720158442E-32 ) ) ;
#120758 = CARTESIAN_POINT ( 'NONE',  ( -10.99998664267163662, -6.472053282365751059, -0.02741317976723587138 ) ) ;
#120760 = ORIENTED_EDGE ( 'NONE', *, *, #89709, .F. ) ;
#120759 = CARTESIAN_POINT ( 'NONE',  ( 4.365362273920250225, 5.155639410070820716, 1.082531754730560403 ) ) ;
#120761 = CARTESIAN_POINT ( 'NONE',  ( -3.972702704004144714, 4.593573561881607148, 1.199719254218462483 ) ) ;
#120762 = CARTESIAN_POINT ( 'NONE',  ( 2.501032641837992454, 1.736685530831501456, -1.287010829427559289 ) ) ;
#120763 = CARTESIAN_POINT ( 'NONE',  ( -6.292392690518202159, 9.394856334696294553, -1.082531754730549967 ) ) ;
#120764 = CARTESIAN_POINT ( 'NONE',  ( 5.383996398402570271, 9.295429874862735531, 0.000000000000000000 ) ) ;
#120765 = CARTESIAN_POINT ( 'NONE',  ( 1.230900525853476868, 1.420129835883350955, -1.575055732827963295 ) ) ;
#120766 = CARTESIAN_POINT ( 'NONE',  ( 5.403274641334286699, 1.493489847867332854, 1.049580640413529276 ) ) ;
#120767 = CARTESIAN_POINT ( 'NONE',  ( 2.460178626894731213, 0.8396039701564265156, 1.783738064433965986 ) ) ;
#120768 = CARTESIAN_POINT ( 'NONE',  ( 5.009976098083095408, -0.6827417919906975108, 1.786564173047608062 ) ) ;
#120769 = VERTEX_POINT ( 'NONE', #21887 ) ;
#120770 = CARTESIAN_POINT ( 'NONE',  ( 4.615651692036619735, 0.4336440386765746946, -1.921039654613013292 ) ) ;
#120771 = CARTESIAN_POINT ( 'NONE',  ( 0.9724825242501096145, -0.04715749842807348546, -1.941539141333733953 ) ) ;
#120772 = ORIENTED_EDGE ( 'NONE', *, *, #201935, .T. ) ;
#120773 = CARTESIAN_POINT ( 'NONE',  ( -5.041653019435350380, 6.975290837464928728, -1.599625672291271394 ) ) ;
#120774 = CARTESIAN_POINT ( 'NONE',  ( -3.298376509874564988, 7.070132704820777825, 0.000000000000000000 ) ) ;
#120776 = CARTESIAN_POINT ( 'NONE',  ( 6.834718834620487016, 7.146462526578263308, 0.000000000000000000 ) ) ;
#120775 = CARTESIAN_POINT ( 'NONE',  ( 6.259060471003163428, 10.45398764947904624, -0.7998128361456291469 ) ) ;
#120778 = ORIENTED_EDGE ( 'NONE', *, *, #75612, .T. ) ;
#120777 = CARTESIAN_POINT ( 'NONE',  ( 5.162724115531083235, 0.5589384127702141658, 1.828758346017298919 ) ) ;
#120779 = CARTESIAN_POINT ( 'NONE',  ( 1.149787729276055437, -1.740433383357189223, -1.356609624190791008 ) ) ;
#120780 =( GEOMETRIC_REPRESENTATION_CONTEXT ( 3 ) GLOBAL_UNCERTAINTY_ASSIGNED_CONTEXT ( ( #53664 ) ) GLOBAL_UNIT_ASSIGNED_CONTEXT ( ( #37696, #116862, #182864 ) ) REPRESENTATION_CONTEXT ( 'NONE', 'WORKASPACE' ) );
#120781 = CARTESIAN_POINT ( 'NONE',  ( 1.533805080506458030, 8.737074443703258808, 2.508413646267935171 ) ) ;
#120782 = CARTESIAN_POINT ( 'NONE',  ( 6.410797320372758179, -0.5389820150160546941, -1.939520479220447902 ) ) ;
#120784 =( BOUNDED_CURVE ( )  B_SPLINE_CURVE ( 3, ( #167478, #19074, #85155, #2807 ),
 .UNSPECIFIED., .F., .T. ) 
 B_SPLINE_CURVE_WITH_KNOTS ( ( 4, 4 ),
 ( 0.000000000000000000, 0.4999999999999993894 ),
 .UNSPECIFIED. ) 
 CURVE ( )  GEOMETRIC_REPRESENTATION_ITEM ( )  RATIONAL_B_SPLINE_CURVE ( ( 1.000000000000000000, 0.3333333333333342030, 0.3333333333333333703, 0.9999999999999992228 ) ) 
 REPRESENTATION_ITEM ( '' )  );
#120783 = FACE_OUTER_BOUND ( 'NONE', #188642, .T. ) ;
#120785 = CARTESIAN_POINT ( 'NONE',  ( -4.694778114904050170, 8.360933773907422761, 0.7116201367730221605 ) ) ;
#120786 = CARTESIAN_POINT ( 'NONE',  ( -0.1841574206260490065, 7.053066645632062759, 4.037422194176029322 ) ) ;
#120787 = CARTESIAN_POINT ( 'NONE',  ( 3.068866956829822801, 1.501395149897828851, -1.425812640530661479 ) ) ;
#120788 = CARTESIAN_POINT ( 'NONE',  ( -5.225778143063529946, 8.184159369294361497, 1.199719254218452047 ) ) ;
#120789 = CARTESIAN_POINT ( 'NONE',  ( -4.767604096130494185, 8.184890741402179870, -0.7573865900243268445 ) ) ;
#120791 = CARTESIAN_POINT ( 'NONE',  ( 0.8663662989462637132, 1.066309655776727539, 1.880320099339624296 ) ) ;
#120790 = CARTESIAN_POINT ( 'NONE',  ( -4.416205349749324327, 6.175325546172740765, 1.599625672291267398 ) ) ;
#120792 = CARTESIAN_POINT ( 'NONE',  ( -12.00000747045989691, 9.073125656298698161, 0.3084868119113360896 ) ) ;
#120793 = CARTESIAN_POINT ( 'NONE',  ( 4.909461021924244051, 6.821066840368686712, 1.443375672974065660 ) ) ;
#120794 = CARTESIAN_POINT ( 'NONE',  ( 0.2167848519283288866, -6.775781654326520353, 9.491250020638730689 ) ) ;
#120795 = EDGE_CURVE ( 'NONE', #33851, #99973, #153653, .T. ) ;
#120796 = CARTESIAN_POINT ( 'NONE',  ( -8.012344526598182026E-15, 13.10937500034140157, -1.575800808251669460 ) ) ;
#120798 = CARTESIAN_POINT ( 'NONE',  ( -4.294900800479008574, 8.232744377192641849, 0.000000000000000000 ) ) ;
#120797 = CARTESIAN_POINT ( 'NONE',  ( 6.925078400183556582, 1.261064080992575498, 2.068696352333323052 ) ) ;
#120799 = CIRCLE ( 'NONE', #183023, 0.04999999999999969746 ) ;
#120800 = CARTESIAN_POINT ( 'NONE',  ( 4.535645802837630747, -1.388783131305007634, 1.038275480396163353 ) ) ;
#120801 = CARTESIAN_POINT ( 'NONE',  ( -3.144601563365788444, 5.756120026313656268, -1.199719254218452935 ) ) ;
#120802 = CARTESIAN_POINT ( 'NONE',  ( 3.080986915251407776, 1.947773190787219555, 0.7018234266842755531 ) ) ;
#120803 = CARTESIAN_POINT ( 'NONE',  ( 4.534827772108455335, -1.699605468249162588, 1.262326912638973786 ) ) ;
#120804 = CARTESIAN_POINT ( 'NONE',  ( 5.750629710490689384, 9.860818428881154674, -0.7998128361456291469 ) ) ;
#120805 = CARTESIAN_POINT ( 'NONE',  ( 0.6823417656249899377, 4.176041667008085767, -1.181850606188754593 ) ) ;
#120806 = CARTESIAN_POINT ( 'NONE',  ( 2.324999910687207461, -1.798643183423669134, -0.8027048682860711271 ) ) ;
#120807 = CARTESIAN_POINT ( 'NONE',  ( 1.089939655121434203, 1.141396045679959004, 1.534244836814010693 ) ) ;
#120808 = CARTESIAN_POINT ( 'NONE',  ( 4.646573614920027850, -1.842837963294202464, 1.363044294324888162 ) ) ;
#120809 = CARTESIAN_POINT ( 'NONE',  ( 2.068725586703868746, -1.668841220716179130, -0.7407507213199536755 ) ) ;
#120810 = CARTESIAN_POINT ( 'NONE',  ( 4.044074958626150185, 7.940114228364351767, 0.7998128361456271485 ) ) ;
#120811 = CARTESIAN_POINT ( 'NONE',  ( 5.680503174001485078, 6.689970460165617361, -1.082531754730543083 ) ) ;
#120812 = CARTESIAN_POINT ( 'NONE',  ( -7.426115451983156923, 9.686887332112256388, -1.599625672291263179 ) ) ;
#120813 = CARTESIAN_POINT ( 'NONE',  ( 2.707291822170342144, 1.724471752635655664, -1.038662168513148965 ) ) ;
#120814 = CARTESIAN_POINT ( 'NONE',  ( 3.766413727395605093, -0.7909564911158167844, -1.795405819223389488 ) ) ;
#120815 = CARTESIAN_POINT ( 'NONE',  ( -7.049349804101573191, 10.31165964050546258, -1.199719254218440723 ) ) ;
#120816 = CARTESIAN_POINT ( 'NONE',  ( -4.062639585589296942, 7.891496616496157301, 0.7998128361456341429 ) ) ;
#120817 = CARTESIAN_POINT ( 'NONE',  ( 0.1755611466353655115, 0.2306421705509461850, -2.278008211689793061 ) ) ;
#120819 = CARTESIAN_POINT ( 'NONE',  ( 4.399107752292472640, 1.421951945714538867, 1.053510053677222613 ) ) ;
#120818 = CARTESIAN_POINT ( 'NONE',  ( 6.070280604649140876, -1.984772539198733865, -0.6570628365835521345 ) ) ;
#120820 = CARTESIAN_POINT ( 'NONE',  ( 4.900944506803885936, 4.854540586819195092, 0.6419561201193320077 ) ) ;
#120821 = CARTESIAN_POINT ( 'NONE',  ( 1.201424296212102893, -0.5295503721958020327, 2.126384922054704862 ) ) ;
#120822 = CARTESIAN_POINT ( 'NONE',  ( 0.2041417395101949583, 1.512754574849054956, 0.8604388899705726068 ) ) ;
#120823 = MECHANICAL_DESIGN_GEOMETRIC_PRESENTATION_REPRESENTATION (  '', ( #82712 ), #162349 ) ;
#120824 = CARTESIAN_POINT ( 'NONE',  ( 6.100279051144945619, 9.204410428722734849, -1.199719254218440723 ) ) ;
#120825 = CARTESIAN_POINT ( 'NONE',  ( 0.2331713839410939626, 4.091360563681152307, -2.508188233588979799 ) ) ;
#120826 = CARTESIAN_POINT ( 'NONE',  ( 0.9842439076201170423, 2.124318566921878482, 0.8778218499742740377 ) ) ;
#120827 = CARTESIAN_POINT ( 'NONE',  ( -0.02351032182101517320, -2.127384168920816165, -0.5261613093957145937 ) ) ;
#120828 = CARTESIAN_POINT ( 'NONE',  ( 6.327464733921618567, -1.223274778582748246, 1.229020038707399065 ) ) ;
#120829 = CARTESIAN_POINT ( 'NONE',  ( 1.700138637298425737, -0.7412910010123253679, 2.078789392164873906 ) ) ;
#120830 =( NAMED_UNIT ( * ) PLANE_ANGLE_UNIT ( ) SI_UNIT ( $, .RADIAN. ) );
#120831 = CARTESIAN_POINT ( 'NONE',  ( 0.7960475122521799562, -1.534068779871503363, -1.536527999751842621 ) ) ;
#120832 = DIRECTION ( 'NONE',  ( 0.000000000000000000, 0.000000000000000000, -1.000000000000000000 ) ) ;
#120833 = CARTESIAN_POINT ( 'NONE',  ( 1.604857428818485587, 1.977717902320776266, 0.7566523057890365278 ) ) ;
#120834 = CARTESIAN_POINT ( 'NONE',  ( 4.250000000000002665, 2.550977938801684432E-13, 2.052068128417944948 ) ) ;
#120835 = CARTESIAN_POINT ( 'NONE',  ( 6.727182134110167411, 4.690976314540481695, 2.651619508270358416 ) ) ;
#120836 = CARTESIAN_POINT ( 'NONE',  ( 4.454074118230034962, 1.925978650549282856, -0.04673309505795821689 ) ) ;
#120837 = ORIENTED_EDGE ( 'NONE', *, *, #128643, .F. ) ;
#120838 = STYLED_ITEM ( 'NONE', ( #98612 ), #36810 ) ;
#120840 = CARTESIAN_POINT ( 'NONE',  ( -1.500000000000011324, 5.129166666666691299, -0.8660254037844313801 ) ) ;
#120839 = CARTESIAN_POINT ( 'NONE',  ( 1.189493828671518427, 1.739998485882883861, 1.492566873345043010 ) ) ;
#120841 = CARTESIAN_POINT ( 'NONE',  ( 2.347533153460546806, 5.890539112345938300, 0.000000000000000000 ) ) ;
#120842 = B_SPLINE_CURVE_WITH_KNOTS ( 'NONE', 3,
 ( #94926, #27767, #93863, #144764, #50155, #67431, #166036, #181209, #177225, #132512 ),
 .UNSPECIFIED., .F., .F.,
 ( 4, 1, 1, 1, 1, 1, 1, 4 ),
 ( 0.000000000000000000, 0.09373397616858752945, 0.1863105892815605236, 0.2574079725677296260, 0.3612190813870841954, 0.5208938042821120717, 0.7336009914826546741, 1.000000000000000000 ),
 .UNSPECIFIED. ) ;
#120843 = CARTESIAN_POINT ( 'NONE',  ( 5.900823170445728572, 7.907379670318584353, 1.599625672291267398 ) ) ;
#120844 = CARTESIAN_POINT ( 'NONE',  ( 4.196076301648347773, 1.450992468586336459, 1.681961854464069983 ) ) ;
#120845 = CARTESIAN_POINT ( 'NONE',  ( -9.029367117021344313, 9.636609179387466639, 0.7216878364870438212 ) ) ;
#120847 = CARTESIAN_POINT ( 'NONE',  ( -1.063464886907111495, -4.211945764156256544, 0.1580247838114293979 ) ) ;
#120846 = VECTOR ( 'NONE', #77482, 1000.000000000000000 ) ;
#120848 = CARTESIAN_POINT ( 'NONE',  ( 4.500943810056890371, 8.194925511800951412, -0.7216878364870207285 ) ) ;
#120849 = CARTESIAN_POINT ( 'NONE',  ( -8.039621902779392926, 9.442275643739831636, 1.082531754730558626 ) ) ;
#120850 = CARTESIAN_POINT ( 'NONE',  ( 5.560252395380206991, 7.580323442733986283, 1.443375672974065660 ) ) ;
#120851 = CARTESIAN_POINT ( 'NONE',  ( 1.371720446232262081, -0.2986288616722633793, -1.994071132515719658 ) ) ;
#120853 = CARTESIAN_POINT ( 'NONE',  ( 0.4618802912403723870, -0.5535076142849646441, 1.986819116141485653 ) ) ;
#120852 = CARTESIAN_POINT ( 'NONE',  ( 7.938462636001388795, 9.220293482545153907, -1.199719254218441611 ) ) ;
#120854 = FILL_AREA_STYLE ('',( #5922 ) ) ;
#120855 = CARTESIAN_POINT ( 'NONE',  ( 4.543390873910894356, 8.314723429622471684, 0.7216878364870317197 ) ) ;
#120856 = CARTESIAN_POINT ( 'NONE',  ( -0.02423404108400224743, -1.785672699080865788, -0.4486397487279417118 ) ) ;
#120857 = CARTESIAN_POINT ( 'NONE',  ( -3.931903513251300275, 8.991426765939651844, 0.7749999999999996891 ) ) ;
#120858 = CARTESIAN_POINT ( 'NONE',  ( 0.6823417656249899377, 2.092708333674753174, 1.181850606188767472 ) ) ;
#120859 = CARTESIAN_POINT ( 'NONE',  ( 1.493014682725684938, 1.335586794047480153, 1.161194053514543745 ) ) ;
#120860 = CARTESIAN_POINT ( 'NONE',  ( -0.1341500063891595818, -0.1486117279969369209, -1.983907055413631992 ) ) ;
#120861 = CARTESIAN_POINT ( 'NONE',  ( 6.427322163675834865, -1.144589508088897478, -1.311236935029986173 ) ) ;
#120862 = CARTESIAN_POINT ( 'NONE',  ( 4.247812404936269992, 2.291854478692372687, -0.05604449276840757499 ) ) ;
#120863 = CARTESIAN_POINT ( 'NONE',  ( 3.749809578975582536, 0.6641696684822319119, 1.717346325712478583 ) ) ;
#120864 = CARTESIAN_POINT ( 'NONE',  ( 7.747594715205354809, 11.12627870345989756, -1.199719254218446718 ) ) ;
#120865 = CARTESIAN_POINT ( 'NONE',  ( 3.856323340278215106, 0.6566615474184741563, 1.703573633380930152 ) ) ;
#120866 = CARTESIAN_POINT ( 'NONE',  ( 4.606092368833686557, -0.09613688574180989654, 2.014232646917232916 ) ) ;
#120867 = CARTESIAN_POINT ( 'NONE',  ( -8.319899820280397762, 12.85830022363583147, -0.7998128361456281477 ) ) ;
#120869 = CARTESIAN_POINT ( 'NONE',  ( -6.933015448541747006, 9.181880338089085214, 1.599625672291269396 ) ) ;
#120868 = CARTESIAN_POINT ( 'NONE',  ( 2.905426592119991991, 1.910755973352752379, 1.211346930818749890 ) ) ;
#120870 = CARTESIAN_POINT ( 'NONE',  ( 6.458053290436937210, 2.100604981398071835, -0.1509308302805877633 ) ) ;
#120871 = CARTESIAN_POINT ( 'NONE',  ( 0.7499999999999920064, 4.264583334016150751, 1.299038105676669330 ) ) ;
#120872 = CARTESIAN_POINT ( 'NONE',  ( 4.158688916442685013, -0.6465363538536235133, -1.966910096795893681 ) ) ;
#120873 = CARTESIAN_POINT ( 'NONE',  ( 9.890836756369282057, 11.49806328964105617, -1.199719254218440723 ) ) ;
#120874 = CARTESIAN_POINT ( 'NONE',  ( -0.6801582343750125492, 2.213541667008059211, 1.178068619123818994 ) ) ;
#120875 = CARTESIAN_POINT ( 'NONE',  ( 6.094406630213896392, -1.134638919006492275, 1.791192486788994120 ) ) ;
#120876 = CONTEXT_DEPENDENT_SHAPE_REPRESENTATION ( #140545, #161321 ) ;
#120878 = CARTESIAN_POINT ( 'NONE',  ( 2.121591023604427306, -1.868723361717766096, 0.4677975013653943859 ) ) ;
#120877 = CARTESIAN_POINT ( 'NONE',  ( -7.967387826325084355, 12.44703623068796361, 0.7998128361456481317 ) ) ;
#120879 = UNCERTAINTY_MEASURE_WITH_UNIT (LENGTH_MEASURE( 1.000000000000000082E-05 ), #10082, 'distance_accuracy_value', 'NONE');
#120880 = CARTESIAN_POINT ( 'NONE',  ( 4.897706171852771462, 4.871974472535213430, 0.6676900015689657408 ) ) ;
#120881 = CARTESIAN_POINT ( 'NONE',  ( 6.508657463561863921, 0.6146053541861602465, 1.871187945041019152 ) ) ;
#120882 = CARTESIAN_POINT ( 'NONE',  ( 5.844973620822844218, 5.991759777147701804, 0.7216878364870328300 ) ) ;
#120883 = CARTESIAN_POINT ( 'NONE',  ( 5.804557637360799660, 6.030435022130575362, 0.4940411958238543066 ) ) ;
#120884 = CARTESIAN_POINT ( 'NONE',  ( 1.872228381520312013, 3.299999999999997158, -0.4000000000000131783 ) ) ;
#120885 = CARTESIAN_POINT ( 'NONE',  ( -5.739179097286464248, 5.590130456455974617, -0.7998128361456221525 ) ) ;
#120886 = CARTESIAN_POINT ( 'NONE',  ( 0.3346308043965214307, -1.195296165414746037, -1.872270659723746622 ) ) ;
#120887 = CARTESIAN_POINT ( 'NONE',  ( 2.854625263381281641, 0.7083305855763160075, 1.983406512126543841 ) ) ;
#120888 = CARTESIAN_POINT ( 'NONE',  ( -4.085803189671902480, 5.860132702740892263, -1.599625672291271394 ) ) ;
#120889 = CARTESIAN_POINT ( 'NONE',  ( 7.263417608619159083, 9.497073181520933716, -1.599625672291262513 ) ) ;
#120890 = CARTESIAN_POINT ( 'NONE',  ( 0.2208628207966298607, -1.659654761427356240, -0.8422171645118268213 ) ) ;
#120891 = CARTESIAN_POINT ( 'NONE',  ( 7.298366762858032430, 7.409182732956175244, 1.040834085586084257E-14 ) ) ;
#120892 = CARTESIAN_POINT ( 'NONE',  ( 4.253507506385319381, 5.985511395581417204, 1.599625672291267398 ) ) ;
#120893 = CARTESIAN_POINT ( 'NONE',  ( -5.641601317062239218, 8.635599732330991429, -1.082531754730549967 ) ) ;
#120894 = CARTESIAN_POINT ( 'NONE',  ( -9.517460647113315630, 10.20605163116143821, 0.7216878364870438212 ) ) ;
#120895 = CARTESIAN_POINT ( 'NONE',  ( 1.652743449602233072, 2.098267697663995790, 0.3060111223712052020 ) ) ;
#120896 = CARTESIAN_POINT ( 'NONE',  ( -6.936931872047518155, 8.122117267924091166, 1.199719254218452047 ) ) ;
#120898 = CARTESIAN_POINT ( 'NONE',  ( 3.156644782993088150, -0.5669402238272451822, -1.878178299617596192 ) ) ;
#120897 = CARTESIAN_POINT ( 'NONE',  ( 1.224999999999951017, 0.1458333333333527160, -0.7072540797573076965 ) ) ;
#120899 = CARTESIAN_POINT ( 'NONE',  ( 2.553791647773369089, 0.5774160426356907960, -2.083079400968433248 ) ) ;
#120900 = CARTESIAN_POINT ( 'NONE',  ( 1.804012939494209267, 1.363607186100148638, -1.237405090928713092 ) ) ;
#120902 = CARTESIAN_POINT ( 'NONE',  ( -5.289711001425910553, 6.400709951683444920, -1.138330407662338617 ) ) ;
#120901 = CARTESIAN_POINT ( 'NONE',  ( -3.634467696915153034, 6.397906858779740524, 1.199719254218452935 ) ) ;
#120903 = CARTESIAN_POINT ( 'NONE',  ( 3.450842174108187610, 0.4214097805228322891, -1.688396943527884053 ) ) ;
#120904 = CYLINDRICAL_SURFACE ( 'NONE', #98087, 3.100000000000000089 ) ;
#120905 = CARTESIAN_POINT ( 'NONE',  ( 4.677199807034550183, 8.400557508274889784, 1.040834085586084257E-14 ) ) ;
#120906 = CARTESIAN_POINT ( 'NONE',  ( -10.57232049882948388, 5.599334429189661400, -4.968988939937085014 ) ) ;
#120907 = CARTESIAN_POINT ( 'NONE',  ( 1.270647086845246188, -1.370953960119488668, 1.671340013135722558 ) ) ;
#120908 = CARTESIAN_POINT ( 'NONE',  ( 3.374374892241317703, -0.3960410224921434574, 1.976653181598592601 ) ) ;
#120909 = CARTESIAN_POINT ( 'NONE',  ( -9.937763408692596556, 11.65677406730528887, -1.082531754730537976 ) ) ;
#120910 = CARTESIAN_POINT ( 'NONE',  ( -3.526002468005825286, 6.271364091718859335, -1.199719254218450271 ) ) ;
#120911 = CARTESIAN_POINT ( 'NONE',  ( 3.731288366010646396, -1.822051990069279315, 0.7533225318517923208 ) ) ;
#120912 = CARTESIAN_POINT ( 'NONE',  ( 6.609000000000064823, 1.245995683336246884, 2.213443714173808807 ) ) ;
#120913 = CARTESIAN_POINT ( 'NONE',  ( 2.243606950041766357, 1.941679294436208680, 0.04551257769231514122 ) ) ;
#120916 = ORIENTED_EDGE ( 'NONE', *, *, #183589, .F. ) ;
#120915 = CARTESIAN_POINT ( 'NONE',  ( -5.506019780925599960, 5.596313630600862510, 0.7216878364870257245 ) ) ;
#120914 = CARTESIAN_POINT ( 'NONE',  ( 6.938893903907228378E-15, 10.64264068711930733, 1.214306433183764966E-14 ) ) ;
#120917 = CARTESIAN_POINT ( 'NONE',  ( -5.465345319640241506, 5.548860092434608760, 0.7216878364870257245 ) ) ;
#120918 = CARTESIAN_POINT ( 'NONE',  ( -0.1106856583841424602, 0.7110496148716296538, -2.078439740052108853 ) ) ;
#120919 = CARTESIAN_POINT ( 'NONE',  ( 6.249382461256315580, 6.255644057745969988, -0.7998128361456481317 ) ) ;
#120920 = CARTESIAN_POINT ( 'NONE',  ( -4.294900800479008574, 8.232744377192641849, 0.000000000000000000 ) ) ;
#120921 = CARTESIAN_POINT ( 'NONE',  ( -6.363572996767778100, 8.517530811019446091, -1.599625672291271394 ) ) ;
#120922 = CARTESIAN_POINT ( 'NONE',  ( -6.533654225826463602, 6.808800017212038647, -0.5559908469023568944 ) ) ;
#120923 = CARTESIAN_POINT ( 'NONE',  ( 6.668959562645871308, -2.105872948262592192, -0.9439719561973120010 ) ) ;
#120924 = CARTESIAN_POINT ( 'NONE',  ( -11.07790593930098311, 9.799999999999998934, -0.7000000000000009548 ) ) ;
#120925 = CARTESIAN_POINT ( 'NONE',  ( 4.416819765676714304, -1.456490764316048292, 1.314424223973277961 ) ) ;
#120926 = CARTESIAN_POINT ( 'NONE',  ( 6.598014311344812199, 10.84943379654430906, 1.040834085586084257E-14 ) ) ;
#120927 = CARTESIAN_POINT ( 'NONE',  ( 1.811172873341511336, 1.158687402475454098, -1.650082692374904125 ) ) ;
#120928 = VERTEX_POINT ( 'NONE', #186552 ) ;
#120929 = CARTESIAN_POINT ( 'NONE',  ( 2.413409855213846544, -1.973772631060242144, 0.7668006401621522139 ) ) ;
#120930 = CARTESIAN_POINT ( 'NONE',  ( -1.201851678989727383E-14, 1.493750000682814383, 1.732050807568877637 ) ) ;
#120932 = CARTESIAN_POINT ( 'NONE',  ( -6.501298352952815662, 7.543601818988450169, -1.199719254218446718 ) ) ;
#120931 = CARTESIAN_POINT ( 'NONE',  ( -10.28586320583439395, 2.972657967447029037, 5.491880110203110732 ) ) ;
#120933 = CARTESIAN_POINT ( 'NONE',  ( 3.064218985076866630, -1.701416833343888824, -0.7040189834505713451 ) ) ;
#120934 = ORIENTED_EDGE ( 'NONE', *, *, #152831, .T. ) ;
#120935 = CARTESIAN_POINT ( 'NONE',  ( -8.513630394377489807, 12.01998699582738972, -1.199719254218446718 ) ) ;
#120936 = CARTESIAN_POINT ( 'NONE',  ( 1.886825320689233809, 2.480000000000016858, 2.459652456995882641 ) ) ;
#120938 = ADVANCED_FACE ( 'NONE', ( #68514 ), #38181, .F. ) ;
#120937 = CARTESIAN_POINT ( 'NONE',  ( 3.867525618572264623, -1.764951123045129577, -1.175235903013646332 ) ) ;
#120939 = B_SPLINE_CURVE_WITH_KNOTS ( 'NONE', 3,
 ( #163784, #15363, #81456, #42846, #92662, #10303 ),
 .UNSPECIFIED., .F., .F.,
 ( 4, 2, 4 ),
 ( 0.000000000000000000, 0.0003157158648874029564, 0.0006314317297748059127 ),
 .UNSPECIFIED. ) ;
#120940 = CARTESIAN_POINT ( 'NONE',  ( 0.4625323210639306071, 0.1833022542275381250, -1.831979997761295165 ) ) ;
#120941 = CARTESIAN_POINT ( 'NONE',  ( -1.387358672534699799, 7.315968950353656020, 4.254625267138158584 ) ) ;
#120942 = CARTESIAN_POINT ( 'NONE',  ( 5.991813822235618758, 9.077867661661846554, 1.199719254218462483 ) ) ;
#120943 = CARTESIAN_POINT ( 'NONE',  ( 4.798151449762615428, -2.060242214822493256, -0.05457638173838111340 ) ) ;
#120944 = AXIS2_PLACEMENT_3D ( 'NONE', #203147, #55852, #74247 ) ;
#120946 = CARTESIAN_POINT ( 'NONE',  ( 1.153568636672014369, 0.7464410156945017194, 1.683350060182234209 ) ) ;
#120945 = CARTESIAN_POINT ( 'NONE',  ( -6.551614543901706611, 8.666636272683888365, 1.599625672291283607 ) ) ;
#120947 = CARTESIAN_POINT ( 'NONE',  ( 9.447334110624092673, 9.916311305349925220, -0.7998128361456281477 ) ) ;
#120948 = CARTESIAN_POINT ( 'NONE',  ( 1.364683531249992088, 5.634375000341417916, 1.214306433183764966E-14 ) ) ;
#120949 = DIRECTION ( 'NONE',  ( 0.000000000000000000, 1.000000000000000000, 0.000000000000000000 ) ) ;
#120950 = CARTESIAN_POINT ( 'NONE',  ( -9.499606442108964544, -9.901472054505708442, 0.08647222121513538362 ) ) ;
#120951 = CARTESIAN_POINT ( 'NONE',  ( 10.96287206819929594, -7.723179855898520962, -0.5577339983718512251 ) ) ;
#120952 = CARTESIAN_POINT ( 'NONE',  ( 1.752831059180045115, 0.6944836804415283060, 2.094827981560241970 ) ) ;
#120953 = CARTESIAN_POINT ( 'NONE',  ( 4.024925711125073136, 2.146699088035211922, 0.7144036547655304714 ) ) ;
#120954 = CARTESIAN_POINT ( 'NONE',  ( -6.710922849084449915, 10.77323439066645783, 0.000000000000000000 ) ) ;
#120955 = CARTESIAN_POINT ( 'NONE',  ( 3.814574336081223649, -0.5739048956562255999, -1.718320587032542202 ) ) ;
#120956 = CARTESIAN_POINT ( 'NONE',  ( 3.872214865662172656, -1.895674933386840344, -0.2753630107846723463 ) ) ;
#120957 = CARTESIAN_POINT ( 'NONE',  ( 5.389151899530504330, 0.1487064154041470299, 2.065066873896327593 ) ) ;
#120958 = CARTESIAN_POINT ( 'NONE',  ( -1.364683531250012516, 4.051041667008088432, -0.7879004041258300672 ) ) ;
#120959 = CARTESIAN_POINT ( 'NONE',  ( 3.713711766734467012, -1.942503170530969436, 0.3358077238896309824 ) ) ;
#120960 = CARTESIAN_POINT ( 'NONE',  ( 1.289925581193847925, -0.8688078642279849495, 1.719429354455022096 ) ) ;
#120961 = CARTESIAN_POINT ( 'NONE',  ( 4.364026845288040413, 0.8817440624687390427, 1.649792572839225091 ) ) ;
#120962 = TOROIDAL_SURFACE ( 'NONE', #58575, 10.75000000000000000, 0.5000000000000007772 ) ;
#120963 = CARTESIAN_POINT ( 'NONE',  ( 3.053680222918000453, -1.886840229487633414, -1.328398743635789803 ) ) ;
#120964 = CARTESIAN_POINT ( 'NONE',  ( 5.019887821480574885, 1.840843491799005527, -0.2725137592536843734 ) ) ;
#120965 = CARTESIAN_POINT ( 'NONE',  ( 1.364683531249988535, 4.655208333674755394, -0.7879004041258300672 ) ) ;
#120966 = CARTESIAN_POINT ( 'NONE',  ( 1.499999999999993117, 8.885416667349462116, 0.8660254037844408170 ) ) ;
#120967 = ADVANCED_FACE ( 'NONE', ( #53355 ), #90145, .F. ) ;
#120968 = CARTESIAN_POINT ( 'NONE',  ( 2.051528240825768012, -1.692106715078506296, -1.253703384363166196 ) ) ;
#120969 = CARTESIAN_POINT ( 'NONE',  ( 4.351804119862229037, 4.179452349368450115, -0.7216878364870188411 ) ) ;
#120971 = DIRECTION ( 'NONE',  ( -3.219646771412963434E-15, -1.665334536937739741E-16, -1.000000000000000000 ) ) ;
#120970 = FACE_OUTER_BOUND ( 'NONE', #116340, .T. ) ;
#120972 = CARTESIAN_POINT ( 'NONE',  ( -1.860351378971601966, 8.967085675740335660, -0.7749999999999996891 ) ) ;
#120973 = CARTESIAN_POINT ( 'NONE',  ( 2.777707764728345907, 0.3069055913166895966, -2.098134212408508059 ) ) ;
#120975 = CARTESIAN_POINT ( 'NONE',  ( 6.387350227230087718, 6.552219065276430499, -2.500000000000000444 ) ) ;
#120974 = B_SPLINE_CURVE_WITH_KNOTS ( 'NONE', 3,
 ( #149853, #5681, #35004, #54475, #67485, #118470, #121693, #100024 ),
 .UNSPECIFIED., .F., .F.,
 ( 4, 2, 2, 4 ),
 ( 0.000000000000000000, 0.0002185754043082790087, 0.0004371508086165580174, 0.0008743016172331179864 ),
 .UNSPECIFIED. ) ;
#120976 = CARTESIAN_POINT ( 'NONE',  ( 0.4572932007271997001, -1.730182198833930318, 1.041906760498239271 ) ) ;
#120977 = CARTESIAN_POINT ( 'NONE',  ( 0.6823417656249899377, 0.8427083336747520637, 1.181850606188755259 ) ) ;
#120978 = CARTESIAN_POINT ( 'NONE',  ( -3.687454593236990430, 4.364747115940301292, 1.082531754730560403 ) ) ;
#120979 = CARTESIAN_POINT ( 'NONE',  ( 5.229694566569264680, 7.124396299129368337, 1.599625672291267398 ) ) ;
#120980 = ORIENTED_EDGE ( 'NONE', *, *, #71437, .T. ) ;
#120981 = CARTESIAN_POINT ( 'NONE',  ( 1.634274655659254005, 1.066924998833935989, -1.879885089102695250 ) ) ;
#120982 = CARTESIAN_POINT ( 'NONE',  ( 3.850152436600940753, 7.435668909435635854, -0.7216878364870309426 ) ) ;
#120985 = CARTESIAN_POINT ( 'NONE',  ( 2.846849069189655967, 5.304779099821139710, -1.082531754730543083 ) ) ;
#120984 = CARTESIAN_POINT ( 'NONE',  ( -4.067937748088393590, 7.725456827083305278, 0.6547958487484796253 ) ) ;
#120983 = CARTESIAN_POINT ( 'NONE',  ( 4.603875680292229156, 7.528882839386387360, 1.199719254218452047 ) ) ;
#120986 =( BOUNDED_CURVE ( )  B_SPLINE_CURVE ( 2, ( #34680, #166831, #102890, #118139, #200364, #18426, #82366, #136471, #84500 ),
 .UNSPECIFIED., .F., .T. ) 
 B_SPLINE_CURVE_WITH_KNOTS ( ( 3, 2, 2, 2, 3 ),
 ( 0.6718749999999998890, 0.6770833333333333703, 0.6875000000000000000, 0.6979166666666666297, 0.7031250000000002220 ),
 .UNSPECIFIED. ) 
 CURVE ( )  GEOMETRIC_REPRESENTATION_ITEM ( )  RATIONAL_B_SPLINE_CURVE ( ( 0.9330127018922192983, 0.9330127018922178550, 1.000000000000000000, 0.8660254037844387076, 1.000000000000000000, 0.8660254037844387076, 1.000000000000000000, 0.9330127018922165227, 0.9330127018922194093 ) ) 
 REPRESENTATION_ITEM ( '' )  );
#120987 = DIRECTION ( 'NONE',  ( 0.8594003466332824637, -0.03762549425793430824, 0.5099170191202098135 ) ) ;
#120988 = CARTESIAN_POINT ( 'NONE',  ( 5.436732529336289588, -1.586671906620169104, 1.244382051841623538 ) ) ;
#120989 = CARTESIAN_POINT ( 'NONE',  ( -7.158341918335454857, 10.33485409049125003, 1.082531754730549967 ) ) ;
#120990 = CARTESIAN_POINT ( 'NONE',  ( 6.374567656919228220, -0.1030857042376011334, -2.088345373630628554 ) ) ;
#120991 = FACE_OUTER_BOUND ( 'NONE', #62935, .T. ) ;
#120993 = CARTESIAN_POINT ( 'NONE',  ( 1.364683531249996529, 11.71354166700806587, 0.7879004041258403923 ) ) ;
#120992 = CARTESIAN_POINT ( 'NONE',  ( 6.737200384369169903, -1.933438233944267060, 0.9670071574134844195 ) ) ;
#120994 = CARTESIAN_POINT ( 'NONE',  ( -9.643927338022246332, 10.14567007064778004, -0.7998128361456291469 ) ) ;
#120995 = CARTESIAN_POINT ( 'NONE',  ( -4.555176424067209240, 8.258196894812975586, 1.040834085586084257E-14 ) ) ;
#120996 = CARTESIAN_POINT ( 'NONE',  ( -1.364683531250014514, 1.551041667008084435, -0.7879004041258289570 ) ) ;
#120997 = CARTESIAN_POINT ( 'NONE',  ( 2.680963302752298993, 0.4788041664877049075, 8.638326563840810896E-32 ) ) ;
#120998 = CARTESIAN_POINT ( 'NONE',  ( -1.500000000000008216, 10.00000000000000178, 3.469446951953614189E-15 ) ) ;
#120999 = CARTESIAN_POINT ( 'NONE',  ( 2.947548438991169473, 0.6205982292267105960, -1.609554129922322163 ) ) ;
#121000 = CARTESIAN_POINT ( 'NONE',  ( 5.337069745634900997, 6.255611453776062980, 1.199719254218452047 ) ) ;
#121001 = CARTESIAN_POINT ( 'NONE',  ( 1.721574597234516890, -0.9778441516922768972, -1.474834890465251291 ) ) ;
#121002 = CARTESIAN_POINT ( 'NONE',  ( 3.053387886640859694, -1.774279702891886190, 0.9510675200815300601 ) ) ;
#121003 = CARTESIAN_POINT ( 'NONE',  ( 5.877994779194309238, 1.310017027744770246, 1.775731318763192013 ) ) ;
#121004 = ORIENTED_EDGE ( 'NONE', *, *, #66712, .T. ) ;
#121005 = CARTESIAN_POINT ( 'NONE',  ( 4.693620712453854260, 1.883065523094022753, -0.7309246526977104530 ) ) ;
#121006 = CARTESIAN_POINT ( 'NONE',  ( -5.641074431737709283, 8.738948049406083385, -1.199719254218452047 ) ) ;
#121008 = CARTESIAN_POINT ( 'NONE',  ( 3.849232595480827079, 0.2440098934328518987, -2.001514877671112025 ) ) ;
#121007 = CARTESIAN_POINT ( 'NONE',  ( 4.459710115430675081, -1.639780234044617035, -1.344486126324248465 ) ) ;
#121010 = ORIENTED_EDGE ( 'NONE', *, *, #19034, .F. ) ;
#121009 = CARTESIAN_POINT ( 'NONE',  ( 4.043061577595566725, 0.09493798274137112136, 1.809245059475625750 ) ) ;
#121011 = CARTESIAN_POINT ( 'NONE',  ( 5.910428620914669473, 5.860197910680708944, 0.000000000000000000 ) ) ;
#121012 = VERTEX_POINT ( 'NONE', #86927 ) ;
#121013 = MECHANICAL_DESIGN_GEOMETRIC_PRESENTATION_REPRESENTATION (  '', ( #20712 ), #3393 ) ;
#121014 = ADVANCED_FACE ( 'NONE', ( #125916 ), #167847, .T. ) ;
#121015 = CARTESIAN_POINT ( 'NONE',  ( 1.358040219746913024, 0.7549631825471068147, 1.711723683848711985 ) ) ;
#121016 = CARTESIAN_POINT ( 'NONE',  ( -10.91850271852025500, -9.971093637360025852, 0.1617895344457901952 ) ) ;
#121017 = CARTESIAN_POINT ( 'NONE',  ( 6.551413666264667590, -1.614568043246225271, 0.8214943993307096681 ) ) ;
#121018 = CARTESIAN_POINT ( 'NONE',  ( -4.831252850731225124, 7.910156596299903420, 0.9996086013765632661 ) ) ;
#121019 = CARTESIAN_POINT ( 'NONE',  ( -10.68988767858338917, 3.994679225574373493, -4.900161361628223133 ) ) ;
#121020 = LINE ( 'NONE', #201081, #104063 ) ;
#121021 = CARTESIAN_POINT ( 'NONE',  ( 0.6823417656249899377, 2.905208333674754062, 1.181850606188765695 ) ) ;
#121022 = CARTESIAN_POINT ( 'NONE',  ( 0.5625819312903358460, 0.5574351770905332515, 1.829310545699929458 ) ) ;
#121023 = ORIENTED_EDGE ( 'NONE', *, *, #66779, .F. ) ;
#121024 = CARTESIAN_POINT ( 'NONE',  ( 6.156811154381533591, 9.236677875870187293, -1.082531754730548412 ) ) ;
#121025 = CARTESIAN_POINT ( 'NONE',  ( 1.293326634533353170, -1.775083115552608559, 0.8357255594537355003 ) ) ;
#121026 = CARTESIAN_POINT ( 'NONE',  ( -4.841670253855968831, 4.821239182352949904, 0.000000000000000000 ) ) ;
#121027 = CARTESIAN_POINT ( 'NONE',  ( -4.773352600463090845, 7.726605912919016106, 1.199719254218452935 ) ) ;
#121028 = CARTESIAN_POINT ( 'NONE',  ( 4.359710196644346780, -1.641147893522959089, -1.343014508298406628 ) ) ;
#121030 = CARTESIAN_POINT ( 'NONE',  ( -10.44369227015510404, 5.112964020592957404, 5.232143560358708534 ) ) ;
#121029 = CARTESIAN_POINT ( 'NONE',  ( -0.02988540731103071432, 0.005807295984020746475, -1.726291166677936362 ) ) ;
#121031 = CARTESIAN_POINT ( 'NONE',  ( 6.028588005634209601, 1.899229357904350879, 0.5280594692760686160 ) ) ;
#121032 = CARTESIAN_POINT ( 'NONE',  ( -1.364683531250012516, 1.530208333674756505, 0.7879004041258379498 ) ) ;
#121033 = CARTESIAN_POINT ( 'NONE',  ( 0.7209482731112315523, 1.521806550355369492, -1.318046908132961104 ) ) ;
#121034 = ORIENTED_EDGE ( 'NONE', *, *, #142095, .F. ) ;
#121035 = CARTESIAN_POINT ( 'NONE',  ( -0.08807185805374209697, -1.306980724784766013, -1.666505321573110265 ) ) ;
#121036 = CARTESIAN_POINT ( 'NONE',  ( 11.84619309640116747, 6.793804897517921049, 1.976512447145533091 ) ) ;
#121037 = CARTESIAN_POINT ( 'NONE',  ( 1.697802635435996743, -1.498143435978617877, -1.429203828351800487 ) ) ;
#121038 = CARTESIAN_POINT ( 'NONE',  ( 5.401997860402196316, 5.267028690082820930, 0.000000000000000000 ) ) ;
#121039 = CARTESIAN_POINT ( 'NONE',  ( 4.875038752565570732, 7.845239757038595663, -1.199719254218452047 ) ) ;
#121040 = ORIENTED_EDGE ( 'NONE', *, *, #149738, .F. ) ;
#121042 = CARTESIAN_POINT ( 'NONE',  ( 6.030679399980265920, 5.930214142932100252, -0.7998128361456281477 ) ) ;
#121041 = CARTESIAN_POINT ( 'NONE',  ( 5.121074860632232273, -1.985326386471301552, 0.6553513102709652705 ) ) ;
#121045 = ORIENTED_EDGE ( 'NONE', *, *, #131446, .F. ) ;
#121044 = CARTESIAN_POINT ( 'NONE',  ( 2.068756839025966521, -1.399621434743709703, 1.149952615172030512 ) ) ;
#121043 = CARTESIAN_POINT ( 'NONE',  ( 2.590611583786633254, -0.3098195481324728107, -1.798931244660670448 ) ) ;
#121046 = CARTESIAN_POINT ( 'NONE',  ( 6.340462157465731607, 2.182225300935904055, 0.3281612982340698093 ) ) ;
#121047 = CARTESIAN_POINT ( 'NONE',  ( 4.296070028909639404, -0.8476096858263427736, 2.037697185916572007 ) ) ;
#121048 = CARTESIAN_POINT ( 'NONE',  ( 6.934105498385400246, 10.17720795050327354, -1.199719254218441611 ) ) ;
#121049 = CARTESIAN_POINT ( 'NONE',  ( -0.6823417656250003738, 8.713541667008065872, 1.181850606188754593 ) ) ;
#121050 = CARTESIAN_POINT ( 'NONE',  ( 2.596233987490266681, -0.9813665562012074961, 1.641104690102652919 ) ) ;
#121051 = STYLED_ITEM ( 'NONE', ( #22451 ), #194826 ) ;
#121052 = CARTESIAN_POINT ( 'NONE',  ( 8.772289083241844310, 10.19309100432570148, -1.199719254218446718 ) ) ;
#121053 = CARTESIAN_POINT ( 'NONE',  ( 6.725056259267968350, -1.891221747171191403, -0.8428681758992571105 ) ) ;
#121054 = CARTESIAN_POINT ( 'NONE',  ( -0.6801582343750334214, 0.3802083336747336118, -1.178068619123869398 ) ) ;
#121055 = CARTESIAN_POINT ( 'NONE',  ( 6.374583145400191775, -0.1054333438532777389, -2.189162923280890904 ) ) ;
#121056 = DIRECTION ( 'NONE',  ( 1.000000000000000000, -0.000000000000000000, 1.779758311459929752E-16 ) ) ;
#121057 = CARTESIAN_POINT ( 'NONE',  ( 0.1753634416057732182, 7.629137130509072051, -2.744001747789548418 ) ) ;
#121058 = EDGE_LOOP ( 'NONE', ( #28692, #60210, #191306, #161473 ) ) ;
#121059 = CARTESIAN_POINT ( 'NONE',  ( 9.499690612162391190, -9.919996481418243306, -0.07742489488623274796 ) ) ;
#121060 = EDGE_CURVE ( 'NONE', #201490, #64100, #171405, .T. ) ;
#121061 = CARTESIAN_POINT ( 'NONE',  ( 3.356579238971897805, -1.418645411611328067, 1.219307012350186126 ) ) ;
#121062 = LINE ( 'NONE', #89564, #55164 ) ;
#121063 = CARTESIAN_POINT ( 'NONE',  ( -0.3000000000000432876, 3.999999999999940936, 0.9782388782688614670 ) ) ;
#121064 = CARTESIAN_POINT ( 'NONE',  ( -8.365017589951714072, 8.861534731139549592, 1.040834085586084257E-14 ) ) ;
#121065 = CARTESIAN_POINT ( 'NONE',  ( 3.898851692381625877, 6.706354853490643642, -1.199719254218452047 ) ) ;
#121066 = CARTESIAN_POINT ( 'NONE',  ( 6.666853767972947153, 1.538155548931797956, -1.385880503156889487 ) ) ;
#121067 = CARTESIAN_POINT ( 'NONE',  ( 1.493767781312784981, -2.000855510370867840, 0.2496291452861176263 ) ) ;
#121068 = CARTESIAN_POINT ( 'NONE',  ( -8.296699936558862731, 11.76690146170562201, 1.199719254218453823 ) ) ;
#121069 = CARTESIAN_POINT ( 'NONE',  ( 7.666209513884374438, 7.908608952478760834, 0.7998128361456281477 ) ) ;
#121070 = PLANE ( 'NONE',  #201672 ) ;
#121071 = CARTESIAN_POINT ( 'NONE',  ( 1.412352946837617473, 1.469754387505791460, -1.625674263109680329 ) ) ;
#121072 = CARTESIAN_POINT ( 'NONE',  ( 5.742758765878789085, 0.3605303665093101406, 1.789564367143759327 ) ) ;
#121073 = CARTESIAN_POINT ( 'NONE',  ( -2.625475302540713152, 6.214804952939456228, -0.7998128361456281477 ) ) ;
#121074 = EDGE_CURVE ( 'NONE', #152353, #23324, #89226, .T. ) ;
#121075 = CARTESIAN_POINT ( 'NONE',  ( 7.024532985656141371, 7.367912369453226695, 0.7216878364870328300 ) ) ;
#121076 = CARTESIAN_POINT ( 'NONE',  ( 9.154780037725547714, 11.70366268214508487, 1.599625672291279388 ) ) ;
#121077 = CARTESIAN_POINT ( 'NONE',  ( -6.466312919074983512, 6.508729591867735031, -0.7998128361456362523 ) ) ;
#121078 = CARTESIAN_POINT ( 'NONE',  ( 2.842405760359353106, 6.467890487061221272, -0.7998128361456291469 ) ) ;
#121079 = CARTESIAN_POINT ( 'NONE',  ( 4.146814880933355596, 5.931313009212638931, 1.599625672291261402 ) ) ;
#121080 = VERTEX_POINT ( 'NONE', #192946 ) ;
#121082 = CARTESIAN_POINT ( 'NONE',  ( 6.135026823787811168, 1.880036687389478489, 0.7205229627402914838 ) ) ;
#121081 = CARTESIAN_POINT ( 'NONE',  ( 3.456447201099471123, -1.625387274077850996, -0.8650149607793489182 ) ) ;
#121083 = CARTESIAN_POINT ( 'NONE',  ( 1.546695614565428922, 2.123301925303363369, -0.8802762395820094010 ) ) ;
#121085 = CARTESIAN_POINT ( 'NONE',  ( 6.561383603009730336, 1.629167342741120406, 1.092533971175007723 ) ) ;
#121084 = CARTESIAN_POINT ( 'NONE',  ( 4.528060117284240071, 5.345453560662148718, 1.082531754730560403 ) ) ;
#121086 = CARTESIAN_POINT ( 'NONE',  ( -3.716906668440817185, 7.488141546489591072, 0.7998128361456341429 ) ) ;
#121087 = FACE_OUTER_BOUND ( 'NONE', #73794, .T. ) ;
#121088 = CARTESIAN_POINT ( 'NONE',  ( 3.445477555875466891, -1.765175379189663607, 0.7362804355328657069 ) ) ;
#121089 = CARTESIAN_POINT ( 'NONE',  ( -9.646789991323334590, 11.21334206375407305, 1.199719254218462483 ) ) ;
#121090 = CARTESIAN_POINT ( 'NONE',  ( 6.132331002353889282, 6.987295666328819266, -0.9434213173033257904 ) ) ;
#121091 = CARTESIAN_POINT ( 'NONE',  ( -4.821859908315634158, 5.654533310236863564, 1.199719254218452935 ) ) ;
#121093 = CARTESIAN_POINT ( 'NONE',  ( 1.428351348257720588, 1.801920623737063520, 0.5021531274154652502 ) ) ;
#121092 = CARTESIAN_POINT ( 'NONE',  ( 2.982061477060811150, -2.060241282245252048, -0.3548380112704754286 ) ) ;
#121094 = CARTESIAN_POINT ( 'NONE',  ( 2.231795861093866851, -1.842164517099669441, -0.8196493499348647127 ) ) ;
#121095 = CARTESIAN_POINT ( 'NONE',  ( 8.595506201384013778, 10.09080732544527592, 1.082531754730558626 ) ) ;
#121096 = CARTESIAN_POINT ( 'NONE',  ( -0.6823417656249969321, 3.780208333674754506, -1.181850606188749264 ) ) ;
#121097 = CARTESIAN_POINT ( 'NONE',  ( 3.333312927339195930, 0.7792813341828198626, -1.556285420506423600 ) ) ;
#121098 = TOROIDAL_SURFACE ( 'NONE', #69029, -0.1799999999926198968, 0.5000000000000013323 ) ;
#121099 = CARTESIAN_POINT ( 'NONE',  ( 2.998324526916512411, 6.649795714711241423, 0.000000000000000000 ) ) ;
#121100 = CYLINDRICAL_SURFACE ( 'NONE', #89308, 0.3999999999999996336 ) ;
#121101 = CARTESIAN_POINT ( 'NONE',  ( 3.422183312176851455, 1.093272757541150719, -1.334144266598129791 ) ) ;
#121102 = CARTESIAN_POINT ( 'NONE',  ( 3.351304529449970371, 0.5305821810032870234, -2.126252377916526992 ) ) ;
#121103 = CARTESIAN_POINT ( 'NONE',  ( 5.813141826352885566, 1.944573597739504889, 1.043518232037063287 ) ) ;
#121104 = CARTESIAN_POINT ( 'NONE',  ( -10.37923916842784422, 4.890109552615133026, -5.358306740738790097 ) ) ;
#121106 = CARTESIAN_POINT ( 'NONE',  ( 3.520551232162504540, 0.9717998864677798165, 1.941468132180910189 ) ) ;
#121105 = B_SPLINE_CURVE_WITH_KNOTS ( 'NONE', 3,
 ( #169716, #115687, #2918, #83119, #185953, #17040, #197935, #99392, #68991, #37585 ),
 .UNSPECIFIED., .F., .F.,
 ( 4, 2, 2, 2, 4 ),
 ( 0.002464548724426622421, 0.002919784301308119001, 0.003375019878189615581, 0.003830255455071112161, 0.004285491031952610476 ),
 .UNSPECIFIED. ) ;
#121107 = CARTESIAN_POINT ( 'NONE',  ( 1.681982107312831154, -0.9779208310041755947, 1.541497997293653555 ) ) ;
#121108 = CARTESIAN_POINT ( 'NONE',  ( 4.580108180932601414, 8.499999999999996447, -0.1719113009628105149 ) ) ;
#121109 = CARTESIAN_POINT ( 'NONE',  ( 4.346934998023818331, -1.892857631927163498, -0.9488708475321022684 ) ) ;
#121110 = CARTESIAN_POINT ( 'NONE',  ( 11.78331023100045627, 11.37999999999999901, -1.800000000000001155 ) ) ;
#121111 = ADVANCED_FACE ( 'NONE', ( #10990 ), #174607, .F. ) ;
#121112 = ORIENTED_EDGE ( 'NONE', *, *, #179509, .F. ) ;
#121114 = CARTESIAN_POINT ( 'NONE',  ( -1.364683531250012516, 3.051041667008083547, -0.7879004041258289570 ) ) ;
#121113 = CARTESIAN_POINT ( 'NONE',  ( 4.880587636231574322, -0.2790779774165750293, -2.275280792031343147 ) ) ;
#121115 = CARTESIAN_POINT ( 'NONE',  ( 6.720655732516650716, 2.984497329163855461, 2.280179935440066252 ) ) ;
#121116 = CARTESIAN_POINT ( 'NONE',  ( 2.218730694130720771, 5.740269576461138890, 0.7998128361456462443 ) ) ;
#121117 = CARTESIAN_POINT ( 'NONE',  ( 0.5750489506927083383, -1.533040007955801531, 1.465245631482835043 ) ) ;
#121118 = CARTESIAN_POINT ( 'NONE',  ( -7.063434843039784639, 7.343021526408956667, 1.040834085586084257E-14 ) ) ;
#121119 = VECTOR ( 'NONE', #38882, 1000.000000000000000 ) ;
#121120 = CARTESIAN_POINT ( 'NONE',  ( -2.535011536075371996, 5.133042487381361596, 2.420000000000010587 ) ) ;
#121121 = CARTESIAN_POINT ( 'NONE',  ( -4.406036734316882253, 8.084200590104265061, -0.7216878364870257245 ) ) ;
#121122 = CARTESIAN_POINT ( 'NONE',  ( -10.99943592164173012, -9.900000000000019895, 0.1113975120799794716 ) ) ;
#121123 = VERTEX_POINT ( 'NONE', #57633 ) ;
#121124 = CARTESIAN_POINT ( 'NONE',  ( 5.766250055133458119, 1.862018000461727052, -0.7743128548072516493 ) ) ;
#121126 = CARTESIAN_POINT ( 'NONE',  ( 3.379784452013841367, -1.989113752706978433, 0.5454275443767720999 ) ) ;
#121125 = CARTESIAN_POINT ( 'NONE',  ( 6.145923705696426431, 6.064665832934283962, 0.7998128361456341429 ) ) ;
#121128 = CARTESIAN_POINT ( 'NONE',  ( -0.2411972340276230808, 0.2378665717568603510, -1.934216014300967235 ) ) ;
#121127 = CARTESIAN_POINT ( 'NONE',  ( 7.503511670520385479, 7.718794801887437274, 0.7998128361456281477 ) ) ;
#121129 = EDGE_CURVE ( 'NONE', #77503, #146971, #195085, .T. ) ;
#121130 = CARTESIAN_POINT ( 'NONE',  ( 7.038618024149998043, 8.240751112043669835, -1.199719254218452047 ) ) ;
#121131 = CARTESIAN_POINT ( 'NONE',  ( -3.285556943750000070, -2.209374999522041527, 0.000000000000000000 ) ) ;
#121132 = DIRECTION ( 'NONE',  ( -1.000000000000000000, 0.000000000000000000, 0.000000000000000000 ) ) ;
#121133 = CARTESIAN_POINT ( 'NONE',  ( 6.386699327874667986, 1.908680410311427655, -1.076638258889956345 ) ) ;
#121134 = CARTESIAN_POINT ( 'NONE',  ( 5.221327349844218091, 1.987046161919112430, 0.3419379449052239450 ) ) ;
#121135 = CARTESIAN_POINT ( 'NONE',  ( 3.069684041021227827, -1.094477399149307306, 1.480508570315848482 ) ) ;
#121136 = ADVANCED_FACE ( 'NONE', ( #191875 ), #76011, .F. ) ;
#121137 = CARTESIAN_POINT ( 'NONE',  ( 4.659198344590585350, 8.587481835331020719, 0.7998128361456462443 ) ) ;
#121138 = CARTESIAN_POINT ( 'NONE',  ( 0.5688600258280833710, 0.1761389027815796759, -1.715759018540372827 ) ) ;
#121139 = CARTESIAN_POINT ( 'NONE',  ( 1.108484992968819416, -0.04990477548066223068, 2.298298319747505758 ) ) ;
#121140 = CARTESIAN_POINT ( 'NONE',  ( -5.575427483717760424, 7.527751369135936343, 1.599625672291269396 ) ) ;
#121141 = CARTESIAN_POINT ( 'NONE',  ( 6.614178507701674370, -1.059427008983104601, -1.999161347636166930 ) ) ;
#121142 = CARTESIAN_POINT ( 'NONE',  ( 3.246800538002168945, 0.5120957664956159450, 2.042728137747833461 ) ) ;
#121143 = CARTESIAN_POINT ( 'NONE',  ( -4.014095998097799267, 6.840806543492835345, -1.199719254218450271 ) ) ;
#121144 = CARTESIAN_POINT ( 'NONE',  ( 7.884230021546724920, 9.157022099014721306, 1.199719254218462483 ) ) ;
#121145 = CARTESIAN_POINT ( 'NONE',  ( 6.821160681006793070, 7.130644680695653825, 0.7216878364870328300 ) ) ;
#121146 = DIRECTION ( 'NONE',  ( -0.7584648096782109494, 0.4241298465061392187, 0.4948181542571714053 ) ) ;
#121147 = CARTESIAN_POINT ( 'NONE',  ( -7.874588291438845644, 8.081441182967111558, -0.7998128361456291469 ) ) ;
#121148 = CARTESIAN_POINT ( 'NONE',  ( 6.439759776366769550, 8.536139043893143707, 1.443375672974076540 ) ) ;
#121149 = CARTESIAN_POINT ( 'NONE',  ( 4.901917485988815493, 6.882077164048857831, 1.422854466155202502 ) ) ;
#121150 = CARTESIAN_POINT ( 'NONE',  ( -5.599681137644054729, 6.491715067794862293, 1.199719254218450271 ) ) ;
#121151 = CARTESIAN_POINT ( 'NONE',  ( 4.465202103771027886, -1.783222260262930181, 1.324459880397445666 ) ) ;
#121152 = CARTESIAN_POINT ( 'NONE',  ( 2.607599380506659514, -2.167453834138896696, 0.3226137089109848421 ) ) ;
#121153 = CARTESIAN_POINT ( 'NONE',  ( -5.900823170445743671, 7.907379670318584353, 1.599625672291269396 ) ) ;
#121154 = CARTESIAN_POINT ( 'NONE',  ( -3.637330350216213759, 7.465578851886037093, -0.7998128361456481317 ) ) ;
#121155 = CARTESIAN_POINT ( 'NONE',  ( 5.195737816846159873, -1.386088135442983260, -1.388664821390848347 ) ) ;
#121156 = CARTESIAN_POINT ( 'NONE',  ( 0.6823417656249899377, 2.092708333674753174, 1.181850606188767472 ) ) ;
#121157 = CARTESIAN_POINT ( 'NONE',  ( 6.610000000000028741, 4.695285100415147461, 2.562642482393460597 ) ) ;
#121158 = CARTESIAN_POINT ( 'NONE',  ( -6.263503779833496488, 6.409768619334935913, 0.7216878364870317197 ) ) ;
#121159 = CARTESIAN_POINT ( 'NONE',  ( 4.623349522974431025, 1.846400237221163865, 1.042759738753673338 ) ) ;
#121160 = CARTESIAN_POINT ( 'NONE',  ( -4.146814880933400005, 5.931313009212638931, 1.599625672291270506 ) ) ;
#121161 = ORIENTED_EDGE ( 'NONE', *, *, #213932, .F. ) ;
#121162 = CARTESIAN_POINT ( 'NONE',  ( 5.084929678302336775, -0.2608814864752464491, -2.145832476913120068 ) ) ;
#121163 = CARTESIAN_POINT ( 'NONE',  ( 5.575427483717746213, 7.527751369135936343, 1.599625672291267398 ) ) ;
#121164 = CARTESIAN_POINT ( 'NONE',  ( 4.950658015114751009, -1.558304906039936988, -0.9804572199803849308 ) ) ;
#121165 = CARTESIAN_POINT ( 'NONE',  ( -5.660981573724272131, 6.153771497223376130, 0.8018600159674215133 ) ) ;
#121166 = CARTESIAN_POINT ( 'NONE',  ( -0.6823417656250003738, 1.030208333674752286, -1.181850606188749264 ) ) ;
#121167 = CARTESIAN_POINT ( 'NONE',  ( 0.08108764725259924588, -0.8233000410203991093, 1.533359828670758374 ) ) ;
#121168 = CARTESIAN_POINT ( 'NONE',  ( -2.974142338115852269, 6.685868392857900133, 0.1038623869373533903 ) ) ;
#121169 = CARTESIAN_POINT ( 'NONE',  ( -1.402160292154681736E-14, -1.115624999658584082, 1.575800808251672791 ) ) ;
#121170 = CARTESIAN_POINT ( 'NONE',  ( -1.045839947578414805E-15, 1.812499999999992673, 1.224999999999988987 ) ) ;
#121171 = COLOUR_RGB ( '', 0.66274510, 0.83137255, 0.94901961) ;
#121172 = CARTESIAN_POINT ( 'NONE',  ( 4.118171802502921253, -1.108985364570359566, -1.855417305202881506 ) ) ;
#121173 = CARTESIAN_POINT ( 'NONE',  ( -3.086452525405351643, 6.752611712948207057, 0.7998128361456341429 ) ) ;
#121174 = CARTESIAN_POINT ( 'NONE',  ( -6.507550544435101614, 10.53596670190887963, 0.000000000000000000 ) ) ;
#121175 = CARTESIAN_POINT ( 'NONE',  ( 4.047864428982482110, 0.7307185629543844207, -2.034579650689218866 ) ) ;
#121176 = CARTESIAN_POINT ( 'NONE',  ( 4.464113681242611875, 0.9267091202830781693, 1.739933209567791073 ) ) ;
#121177 = CARTESIAN_POINT ( 'NONE',  ( 3.760871765136180933, -1.731833850012770126, -0.08630056690941270703 ) ) ;
#121178 = CARTESIAN_POINT ( 'NONE',  ( 1.242012060539962492, 2.189267750446591609, 0.1026977899005257211 ) ) ;
#121179 = CARTESIAN_POINT ( 'NONE',  ( 2.169360633853111509, -2.109970246048063380, -0.9347365353246681607 ) ) ;
#121180 = CARTESIAN_POINT ( 'NONE',  ( 3.743479925124373331, -1.557965094614376378, -1.348979221448711519 ) ) ;
#121181 = CARTESIAN_POINT ( 'NONE',  ( 6.005412763054238212, -1.926851508234005195, 0.2422190414417753623 ) ) ;
#121183 = EDGE_LOOP ( 'NONE', ( #135157, #29014, #115003, #154029 ) ) ;
#121182 = CARTESIAN_POINT ( 'NONE',  ( -8.039621902779392926, 9.442275643739831636, 1.082531754730558626 ) ) ;
#121184 = CARTESIAN_POINT ( 'NONE',  ( -4.457598643843001973, 8.422558527783969851, 0.000000000000000000 ) ) ;
#121185 = CARTESIAN_POINT ( 'NONE',  ( -11.88235317400313917, 13.75664239773029784, -0.9089793033029951452 ) ) ;
#121186 = CARTESIAN_POINT ( 'NONE',  ( -4.085803189671902480, 5.860132702740892263, -1.599625672291271394 ) ) ;
#121187 = CARTESIAN_POINT ( 'NONE',  ( -6.182154857707119255, 10.15633840072622363, 0.000000000000000000 ) ) ;
#121188 = CARTESIAN_POINT ( 'NONE',  ( 3.100804818134130780, -0.6391501652806098610, -2.112195066926085829 ) ) ;
#121189 = CARTESIAN_POINT ( 'NONE',  ( 3.285556943749998737, -3.492708332855374742, -1.896917185911906500 ) ) ;
#121190 = ORIENTED_EDGE ( 'NONE', *, *, #150613, .F. ) ;
#121191 = CARTESIAN_POINT ( 'NONE',  ( 0.7603355536747276044, -0.6198598984368717257, -1.754846704163029125 ) ) ;
#121192 = CARTESIAN_POINT ( 'NONE',  ( -0.1290005225502398323, 0.2247172878383028038, -2.207197350255707402 ) ) ;
#121193 = CYLINDRICAL_SURFACE ( 'NONE', #21198, 0.3999999999999997446 ) ;
#121194 = CARTESIAN_POINT ( 'NONE',  ( 4.264789376140788235, 7.497597942732838305, -1.024658161349981444 ) ) ;
#121196 = CARTESIAN_POINT ( 'NONE',  ( 6.925078400183593885, 7.051837472187183486, 2.742497896504832333 ) ) ;
#121195 = CARTESIAN_POINT ( 'NONE',  ( -6.600870636098118638, 6.767368133241304484, -0.2259646751960984468 ) ) ;
#121197 = CARTESIAN_POINT ( 'NONE',  ( 11.97181073603049484, 13.88000000000000256, 0.8318477717169565633 ) ) ;
#121198 = EDGE_LOOP ( 'NONE', ( #645, #141811, #102291, #116183 ) ) ;
#121199 = CARTESIAN_POINT ( 'NONE',  ( 2.166935907724653720, -1.883791910722651952, -0.8362540481525667646 ) ) ;
#121200 = CARTESIAN_POINT ( 'NONE',  ( 0.6801582343749970061, 0.5572916670080683144, -1.178068619123862515 ) ) ;
#121201 = CARTESIAN_POINT ( 'NONE',  ( -7.019370843573183194, 9.212351955633947043, 1.599625672291283607 ) ) ;
#121202 = FILL_AREA_STYLE ('',( #123347 ) ) ;
#121204 = EDGE_CURVE ( 'NONE', #207748, #20507, #73882, .T. ) ;
#121203 = DIRECTION ( 'NONE',  ( 0.000000000000000000, 0.000000000000000000, -1.000000000000000000 ) ) ;
#121205 = CARTESIAN_POINT ( 'NONE',  ( 5.345992642490140057, 5.131412925860272090, 1.040834085586084257E-14 ) ) ;
#121206 = CARTESIAN_POINT ( 'NONE',  ( 1.920846698078120474, 1.922532266116746325, 0.7428477115608185244 ) ) ;
#121208 = CARTESIAN_POINT ( 'NONE',  ( 0.6823417656249934904, 13.69270833367473195, 1.181850606188764807 ) ) ;
#121207 = LINE ( 'NONE', #88634, #111137 ) ;
#121209 = CARTESIAN_POINT ( 'NONE',  ( 6.681470773436232413, 6.689470745297396270, -0.7998128361456281477 ) ) ;
#121210 = CARTESIAN_POINT ( 'NONE',  ( 3.620328817674754340, 3.489345133411980715, 2.447831560964480513 ) ) ;
#121211 = CARTESIAN_POINT ( 'NONE',  ( 5.584669497696876483, -2.152379054646291756, -0.4867646435422824935 ) ) ;
#121212 = CARTESIAN_POINT ( 'NONE',  ( 0.7026770610618977564, -0.7276074859871293210, -2.035605373553108777 ) ) ;
#121213 = CARTESIAN_POINT ( 'NONE',  ( -5.924549939491850381, 6.014322472269677533, 0.000000000000000000 ) ) ;
#121214 = CARTESIAN_POINT ( 'NONE',  ( 0.05278957052760185897, 0.3289079202175131389, 1.883742972368242174 ) ) ;
#121215 = CARTESIAN_POINT ( 'NONE',  ( 1.165250339122084533, 1.861343190080061882, -0.7762330495894869120 ) ) ;
#121216 = CARTESIAN_POINT ( 'NONE',  ( 0.000000000000000000, 8.999999999999998224, 0.000000000000000000 ) ) ;
#121217 = CARTESIAN_POINT ( 'NONE',  ( 1.476342052747819045, 2.027250371889641301, 1.083024425860839690 ) ) ;
#121218 = CARTESIAN_POINT ( 'NONE',  ( -5.204170427930421283E-15, -6.796015482748915204, -10.25773349932950929 ) ) ;
#121219 = CARTESIAN_POINT ( 'NONE',  ( 6.358066468859800757, 0.7272683628555456359, -1.768788954293845528 ) ) ;
#121220 = PRESENTATION_STYLE_ASSIGNMENT (( #169870 ) ) ;
#121221 = CARTESIAN_POINT ( 'NONE',  ( 1.815107966846595255, -0.2319292346777863389, 1.856160199827073587 ) ) ;
#121222 = CARTESIAN_POINT ( 'NONE',  ( 3.520720487665735643, 0.3006478860226591276, 1.993893439002386581 ) ) ;
#121224 = CARTESIAN_POINT ( 'NONE',  ( 11.55950211276791251, 13.79999999999998472, 3.221476510067111665 ) ) ;
#121223 = CARTESIAN_POINT ( 'NONE',  ( -1.201851678989727383E-14, 1.321875000341419248, 1.575800808251672791 ) ) ;
#121226 = CARTESIAN_POINT ( 'NONE',  ( 5.285806214103678791, 1.413684203821091945, 1.561263235811745309 ) ) ;
#121225 = CARTESIAN_POINT ( 'NONE',  ( -9.664264568442742842, 10.16939683947169115, -0.7998128361456291469 ) ) ;
#121227 = CARTESIAN_POINT ( 'NONE',  ( 7.151035956204054855, 10.43029348462504124, 1.199719254218460707 ) ) ;
#121229 = CARTESIAN_POINT ( 'NONE',  ( -7.283754839039664475, 9.520799950344851936, -1.599625672291263179 ) ) ;
#121228 = CARTESIAN_POINT ( 'NONE',  ( 5.571474780572990504, 5.464751763615448787, 0.7998128361456352531 ) ) ;
#121230 = CARTESIAN_POINT ( 'NONE',  ( -0.1062647697984078210, -6.683951901172095589, -9.488025208946956113 ) ) ;
#121231 = CARTESIAN_POINT ( 'NONE',  ( 4.342060261306793123, -1.245981751006501437, -1.589553384294100091 ) ) ;
#121232 = CARTESIAN_POINT ( 'NONE',  ( -0.6823417656249969321, 4.467708333674755394, -1.181850606188749264 ) ) ;
#121233 = CARTESIAN_POINT ( 'NONE',  ( 6.478975546884585768, 1.923237475310497047, 0.7459448616168369295 ) ) ;
#121234 = CARTESIAN_POINT ( 'NONE',  ( 9.463228032658635769, 11.10314946193233965, -1.082531754730543083 ) ) ;
#121235 = CARTESIAN_POINT ( 'NONE',  ( 5.079442160427912967, 2.018932005888602887, -0.7727740077691500620 ) ) ;
#121236 = CARTESIAN_POINT ( 'NONE',  ( 5.176180785367283654, 9.260904359562321275, -0.7998128361456481317 ) ) ;
#121237 = CARTESIAN_POINT ( 'NONE',  ( 1.364683531249986981, -1.053124999658580752, 0.000000000000000000 ) ) ;
#121239 = CARTESIAN_POINT ( 'NONE',  ( 9.681502816803464029, 4.134754161804807815, -7.090028435276412466 ) ) ;
#121238 = CARTESIAN_POINT ( 'NONE',  ( 7.028976294042106332, 7.165170195996068969, 0.000000000000000000 ) ) ;
#121240 = CARTESIAN_POINT ( 'NONE',  ( 6.439759776366758892, 10.45687747249582955, 0.7216878364870438212 ) ) ;
#121242 = DIRECTION ( 'NONE',  ( 0.8164965809277274778, -1.132850316508781087E-13, -0.5773502691896237327 ) ) ;
#121241 = CARTESIAN_POINT ( 'NONE',  ( 3.385384905382606391, 0.05040654291960967176, 2.170743301239473233 ) ) ;
#121244 = CARTESIAN_POINT ( 'NONE',  ( 1.610644152589552958, -0.2245515952020246675, 1.827417025815617935 ) ) ;
#121243 = CARTESIAN_POINT ( 'NONE',  ( -4.744990575102892905, 8.479646737687938085, 0.7216878364870458196 ) ) ;
#121245 = CARTESIAN_POINT ( 'NONE',  ( 1.364683531249990311, 3.134375000341423245, 1.214306433183764966E-14 ) ) ;
#121246 = CARTESIAN_POINT ( 'NONE',  ( 3.562233144267571650, -1.470601008620987749, 1.625073949779440419 ) ) ;
#121247 = CARTESIAN_POINT ( 'NONE',  ( 6.983263157960365675, 7.629137130509070275, 2.653810918356712900 ) ) ;
#121248 = CARTESIAN_POINT ( 'NONE',  ( 3.344836307015612409, 0.5477570922035517320, 2.195101814764536030 ) ) ;
#121249 = CARTESIAN_POINT ( 'NONE',  ( -6.728924311084075960, 6.744833205886536120, 1.040834085586084257E-14 ) ) ;
#121250 = CARTESIAN_POINT ( 'NONE',  ( -1.201851678989727383E-14, 5.509375000341415252, -1.575800808251660134 ) ) ;
#121251 = CARTESIAN_POINT ( 'NONE',  ( 6.132331002353889282, 6.987295666328819266, -0.9434213173033257904 ) ) ;
#121252 = CARTESIAN_POINT ( 'NONE',  ( -1.402160292154681736E-14, 13.81250000000000000, 1.732050807568881190 ) ) ;
#121253 = CARTESIAN_POINT ( 'NONE',  ( 5.614485009834906393, 6.683225611963085733, -1.082531754730548412 ) ) ;
#121254 = CARTESIAN_POINT ( 'NONE',  ( 5.817594836490700416, -1.726241941513080747, 0.3891773745644273030 ) ) ;
#121255 = CARTESIAN_POINT ( 'NONE',  ( 2.292140615954643579, -0.9012634372634602542, 1.903512165690796065 ) ) ;
#121257 = CARTESIAN_POINT ( 'NONE',  ( -1.500000000000011324, 2.670833333333352044, 0.8660254037844403729 ) ) ;
#121256 = CARTESIAN_POINT ( 'NONE',  ( 0.6823417656249969321, 12.27604166700806054, -1.181850606188757036 ) ) ;
#121258 = CARTESIAN_POINT ( 'NONE',  ( 0.6077773097897182231, 0.6213696771984353884, -1.869019927991413921 ) ) ;
#121259 = CARTESIAN_POINT ( 'NONE',  ( -3.122120512896910505, 6.864500708346841229, 0.7998128361456352531 ) ) ;
#121260 = CARTESIAN_POINT ( 'NONE',  ( -0.006768871532359390167, 8.210909518262125673, -2.038649385027042626 ) ) ;
#121262 = ORIENTED_EDGE ( 'NONE', *, *, #170740, .F. ) ;
#121261 = CARTESIAN_POINT ( 'NONE',  ( 5.853729002925880387, -1.318332981873654441, -1.242799640730863464 ) ) ;
#121263 = CARTESIAN_POINT ( 'NONE',  ( 7.321039761699430493, 7.643560598178549270, -0.7216878364870257245 ) ) ;
#121264 = CARTESIAN_POINT ( 'NONE',  ( -1.364683531250000748, -0.1781249996585798634, 0.000000000000000000 ) ) ;
#121265 = ADVANCED_FACE ( 'NONE', ( #159391 ), #96664, .T. ) ;
#121266 = CARTESIAN_POINT ( 'NONE',  ( 4.364026845288040413, 0.8817440624687390427, 1.649792572839225091 ) ) ;
#121267 = CARTESIAN_POINT ( 'NONE',  ( 5.946161111532238586, -0.9360204806616537754, 1.846680006623670156 ) ) ;
#121268 = CARTESIAN_POINT ( 'NONE',  ( -1.225000000000004086, 1.979166666666657193, -0.7072540797572898219 ) ) ;
#121269 = CARTESIAN_POINT ( 'NONE',  ( -5.600926855776894975, 6.667407765562058053, -1.082531754730549967 ) ) ;
#121270 = CARTESIAN_POINT ( 'NONE',  ( -1.402160292154681736E-14, 0.3375000000000208389, -1.732050807568870754 ) ) ;
#121271 = CARTESIAN_POINT ( 'NONE',  ( 6.751070424600909448, 9.963667031088037973, -1.199719254218441611 ) ) ;
#121272 = CARTESIAN_POINT ( 'NONE',  ( -8.533967624797991647, 12.04371376465130439, -1.199719254218446718 ) ) ;
#121273 = CARTESIAN_POINT ( 'NONE',  ( 7.367930134383754215, 7.560616343061329125, -0.7998128361456341429 ) ) ;
#121274 = CARTESIAN_POINT ( 'NONE',  ( 0.6823417656249882723, 0.4260416670080896528, -1.181850606188749264 ) ) ;
#121275 = CARTESIAN_POINT ( 'NONE',  ( -1.500000000000013101, 1.420833333333354043, 0.8660254037844403729 ) ) ;
#121277 = CARTESIAN_POINT ( 'NONE',  ( 5.983225862332436584, 5.874851682342960402, 0.7998128361456341429 ) ) ;
#121276 = CARTESIAN_POINT ( 'NONE',  ( 5.318788500806308051, -1.422220495204097546, 1.351624447685224162 ) ) ;
#121278 = CARTESIAN_POINT ( 'NONE',  ( 1.809922493048341074, -1.704678386728165185, 1.076150803433255865 ) ) ;
#121279 = CARTESIAN_POINT ( 'NONE',  ( 6.966220764712143243, 6.002124920821316323, -2.420000000000000373 ) ) ;
#121280 = CARTESIAN_POINT ( 'NONE',  ( 0.3456114054924685486, 0.6817542107791437767, -2.082909237240769151 ) ) ;
#121281 = CARTESIAN_POINT ( 'NONE',  ( -11.84668729410370602, 10.09379487675469633, 1.399999999999998357 ) ) ;
#121282 = CARTESIAN_POINT ( 'NONE',  ( 2.354581831802166736, -1.448805955455864769, 1.183207591018392568 ) ) ;
#121283 = CARTESIAN_POINT ( 'NONE',  ( 1.364683531249988535, 5.155208333674749177, -0.7879004041258300672 ) ) ;
#121284 = CARTESIAN_POINT ( 'NONE',  ( 3.885024706246028803, -1.880017414580990032, -0.7205730073996403640 ) ) ;
#121285 =( REPRESENTATION_RELATIONSHIP ('NONE','NONE', #84563, #211717 ) REPRESENTATION_RELATIONSHIP_WITH_TRANSFORMATION ( #188989 )SHAPE_REPRESENTATION_RELATIONSHIP( ) );
#121286 = CARTESIAN_POINT ( 'NONE',  ( -7.374745490829552885, 10.69128794168811680, -1.199719254218446718 ) ) ;
#121288 = CARTESIAN_POINT ( 'NONE',  ( 4.499685226448436381, -2.076086866053193258, 0.4145649545581850393 ) ) ;
#121287 = CARTESIAN_POINT ( 'NONE',  ( -4.229780737783618072, 6.918199379847403740, 1.082531754730560403 ) ) ;
#121289 = CARTESIAN_POINT ( 'NONE',  ( -1.886825320689270225, 2.480000000000016858, -2.459652456995881753 ) ) ;
#121290 = CARTESIAN_POINT ( 'NONE',  ( 6.373496627357888578, -0.2573980274669443458, 2.054251119134167691 ) ) ;
#121292 = CARTESIAN_POINT ( 'NONE',  ( 6.720655732516647163, -0.001531948155462491612, 2.073773125298985054 ) ) ;
#121291 = CARTESIAN_POINT ( 'NONE',  ( 1.030938747749777118, -1.888616091942503461, 0.8971857714693499686 ) ) ;
#121294 = ORIENTED_EDGE ( 'NONE', *, *, #129667, .F. ) ;
#121293 = CARTESIAN_POINT ( 'NONE',  ( 6.317409609008933558, -0.2203418483949574069, 1.812181760327068680 ) ) ;
#121295 = EDGE_CURVE ( 'NONE', #153422, #56362, #186446, .T. ) ;
#121296 = CARTESIAN_POINT ( 'NONE',  ( 6.753933077901968396, 11.03133902419432566, 0.7998128361456462443 ) ) ;
#121297 = CARTESIAN_POINT ( 'NONE',  ( 7.886602582589865129, -6.765616048178569208, -7.668547801473498460 ) ) ;
#121298 = CARTESIAN_POINT ( 'NONE',  ( -11.94105721237523277, 13.40000000000000036, 1.187919463087245386 ) ) ;
#121299 = CARTESIAN_POINT ( 'NONE',  ( -10.81012925547440773, 5.523932969818027949, 6.547168141744070802 ) ) ;
#121300 = CARTESIAN_POINT ( 'NONE',  ( 6.426201622753093368, 10.44105962661321563, 1.040834085586084257E-14 ) ) ;
#121301 = CARTESIAN_POINT ( 'NONE',  ( 1.364683531250000748, 12.81770833367473372, -0.7879004041258355073 ) ) ;
#121302 = CARTESIAN_POINT ( 'NONE',  ( 6.111958284735683478, -0.6397702040911549259, 1.802229686255519603 ) ) ;
#121303 = CARTESIAN_POINT ( 'NONE',  ( -6.496328159242330536, 10.73079995242472862, 0.000000000000000000 ) ) ;
#121304 = CARTESIAN_POINT ( 'NONE',  ( 6.179819089730593795, 6.104210447640811665, 1.040834085586084257E-14 ) ) ;
#121305 = CARTESIAN_POINT ( 'NONE',  ( -1.364683531250000748, 8.359375000341396245, 0.000000000000000000 ) ) ;
#121306 = CARTESIAN_POINT ( 'NONE',  ( 1.220146605508150803E-14, 9.937500000000000000, -1.499999999999998446 ) ) ;
#121307 = EDGE_CURVE ( 'NONE', #200740, #37563, #105732, .T. ) ;
#121308 = CARTESIAN_POINT ( 'NONE',  ( 2.198393463710220264, 5.716542807637226886, 0.7998128361456462443 ) ) ;
#121309 = VERTEX_POINT ( 'NONE', #169537 ) ;
#121310 = AXIS2_PLACEMENT_3D ( 'NONE', #4784, #73012, #8013 ) ;
#121311 = CARTESIAN_POINT ( 'NONE',  ( 5.571888728144736902, -0.9040954357531080232, 1.802425742427179012 ) ) ;
#121312 = CARTESIAN_POINT ( 'NONE',  ( 0.2586463447097427926, 2.115114616003030079, 0.1516365082330217162 ) ) ;
#121313 = DIRECTION ( 'NONE',  ( 1.276756478318932585E-15, -1.000000000000000000, 1.665334536937738262E-16 ) ) ;
#121314 = CARTESIAN_POINT ( 'NONE',  ( -0.1394461523061377994, 7.629137130509062281, -2.880276239818948536 ) ) ;
#121315 = CARTESIAN_POINT ( 'NONE',  ( -4.284013352238250860, 7.941839977679187257, -0.7216878364870267237 ) ) ;
#121316 = CARTESIAN_POINT ( 'NONE',  ( 10.22248463502393001, 11.02857961705718282, 0.7216878364870438212 ) ) ;
#121317 = CARTESIAN_POINT ( 'NONE',  ( 3.291813281336749331, -1.319317765291039946, -1.462433841519056532 ) ) ;
#121318 = CARTESIAN_POINT ( 'NONE',  ( 4.235953958900400274, 2.015913684659226490, -0.05231418598541925924 ) ) ;
#121319 = CARTESIAN_POINT ( 'NONE',  ( -7.314787569772770226, 8.492672571945082183, -1.199719254218452935 ) ) ;
#121320 = CARTESIAN_POINT ( 'NONE',  ( 0.000000000000000000, 3.799999999999998046, 6.249999999999995559 ) ) ;
#121321 = CARTESIAN_POINT ( 'NONE',  ( 5.121103774788174690, -2.081602751171758747, 0.6852947426586111224 ) ) ;
#121322 = DIRECTION ( 'NONE',  ( 0.000000000000000000, -0.7999999999999973799, -0.6000000000000034195 ) ) ;
#121323 = CARTESIAN_POINT ( 'NONE',  ( 3.364200941815390866, 0.8650686769993837233, 1.721291803412771992 ) ) ;
#121324 = CARTESIAN_POINT ( 'NONE',  ( -6.482770005628665011, 10.71498210654212002, 0.7998128361456481317 ) ) ;
#121325 = CARTESIAN_POINT ( 'NONE',  ( -0.02948999725182251466, 0.2504340119564217870, -1.961592983597350459 ) ) ;
#121326 = CARTESIAN_POINT ( 'NONE',  ( 0.3115100037339203487, 1.922317768103290803, 1.083863418116323807 ) ) ;
#121327 = EDGE_CURVE ( 'NONE', #210405, #74826, #193411, .T. ) ;
#121328 = CARTESIAN_POINT ( 'NONE',  ( -4.379728251965876673, 15.51893462891072595, -11.18122699412752397 ) ) ;
#121329 = CARTESIAN_POINT ( 'NONE',  ( 4.407809338218622308, 8.156544971314787063, 0.000000000000000000 ) ) ;
#121330 = VERTEX_POINT ( 'NONE', #200939 ) ;
#121331 = CARTESIAN_POINT ( 'NONE',  ( 5.722950238744211937, 5.849399164722627553, 0.7216878364870328300 ) ) ;
#121332 = CARTESIAN_POINT ( 'NONE',  ( 5.366046204681790499, -1.960318410495393238, 0.1889891646899461708 ) ) ;
#121333 = ORIENTED_EDGE ( 'NONE', *, *, #76048, .F. ) ;
#121335 = CARTESIAN_POINT ( 'NONE',  ( 4.301435403400270197, 1.797132274555211184, -0.9072848608384380675 ) ) ;
#121334 = CARTESIAN_POINT ( 'NONE',  ( 0.02871324022350740107, -1.775192216153992808, 0.7880070256306227483 ) ) ;
#121336 = CARTESIAN_POINT ( 'NONE',  ( 5.519047587058080850, 2.296088720628499669, -0.1051655125834053545 ) ) ;
#121338 = CARTESIAN_POINT ( 'NONE',  ( 3.643253357272932647, 1.684219189441754416, -0.7917782423425399063 ) ) ;
#121337 =( NAMED_UNIT ( * ) PLANE_ANGLE_UNIT ( ) SI_UNIT ( $, .RADIAN. ) );
#121339 = CARTESIAN_POINT ( 'NONE',  ( 5.989670002187236442, 10.20997511251894529, -0.7998128361456481317 ) ) ;
#121340 = CARTESIAN_POINT ( 'NONE',  ( -11.29689844398643572, -5.530538574611986391, 1.138412281109779656E-15 ) ) ;
#121341 = CYLINDRICAL_SURFACE ( 'NONE', #40203, 1.249999999999999778 ) ;
#121342 = CARTESIAN_POINT ( 'NONE',  ( -7.314787569772770226, 8.492672571945082183, -1.199719254218452935 ) ) ;
#121343 = CARTESIAN_POINT ( 'NONE',  ( -4.285785955695645910, 7.053815144069948140, 1.082531754730549967 ) ) ;
#121344 = CARTESIAN_POINT ( 'NONE',  ( 5.671452434703694756, 1.246268910035509991, 1.678523727997438986 ) ) ;
#121345 = CARTESIAN_POINT ( 'NONE',  ( 6.480434237652135998, 6.662854153456708950, 0.7216878364870317197 ) ) ;
#121346 = ORIENTED_EDGE ( 'NONE', *, *, #70880, .F. ) ;
#121347 = CARTESIAN_POINT ( 'NONE',  ( 4.686350348575522240, 8.284075936624162750, 0.5876776440279610769 ) ) ;
#121348 = CARTESIAN_POINT ( 'NONE',  ( 0.8557438351849018243, 1.823752217391808372, -0.08689656109241167270 ) ) ;
#121349 = CARTESIAN_POINT ( 'NONE',  ( -6.410307701162927252, 6.373113827645189744, -0.7998128361456291469 ) ) ;
#121350 = STYLED_ITEM ( 'NONE', ( #184964 ), #47143 ) ;
#121351 = CARTESIAN_POINT ( 'NONE',  ( 2.601899516932767220, -0.1674142849007881351, 1.726012112926772701 ) ) ;
#121352 = CARTESIAN_POINT ( 'NONE',  ( 1.000000000000003553, 6.120000000000020535, 1.214306433183764966E-14 ) ) ;
#121353 = CARTESIAN_POINT ( 'NONE',  ( -6.007394966791244961, 6.077829431809393945, -0.6506939885215150543 ) ) ;
#121354 = CARTESIAN_POINT ( 'NONE',  ( -5.693534442735004752, 8.729875052244421951, 1.199719254218452047 ) ) ;
#121355 = CARTESIAN_POINT ( 'NONE',  ( -5.854831387906667572, 6.034345315880532468, 0.4035957558334040685 ) ) ;
#121356 = CARTESIAN_POINT ( 'NONE',  ( 6.684450694706582929, 1.257157530024972658, -1.769884466434832548 ) ) ;
#121357 = CARTESIAN_POINT ( 'NONE',  ( 5.039593146249602640, -1.293522693445446015, -1.288650932716684849 ) ) ;
#121358 = CARTESIAN_POINT ( 'NONE',  ( 3.063279882407277999, 1.654721480355027863, 1.053479689057647217 ) ) ;
#121359 = CARTESIAN_POINT ( 'NONE',  ( 0.6124999999999811706, -0.2708333326505441008, -1.060881119635955327 ) ) ;
#121360 = CARTESIAN_POINT ( 'NONE',  ( -8.154339323615371171, 11.60081407993821045, 1.199719254218453823 ) ) ;
#121361 = CARTESIAN_POINT ( 'NONE',  ( 6.076025397218672630, 10.24044673006381245, -0.7998128361456291469 ) ) ;
#121362 = CARTESIAN_POINT ( 'NONE',  ( 4.020270485675044192, -2.114722421624544157, 0.1573160286183969692 ) ) ;
#121363 = CARTESIAN_POINT ( 'NONE',  ( 5.969332771766739931, 10.18624834369502885, -0.7998128361456481317 ) ) ;
#121364 = CARTESIAN_POINT ( 'NONE',  ( -10.08065090696061716, 11.71951313199760136, -1.199719254218441611 ) ) ;
#121365 = CARTESIAN_POINT ( 'NONE',  ( 1.235311698660218838, -0.04697018572753957483, -2.069874154031334790 ) ) ;
#121367 = CARTESIAN_POINT ( 'NONE',  ( -0.7500000000000179856, 14.57291666734946567, 1.299038105676658228 ) ) ;
#121366 =( LENGTH_UNIT ( ) NAMED_UNIT ( * ) SI_UNIT ( .MILLI., .METRE. ) );
#121369 = ORIENTED_EDGE ( 'NONE', *, *, #140872, .T. ) ;
#121368 = CARTESIAN_POINT ( 'NONE',  ( 4.442156590966897411, -1.366343709131916828, -1.751266766990001944 ) ) ;
#121370 = CARTESIAN_POINT ( 'NONE',  ( 2.092814488687055441, -0.4990534829178472354, 2.243750245495256035 ) ) ;
#121372 = CARTESIAN_POINT ( 'NONE',  ( 6.332891742935283119, -1.956728314951971637, -0.6523575503349694493 ) ) ;
#121371 = CARTESIAN_POINT ( 'NONE',  ( 8.866669273657322492, 12.32790267170016207, -1.082531754730543083 ) ) ;
#121374 = CARTESIAN_POINT ( 'NONE',  ( 3.475000000000000533, -0.9041666666666666741, 2.006292185433948827 ) ) ;
#121373 = CARTESIAN_POINT ( 'NONE',  ( 7.675324359112103423, 8.127168971818530707, 0.7216878364870267237 ) ) ;
#121375 = ADVANCED_FACE ( 'NONE', ( #153287 ), #599, .F. ) ;
#121376 = CARTESIAN_POINT ( 'NONE',  ( 0.000000000000000000, 8.500000000000000000, 0.000000000000000000 ) ) ;
#121377 = CARTESIAN_POINT ( 'NONE',  ( -10.94445979172680694, -5.609732095436336330, 0.02903434592766030581 ) ) ;
#121378 = CARTESIAN_POINT ( 'NONE',  ( -5.623048529261291506, 6.177845134385851367, -0.8520226256489031869 ) ) ;
#121379 = EDGE_CURVE ( 'NONE', #44633, #65489, #133989, .T. ) ;
#121380 = CARTESIAN_POINT ( 'NONE',  ( 2.566550162062298579, 0.6480892470011965223, 1.799338185917313870 ) ) ;
#121381 = CARTESIAN_POINT ( 'NONE',  ( -0.3532385256851401367, 6.953154881905717843, -3.904206509207633680 ) ) ;
#121382 = CARTESIAN_POINT ( 'NONE',  ( 4.401177694619070380, 1.385992036768167068, 1.026327495003590551 ) ) ;
#121383 = CARTESIAN_POINT ( 'NONE',  ( 2.571500236035813902, 1.429449181443824823, 1.422607194786096541 ) ) ;
#121384 = CARTESIAN_POINT ( 'NONE',  ( 4.149308075173010479, 1.083998706471595463, 2.027078093135482817 ) ) ;
#121385 = CARTESIAN_POINT ( 'NONE',  ( 3.726065177040696952, -1.343991584994163269, -1.819822530443465425 ) ) ;
#121386 = CARTESIAN_POINT ( 'NONE',  ( -0.004863692847738298151, -0.4900785244342681368, -2.159743284330918112 ) ) ;
#121387 = CARTESIAN_POINT ( 'NONE',  ( -6.617788377246204945, 6.893376992974917350, -0.7216878364870338292 ) ) ;
#121388 = VERTEX_POINT ( 'NONE', #132812 ) ;
#121389 = CARTESIAN_POINT ( 'NONE',  ( 4.850734264762338377, -1.421546097138610243, 1.053919008203674013 ) ) ;
#121391 = CARTESIAN_POINT ( 'NONE',  ( 1.043418098205237676, -1.810020423698131653, -1.406424589915030943 ) ) ;
#121390 = CARTESIAN_POINT ( 'NONE',  ( 6.526270840131753737, 8.707344961610770540, -1.599625672291283607 ) ) ;
#121392 = CARTESIAN_POINT ( 'NONE',  ( 5.367088761235753402, 1.773375748883701419, -0.4946613714205680967 ) ) ;
#121393 = CARTESIAN_POINT ( 'NONE',  ( -4.973143418114339021, 4.696422164088486895, 0.7998128361456341429 ) ) ;
#121394 = CARTESIAN_POINT ( 'NONE',  ( 6.228506716250251429, 0.2110190803071687327, 2.181275323772186248 ) ) ;
#121395 = CARTESIAN_POINT ( 'NONE',  ( -3.969505113751027547, 7.853116076009993840, 1.214306433183764966E-14 ) ) ;
#121396 = CARTESIAN_POINT ( 'NONE',  ( -4.783329267523015460, 4.474972321731942593, -0.7998128361456221525 ) ) ;
#121397 = CARTESIAN_POINT ( 'NONE',  ( -1.748073236337231107, 15.51991758800158117, 11.90628676210878822 ) ) ;
#121398 =( BOUNDED_CURVE ( )  B_SPLINE_CURVE ( 2, ( #116406, #168299, #49231, #52418, #69704, #19896, #17746, #35078, #117480 ),
 .UNSPECIFIED., .F., .T. ) 
 B_SPLINE_CURVE_WITH_KNOTS ( ( 3, 2, 2, 2, 3 ),
 ( 0.2341475240440091254, 0.2361111111111111049, 0.2500000000000000000, 0.2638888888888888951, 0.2708333333333333703 ),
 .UNSPECIFIED. ) 
 CURVE ( )  GEOMETRIC_REPRESENTATION_ITEM ( )  RATIONAL_B_SPLINE_CURVE ( ( 0.9674735258996458587, 0.9810589035196658481, 1.000000000000000000, 0.8660254037844387076, 1.000000000000000000, 0.8660254037844387076, 1.000000000000000000, 0.9330127018922190762, 0.9330127018922194093 ) ) 
 REPRESENTATION_ITEM ( '' )  );
#121399 = CARTESIAN_POINT ( 'NONE',  ( 5.318829906782316819, -1.502041817331278173, 1.425132596443792643 ) ) ;
#121400 = CARTESIAN_POINT ( 'NONE',  ( 1.604704241733472037, 1.883313803065278513, 0.7212895827233902768 ) ) ;
#121401 = CARTESIAN_POINT ( 'NONE',  ( -0.7500000000000006661, -0.8604166659838472508, -1.299038105676652011 ) ) ;
#121402 = CARTESIAN_POINT ( 'NONE',  ( 3.826716429392281071, 1.829700617163315002, 0.6032043533580729866 ) ) ;
#121403 = CARTESIAN_POINT ( 'NONE',  ( 1.364683531250000303, 10.75520833367473195, -0.7879004041258355073 ) ) ;
#121404 = CARTESIAN_POINT ( 'NONE',  ( 1.213460986420217047, 1.812193587075833667, -1.284517086575332367 ) ) ;
#121406 = ORIENTED_EDGE ( 'NONE', *, *, #211660, .F. ) ;
#121405 = CARTESIAN_POINT ( 'NONE',  ( 3.444653546323793947, 6.176457016423196222, 1.199719254218451159 ) ) ;
#121408 = CARTESIAN_POINT ( 'NONE',  ( 1.734723475976807094E-15, 0.2401923788623739342, 3.469446951953614189E-15 ) ) ;
#121407 = CARTESIAN_POINT ( 'NONE',  ( 1.468321960011987670, 7.242494692102993348, -4.289992922803929076 ) ) ;
#121409 = CARTESIAN_POINT ( 'NONE',  ( 2.205172540517054802, 5.724451730578533848, 1.040834085586084257E-14 ) ) ;
#121410 = CARTESIAN_POINT ( 'NONE',  ( 0.000000000000000000, 7.000000000000000000, 0.000000000000000000 ) ) ;
#121411 = DIRECTION ( 'NONE',  ( 0.000000000000000000, 0.000000000000000000, 1.000000000000000000 ) ) ;
#121412 = CARTESIAN_POINT ( 'NONE',  ( 5.510910596163088569E-16, -3.600000000000005862, 4.500000000000000000 ) ) ;
#121413 = CARTESIAN_POINT ( 'NONE',  ( 2.857805160684105950, -0.6180756922911297968, 1.862011555624979886 ) ) ;
#121415 = CARTESIAN_POINT ( 'NONE',  ( -1.364683531250012516, 2.842708333674754506, 0.7879004041258379498 ) ) ;
#121414 = CARTESIAN_POINT ( 'NONE',  ( 4.852928918687680948, 7.749168607522574526, 1.199719254218462483 ) ) ;
#121416 = CARTESIAN_POINT ( 'NONE',  ( 11.86239285000045740, 12.21999999999998288, 1.812080536912751061 ) ) ;
#121417 = CARTESIAN_POINT ( 'NONE',  ( 6.162552467866693640, -0.7048080804108979303, -1.831077584432870609 ) ) ;
#121418 = CARTESIAN_POINT ( 'NONE',  ( -8.727698198895085469, 11.20540053684285553, -1.599625672291263179 ) ) ;
#121419 = STYLED_ITEM ( 'NONE', ( #92346 ), #85507 ) ;
#121420 = CARTESIAN_POINT ( 'NONE',  ( -5.056828107772872727, 5.001980335264194721, -0.7216878364870197293 ) ) ;
#121421 = CARTESIAN_POINT ( 'NONE',  ( 5.296111364736042937, -0.9110065213352031011, -1.799124599017036585 ) ) ;
#121422 = CARTESIAN_POINT ( 'NONE',  ( 0.4446536212460248105, 2.256715800172736763, 0.1630166291790128841 ) ) ;
#121424 = ORIENTED_EDGE ( 'NONE', *, *, #28439, .F. ) ;
#121423 = CARTESIAN_POINT ( 'NONE',  ( -4.557512192488103686, 8.468847991211438497, -0.7998128361456281477 ) ) ;
#121425 = CARTESIAN_POINT ( 'NONE',  ( -1.500000000000015099, -1.089583332650509773, -0.8660254037844383745 ) ) ;
#121426 = CARTESIAN_POINT ( 'NONE',  ( 1.159204581426832803, 0.3705859133612994794, -1.833297903905316772 ) ) ;
#121427 = CARTESIAN_POINT ( 'NONE',  ( 6.854911444608583260, -0.7389736882487309977, 1.567799899397160912 ) ) ;
#121429 = CARTESIAN_POINT ( 'NONE',  ( 3.702820756938397295, 1.880440254450808757, 1.125299312022425280 ) ) ;
#121428 = CARTESIAN_POINT ( 'NONE',  ( 1.360316468749966257, 1.765625000341414230, -3.642919299551294898E-14 ) ) ;
#121430 = CARTESIAN_POINT ( 'NONE',  ( 5.719831105939597649, -2.253009325453013023, 0.4983019283236743702 ) ) ;
#121431 = B_SPLINE_CURVE_WITH_KNOTS ( 'NONE', 3,
 ( #7581, #109444, #175451, #27035, #76857, #72588 ),
 .UNSPECIFIED., .F., .F.,
 ( 4, 2, 4 ),
 ( 0.000000000000000000, 0.0003844267940947831432, 0.0007688535881895662864 ),
 .UNSPECIFIED. ) ;
#121432 = CARTESIAN_POINT ( 'NONE',  ( 6.714142707505978080, -0.9671387161254895171, -1.819716304366093551 ) ) ;
#121433 = CARTESIAN_POINT ( 'NONE',  ( 2.536971540620248433, -1.439279119694805820, -1.303886525222669901 ) ) ;
#121434 = CARTESIAN_POINT ( 'NONE',  ( -6.195713011320807873, 6.330679389403470303, -0.7216878364870267237 ) ) ;
#121435 = PRODUCT ( 'MAS-692', 'MAS-692', '', ( #150109 ) ) ;
#121436 = CARTESIAN_POINT ( 'NONE',  ( -2.820451594992841482, 6.512553637458760036, 0.000000000000000000 ) ) ;
#121437 = CARTESIAN_POINT ( 'NONE',  ( 4.584065335196260804, 6.441438539186039591, 1.443375672974065660 ) ) ;
#121438 = CARTESIAN_POINT ( 'NONE',  ( -0.6801582343750074422, 0.5989583336747372755, -1.178068619123841643 ) ) ;
#121439 = CARTESIAN_POINT ( 'NONE',  ( 3.006482587178582300, -1.942541511447487990, 0.5404910644229294903 ) ) ;
#121440 = CARTESIAN_POINT ( 'NONE',  ( -3.375617059678305054, 5.921675088724528635, 1.082531754730560403 ) ) ;
#121441 = CARTESIAN_POINT ( 'NONE',  ( -7.306918443122272677, 7.489436036589583345, 0.7998128361456341429 ) ) ;
#121442 = CARTESIAN_POINT ( 'NONE',  ( 9.694243528971124846, 11.26870452434320491, 1.199719254218450271 ) ) ;
#121444 = CARTESIAN_POINT ( 'NONE',  ( -6.981856502303775969, -6.709867743870995049, 6.429544252029575802 ) ) ;
#121443 = CARTESIAN_POINT ( 'NONE',  ( 0.7326872660318053398, 0.1314506862302306234, 1.821024990000128518 ) ) ;
#121445 = CARTESIAN_POINT ( 'NONE',  ( -5.773793314573309132, 7.829454515125894964, 1.599625672291263179 ) ) ;
#121446 = CARTESIAN_POINT ( 'NONE',  ( -4.630991987519598396, 7.560518531151607213, 1.199719254218452935 ) ) ;
#121447 = CARTESIAN_POINT ( 'NONE',  ( -10.32184838934336213, 3.007359993651753438, 7.367400555339857604 ) ) ;
#121448 = VERTEX_POINT ( 'NONE', #4863 ) ;
#121449 = CARTESIAN_POINT ( 'NONE',  ( 6.526252491562488878, 1.188822440972692185, -1.683233108126303446 ) ) ;
#121450 = CARTESIAN_POINT ( 'NONE',  ( -5.926322542504860458, 9.928143709648733051, -0.7216878364870338292 ) ) ;
#121451 = CARTESIAN_POINT ( 'NONE',  ( -3.602337597214539753E-15, 11.84375000068279604, 1.500000000000001554 ) ) ;
#121452 = FACE_OUTER_BOUND ( 'NONE', #187309, .T. ) ;
#121453 = CARTESIAN_POINT ( 'NONE',  ( 5.444012513273879250, -1.283034597847107161, -1.559753263307301463 ) ) ;
#121455 = ORIENTED_EDGE ( 'NONE', *, *, #130804, .F. ) ;
#121454 = CARTESIAN_POINT ( 'NONE',  ( 5.233148740271514221, 2.051824077619863296, 0.8514482647801949744 ) ) ;
#121456 = CARTESIAN_POINT ( 'NONE',  ( -7.370792787684826486, 8.628288336167626582, -1.199719254218452047 ) ) ;
#121457 = CARTESIAN_POINT ( 'NONE',  ( 4.984594031318565932, 8.967110136513669616, 0.7998128361456462443 ) ) ;
#121458 = MECHANICAL_DESIGN_GEOMETRIC_PRESENTATION_REPRESENTATION (  '', ( #38341 ), #100642 ) ;
#121459 = CARTESIAN_POINT ( 'NONE',  ( 5.067286680778130936, 0.2040240636430467047, -2.050771057314598966 ) ) ;
#121460 = CARTESIAN_POINT ( 'NONE',  ( 3.674454069786535548, 1.462445212485608437, 1.388486266691544957 ) ) ;
#121461 = ORIENTED_EDGE ( 'NONE', *, *, #166426, .T. ) ;
#121462 = DIRECTION ( 'NONE',  ( 1.000000000000000000, -0.000000000000000000, -0.000000000000000000 ) ) ;
#121463 = CARTESIAN_POINT ( 'NONE',  ( 4.891794496432329886, 4.601515088792824670, -0.7998128361456211532 ) ) ;
#121464 =( BOUNDED_CURVE ( )  B_SPLINE_CURVE ( 3, ( #137992, #188858, #6882, #40494 ),
 .UNSPECIFIED., .F., .T. ) 
 B_SPLINE_CURVE_WITH_KNOTS ( ( 4, 4 ),
 ( 0.000000000000000000, 0.4999999999999963918 ),
 .UNSPECIFIED. ) 
 CURVE ( )  GEOMETRIC_REPRESENTATION_ITEM ( )  RATIONAL_B_SPLINE_CURVE ( ( 1.000000000000000000, 0.3333333333333381998, 0.3333333333333333703, 0.9999999999999952260 ) ) 
 REPRESENTATION_ITEM ( '' )  );
#121466 = ORIENTED_EDGE ( 'NONE', *, *, #126196, .F. ) ;
#121465 = CARTESIAN_POINT ( 'NONE',  ( -5.433785704026946384, 9.561443431331920095, 0.000000000000000000 ) ) ;
#121467 = CARTESIAN_POINT ( 'NONE',  ( 5.010605496441194795, 7.906410611435644498, -1.080668833775387139 ) ) ;
#121468 = CARTESIAN_POINT ( 'NONE',  ( 4.077499844852236599, 1.427718728413525318, -1.423743541103118737 ) ) ;
#121469 = CARTESIAN_POINT ( 'NONE',  ( 3.468544592087896561, 0.04396668885017079864, -1.840778273432375212 ) ) ;
#121470 = CARTESIAN_POINT ( 'NONE',  ( 2.493461049780987260, 3.507114751586604129, -11.73081193161139169 ) ) ;
#121471 = CARTESIAN_POINT ( 'NONE',  ( 1.911159365042811809, 1.708073263224022975, -1.551933148444275989 ) ) ;
#121472 = CARTESIAN_POINT ( 'NONE',  ( 3.953084306836263995, 6.769626237021087789, 1.199719254218452047 ) ) ;
#121473 = CARTESIAN_POINT ( 'NONE',  ( 4.095124908492456584, 1.828510582809875107, -1.152538879107746439 ) ) ;
#121474 = CARTESIAN_POINT ( 'NONE',  ( 7.584896871841365851, 10.93646455286856956, -1.199719254218446718 ) ) ;
#121475 = CARTESIAN_POINT ( 'NONE',  ( -5.925076824372040640, 6.871343368977510302, 1.199719254218450271 ) ) ;
#121476 = PRESENTATION_LAYER_ASSIGNMENT (  '', '', ( #45191 ) ) ;
#121477 = CARTESIAN_POINT ( 'NONE',  ( 3.128558558221442354, 0.3401759809690939051, -2.272988164180503201 ) ) ;
#121478 = CARTESIAN_POINT ( 'NONE',  ( 4.702146809683721784, 5.356480858934594025, 2.420000000000010587 ) ) ;
#121479 = CARTESIAN_POINT ( 'NONE',  ( 2.272138710904994863, -1.152746988206950096, 1.473173409640892162 ) ) ;
#121480 = CARTESIAN_POINT ( 'NONE',  ( 6.438353018038387887, 1.949953777973761015, 0.2897296601065552091 ) ) ;
#121482 = CARTESIAN_POINT ( 'NONE',  ( -5.589704470584107909, 9.743348658981940247, -0.7998128361456362523 ) ) ;
#121481 = CARTESIAN_POINT ( 'NONE',  ( 1.364683531249990311, 4.863541667008084879, 0.7879004041258500513 ) ) ;
#121483 = CARTESIAN_POINT ( 'NONE',  ( 1.664966938652842954, -1.558911317520403239, 1.562347339584921002 ) ) ;
#121484 = ORIENTED_EDGE ( 'NONE', *, *, #68124, .F. ) ;
#121485 = CARTESIAN_POINT ( 'NONE',  ( -1.451998047843646500, 7.315968950353777700, -4.301760722578332086 ) ) ;
#121486 = CARTESIAN_POINT ( 'NONE',  ( 3.680148631105580215, 6.380924938676771241, -1.199719254218446718 ) ) ;
#121487 = CARTESIAN_POINT ( 'NONE',  ( -5.935772324684618795, 5.819489221753827657, 0.000000000000000000 ) ) ;
#121488 = CARTESIAN_POINT ( 'NONE',  ( 11.94980361058169116, 13.39999999999999858, 1.099999999999994982 ) ) ;
#121489 = CARTESIAN_POINT ( 'NONE',  ( 5.911001178172424986, 1.738356976118849984, 0.9299647631116741975 ) ) ;
#121490 = CARTESIAN_POINT ( 'NONE',  ( 5.901056178406707708, 1.890114102979102650, -1.323741089068092958 ) ) ;
#121491 = CARTESIAN_POINT ( 'NONE',  ( 6.777813018113469923, -1.804774468322063452, 0.4538611949938906043 ) ) ;
#121492 = CARTESIAN_POINT ( 'NONE',  ( 4.715719689075464238, 0.4568931354213046636, -2.011171341922016076 ) ) ;
#121493 = CARTESIAN_POINT ( 'NONE',  ( 5.612712406377503349, 8.531619659873665995, -1.082531754730543083 ) ) ;
#121494 = CARTESIAN_POINT ( 'NONE',  ( 5.096939404094710468, 4.911127157724081371, 0.000000000000000000 ) ) ;
#121495 = CARTESIAN_POINT ( 'NONE',  ( 7.171900071504736296, 9.390302721554109056, -1.443375672974058777 ) ) ;
#121496 = CARTESIAN_POINT ( 'NONE',  ( -1.201851678989727383E-14, 3.509375000341421469, -1.575800808251660134 ) ) ;
#121497 = CARTESIAN_POINT ( 'NONE',  ( -9.604686356149274573, 3.530925729795075796, -7.193747284969078670 ) ) ;
#121498 = CARTESIAN_POINT ( 'NONE',  ( 3.823036128929238942, 7.404033217152015567, 1.040834085586084257E-14 ) ) ;
#121499 = CARTESIAN_POINT ( 'NONE',  ( 6.584450689261575285, 1.255587272919860942, -1.771131291935989616 ) ) ;
#121501 = CARTESIAN_POINT ( 'NONE',  ( 4.933073973922719624, -1.305863698873997780, -1.298312775753200699 ) ) ;
#121500 = CARTESIAN_POINT ( 'NONE',  ( -1.734723475976807094E-15, 2.999999999999988898, -6.938893903907228378E-15 ) ) ;
#121502 = CARTESIAN_POINT ( 'NONE',  ( 11.88172094500853859, 12.22000005601592321, 1.685553348215818925 ) ) ;
#121503 = DIRECTION ( 'NONE',  ( -0.000000000000000000, -1.000000000000000000, -0.000000000000000000 ) ) ;
#121504 = CARTESIAN_POINT ( 'NONE',  ( 0.7724589312842686795, -1.759198622581410021, -0.6360808729843556719 ) ) ;
#121506 = ADVANCED_FACE ( 'NONE', ( #51534 ), #118824, .T. ) ;
#121505 = CARTESIAN_POINT ( 'NONE',  ( -4.127447729399665199, 7.650344214561823009, 0.8192481249636590634 ) ) ;
#121507 = CARTESIAN_POINT ( 'NONE',  ( 1.333315192109691072, 8.250054423670810877, -10.85938449304426356 ) ) ;
#121508 = CARTESIAN_POINT ( 'NONE',  ( 6.604949037901548969, 6.766875157141204689, 0.08182522243922914218 ) ) ;
#121509 = CARTESIAN_POINT ( 'NONE',  ( 0.3110002902955294468, 1.589785527739733695, -1.062417771062994287 ) ) ;
#121510 = CARTESIAN_POINT ( 'NONE',  ( 1.727073733189425031, -1.667858853059518420, 0.5925122568580538651 ) ) ;
#121511 = AXIS2_PLACEMENT_3D ( 'NONE', #211137, #195982, #47614 ) ;
#121512 = CARTESIAN_POINT ( 'NONE',  ( 6.305343602688459725, 1.750316497599126331, -0.9943532346578187742 ) ) ;
#121514 = CARTESIAN_POINT ( 'NONE',  ( 4.921452907191903314, -1.357786409588169096, -1.351554235494869749 ) ) ;
#121513 = CARTESIAN_POINT ( 'NONE',  ( -8.696665468161981494, 12.23352791524263239, -1.199719254218446718 ) ) ;
#121515 = AXIS2_PLACEMENT_3D ( 'NONE', #20435, #17226, #166708 ) ;
#121516 = DIRECTION ( 'NONE',  ( 0.000000000000000000, 1.000000000000000000, 0.000000000000000000 ) ) ;
#121517 = CARTESIAN_POINT ( 'NONE',  ( 5.424252406547988237, 0.9690106866696795995, 1.714583495817107783 ) ) ;
#121519 = EDGE_CURVE ( 'NONE', #130695, #95488, #40106, .T. ) ;
#121518 = CARTESIAN_POINT ( 'NONE',  ( -0.1577409392781377873, -1.310076727147227560, -1.668215054097483385 ) ) ;
#121520 = CARTESIAN_POINT ( 'NONE',  ( -2.128168088883454642E-12, -3.089410100848593466, 3.428390338093493028 ) ) ;
#121521 = CARTESIAN_POINT ( 'NONE',  ( 3.362029495745801899, 0.8400119854848131506, 1.671504782411597612 ) ) ;
#121523 = EDGE_LOOP ( 'NONE', ( #18254, #38632, #161534, #168711 ) ) ;
#121522 = CARTESIAN_POINT ( 'NONE',  ( 6.533849689656099358, -1.133137674240388248, -1.300586445545851344 ) ) ;
#121525 = CARTESIAN_POINT ( 'NONE',  ( 2.223174002961016082, 5.537527403522402025, -0.7216878364870267237 ) ) ;
#121524 = CARTESIAN_POINT ( 'NONE',  ( 2.332911791115964473, 2.140974936812658935, 0.5348262304398290201 ) ) ;
#121526 = CARTESIAN_POINT ( 'NONE',  ( 0.6823417656249899377, 3.988541667008085767, -1.181850606188754593 ) ) ;
#121527 = CARTESIAN_POINT ( 'NONE',  ( 0.5376419320063254847, 1.925266156408891316, -0.7407299734314594097 ) ) ;
#121529 = ADVANCED_FACE ( 'NONE', ( #154361 ), #156104, .F. ) ;
#121528 = CARTESIAN_POINT ( 'NONE',  ( 6.317209508963599340, 9.457495962844502557, 1.199719254218462483 ) ) ;
#121530 = CARTESIAN_POINT ( 'NONE',  ( -10.10098813738111545, 11.74323990082152491, -1.199719254218441611 ) ) ;
#121531 = CARTESIAN_POINT ( 'NONE',  ( -15.75000000000000000, 12.29999999999998295, 1.799999999999999600 ) ) ;
#121532 = CARTESIAN_POINT ( 'NONE',  ( -5.278201874421822204, 5.052323696447222900, 0.7998128361456341429 ) ) ;
#121533 = CARTESIAN_POINT ( 'NONE',  ( -7.586009164902065116, -6.657020681837092724, -7.796438949605414948 ) ) ;
#121534 = ORIENTED_EDGE ( 'NONE', *, *, #72903, .F. ) ;
#121535 = CARTESIAN_POINT ( 'NONE',  ( 3.227070907399377298, -1.911900318415656441, -0.7948586591664741352 ) ) ;
#121536 = CARTESIAN_POINT ( 'NONE',  ( -0.7500000000000215383, 4.691666666666684193, 1.299038105676671107 ) ) ;
#121537 = CARTESIAN_POINT ( 'NONE',  ( 5.443762371086860341, 6.309809840144842141, 1.199719254218462483 ) ) ;
#121538 = CARTESIAN_POINT ( 'NONE',  ( -6.612840081267999714, 6.759580388257274919, -0.1161152146933758927 ) ) ;
#121539 = CARTESIAN_POINT ( 'NONE',  ( 0.4166731193052671256, -0.6827031231213858131, -1.900913249881502232 ) ) ;
#121540 = CARTESIAN_POINT ( 'NONE',  ( -1.201851678989727383E-14, 4.071875000341425022, 1.575800808251672791 ) ) ;
#121541 = ORIENTED_EDGE ( 'NONE', *, *, #62145, .T. ) ;
#121543 = CARTESIAN_POINT ( 'NONE',  ( 9.002250809793993724, 11.52571191622492464, -1.443375672974057666 ) ) ;
#121542 = CARTESIAN_POINT ( 'NONE',  ( 0.07459516483345349225, 1.413926688351078154, -2.016100038618890089 ) ) ;
#121544 = CARTESIAN_POINT ( 'NONE',  ( 5.923203835008548523, 0.8145033986626595279, 1.844426808122232142 ) ) ;
#121545 = CARTESIAN_POINT ( 'NONE',  ( 5.489432593909100433, -0.4588279098093718256, 1.859853701273159743 ) ) ;
#121546 = CARTESIAN_POINT ( 'NONE',  ( 6.639320575229251453, 2.441375407831634536, 2.385816205380648203 ) ) ;
#121547 = CARTESIAN_POINT ( 'NONE',  ( 3.527062600443749307, -2.024233912922444478, 0.8403589366152917073 ) ) ;
#121548 = CARTESIAN_POINT ( 'NONE',  ( -1.201851678989727383E-14, 1.993750000682816381, 1.732050807568877637 ) ) ;
#121549 = CARTESIAN_POINT ( 'NONE',  ( 2.338023529656753752, -1.104205016203146705, -1.561194055274425452 ) ) ;
#121550 = CARTESIAN_POINT ( 'NONE',  ( -5.259673527097670664, 8.223703984000886535, -1.199719254218446718 ) ) ;
#121551 = CARTESIAN_POINT ( 'NONE',  ( 4.270455198180219902, 6.965652916976816655, -1.082531754730548412 ) ) ;
#121552 = CARTESIAN_POINT ( 'NONE',  ( 0.7730648107450198703, 1.777001872080404166, -0.9530316558409923644 ) ) ;
#121553 = CARTESIAN_POINT ( 'NONE',  ( -0.6823417656250039265, 10.88020833367472839, -1.181850606188755259 ) ) ;
#121555 = CARTESIAN_POINT ( 'NONE',  ( -7.279802135894939852, 7.457800344824362604, -0.7998128361456362523 ) ) ;
#121554 = CARTESIAN_POINT ( 'NONE',  ( 6.110890996357365879, -0.2699588104537915534, 2.174781792473476472 ) ) ;
#121557 = VERTEX_POINT ( 'NONE', #41340 ) ;
#121556 = CARTESIAN_POINT ( 'NONE',  ( 3.522183196695947593, 1.094745356718468399, -1.332776395737497399 ) ) ;
#121558 = CARTESIAN_POINT ( 'NONE',  ( 0.1399997263886003374, 0.002789056014650820314, -1.999853399661279063 ) ) ;
#121559 = CARTESIAN_POINT ( 'NONE',  ( 7.416473721875251890, 8.611306416064660851, 1.199719254218462483 ) ) ;
#121560 = CARTESIAN_POINT ( 'NONE',  ( 3.486418057008484617, 7.219238166485217434, 1.040834085586084257E-14 ) ) ;
#121561 = DIRECTION ( 'NONE',  ( 1.000000000000000000, -7.387867266669436732E-31, 0.000000000000000000 ) ) ;
#121562 = CARTESIAN_POINT ( 'NONE',  ( -3.474999999999997868, -2.377083332377420088, 2.006292185433951047 ) ) ;
#121563 = DIRECTION ( 'NONE',  ( -5.551115123125765446E-17, 0.000000000000000000, 1.000000000000000000 ) ) ;
#121564 = CARTESIAN_POINT ( 'NONE',  ( 5.168682875307768931, 7.053215992657626110, -1.599625672291256295 ) ) ;
#121565 = CARTESIAN_POINT ( 'NONE',  ( 3.469446951953614189E-15, 8.900000000000019895, 1.214306433183764966E-14 ) ) ;
#121566 = ORIENTED_EDGE ( 'NONE', *, *, #121295, .F. ) ;
#121567 = DIRECTION ( 'NONE',  ( -0.7592566023652995710, -0.6507913734559650498, 0.000000000000000000 ) ) ;
#121568 = ORIENTED_EDGE ( 'NONE', *, *, #126729, .F. ) ;
#121569 = CARTESIAN_POINT ( 'NONE',  ( 4.090334381980924583, -1.039670344891037601, 1.483205724144847748 ) ) ;
#121570 = VERTEX_POINT ( 'NONE', #8807 ) ;
#121571 = CARTESIAN_POINT ( 'NONE',  ( 9.901532256681887745, 10.44620914241737530, 0.000000000000000000 ) ) ;
#121572 = CARTESIAN_POINT ( 'NONE',  ( 3.237364818613055473, 6.998952398349030268, -1.734723475976807094E-15 ) ) ;
#121573 = CARTESIAN_POINT ( 'NONE',  ( 4.688045340743730804, 1.047092163662701525, 1.477968688824328858 ) ) ;
#121574 = CARTESIAN_POINT ( 'NONE',  ( 6.658462837642791676, 8.861568958707010779, 1.443375672974063439 ) ) ;
#121575 = CARTESIAN_POINT ( 'NONE',  ( 3.469446951953614189E-15, 5.290451655907108197, 1.214306433183764966E-14 ) ) ;
#121576 = CARTESIAN_POINT ( 'NONE',  ( 5.490683550995299811, 6.230756917952954055, 0.9772120879164881702 ) ) ;
#121578 = CARTESIAN_POINT ( 'NONE',  ( -0.6823417656250003738, 14.15104166700806232, 1.181850606188754593 ) ) ;
#121577 = CARTESIAN_POINT ( 'NONE',  ( 5.283604245000163679, -1.767202373759840572, 0.5838029059755837080 ) ) ;
#121579 = CARTESIAN_POINT ( 'NONE',  ( 2.882342042720618558, -0.5589011775578194285, -1.832234547041192929 ) ) ;
#121580 = FILL_AREA_STYLE ('',( #8803 ) ) ;
#121581 = CARTESIAN_POINT ( 'NONE',  ( -11.82816107619417778, 7.167718870070345361, 1.885585305228718589 ) ) ;
#121582 = TOROIDAL_SURFACE ( 'NONE', #97386, 11.92000000000000171, 0.08000000000000000167 ) ;
#121583 = CARTESIAN_POINT ( 'NONE',  ( 9.499606442108964544, -9.900000000000005684, -0.08647222121513538362 ) ) ;
#121584 = CARTESIAN_POINT ( 'NONE',  ( 6.968527767744098433, 9.153035033833367251, 1.443375672974076540 ) ) ;
#121585 = CARTESIAN_POINT ( 'NONE',  ( -2.740719608256871442, 6.349256642941639051, 0.7998128361456341429 ) ) ;
#121586 = FILL_AREA_STYLE ('',( #123733 ) ) ;
#121587 = CARTESIAN_POINT ( 'NONE',  ( 1.763735852432495754, 1.075751846022491964, 1.792481376920366687 ) ) ;
#121588 = CARTESIAN_POINT ( 'NONE',  ( 6.690022453700429139, 6.769724048930809701, 0.7998128361456331437 ) ) ;
#121589 = CARTESIAN_POINT ( 'NONE',  ( 6.739296538182359519, -1.720230304288400625, 0.8672215684524892110 ) ) ;
#121590 = CARTESIAN_POINT ( 'NONE',  ( -5.148345644887285744, 7.029489223833707001, -1.599625672291256295 ) ) ;
#121591 = CARTESIAN_POINT ( 'NONE',  ( 2.643341535394112540, -1.351257319430071435, -1.227710988083303256 ) ) ;
#121592 = EDGE_CURVE ( 'NONE', #39437, #210054, #172951, .T. ) ;
#121593 = CARTESIAN_POINT ( 'NONE',  ( 10.68054077891637377, -8.644755361503010604, -0.1864295327644151512 ) ) ;
#121594 = CARTESIAN_POINT ( 'NONE',  ( 1.486696478045932635, 1.897211281248304848, 0.5285659569534242319 ) ) ;
#121595 = CARTESIAN_POINT ( 'NONE',  ( 3.825673241664818036, 1.036335792742661299, -1.642260645495984495 ) ) ;
#121596 = ORIENTED_EDGE ( 'NONE', *, *, #148262, .T. ) ;
#121597 = CARTESIAN_POINT ( 'NONE',  ( -4.038971567461725698, 3.986455684509185193, -0.5169845646830102392 ) ) ;
#121599 = CARTESIAN_POINT ( 'NONE',  ( 6.578945215809504532, 1.736110340762307969, 0.6705269824554618285 ) ) ;
#121598 = CARTESIAN_POINT ( 'NONE',  ( -5.978219388983010418, 5.939287140093762574, -0.7998128361456362523 ) ) ;
#121601 = CARTESIAN_POINT ( 'NONE',  ( 3.779626292077961747, 0.2561244552635975058, -2.104982076983111572 ) ) ;
#121600 = CARTESIAN_POINT ( 'NONE',  ( 2.911969131885072670, 6.619324097166378706, 0.000000000000000000 ) ) ;
#121602 = CARTESIAN_POINT ( 'NONE',  ( 6.634380621478824125, -6.684699875907186062, 6.783773251375872171 ) ) ;
#121603 = CARTESIAN_POINT ( 'NONE',  ( 9.921869487102386032, 10.46993591124128997, 0.000000000000000000 ) ) ;
#121604 = CARTESIAN_POINT ( 'NONE',  ( -7.096767062110449942, 7.244259425409119046, -0.7998128361456362523 ) ) ;
#121605 = FILL_AREA_STYLE_COLOUR ( '', #180878 ) ;
#121606 = VERTEX_POINT ( 'NONE', #89016 ) ;
#121607 = CIRCLE ( 'NONE', #149185, 0.07999999999999998779 ) ;
#121608 = CARTESIAN_POINT ( 'NONE',  ( 7.062871678076271920, 7.204714810702593120, -0.7998128361456341429 ) ) ;
#121609 = CARTESIAN_POINT ( 'NONE',  ( 11.86145016429273191, 12.69999999999999929, -1.100000000000000533 ) ) ;
#121612 = ADVANCED_FACE ( 'NONE', ( #209120 ), #83959, .T. ) ;
#121611 = CARTESIAN_POINT ( 'NONE',  ( 5.911342272548038679, -1.897112096406332382, 0.6839327336411115121 ) ) ;
#121610 = CARTESIAN_POINT ( 'NONE',  ( 3.369579884941567016, 1.780956498284639533, -0.4009276245297774266 ) ) ;
#121613 = CARTESIAN_POINT ( 'NONE',  ( -0.4019237886466871523, 12.97991455036742892, -1.499999999999998668 ) ) ;
#121614 = CARTESIAN_POINT ( 'NONE',  ( -9.653042183249970876, 11.32459930428888306, -1.082531754730539753 ) ) ;
#121615 = CARTESIAN_POINT ( 'NONE',  ( -5.370252646843524325, 7.685795487962019834, 1.333085116894404232 ) ) ;
#121616 = CARTESIAN_POINT ( 'NONE',  ( -0.4000000000000201172, 4.000000000000003553, -0.9782388782689169782 ) ) ;
#121617 = CARTESIAN_POINT ( 'NONE',  ( 4.399188623838041323, 1.502396186649012311, 1.114296746780506497 ) ) ;
#121618 = CARTESIAN_POINT ( 'NONE',  ( 9.399880572976245574, 9.860948844760784482, 0.7998128361456462443 ) ) ;
#121619 = CARTESIAN_POINT ( 'NONE',  ( 1.805176890173798565, 1.601487618425012638, 1.070529213009919101 ) ) ;
#121620 = CARTESIAN_POINT ( 'NONE',  ( -0.7158994178059416846, 2.800000000000024691, 1.161830092591057184 ) ) ;
#121621 = PRESENTATION_LAYER_ASSIGNMENT (  '', '', ( #52270 ) ) ;
#121622 = CARTESIAN_POINT ( 'NONE',  ( 1.364683531250000303, 8.567708333674730170, -0.7879004041258355073 ) ) ;
#121623 = CARTESIAN_POINT ( 'NONE',  ( -6.470265622219711688, 8.571729197388226140, -1.599625672291263179 ) ) ;
#121624 = CARTESIAN_POINT ( 'NONE',  ( 3.822509244049070887, 6.547012320444182798, -1.199719254218452047 ) ) ;
#121625 = CARTESIAN_POINT ( 'NONE',  ( -3.946832114909637479, 7.618738210787614484, 0.7216878364870338292 ) ) ;
#121626 = CARTESIAN_POINT ( 'NONE',  ( 1.300578652796330115, 1.418844934001600944, -1.571659118156268908 ) ) ;
#121627 = CARTESIAN_POINT ( 'NONE',  ( 8.703444544968814256, 12.24143683818393313, -1.199719254218446718 ) ) ;
#121628 = CARTESIAN_POINT ( 'NONE',  ( -2.318081078256692518, 5.648252324700675508, 1.040834085586084257E-14 ) ) ;
#121629 = CARTESIAN_POINT ( 'NONE',  ( 4.838769763947080804, -2.006773940031422399, -0.5081810985937407210 ) ) ;
#121631 = CARTESIAN_POINT ( 'NONE',  ( 0.6823417656249899377, 3.155208333674754062, 1.181850606188765695 ) ) ;
#121630 = CARTESIAN_POINT ( 'NONE',  ( 0.6789530235665336422, 1.236279375446739603, 1.364625092910062953 ) ) ;
#121632 = CARTESIAN_POINT ( 'NONE',  ( 5.660817213934862480, 1.366460917787317930, 1.848312285176759717 ) ) ;
#121633 = CARTESIAN_POINT ( 'NONE',  ( 5.341549334104176872, 9.175631956522799726, 0.7216878364870438212 ) ) ;
#121635 = DIRECTION ( 'NONE',  ( 0.000000000000000000, -1.000000000000000000, 0.000000000000000000 ) ) ;
#121634 = CARTESIAN_POINT ( 'NONE',  ( 3.282482588284323821, 6.843663763058119187, 0.7216878364870257245 ) ) ;
#121636 = CARTESIAN_POINT ( 'NONE',  ( 1.570720025219290328, -2.177795595024238473, -0.7155201368211090429 ) ) ;
#121638 = EDGE_CURVE ( 'NONE', #206352, #163559, #161058, .T. ) ;
#121637 = CARTESIAN_POINT ( 'NONE',  ( 5.024051501469349645, 4.898199347683565463, -0.07077548676925468629 ) ) ;
#121639 = CARTESIAN_POINT ( 'NONE',  ( -6.454563648557663846, 9.688018802362710957, -1.199719254218452047 ) ) ;
#121640 = CARTESIAN_POINT ( 'NONE',  ( 4.822180446859828606, 1.858854579410177843, 0.5619951038204271665 ) ) ;
#121641 = ORIENTED_EDGE ( 'NONE', *, *, #22519, .T. ) ;
#121642 = CARTESIAN_POINT ( 'NONE',  ( 7.361714222096048310, 10.57212177821199184, -1.082531754730537976 ) ) ;
#121643 = EDGE_CURVE ( 'NONE', #80483, #22839, #192367, .T. ) ;
#121644 = ORIENTED_EDGE ( 'NONE', *, *, #105829, .T. ) ;
#121645 = CARTESIAN_POINT ( 'NONE',  ( 5.853752780977106163, -1.389761788226477002, -1.313969904969368496 ) ) ;
#121646 = CARTESIAN_POINT ( 'NONE',  ( 5.489470343000498076, -0.4852711138302409077, 1.957169415941109269 ) ) ;
#121648 = DIRECTION ( 'NONE',  ( -0.000000000000000000, -1.000000000000000000, -0.000000000000000000 ) ) ;
#121647 = CARTESIAN_POINT ( 'NONE',  ( -9.501566725078754772, 9.979582688880366703, -0.7998128361456291469 ) ) ;
#121649 = CARTESIAN_POINT ( 'NONE',  ( 3.285556943750000070, -1.421874999522041660, 0.000000000000000000 ) ) ;
#121651 = CARTESIAN_POINT ( 'NONE',  ( 1.762210296550786204, -1.254468555733399660, 1.248734745320427830 ) ) ;
#121650 = CARTESIAN_POINT ( 'NONE',  ( 2.959016038526005143, 0.3060221511422682727, -2.067984839732572855 ) ) ;
#121652 = DIRECTION ( 'NONE',  ( 1.000000000000000000, -7.771561172376097755E-16, -4.440892098500627148E-16 ) ) ;
#121654 = CARTESIAN_POINT ( 'NONE',  ( 4.716876218882520178, -0.1156266834452194386, 2.289457304130739779 ) ) ;
#121653 = CARTESIAN_POINT ( 'NONE',  ( 3.736153849017632922, 6.516540702899320081, -1.199719254218453823 ) ) ;
#121655 = CARTESIAN_POINT ( 'NONE',  ( 2.167524683544871600, -1.071679988950867024, 1.371128027196461208 ) ) ;
#121656 = CARTESIAN_POINT ( 'NONE',  ( 4.487912541323413329, 5.194651705420806564, 1.199719254218462483 ) ) ;
#121657 = DIRECTION ( 'NONE',  ( 0.8660254037844385966, 0.000000000000000000, 0.5000000000000001110 ) ) ;
#121658 = CARTESIAN_POINT ( 'NONE',  ( 2.723678392350858957, -1.506833864184083493, -0.8575499777047421723 ) ) ;
#121659 = CARTESIAN_POINT ( 'NONE',  ( -2.754243431018125239E-14, 1.984375000341467299, 1.570758158831788265 ) ) ;
#121660 = CARTESIAN_POINT ( 'NONE',  ( 2.067058339702015246, 1.609816819982702985, -1.457078277656477905 ) ) ;
#121661 = CARTESIAN_POINT ( 'NONE',  ( 4.123651276850781144, 7.962676922967908411, -0.7998128361456221525 ) ) ;
#121662 = CARTESIAN_POINT ( 'NONE',  ( 4.048064755690682581, 0.9548552675892291175, 1.776167154503265566 ) ) ;
#121663 = CARTESIAN_POINT ( 'NONE',  ( 2.343750000000001332, 1.895863743164134307, 0.7852924748298687474 ) ) ;
#121664 = VECTOR ( 'NONE', #185687, 1000.000000000000000 ) ;
#121665 = CARTESIAN_POINT ( 'NONE',  ( -1.500000000000011324, 3.202083334016150307, 0.8660254037844403729 ) ) ;
#121666 = CARTESIAN_POINT ( 'NONE',  ( 1.166875649673270399, -1.740261045891202230, -0.8264182621567657261 ) ) ;
#121667 = CARTESIAN_POINT ( 'NONE',  ( 1.364683531249996529, 13.96354166700806765, 0.7879004041258405033 ) ) ;
#121668 = CARTESIAN_POINT ( 'NONE',  ( 4.113701061080524468, 1.785520537663972451, 1.321432767922005924 ) ) ;
#121669 = EDGE_LOOP ( 'NONE', ( #103200, #78588, #119848 ) ) ;
#121671 = AXIS2_PLACEMENT_3D ( 'NONE', #185413, #2376, #134583 ) ;
#121670 = CARTESIAN_POINT ( 'NONE',  ( -0.2106854629475270468, 2.024676876401194203, -2.413177685601196831 ) ) ;
#121672 = CARTESIAN_POINT ( 'NONE',  ( 0.7499999999999885647, 0.9833333333333569293, 1.299038105676657340 ) ) ;
#121673 = CARTESIAN_POINT ( 'NONE',  ( 6.588372581236919601, 9.773852880496709972, -1.199719254218440723 ) ) ;
#121674 = CARTESIAN_POINT ( 'NONE',  ( 4.758548728272192108, 7.535095368750792666, -1.082531754730549078 ) ) ;
#121675 = CARTESIAN_POINT ( 'NONE',  ( -3.285556943749998737, -1.130208332855376918, 1.896917185911908721 ) ) ;
#121676 = CARTESIAN_POINT ( 'NONE',  ( 0.3818600843802121836, 0.2116341679995105141, -2.211193375792892546 ) ) ;
#121677 = CARTESIAN_POINT ( 'NONE',  ( 6.039501783790233169, 1.813256598412491982, -0.7494862575098263369 ) ) ;
#121678 = CARTESIAN_POINT ( 'NONE',  ( 8.405692050792682224, 12.75046512599275772, -0.7216878364870328300 ) ) ;
#121679 = CARTESIAN_POINT ( 'NONE',  ( 0.000000000000000000, 0.06698729810653621108, 10.99999999999751665 ) ) ;
#121680 = CARTESIAN_POINT ( 'NONE',  ( 0.5620833348847533717, 2.138143771118843350, -0.3165822943479515983 ) ) ;
#121681 = CARTESIAN_POINT ( 'NONE',  ( -4.312902262922974295, 8.045820050136510915, 0.7216878364870338292 ) ) ;
#121682 = CARTESIAN_POINT ( 'NONE',  ( 3.068856176772206457, 1.495872946324308783, -1.420456422295824916 ) ) ;
#121683 = CARTESIAN_POINT ( 'NONE',  ( -4.882907879216086933, 8.848476292394087395, -0.7998128361456281477 ) ) ;
#121684 = CARTESIAN_POINT ( 'NONE',  ( 1.499999999999989120, 2.806250000682818158, 1.214306433183764966E-14 ) ) ;
#121685 = CARTESIAN_POINT ( 'NONE',  ( -1.001543065824772872E-14, 5.634375000341415252, 1.575800808251672791 ) ) ;
#121686 = CARTESIAN_POINT ( 'NONE',  ( 4.815616550699190590, -1.834762568278673900, 0.3632225495420540184 ) ) ;
#121687 = CARTESIAN_POINT ( 'NONE',  ( 4.166485388134741008, 1.137239580169274067, 1.309253364134143505 ) ) ;
#121688 = CARTESIAN_POINT ( 'NONE',  ( 2.964111632446063016, -1.609175542312387908, -0.6635834015607346981 ) ) ;
#121689 = CARTESIAN_POINT ( 'NONE',  ( 0.3633196395196974793, 0.2168307188613327052, -2.282096724506751162 ) ) ;
#121690 = CARTESIAN_POINT ( 'NONE',  ( -1.364683531250010295, 3.842708333674751398, 0.7879004041258379498 ) ) ;
#121691 = CARTESIAN_POINT ( 'NONE',  ( 4.792568760853118448, 1.737405308921141645, -1.162709912544395152 ) ) ;
#121692 = CARTESIAN_POINT ( 'NONE',  ( 6.421825219014824171, 1.115965409679237963, -1.589096094497045142 ) ) ;
#121694 = VERTEX_POINT ( 'NONE', #163605 ) ;
#121693 = CARTESIAN_POINT ( 'NONE',  ( -0.06263693352612853538, -7.008128100062068988, 9.499802063084667125 ) ) ;
#121695 = SURFACE_STYLE_FILL_AREA ( #173593 ) ;
#121696 = CARTESIAN_POINT ( 'NONE',  ( 0.4752326960846975923, -2.001511663014220677, -0.2440270837566413387 ) ) ;
#121697 = CARTESIAN_POINT ( 'NONE',  ( 0.7211286721200690364, 1.601891702520108485, -1.389630591760198541 ) ) ;
#121698 = CARTESIAN_POINT ( 'NONE',  ( -5.126981680758313876E-15, -9.091017468556977121, 10.23550087314637302 ) ) ;
#121699 = CARTESIAN_POINT ( 'NONE',  ( 6.346327303948391396, 0.3419391630616851474, -1.987045965717588958 ) ) ;
#121700 = CARTESIAN_POINT ( 'NONE',  ( -8.097244055859620815, 10.46987070330147063, -1.599625672291263179 ) ) ;
#121701 = CARTESIAN_POINT ( 'NONE',  ( 4.632082037363250748, 8.555846143565791095, -0.7998128361456231517 ) ) ;
#121702 = CARTESIAN_POINT ( 'NONE',  ( 2.491022521637117570, -2.029929026191950925, -0.6131127883793399125 ) ) ;
#121703 = DIRECTION ( 'NONE',  ( -0.000000000000000000, 1.000000000000000000, -0.000000000000000000 ) ) ;
#121704 = CARTESIAN_POINT ( 'NONE',  ( 4.213378774425760476, -0.3099129147984269195, 1.799030153321119263 ) ) ;
#121705 = ADVANCED_FACE ( 'NONE', ( #66051 ), #145256, .T. ) ;
#121706 = ORIENTED_EDGE ( 'NONE', *, *, #48666, .F. ) ;
#121707 = CARTESIAN_POINT ( 'NONE',  ( -6.474900878978163021, 9.711745571186627402, -1.199719254218452047 ) ) ;
#121708 = CARTESIAN_POINT ( 'NONE',  ( 0.03919461954074245080, -7.818966704647666965, -9.500338091956020747 ) ) ;
#121709 = CARTESIAN_POINT ( 'NONE',  ( -1.642778471874998480, -0.4885416661887104217, 2.845375778867863303 ) ) ;
#121711 = CARTESIAN_POINT ( 'NONE',  ( -5.859094939400033120, 9.987361195942037639, -0.7998128361456231517 ) ) ;
#121710 = B_SPLINE_CURVE_WITH_KNOTS ( 'NONE', 3,
 ( #173863, #105664, #11319, #140304, #108905, #126237 ),
 .UNSPECIFIED., .F., .F.,
 ( 4, 2, 4 ),
 ( 0.000000000000000000, 0.002406312826513442183, 0.004812625653026884366 ),
 .UNSPECIFIED. ) ;
#121712 = CARTESIAN_POINT ( 'NONE',  ( 2.021745798758204149, -0.4384165714973499162, 1.971471537551409803 ) ) ;
#121713 = CARTESIAN_POINT ( 'NONE',  ( 5.842855468016632692, 0.4250294216477692455, 2.165293060021292515 ) ) ;
#121714 = CARTESIAN_POINT ( 'NONE',  ( -4.285259070371116863, 7.157163461145040095, 1.199719254218452935 ) ) ;
#121715 = CARTESIAN_POINT ( 'NONE',  ( 3.080726782406420838, 1.750568488035513681, 0.6316850995219197573 ) ) ;
#121716 = CARTESIAN_POINT ( 'NONE',  ( 4.376584659113025744, 4.000436945253625254, 0.7998128361456341429 ) ) ;
#121717 = CYLINDRICAL_SURFACE ( 'NONE', #50498, 0.09999999999999982514 ) ;
#121718 = CARTESIAN_POINT ( 'NONE',  ( -4.120788623549732854, 6.895004929861607401, -1.199719254218452047 ) ) ;
#121719 = CARTESIAN_POINT ( 'NONE',  ( -9.996439331977562404, 10.55693406359564790, 0.7998128361456462443 ) ) ;
#121720 = CARTESIAN_POINT ( 'NONE',  ( 5.479063914364931343, -0.04889757770590653918, -1.825204647902956889 ) ) ;
#121722 = CARTESIAN_POINT ( 'NONE',  ( -4.201979666139121328, 7.560802217138083314, -0.9697280773930611053 ) ) ;
#121721 = CARTESIAN_POINT ( 'NONE',  ( -5.490125858891038213, 5.369844688319787451, -0.7998128361456362523 ) ) ;
#121723 = CARTESIAN_POINT ( 'NONE',  ( -0.6823417656250003738, -0.2822916663252489355, -1.181850606188749264 ) ) ;
#121724 = CARTESIAN_POINT ( 'NONE',  ( 6.884150277402729223, -0.1485532345978715640, 1.983297619905934006 ) ) ;
#121725 = CARTESIAN_POINT ( 'NONE',  ( 0.02286245922865359423, -1.065969982613410583, -1.375977130364250955 ) ) ;
#121726 = CARTESIAN_POINT ( 'NONE',  ( 5.707753894846095299, -0.5660891107236701858, 2.237086922978877457 ) ) ;
#121727 = CARTESIAN_POINT ( 'NONE',  ( 3.528865121306874464, 7.339036084825155015, -0.7998128361456362523 ) ) ;
#121728 = CARTESIAN_POINT ( 'NONE',  ( 0.6146155864290882009, 1.423047967033652883, -1.490775708471054006 ) ) ;
#121729 = CARTESIAN_POINT ( 'NONE',  ( 4.957477724091233995, 8.935474444748447098, -0.7998128361456281477 ) ) ;
#121730 = CARTESIAN_POINT ( 'NONE',  ( 5.202631756544580988, -1.620200680833181694, -1.630429044757361723 ) ) ;
#121731 = CARTESIAN_POINT ( 'NONE',  ( 6.471393748265543699, 5.229711127717882491, 2.500000000000011102 ) ) ;
#121732 = CARTESIAN_POINT ( 'NONE',  ( -5.250750630242457362, 9.347902511916677426, 0.000000000000000000 ) ) ;
#121733 = CONICAL_SURFACE ( 'NONE', #142394, 11.53746066217573940, 0.1181278931043537039 ) ;
#121734 = CARTESIAN_POINT ( 'NONE',  ( 5.910993886665249164, 1.650546521282238110, 0.8803886038859505270 ) ) ;
#121736 = CARTESIAN_POINT ( 'NONE',  ( -4.984557751679625781, 5.844347460828191565, 1.199719254218452935 ) ) ;
#121735 = CARTESIAN_POINT ( 'NONE',  ( 3.726736447152957599, 1.348887845406310682, -1.355897031963343213 ) ) ;
#121737 = CARTESIAN_POINT ( 'NONE',  ( 5.074942902252104204, -2.077123540546990110, -0.7459609299403434646 ) ) ;
#121738 = CARTESIAN_POINT ( 'NONE',  ( 1.224999999999979217, 1.208333334016137739, -0.7072540797573076965 ) ) ;
#121739 = CARTESIAN_POINT ( 'NONE',  ( 4.231553341240931410, 7.950912974840878888, -0.7216878364870107365 ) ) ;
#121740 = CARTESIAN_POINT ( 'NONE',  ( 4.217995187182920880, 6.974725914138481642, 1.082531754730549078 ) ) ;
#121741 = CARTESIAN_POINT ( 'NONE',  ( -6.089020385868876062, 6.276481003034692030, -0.7216878364870338292 ) ) ;
#121742 = CARTESIAN_POINT ( 'NONE',  ( 5.918629486560170960, -0.7630358368452618834, -1.978611909900826582 ) ) ;
#121743 = CARTESIAN_POINT ( 'NONE',  ( 2.345130104517737291, 0.5056967325399002178, 2.251352274652190122 ) ) ;
#121744 = CARTESIAN_POINT ( 'NONE',  ( 3.754310534785664899, -1.959519245081872585, -0.09869234604030494018 ) ) ;
#121745 = CARTESIAN_POINT ( 'NONE',  ( 0.2507196182260813533, -0.4238382354822354259, -1.922440920834954436 ) ) ;
#121746 = CARTESIAN_POINT ( 'NONE',  ( 9.100815109899395239, 14.29680943629558776, 7.752531514792824652 ) ) ;
#121747 = CARTESIAN_POINT ( 'NONE',  ( 3.607351389687783794, 6.366271167014519783, 1.199719254218451159 ) ) ;
#121748 = ORIENTED_EDGE ( 'NONE', *, *, #16332, .F. ) ;
#121749 = CARTESIAN_POINT ( 'NONE',  ( 5.630092293170263495, 2.014432788975322630, 0.09412139267171715229 ) ) ;
#121750 = CARTESIAN_POINT ( 'NONE',  ( -9.158696461231359720, 10.64389961198009615, 1.199719254218462483 ) ) ;
#121751 = CARTESIAN_POINT ( 'NONE',  ( 0.2515690823673248921, 0.7017594223384625574, 1.702352774230586618 ) ) ;
#121752 = CARTESIAN_POINT ( 'NONE',  ( -11.52114515671133610, 8.081606464056415362, 2.192706985476595261 ) ) ;
#121753 = CARTESIAN_POINT ( 'NONE',  ( 3.397511025282150321, -1.916906860828609727, 1.019255427985159779 ) ) ;
#121754 = CARTESIAN_POINT ( 'NONE',  ( 0.000000000000000000, -4.000000000000003553, 0.000000000000000000 ) ) ;
#121755 = CARTESIAN_POINT ( 'NONE',  ( 0.4926326669930108371, -1.172979896111199904, 1.766458537607276114 ) ) ;
#121756 = CARTESIAN_POINT ( 'NONE',  ( 1.499999999999987121, 1.077083334016148308, -0.8660254037844253849 ) ) ;
#121757 = CARTESIAN_POINT ( 'NONE',  ( -3.543593105830169065, 14.52998843158304254, -11.47354445632842257 ) ) ;
#121758 = DIRECTION ( 'NONE',  ( 0.7613463080411785322, -0.000000000000000000, 0.6483454320283801309 ) ) ;
#121759 = CARTESIAN_POINT ( 'NONE',  ( 5.403926048761924505, 7.658933883257522446, 1.327442161737320436 ) ) ;
#121760 = CARTESIAN_POINT ( 'NONE',  ( 0.9310180319365793933, 0.1487380178207615700, 2.055447871051790720 ) ) ;
#121761 = AXIS2_PLACEMENT_3D ( 'NONE', #135300, #204516, #172056 ) ;
#121763 = CARTESIAN_POINT ( 'NONE',  ( -1.115562610750309283E-14, 8.343750000682796042, 1.500000000000001554 ) ) ;
#121762 = CARTESIAN_POINT ( 'NONE',  ( -8.143643823302737061, 12.65266822716189843, 0.000000000000000000 ) ) ;
#121764 = CARTESIAN_POINT ( 'NONE',  ( -0.6823417656250003738, 0.2177083336747515085, -1.181850606188749264 ) ) ;
#121765 = ORIENTED_EDGE ( 'NONE', *, *, #48284, .F. ) ;
#121766 = CARTESIAN_POINT ( 'NONE',  ( 3.457576163436149486, -1.449788379102138869, -1.247086912153513749 ) ) ;
#121767 = CARTESIAN_POINT ( 'NONE',  ( 5.594547536969180612, -0.4332151766474266474, -1.715878325482506517 ) ) ;
#121768 = CARTESIAN_POINT ( 'NONE',  ( 5.905458427204159477, 9.047396044116986502, 1.199719254218452047 ) ) ;
#121769 = CARTESIAN_POINT ( 'NONE',  ( -4.660252114795309097, 6.460046772059735432, -1.599625672291256295 ) ) ;
#121770 = CARTESIAN_POINT ( 'NONE',  ( 0.3514446173804542939, -1.281351489097491303, -1.280874292944272685 ) ) ;
#121772 = CARTESIAN_POINT ( 'NONE',  ( 0.4267777427376097665, -1.641576225293687630, 0.9873106011929821957 ) ) ;
#121771 = CARTESIAN_POINT ( 'NONE',  ( -6.663994888585890841, -7.154544010626969985, 6.770610912236882939 ) ) ;
#121773 = CARTESIAN_POINT ( 'NONE',  ( 2.277862540309500083, -2.008769142935047380, 0.5008063122204224893 ) ) ;
#121774 = CARTESIAN_POINT ( 'NONE',  ( 1.364683531249988757, 0.1968750003414204697, 0.000000000000000000 ) ) ;
#121776 = EDGE_CURVE ( 'NONE', #21552, #54906, #174834, .T. ) ;
#121775 = CIRCLE ( 'NONE', #187384, 0.1399999999999995970 ) ;
#121777 = CARTESIAN_POINT ( 'NONE',  ( 6.385618529757402406, 1.291587659170100766, 1.353439767483602285 ) ) ;
#121778 = CARTESIAN_POINT ( 'NONE',  ( 2.525780997283606499, -1.050937884436175418, -1.492673824175783093 ) ) ;
#121780 = CARTESIAN_POINT ( 'NONE',  ( 6.348661983278831578, 6.841051910588018536, 0.6299351563821649069 ) ) ;
#121779 = CARTESIAN_POINT ( 'NONE',  ( 6.639307388351803674, -1.973492857608965423, 0.9879489342229507143 ) ) ;
#121781 = CARTESIAN_POINT ( 'NONE',  ( -1.364683531250012516, 0.5302083336747518416, 0.7879004041258379498 ) ) ;
#121782 = CARTESIAN_POINT ( 'NONE',  ( 4.369619704168957952, -0.3557292467365941180, 2.031631830423554774 ) ) ;
#121783 = CARTESIAN_POINT ( 'NONE',  ( -8.199983978166823562, 8.461069484149769337, -0.7998128361456291469 ) ) ;
#121784 = CARTESIAN_POINT ( 'NONE',  ( 7.879259827836241570, 12.34422023245099176, 1.040834085586084257E-14 ) ) ;
#121785 = CARTESIAN_POINT ( 'NONE',  ( 6.017121246366603060, 5.914396297049491658, 1.040834085586084257E-14 ) ) ;
#121786 = CARTESIAN_POINT ( 'NONE',  ( -0.09263662810812897663, -9.999999999999994671, -10.91955560153696148 ) ) ;
#121787 = CARTESIAN_POINT ( 'NONE',  ( 6.877413708759195998, -0.1538780216673047430, 2.036608477593480959 ) ) ;
#121788 = CARTESIAN_POINT ( 'NONE',  ( 1.364683531249986537, 0.9677083336747538400, -0.7879004041258239610 ) ) ;
#121789 = CARTESIAN_POINT ( 'NONE',  ( 4.007220386668823409, 1.851715269821294418, 1.114988852100415428 ) ) ;
#121790 = CARTESIAN_POINT ( 'NONE',  ( 3.967448252881644155, -1.680364903119958120, -1.120146540189705497 ) ) ;
#121791 = CARTESIAN_POINT ( 'NONE',  ( 6.620655732516642189, 2.417337544263608251, 2.554705107920357321 ) ) ;
#121792 = B_SPLINE_CURVE_WITH_KNOTS ( 'NONE', 3,
 ( #159607, #17588, #133541, #131425, #201671, #16526, #184369, #197425, #99940, #37058 ),
 .UNSPECIFIED., .F., .F.,
 ( 4, 1, 1, 1, 1, 1, 1, 4 ),
 ( 0.000000000000000000, 0.09599525230796020214, 0.1893027314675523320, 0.2592390727089966540, 0.3619855251144610819, 0.5211967264240887632, 0.7336899926499302893, 1.000000000000000000 ),
 .UNSPECIFIED. ) ;
#121794 = CARTESIAN_POINT ( 'NONE',  ( 6.995644074971448134, 7.263932296995902149, -0.7216878364870257245 ) ) ;
#121793 = CARTESIAN_POINT ( 'NONE',  ( 1.001543065824772753E-15, -3.871874999522043836, 3.793834371823811669 ) ) ;
#121795 = CARTESIAN_POINT ( 'NONE',  ( -8.106849506328558164, 8.422688943663599659, 0.000000000000000000 ) ) ;
#121796 = CARTESIAN_POINT ( 'NONE',  ( 2.132046339962359038, 2.016188815772378629, 0.04465230659478347519 ) ) ;
#121797 = CARTESIAN_POINT ( 'NONE',  ( -7.552055258011950656, 8.769484874890757453, 1.199719254218462483 ) ) ;
#121799 = CARTESIAN_POINT ( 'NONE',  ( -4.303094902415906198, 7.389312076987425648, -1.073240500945132236 ) ) ;
#121798 = CARTESIAN_POINT ( 'NONE',  ( -3.253066792275140173, 5.882662793374543675, 1.199719254218462483 ) ) ;
#121800 = CARTESIAN_POINT ( 'NONE',  ( -7.065207446497166366, 9.336104335703744539, 0.000000000000000000 ) ) ;
#121801 = CARTESIAN_POINT ( 'NONE',  ( 5.273660385517703553, 0.3669835118517565942, -1.876681294024809210 ) ) ;
#121802 = CARTESIAN_POINT ( 'NONE',  ( -2.415323921528888196, 5.969628341758991930, 0.7998128361456341429 ) ) ;
#121803 = CARTESIAN_POINT ( 'NONE',  ( 4.812781342726855982, 7.598366752281232372, 1.082531754730558626 ) ) ;
#121805 = CARTESIAN_POINT ( 'NONE',  ( 4.218375177057286152, 1.978055892313890229, 0.3905773888849966013 ) ) ;
#121804 = CARTESIAN_POINT ( 'NONE',  ( -6.982085920913410071, 11.08959130780024260, 0.7216878364870458196 ) ) ;
#121806 = CARTESIAN_POINT ( 'NONE',  ( -1.201851678989727383E-14, 4.087500000000022560, -1.732050807568863648 ) ) ;
#121807 = CARTESIAN_POINT ( 'NONE',  ( -0.6823417656250003738, 15.21354166700806410, 1.181850606188754593 ) ) ;
#121808 = CARTESIAN_POINT ( 'NONE',  ( 6.422847680425099348, 1.611446996373969265, 0.6153535913232581755 ) ) ;
#121809 = CARTESIAN_POINT ( 'NONE',  ( 6.235824307642648279, 6.239826211863360506, 0.000000000000000000 ) ) ;
#121810 = CARTESIAN_POINT ( 'NONE',  ( 8.676855123066012254, 11.14608361504227574, -1.443375672974052559 ) ) ;
#121811 = CARTESIAN_POINT ( 'NONE',  ( -9.333041836230696831, 14.55305236563169302, -7.472413793098840351 ) ) ;
#121812 = CARTESIAN_POINT ( 'NONE',  ( 6.028550586359523678, 1.802609027081774951, 0.4991829554215552744 ) ) ;
#121813 = CARTESIAN_POINT ( 'NONE',  ( -10.45358220256320436, 1.000000000000000888, 5.892590188894342162 ) ) ;
#121815 = STYLED_ITEM ( 'NONE', ( #34728 ), #61220 ) ;
#121814 = CARTESIAN_POINT ( 'NONE',  ( 2.149362472714404504, 1.803301116200561882, -1.016697834320609672 ) ) ;
#121816 = CARTESIAN_POINT ( 'NONE',  ( -6.414416072596837104, 9.537216947121368804, -1.082531754730549967 ) ) ;
#121817 = VERTEX_POINT ( 'NONE', #63957 ) ;
#121818 = AXIS2_PLACEMENT_3D ( 'NONE', #65001, #147351, #213378 ) ;
#121819 = CARTESIAN_POINT ( 'NONE',  ( 0.5445462702219765472, -1.458543044971000402, 1.392561646250379814 ) ) ;
#121820 = CARTESIAN_POINT ( 'NONE',  ( 5.207740400980577888, 5.248321020665011716, 0.000000000000000000 ) ) ;
#121821 = CARTESIAN_POINT ( 'NONE',  ( -0.4635785636673758758, -6.836568542495036205, -10.85353573482950829 ) ) ;
#121822 = CARTESIAN_POINT ( 'NONE',  ( 6.900736999231407154, 10.99468423250458038, -0.7216878364870267237 ) ) ;
#121823 = CARTESIAN_POINT ( 'NONE',  ( 8.586391356156291010, 8.911878091804165791, 0.7998128361456481317 ) ) ;
#121825 = CARTESIAN_POINT ( 'NONE',  ( 5.817977454128726578, 0.9396041113334742123, -1.669243033268079879 ) ) ;
#121824 = CARTESIAN_POINT ( 'NONE',  ( -6.368579470117215813, 8.453095353268645695, 1.599625672291283607 ) ) ;
#121826 = CARTESIAN_POINT ( 'NONE',  ( 0.1749903794560746517, 0.004523422195302349846, -1.955468523092759314 ) ) ;
#121827 = CARTESIAN_POINT ( 'NONE',  ( -4.151992249809804747, 3.976174039945850502, -0.5918415319043066614 ) ) ;
#121828 = CARTESIAN_POINT ( 'NONE',  ( -0.6823417656250246877, -0.8864583329919115684, 1.181850606188755259 ) ) ;
#121830 = EDGE_LOOP ( 'NONE', ( #52145, #190896, #11096, #98306 ) ) ;
#121829 = CARTESIAN_POINT ( 'NONE',  ( 4.202664430556254160, 5.926194473780837413, 1.443375672974062551 ) ) ;
#121831 = CARTESIAN_POINT ( 'NONE',  ( -6.710922849084449915, 10.77323439066645783, 0.000000000000000000 ) ) ;
#121832 = CARTESIAN_POINT ( 'NONE',  ( 3.045950098598048328, 0.7793912989166664751, -2.016482303682599841 ) ) ;
#121833 = CARTESIAN_POINT ( 'NONE',  ( -2.972980823146582186, 6.690504403638126263, 0.000000000000000000 ) ) ;
#121834 = CARTESIAN_POINT ( 'NONE',  ( 5.506019780925567986, 8.477421273504887722, -1.082531754730548412 ) ) ;
#121835 = CARTESIAN_POINT ( 'NONE',  ( 1.107859837811319581, 1.609452232531217275, 1.380942675281403353 ) ) ;
#121836 = CARTESIAN_POINT ( 'NONE',  ( 5.983392046985361645, 1.685759371660649375, -0.7011634845648376801 ) ) ;
#121837 = ADVANCED_FACE ( 'NONE', ( #95429 ), #33026, .T. ) ;
#121838 = CARTESIAN_POINT ( 'NONE',  ( 1.932829124449897851, 0.1894527445373411501, 1.962211987329742113 ) ) ;
#121839 = CARTESIAN_POINT ( 'NONE',  ( 4.095896644567202038, 1.253117935160457552, 1.444681106026260320 ) ) ;
#121840 = VERTEX_POINT ( 'NONE', #211261 ) ;
#121841 = CARTESIAN_POINT ( 'NONE',  ( -11.52901446936791352, 9.805744725324480271, -3.330874149801263506 ) ) ;
#121842 = CARTESIAN_POINT ( 'NONE',  ( 4.650814871655007288, -0.4294639348428323511, -1.921992245654633447 ) ) ;
#121843 = CARTESIAN_POINT ( 'NONE',  ( 6.585517519612275272, -0.8250364709028266130, 1.756089425624817180 ) ) ;
#121844 = EDGE_LOOP ( 'NONE', ( #101853, #66172, #58606, #142099, #182125 ) ) ;
#121845 = CARTESIAN_POINT ( 'NONE',  ( -4.437261413422502798, 8.398831758960053406, 0.000000000000000000 ) ) ;
#121846 = CARTESIAN_POINT ( 'NONE',  ( -4.442231607132987925, 5.211633625523774960, -1.199719254218453823 ) ) ;
#121848 = CARTESIAN_POINT ( 'NONE',  ( 7.173672674962134899, 7.541908673643526129, -0.7216878364870317197 ) ) ;
#121847 = CARTESIAN_POINT ( 'NONE',  ( 7.741869408603235136, 8.990934717247309749, 1.199719254218462483 ) ) ;
#121850 = ORIENTED_EDGE ( 'NONE', *, *, #110858, .F. ) ;
#121849 = CARTESIAN_POINT ( 'NONE',  ( 5.338497774373327509, 1.135723818413657549, -1.538349510941657838 ) ) ;
#121851 = CARTESIAN_POINT ( 'NONE',  ( 1.360703683432495259, 0.8952624662355922469, 2.017188127302282030 ) ) ;
#121852 = COLOUR_RGB ( '', 0.31764706, 0.68627451, 0.89019608) ;
#121853 = CARTESIAN_POINT ( 'NONE',  ( 9.445304453185899618, 4.469082159062008230, -7.402818517570769252 ) ) ;
#121854 = CARTESIAN_POINT ( 'NONE',  ( 5.777995030156034773, 1.982912992605226465, -0.3464542934713372158 ) ) ;
#121855 = CARTESIAN_POINT ( 'NONE',  ( -0.02319159430947541692, 2.051704324979522820, -2.228571760951563618 ) ) ;
#121856 = CYLINDRICAL_SURFACE ( 'NONE', #194242, 0.07999999999999998779 ) ;
#121857 = CARTESIAN_POINT ( 'NONE',  ( -6.500815856195037767, -6.554751173179672818, -6.901817412891865011 ) ) ;
#121858 = CARTESIAN_POINT ( 'NONE',  ( 3.613788337741298040, 0.5058112091442801272, -2.007490274132675445 ) ) ;
#121859 = CARTESIAN_POINT ( 'NONE',  ( -7.088215381846223906, 7.164006121775713609, 0.7998128361456341429 ) ) ;
#121860 = CARTESIAN_POINT ( 'NONE',  ( -4.934256961717153445, 8.002024883745839645, -1.000413331142641526 ) ) ;
#121862 = CARTESIAN_POINT ( 'NONE',  ( 0.9366540776252421097, 2.129889809250965271, 0.3686189752144660714 ) ) ;
#121861 = CARTESIAN_POINT ( 'NONE',  ( -3.716906668440817185, 7.488141546489591072, 0.7998128361456341429 ) ) ;
#121863 = CARTESIAN_POINT ( 'NONE',  ( -11.32514615057358043, 7.707209080198650142, -3.974810102870973694 ) ) ;
#121864 = CARTESIAN_POINT ( 'NONE',  ( 4.828112100242277549, 6.726159765073026264, -1.443375672974068769 ) ) ;
#121865 = CARTESIAN_POINT ( 'NONE',  ( 1.419999999999990603, 6.216000000000041048, 2.921333333333336668 ) ) ;
#121866 = CARTESIAN_POINT ( 'NONE',  ( -1.364683531250000748, 12.67187500034139980, 0.000000000000000000 ) ) ;
#121868 = CARTESIAN_POINT ( 'NONE',  ( -6.967964602780620353, 7.093989889524320525, 0.000000000000000000 ) ) ;
#121867 = CARTESIAN_POINT ( 'NONE',  ( 6.925078400183555694, 1.300159714275823664, 1.872400972051186496 ) ) ;
#121869 = CARTESIAN_POINT ( 'NONE',  ( 4.957493672250036454, -1.635265592371325960, -0.5776676170772595542 ) ) ;
#121870 = AXIS2_PLACEMENT_3D ( 'NONE', #97966, #180265, #15599 ) ;
#121871 = CARTESIAN_POINT ( 'NONE',  ( -4.548924232584923288, 5.265832011892554121, -1.199719254218446718 ) ) ;
#121872 = CARTESIAN_POINT ( 'NONE',  ( 2.043885321627556095, 1.424625833772466210, 1.502381739045772546 ) ) ;
#121873 = CARTESIAN_POINT ( 'NONE',  ( 4.921547094770428288, -1.498112151610554665, -1.496348102564814209 ) ) ;
#121874 = CARTESIAN_POINT ( 'NONE',  ( 7.786460292950004636, 7.978625184730144149, 1.040834085586084257E-14 ) ) ;
#121875 = CARTESIAN_POINT ( 'NONE',  ( 0.4170821662628915183, 3.033599471985643170, 0.4170821662628724225 ) ) ;
#121876 = CARTESIAN_POINT ( 'NONE',  ( 2.061320199224637051, 1.634538341387161475, 1.098309876814192565 ) ) ;
#121877 = CARTESIAN_POINT ( 'NONE',  ( 5.904500254309781759, 6.149185751451256898, 0.8064407133735688182 ) ) ;
#121878 = CARTESIAN_POINT ( 'NONE',  ( -0.4655551865852154414, -8.176568542494919711, -9.512045263456256450 ) ) ;
#121879 = CARTESIAN_POINT ( 'NONE',  ( 5.033284615878021562, -1.618354306187347769, -1.623638663579999752 ) ) ;
#121881 = EDGE_CURVE ( 'NONE', #135098, #13166, #178794, .T. ) ;
#121880 = CARTESIAN_POINT ( 'NONE',  ( 1.471042373949003501, 0.1361147407585860392, -1.820667060309004937 ) ) ;
#121882 = CARTESIAN_POINT ( 'NONE',  ( 6.039231080244466199, 6.010467446565510130, 0.7998128361456352531 ) ) ;
#121883 = CARTESIAN_POINT ( 'NONE',  ( 6.466876083594112146, 6.647036307055676829, -0.7216878364870257245 ) ) ;
#121884 = CARTESIAN_POINT ( 'NONE',  ( -8.355902744723985975, 8.642974711799791265, 1.040834085586084257E-14 ) ) ;
#121885 = CARTESIAN_POINT ( 'NONE',  ( 2.320566727126192053, -0.7743817983801875027, -1.858503283895854841 ) ) ;
#121886 = CARTESIAN_POINT ( 'NONE',  ( 3.010546455304231372, 0.6564385890225448161, 1.848828695667027677 ) ) ;
#121887 = CARTESIAN_POINT ( 'NONE',  ( -9.345647958521597687, 9.797677461230342999, 0.7998128361456462443 ) ) ;
#121888 = CARTESIAN_POINT ( 'NONE',  ( -4.564291269294938225, 8.476756914152748124, 1.040834085586084257E-14 ) ) ;
#121890 = ADVANCED_FACE ( 'NONE', ( #148419 ), #181734, .T. ) ;
#121889 = DIRECTION ( 'NONE',  ( 0.000000000000000000, -1.000000000000000000, 0.000000000000000000 ) ) ;
#121892 = CARTESIAN_POINT ( 'NONE',  ( 4.645211000723334926, -1.368906681764755939, -1.121767690593698186 ) ) ;
#121891 = CARTESIAN_POINT ( 'NONE',  ( 5.982390446235332782, -0.3055207467456683701, -2.068066053634140200 ) ) ;
#121893 = CARTESIAN_POINT ( 'NONE',  ( -1.499999999999997780, 3.431250000682818602, 1.214306433183764966E-14 ) ) ;
#121894 = CARTESIAN_POINT ( 'NONE',  ( 1.236564921189796662, 0.4304113295856801247, 2.148598399174222351 ) ) ;
#121895 = CARTESIAN_POINT ( 'NONE',  ( -0.04197470322641042723, -1.553021824201283208, -0.7857045047398486526 ) ) ;
#121896 = MECHANICAL_DESIGN_GEOMETRIC_PRESENTATION_REPRESENTATION (  '', ( #25028 ), #111526 ) ;
#121897 = CARTESIAN_POINT ( 'NONE',  ( 6.577677080924314801, 10.82570702772039262, 1.040834085586084257E-14 ) ) ;
#121898 = CARTESIAN_POINT ( 'NONE',  ( 0.1333692844072802142, 0.2389375359408679178, -2.087895146362698906 ) ) ;
#121899 = CARTESIAN_POINT ( 'NONE',  ( 5.678471694547736703, 1.738760799997655537, 1.503693327295371862 ) ) ;
#121900 = CARTESIAN_POINT ( 'NONE',  ( -0.09381621004311831158, -0.9424329983100244723, -1.976553698157037076 ) ) ;
#121901 = CARTESIAN_POINT ( 'NONE',  ( 5.993412714446900047, 1.671717086469927560, 0.4595231857335341785 ) ) ;
#121902 = CARTESIAN_POINT ( 'NONE',  ( 2.368051099418837069, 2.164043333312406503, -0.4318774905316472013 ) ) ;
#121903 = CARTESIAN_POINT ( 'NONE',  ( 0.2511275705787468504, -0.4786951167374750571, -2.125832126681607370 ) ) ;
#121904 = DIRECTION ( 'NONE',  ( 0.000000000000000000, 0.000000000000000000, 1.000000000000000000 ) ) ;
#121905 = CARTESIAN_POINT ( 'NONE',  ( 1.446650934045516701, -1.493148645901293925, 1.501467539593546840 ) ) ;
#121906 = CARTESIAN_POINT ( 'NONE',  ( 3.531250000000002220, -0.7852924748301699509, -1.895863743164005744 ) ) ;
#121907 = CARTESIAN_POINT ( 'NONE',  ( 6.727182134110195832, 3.687949058358138466, 2.603069318070629912 ) ) ;
#121908 = CARTESIAN_POINT ( 'NONE',  ( 4.313445203237777470, -0.3300861979738233254, 1.897755268844825816 ) ) ;
#121909 = CARTESIAN_POINT ( 'NONE',  ( 0.9619568641448449364, -1.754440713604523916, -1.362318395052774633 ) ) ;
#121910 = ORIENTED_EDGE ( 'NONE', *, *, #53099, .T. ) ;
#121912 = CARTESIAN_POINT ( 'NONE',  ( -0.7500000000000215383, 4.191666666666690411, 1.299038105676671107 ) ) ;
#121911 = CARTESIAN_POINT ( 'NONE',  ( 1.611265326866499148, -0.2753845699034764838, 2.275703152891339176 ) ) ;
#121913 = CARTESIAN_POINT ( 'NONE',  ( 3.486418057008484617, 7.219238166485217434, 1.040834085586084257E-14 ) ) ;
#121914 = CARTESIAN_POINT ( 'NONE',  ( 6.817052309572890323, 6.847649204123507083, 0.7998128361456341429 ) ) ;
#121915 = CARTESIAN_POINT ( 'NONE',  ( 3.756649600333416217, 2.210663847611141986, 0.2169408864148083815 ) ) ;
#121916 = CARTESIAN_POINT ( 'NONE',  ( -9.015808963407680565, 9.620791333504852716, 1.040834085586084257E-14 ) ) ;
#121917 = CARTESIAN_POINT ( 'NONE',  ( -0.9679107548764689373, -4.157144623729469579, 0.3235293953616469320 ) ) ;
#121918 = CARTESIAN_POINT ( 'NONE',  ( 6.480434237652124452, 8.583592582059388576, 1.443375672974076540 ) ) ;
#121919 = CARTESIAN_POINT ( 'NONE',  ( -7.483737604619046913, 11.67485160545682987, 0.000000000000000000 ) ) ;
#121920 = EDGE_CURVE ( 'NONE', #169596, #124, #16659, .T. ) ;
#121921 = CARTESIAN_POINT ( 'NONE',  ( 6.916067756746836714, 8.201738816693689316, -1.082531754730548412 ) ) ;
#121922 = ORIENTED_EDGE ( 'NONE', *, *, #66705, .T. ) ;
#121923 = CARTESIAN_POINT ( 'NONE',  ( 1.617814789376757156, 0.2004366740697149929, 2.006445999502483257 ) ) ;
#121925 = CARTESIAN_POINT ( 'NONE',  ( 6.232891784722141892, -1.957473889884550289, -0.6504925196839649315 ) ) ;
#121924 = CARTESIAN_POINT ( 'NONE',  ( 8.535021395002688749, 9.916278701380017324, 1.199719254218462483 ) ) ;
#121926 = CARTESIAN_POINT ( 'NONE',  ( 6.333067150914808430, 8.481940657524365434, 1.443375672974063439 ) ) ;
#121927 = CARTESIAN_POINT ( 'NONE',  ( -0.1296875068448159751, 0.001480089298542403009, -1.826395826379861864 ) ) ;
#121928 = CARTESIAN_POINT ( 'NONE',  ( -2.300042508418743914, 5.503185706334628335, -0.7429425145402666075 ) ) ;
#121929 = CARTESIAN_POINT ( 'NONE',  ( 0.6823417656249899377, 2.592708333674753618, 1.181850606188767472 ) ) ;
#121930 = CARTESIAN_POINT ( 'NONE',  ( 1.246904684444858136, -1.390570190391905658, -1.094529049636628226 ) ) ;
#121931 = CARTESIAN_POINT ( 'NONE',  ( 0.3873425458618062200, -0.6819987885887256462, -1.897696807414723796 ) ) ;
#121932 = CARTESIAN_POINT ( 'NONE',  ( -0.07694640568740516995, -1.131669979810394633, -1.452919414246391261 ) ) ;
#121933 = CARTESIAN_POINT ( 'NONE',  ( 3.650172380179962150, 0.8259502761284505112, 2.138564905064809896 ) ) ;
#121934 = CARTESIAN_POINT ( 'NONE',  ( 3.152128525617302834, -1.393660036906883226, 1.203213496783587910 ) ) ;
#121935 = CARTESIAN_POINT ( 'NONE',  ( 9.284636267260101050, 9.726497154758602548, -0.7998128361456281477 ) ) ;
#121936 = CARTESIAN_POINT ( 'NONE',  ( 10.20550892794189579, 9.995811918519301287, 6.492953855302722843 ) ) ;
#121937 = CARTESIAN_POINT ( 'NONE',  ( 3.047666980291532823, 0.6586017179070653427, -1.702814618940437619 ) ) ;
#121938 = CARTESIAN_POINT ( 'NONE',  ( 3.920546200773936896, -1.392545040883992336, -1.458557299768625581 ) ) ;
#121939 = CARTESIAN_POINT ( 'NONE',  ( -9.317477881089553549, 11.89347683273641820, 1.599625672291281386 ) ) ;
#121941 = CARTESIAN_POINT ( 'NONE',  ( -5.420227550413282636, 9.545625585449309725, 0.7998128361456291469 ) ) ;
#121940 = CARTESIAN_POINT ( 'NONE',  ( 3.327297708271567345, 0.05365531978675056046, 2.262033696468904065 ) ) ;
#121942 = CARTESIAN_POINT ( 'NONE',  ( 5.526436043951506782, 1.257118228488460110, -1.689427636868174210 ) ) ;
#121943 = CARTESIAN_POINT ( 'NONE',  ( 8.057215556046470439, 15.94308538975788281, 9.795211633567449283 ) ) ;
#121944 = CARTESIAN_POINT ( 'NONE',  ( 3.420434311836465291, 0.9283866757503267397, 1.850595421526677775 ) ) ;
#121945 = CARTESIAN_POINT ( 'NONE',  ( 4.390142812726693045, 4.016254791136236513, 1.214306433183764966E-14 ) ) ;
#121946 = CARTESIAN_POINT ( 'NONE',  ( 1.360316468749987573, 1.817708333674738608, -0.7853790794158981292 ) ) ;
#121947 = CARTESIAN_POINT ( 'NONE',  ( 5.268275487455277073, 2.118052368503114291, -0.1043780312826799589 ) ) ;
#121949 = CARTESIAN_POINT ( 'NONE',  ( 1.137189532436083672, -1.741952243817600721, 0.8230948124841385161 ) ) ;
#121948 = CARTESIAN_POINT ( 'NONE',  ( -9.677822722056413696, 10.18521468535430685, 1.040834085586084257E-14 ) ) ;
#121950 = CARTESIAN_POINT ( 'NONE',  ( -3.546339698426324460, 6.295090860542775779, -1.199719254218450271 ) ) ;
#121951 = CARTESIAN_POINT ( 'NONE',  ( 9.368847842243145152, 10.88907622316056312, 1.199719254218453823 ) ) ;
#121952 = CARTESIAN_POINT ( 'NONE',  ( 3.675669042636310557, 6.342012078834061484, -1.082531754730549967 ) ) ;
#121953 = CARTESIAN_POINT ( 'NONE',  ( 5.335014106237911946, 6.336523053015567619, 1.100733037772538170 ) ) ;
#121954 = DIRECTION ( 'NONE',  ( 0.000000000000000000, -1.000000000000000000, 0.000000000000000000 ) ) ;
#121955 = CARTESIAN_POINT ( 'NONE',  ( -4.765854690403601879, 5.518917546014321829, 1.199719254218462483 ) ) ;
#121956 = CARTESIAN_POINT ( 'NONE',  ( 0.7212869692094016072, 1.677245448433011710, -1.456619292340176841 ) ) ;
#121957 = CARTESIAN_POINT ( 'NONE',  ( 2.221831145078187575, -2.042928948074810069, 0.5108812299794410761 ) ) ;
#121958 = CARTESIAN_POINT ( 'NONE',  ( -2.830620210203090181, 6.524417021870718258, 0.000000000000000000 ) ) ;
#121959 = CARTESIAN_POINT ( 'NONE',  ( 7.426115451983150706, 9.686887332112256388, -1.599625672291262513 ) ) ;
#121960 = CARTESIAN_POINT ( 'NONE',  ( 0.1388275050690327694, -0.1366109201720016320, -1.830645452005694951 ) ) ;
#121961 = CARTESIAN_POINT ( 'NONE',  ( 7.786460292950004636, 7.978625184730144149, 1.040834085586084257E-14 ) ) ;
#121962 = DIRECTION ( 'NONE',  ( 0.000000000000000000, 0.000000000000000000, 1.000000000000000000 ) ) ;
#121963 = CARTESIAN_POINT ( 'NONE',  ( -6.617788377246193399, 8.814115421577600529, -1.443375672974066548 ) ) ;
#121964 = CARTESIAN_POINT ( 'NONE',  ( -7.361714222540411967, 11.53249099303175385, 0.000000000000000000 ) ) ;
#121965 = AXIS2_PLACEMENT_3D ( 'NONE', #137633, #152797, #85659 ) ;
#121966 = CARTESIAN_POINT ( 'NONE',  ( 1.758217466200185042, 0.8068918862002281145, -1.961288232260410380 ) ) ;
#121967 = CARTESIAN_POINT ( 'NONE',  ( -7.370792787684826486, 8.628288336167626582, -1.199719254218452047 ) ) ;
#121969 = CARTESIAN_POINT ( 'NONE',  ( 3.771884902471400292, -1.933230903833718539, 0.3329965046865584477 ) ) ;
#121968 = CARTESIAN_POINT ( 'NONE',  ( -4.757329562667670667E-14, -0.1874999999999768518, 1.414508159514551444 ) ) ;
#121970 = CARTESIAN_POINT ( 'NONE',  ( 1.780366757100563913, -1.156431984057613827, 1.826190802295484472 ) ) ;
#121971 = EDGE_CURVE ( 'NONE', #75305, #82411, #140637, .T. ) ;
#121972 = CARTESIAN_POINT ( 'NONE',  ( 1.768857366986800406, 1.761637791510446860, -0.5354853023365884201 ) ) ;
#121973 =( GEOMETRIC_REPRESENTATION_CONTEXT ( 3 ) GLOBAL_UNCERTAINTY_ASSIGNED_CONTEXT ( ( #112346 ) ) GLOBAL_UNIT_ASSIGNED_CONTEXT ( ( #145452, #62026, #209304 ) ) REPRESENTATION_CONTEXT ( 'NONE', 'WORKASPACE' ) );
#121975 = CARTESIAN_POINT ( 'NONE',  ( -4.610256348478378285, 6.944848931137240555, -1.199160056556654697 ) ) ;
#121974 = CARTESIAN_POINT ( 'NONE',  ( -5.255720823952942489, 6.160704378480398979, -1.199719254218453823 ) ) ;
#121976 = CARTESIAN_POINT ( 'NONE',  ( 3.679424820307465538, -0.8558964687110992564, 1.515225693578539978 ) ) ;
#121977 = CARTESIAN_POINT ( 'NONE',  ( 6.399085315970131305, 8.488685506763726352, -1.443375672974057666 ) ) ;
#121978 = CARTESIAN_POINT ( 'NONE',  ( -11.30309668167796922, 5.150585336095397260, -5.742054036728555744 ) ) ;
#121979 = CARTESIAN_POINT ( 'NONE',  ( 0.7608789386071808103, -1.564954856162886765, 1.491513986042219297 ) ) ;
#121980 = CARTESIAN_POINT ( 'NONE',  ( 3.919295934624257960, 0.7230291454519314209, 1.882185965797255278 ) ) ;
#121981 = CARTESIAN_POINT ( 'NONE',  ( 6.825078400183518745, 0.5555073798480349989, 2.295529415773037929 ) ) ;
#121982 = CARTESIAN_POINT ( 'NONE',  ( 0.1105426557568081891, -0.9253945370547181914, -1.951590883024490353 ) ) ;
#121983 = SHAPE_REPRESENTATION ( 'screw coil', ( #200407 ), #141734 ) ;
#121984 = CARTESIAN_POINT ( 'NONE',  ( 2.799638878761875116, -0.6198165829789729075, 1.871555056500016745 ) ) ;
#121985 = CARTESIAN_POINT ( 'NONE',  ( 6.609000000000042618, 6.036791015687303918, 2.594900324319386886 ) ) ;
#121986 = CARTESIAN_POINT ( 'NONE',  ( 2.454547613406708351, -1.690768538996465509, -0.9553028803331271579 ) ) ;
#121989 = ORIENTED_EDGE ( 'NONE', *, *, #174645, .T. ) ;
#121988 = CARTESIAN_POINT ( 'NONE',  ( -4.123088112331656951, 6.864000993478624579, 1.082531754730549967 ) ) ;
#121987 = CARTESIAN_POINT ( 'NONE',  ( -2.440293211016301606E-15, 1.312499999999991118, 1.224999999999973888 ) ) ;
#121990 = CARTESIAN_POINT ( 'NONE',  ( -5.329763783503577379, 6.351050847909847086, 1.082531754730549078 ) ) ;
#121991 = CARTESIAN_POINT ( 'NONE',  ( -0.1106856583840877539, 4.089587022985669229, -2.551888050631024640 ) ) ;
#121992 = CARTESIAN_POINT ( 'NONE',  ( 3.739016502318667445, 7.584212696005614873, 0.7998128361456271485 ) ) ;
#121993 = CARTESIAN_POINT ( 'NONE',  ( -6.303615075710993665, 6.318915441276411471, -0.7998128361456362523 ) ) ;
#121994 = CARTESIAN_POINT ( 'NONE',  ( -5.108390017298964914, 9.181815130149269422, 0.000000000000000000 ) ) ;
#121995 = CARTESIAN_POINT ( 'NONE',  ( -0.4000000000000131783, 3.372708439410149417, -0.5000000000000160982 ) ) ;
#121996 = CARTESIAN_POINT ( 'NONE',  ( 6.352564483950959406, 0.7153834962906236994, 2.193980215933882150 ) ) ;
#121997 = CARTESIAN_POINT ( 'NONE',  ( 6.760214184729610665, -1.961454122871961747, 0.04698431645466792650 ) ) ;
#121998 = CARTESIAN_POINT ( 'NONE',  ( 4.223457129239616137, 0.2443821477370981265, -1.946437379933690481 ) ) ;
#121999 = CARTESIAN_POINT ( 'NONE',  ( 6.611572464958476836, 10.86525164242692298, 0.7998128361456462443 ) ) ;
#122000 = CARTESIAN_POINT ( 'NONE',  ( 0.9674229098759130618, -1.967888300253183953, -0.4390273639364171698 ) ) ;
#122001 = ORIENTED_EDGE ( 'NONE', *, *, #71255, .F. ) ;
#122002 = CARTESIAN_POINT ( 'NONE',  ( 2.501287867402203879, -0.2026288386562236921, 2.107594835487134777 ) ) ;
#122003 = CARTESIAN_POINT ( 'NONE',  ( -1.500000000000013101, 2.202083334016153859, 0.8660254037844403729 ) ) ;
#122005 = CARTESIAN_POINT ( 'NONE',  ( -7.542413527904030524, 7.693903958843159252, 1.040834085586084257E-14 ) ) ;
#122004 = CARTESIAN_POINT ( 'NONE',  ( -3.810004860640155311, 4.403759411290286252, 1.199719254218462483 ) ) ;
#122006 = CARTESIAN_POINT ( 'NONE',  ( 3.609164914601064922, -1.813629950718143702, 0.3161406477080672128 ) ) ;
#122007 = ORIENTED_EDGE ( 'NONE', *, *, #131977, .F. ) ;
#122008 = CARTESIAN_POINT ( 'NONE',  ( -10.08065090696061716, 11.71951313199760136, -1.199719254218441611 ) ) ;
#122009 = CARTESIAN_POINT ( 'NONE',  ( 4.166350089634453191, 2.120059694336435374, -0.05518752902338577848 ) ) ;
#122010 = CARTESIAN_POINT ( 'NONE',  ( 0.1636598862229492191, -1.205073137261414962, 1.392071761982638378 ) ) ;
#122011 = DIRECTION ( 'NONE',  ( -1.000000000000000000, -1.224646799147343593E-16, 0.000000000000000000 ) ) ;
#122012 = CARTESIAN_POINT ( 'NONE',  ( 6.449928391799196525, 8.548002428564306143, -1.599625672291262513 ) ) ;
#122013 = CARTESIAN_POINT ( 'NONE',  ( 5.203297092594585393, 9.292540051327542017, 0.7998128361456341429 ) ) ;
#122014 = CARTESIAN_POINT ( 'NONE',  ( 4.077457721052785367, 1.941698500476006117, -0.6908173846359686454 ) ) ;
#122016 = CARTESIAN_POINT ( 'NONE',  ( 1.505144418776669601, -1.827259764946763454, 0.2261131901925839127 ) ) ;
#122015 = CARTESIAN_POINT ( 'NONE',  ( -7.901704598666176693, 8.113076874732334076, 0.7998128361456602331 ) ) ;
#122017 = CARTESIAN_POINT ( 'NONE',  ( 1.364683531249988535, 4.905208333674756283, -0.7879004041258300672 ) ) ;
#122018 = CARTESIAN_POINT ( 'NONE',  ( -5.458264003855187951, 7.602368174425947700, -1.382272695577278387 ) ) ;
#122019 =( NAMED_UNIT ( * ) PLANE_ANGLE_UNIT ( ) SI_UNIT ( $, .RADIAN. ) );
#122020 = CARTESIAN_POINT ( 'NONE',  ( 10.99861980075107581, -8.407420853759273172, -0.1919816227428499389 ) ) ;
#122021 = CARTESIAN_POINT ( 'NONE',  ( 0.6630615684519860498, -1.595754342771567025, 1.524677653706180802 ) ) ;
#122022 = B_SPLINE_CURVE_WITH_KNOTS ( 'NONE', 3,
 ( #99502, #196989, #133098, #82165, #146141, #78968, #96321, #162375, #214259, #179688 ),
 .UNSPECIFIED., .F., .F.,
 ( 4, 3, 3, 4 ),
 ( 0.000000000000000000, 8.736270215687113379E-05, 0.0001565438449761693651, 0.0002258025094466979254 ),
 .UNSPECIFIED. ) ;
#122023 = CARTESIAN_POINT ( 'NONE',  ( 3.901889172025752472, -0.6612649319669267056, 2.163591406342895596 ) ) ;
#122024 = CARTESIAN_POINT ( 'NONE',  ( -8.703971430293361067, 9.256980878204810637, 0.7216878364870438212 ) ) ;
#122025 = CARTESIAN_POINT ( 'NONE',  ( 3.498146571883210321, -0.8881612436112231723, 1.578813691393302410 ) ) ;
#122026 = CARTESIAN_POINT ( 'NONE',  ( 3.784325452683900526, -0.6063896298742013080, -1.817255877250848473 ) ) ;
#122027 = CARTESIAN_POINT ( 'NONE',  ( 5.898901817742318698, 0.4001337562283372451, 2.031160294743330486 ) ) ;
#122028 = CARTESIAN_POINT ( 'NONE',  ( 1.364683531249988535, 4.717708333674756283, -0.7879004041258300672 ) ) ;
#122029 = ADVANCED_FACE ( 'NONE', ( #51977, #152664, #86598 ), #184087, .T. ) ;
#122030 = CARTESIAN_POINT ( 'NONE',  ( 2.395336953769642729, 1.522948423943527363, 1.251906274522778251 ) ) ;
#122031 = CARTESIAN_POINT ( 'NONE',  ( 1.237189336409921570, -1.742702465754492058, 0.8212270227533255973 ) ) ;
#122032 = CARTESIAN_POINT ( 'NONE',  ( 4.117926171558832671, -0.9613396577640184182, -1.604580606731422554 ) ) ;
#122033 = CARTESIAN_POINT ( 'NONE',  ( 3.317284684000018746, 2.086097511483188338, 0.9870085806921449212 ) ) ;
#122034 = CARTESIAN_POINT ( 'NONE',  ( 3.174093412877276865, -0.9148440431442562693, -1.620569831483926082 ) ) ;
#122035 = CARTESIAN_POINT ( 'NONE',  ( -1.201851678989727383E-14, 3.946875000341423689, -1.575800808251660134 ) ) ;
#122036 = VECTOR ( 'NONE', #5802, 1000.000000000000000 ) ;
#122037 = CARTESIAN_POINT ( 'NONE',  ( 4.857564175446106525, 8.889184981320973122, 0.7998128361456331437 ) ) ;
#122038 = DIRECTION ( 'NONE',  ( 0.9982742078614211811, 0.000000000000000000, 0.05872483221476467591 ) ) ;
#122039 = CARTESIAN_POINT ( 'NONE',  ( 1.014449334229026611, -0.9484566428747326361, -1.880489036503508959 ) ) ;
#122040 = CARTESIAN_POINT ( 'NONE',  ( 3.592547517496925913, 5.214391408544949869, -1.443375672974058777 ) ) ;
#122042 = DIRECTION ( 'NONE',  ( -0.000000000000000000, 1.000000000000000000, -0.000000000000000000 ) ) ;
#122041 = CARTESIAN_POINT ( 'NONE',  ( -0.6823417656249969321, 5.280208333674756283, -1.181850606188749264 ) ) ;
#122043 = DIRECTION ( 'NONE',  ( 1.000000000000000000, -0.000000000000000000, -0.000000000000000000 ) ) ;
#122044 = CARTESIAN_POINT ( 'NONE',  ( 4.450244736157840109, 7.987476157872942295, -2.500000000000000444 ) ) ;
#122045 = CARTESIAN_POINT ( 'NONE',  ( 1.090109951703751801, 1.206612241219229942, 1.619577932830415623 ) ) ;
#122046 = CARTESIAN_POINT ( 'NONE',  ( 0.6823417656249899377, 1.342708333674752508, 1.181850606188755259 ) ) ;
#122047 = CARTESIAN_POINT ( 'NONE',  ( -4.772106882330247046, 4.669805572247793357, -0.7216878364870207285 ) ) ;
#122048 = CARTESIAN_POINT ( 'NONE',  ( 3.811813743736467419, 7.598866467667865443, 1.040834085586084257E-14 ) ) ;
#122049 = EDGE_LOOP ( 'NONE', ( #22885, #102693, #51599, #174725 ) ) ;
#122050 = CARTESIAN_POINT ( 'NONE',  ( 1.581558009922879204, 1.997867266642009643, -0.8257073301623578665 ) ) ;
#122051 = DIRECTION ( 'NONE',  ( 0.000000000000000000, 1.000000000000000000, 0.000000000000000000 ) ) ;
#122054 = CARTESIAN_POINT ( 'NONE',  ( 3.063779527008311021, 5.557864633942907417, 1.082531754730546636 ) ) ;
#122053 = CARTESIAN_POINT ( 'NONE',  ( 6.825078400183548055, 3.702925343214446663, 2.370119418288775925 ) ) ;
#122052 = CARTESIAN_POINT ( 'NONE',  ( 6.561219994370630637, 6.619454513046008515, 0.000000000000000000 ) ) ;
#122055 = CARTESIAN_POINT ( 'NONE',  ( -1.299038105676632915, 6.499999999999999112, -0.7500000000000006661 ) ) ;
#122056 = CARTESIAN_POINT ( 'NONE',  ( 5.366422816783521732, -1.968444216653497003, -0.4370823996120917765 ) ) ;
#122057 = CARTESIAN_POINT ( 'NONE',  ( -6.697364695470783502, 10.75741654478384035, 0.7216878364870458196 ) ) ;
#122058 = CARTESIAN_POINT ( 'NONE',  ( 0.06437606466144081552, -1.426665095847098330, 1.663708609037084951 ) ) ;
#122059 = CARTESIAN_POINT ( 'NONE',  ( 1.897353801849633006E-16, -6.452016312669676346, -11.25751254361623843 ) ) ;
#122061 = CARTESIAN_POINT ( 'NONE',  ( -0.6823417656250003738, 11.15104166700806765, 1.181850606188754593 ) ) ;
#122060 = CARTESIAN_POINT ( 'NONE',  ( 6.702040708066513197, -2.161345696851162845, 0.04751196314212167288 ) ) ;
#122062 = CARTESIAN_POINT ( 'NONE',  ( -7.947050595904583403, 12.42330946186405249, 0.7998128361456481317 ) ) ;
#122064 = CARTESIAN_POINT ( 'NONE',  ( 1.458442676765151269, -1.819496111524568027, -0.5994125798251969117 ) ) ;
#122063 = CARTESIAN_POINT ( 'NONE',  ( -4.406036734316882253, 8.084200590104265061, -0.7216878364870257245 ) ) ;
#122065 = CARTESIAN_POINT ( 'NONE',  ( 1.364683531249988535, 2.426041667008088432, 0.7879004041258500513 ) ) ;
#122066 = CARTESIAN_POINT ( 'NONE',  ( 6.343551558972070126, 6.506286488053498296, 2.500000000000000000 ) ) ;
#122067 = AXIS2_PLACEMENT_3D ( 'NONE', #26393, #3984, #122126 ) ;
#122068 = CARTESIAN_POINT ( 'NONE',  ( -0.7500000000000006661, 9.458333333333332149, -1.299038105676657340 ) ) ;
#122069 = CARTESIAN_POINT ( 'NONE',  ( 2.789346554370454534, 1.219787599184172233, 1.219827592095571456 ) ) ;
#122070 = CARTESIAN_POINT ( 'NONE',  ( 4.553559489343365740, 6.405848385690952718, -1.599625672291269396 ) ) ;
#122071 = CARTESIAN_POINT ( 'NONE',  ( 1.985279565377489508, 1.216254750358658487, 1.285827030011628347 ) ) ;
#122072 =( BOUNDED_CURVE ( )  B_SPLINE_CURVE ( 3, ( #133490, #198429, #97776, #16477 ),
 .UNSPECIFIED., .F., .T. ) 
 B_SPLINE_CURVE_WITH_KNOTS ( ( 4, 4 ),
 ( 3.705870088530484718, 4.712388980384521808 ),
 .UNSPECIFIED. ) 
 CURVE ( )  GEOMETRIC_REPRESENTATION_ITEM ( )  RATIONAL_B_SPLINE_CURVE ( ( 1.000000000000000000, 0.9173434942194278463, 0.9173434942194278463, 1.000000000000000000 ) ) 
 REPRESENTATION_ITEM ( '' )  );
#122073 = CARTESIAN_POINT ( 'NONE',  ( 2.490887342608373078, -1.927107516443892221, -0.5821121120333644372 ) ) ;
#122074 = CARTESIAN_POINT ( 'NONE',  ( 10.07387183015377197, 11.71160420905630062, -1.199719254218440723 ) ) ;
#122075 = CARTESIAN_POINT ( 'NONE',  ( 5.280388062626482970, -1.229865305990836877, 1.832093573602276759 ) ) ;
#122076 = VERTEX_POINT ( 'NONE', #2114 ) ;
#122077 = CARTESIAN_POINT ( 'NONE',  ( -7.937372586157736443, 8.224965870130965584, 0.7998128361456341429 ) ) ;
#122079 = CARTESIAN_POINT ( 'NONE',  ( 4.271111354109316416, 1.799915745204151429, -0.9091612155255476280 ) ) ;
#122078 = CARTESIAN_POINT ( 'NONE',  ( 4.617906949270495609, -0.5647423089508787353, 2.043846993246847710 ) ) ;
#122081 = EDGE_LOOP ( 'NONE', ( #29307, #145433, #2496, #192979 ) ) ;
#122080 = CARTESIAN_POINT ( 'NONE',  ( 4.588045372560112689, 1.048790434826195384, 1.476901585074356316 ) ) ;
#122082 = CARTESIAN_POINT ( 'NONE',  ( 4.199993725183334803, 8.122019456014369254, -0.7998128361456362523 ) ) ;
#122083 = ORIENTED_EDGE ( 'NONE', *, *, #168967, .T. ) ;
#122084 = CARTESIAN_POINT ( 'NONE',  ( 1.639302681421180852, -1.352760811461351187, -1.292285834730774852 ) ) ;
#122085 = CARTESIAN_POINT ( 'NONE',  ( 6.674438497507635404, -1.118711561685633349, 1.443368817030561635 ) ) ;
#122086 = CARTESIAN_POINT ( 'NONE',  ( 6.076794983551159213, -1.275939312151072258, 1.286130553019491307 ) ) ;
#122087 = CARTESIAN_POINT ( 'NONE',  ( -3.277320446201389181, 4.846626492033466072, 1.599625672291267398 ) ) ;
#122088 = CARTESIAN_POINT ( 'NONE',  ( -11.69084473744764097, 4.401359152538248054, -5.144113628910231384 ) ) ;
#122089 = CARTESIAN_POINT ( 'NONE',  ( -3.939498435241230556, 2.812004590916141744, 0.7750000000000135669 ) ) ;
#122090 = CARTESIAN_POINT ( 'NONE',  ( 0.6823417656249899377, 3.155208333674754062, 1.181850606188765695 ) ) ;
#122091 = FILL_AREA_STYLE ('',( #158775 ) ) ;
#122092 = CARTESIAN_POINT ( 'NONE',  ( 5.994113311017540191, 9.046863725278862844, -1.082531754730548412 ) ) ;
#122093 = CARTESIAN_POINT ( 'NONE',  ( -4.828112100242303306, 4.805421336470338645, -0.7216878364870338292 ) ) ;
#122094 = CARTESIAN_POINT ( 'NONE',  ( -6.448838341955544173, 7.552674816150118708, 1.199719254218452047 ) ) ;
#122095 = CARTESIAN_POINT ( 'NONE',  ( 4.183913158364858553, 2.056144659531285779, -0.5182805708664263156 ) ) ;
#122097 = CARTESIAN_POINT ( 'NONE',  ( -10.05286969158539812, 5.876479340494690895, 5.831501649199077875 ) ) ;
#122096 = CARTESIAN_POINT ( 'NONE',  ( -0.1296875068447916890, 6.948706544289747988, -2.421546651465163347 ) ) ;
#122098 = CARTESIAN_POINT ( 'NONE',  ( 6.098895391831223201, 1.613120528903468243, -1.132937624142603905 ) ) ;
#122099 = CARTESIAN_POINT ( 'NONE',  ( 0.6823417656249882723, 0.6760416670080898749, -1.181850606188749264 ) ) ;
#122100 = CARTESIAN_POINT ( 'NONE',  ( 0.4396980093101590659, -1.910362728465137439, 0.6353400594101745735 ) ) ;
#122101 = ORIENTED_EDGE ( 'NONE', *, *, #66969, .T. ) ;
#122102 = CARTESIAN_POINT ( 'NONE',  ( 0.1931602983361295767, 1.844477155017531844, 1.039358475685886907 ) ) ;
#122103 = CARTESIAN_POINT ( 'NONE',  ( 8.880228351732188941, 12.81718488518845156, 8.003373899717370676 ) ) ;
#122104 = CARTESIAN_POINT ( 'NONE',  ( 2.049362625460974030, 1.802418521853879962, -1.018503948505583789 ) ) ;
#122105 = ORIENTED_EDGE ( 'NONE', *, *, #137465, .F. ) ;
#122106 = CARTESIAN_POINT ( 'NONE',  ( 5.204350862799327793, 7.165104988056252289, -1.599625672291281386 ) ) ;
#122107 = CARTESIAN_POINT ( 'NONE',  ( 4.549643065837591038, 7.465611455855944101, -1.199719254218452047 ) ) ;
#122109 = CARTESIAN_POINT ( 'NONE',  ( 4.924636110261782385, 6.768494766770632332, 1.599625672291267398 ) ) ;
#122108 = CARTESIAN_POINT ( 'NONE',  ( 4.769523239323490316, 1.203412094891454842, 1.709343392706575315 ) ) ;
#122110 = CARTESIAN_POINT ( 'NONE',  ( 6.068156270568149324, 9.237210194708310951, 1.199719254218452047 ) ) ;
#122113 = EDGE_LOOP ( 'NONE', ( #109921, #190876, #68911, #81309 ) ) ;
#122112 = CARTESIAN_POINT ( 'NONE',  ( 1.769862606763368706, 1.806619053477545700, -0.1335387089566111574 ) ) ;
#122111 = CARTESIAN_POINT ( 'NONE',  ( 3.188313505853744179, -1.798300186086329688, -0.3134973320952222364 ) ) ;
#122114 = CARTESIAN_POINT ( 'NONE',  ( 9.486581398170528701, -9.006862915010220405, -0.5116190538792210196 ) ) ;
#122115 = DIRECTION ( 'NONE',  ( 1.276756478318932585E-15, -1.000000000000000000, 1.665334536937738262E-16 ) ) ;
#122116 = CARTESIAN_POINT ( 'NONE',  ( 4.700333112842928429, -2.206180118464650786, -0.05804534286662357823 ) ) ;
#122117 = CARTESIAN_POINT ( 'NONE',  ( 7.096803341749390981, 10.36702210109460154, -1.199719254218441611 ) ) ;
#122118 = CARTESIAN_POINT ( 'NONE',  ( -1.402160292154681736E-14, 9.234375000341398021, 1.575800808251682339 ) ) ;
#122119 = CARTESIAN_POINT ( 'NONE',  ( 2.332540574144434053, 1.247770424613745543, -1.449200414897835687 ) ) ;
#122120 = CIRCLE ( 'NONE', #14858, 6.200000000000000178 ) ;
#122121 = CARTESIAN_POINT ( 'NONE',  ( 9.094822116668764167, 9.505047312402055582, 0.7998128361456462443 ) ) ;
#122122 = CARTESIAN_POINT ( 'NONE',  ( 6.637176860265922684, -0.09746846054551477900, -2.068182370504913159 ) ) ;
#122123 = CARTESIAN_POINT ( 'NONE',  ( -0.6801582343750438575, 0.6302083336747199560, -1.178068619123869398 ) ) ;
#122124 = CARTESIAN_POINT ( 'NONE',  ( 5.390230798962840630, -0.5317533105795355652, -2.125930911514521959 ) ) ;
#122125 = CARTESIAN_POINT ( 'NONE',  ( -5.204170427930421283E-15, 3.499999999999989342, -11.99999999999997868 ) ) ;
#122126 = DIRECTION ( 'NONE',  ( 0.000000000000000000, 0.000000000000000000, 1.000000000000000000 ) ) ;
#122127 = VERTEX_POINT ( 'NONE', #17311 ) ;
#122128 = ORIENTED_EDGE ( 'NONE', *, *, #205728, .T. ) ;
#122129 = CARTESIAN_POINT ( 'NONE',  ( 5.717785742877111055, 7.006476535625807855, -2.500000000000000000 ) ) ;
#122130 = CARTESIAN_POINT ( 'NONE',  ( 5.734172623936983904, 5.654565914206774124, 0.7998128361456352531 ) ) ;
#122131 = CARTESIAN_POINT ( 'NONE',  ( 1.642778471875000035, -2.063541666188710266, -2.845375778867859751 ) ) ;
#122132 = CARTESIAN_POINT ( 'NONE',  ( -11.94105721237523099, 13.40000000000000036, -1.187919463087249827 ) ) ;
#122133 = CARTESIAN_POINT ( 'NONE',  ( -7.619319141200077361, 9.912291636198670375, 1.443375672974090751 ) ) ;
#122134 = CARTESIAN_POINT ( 'NONE',  ( 4.760848217054122422, 5.583353003765119560, -1.199719254218452047 ) ) ;
#122135 = CARTESIAN_POINT ( 'NONE',  ( 5.752806990244247132, -0.4974732019265226679, -2.009498513695342936 ) ) ;
#122136 = CARTESIAN_POINT ( 'NONE',  ( 1.704704067347760699, 1.882482151684254923, 0.7231221989368596947 ) ) ;
#122137 = CARTESIAN_POINT ( 'NONE',  ( -9.215791728987058562, 11.77484298861683598, -1.599625672291263179 ) ) ;
#122138 = CARTESIAN_POINT ( 'NONE',  ( 4.934241560730721510, 4.721313007132757811, 0.000000000000000000 ) ) ;
#122139 = CARTESIAN_POINT ( 'NONE',  ( 1.570551226722196381, -2.081687204081467346, -0.6850663153453034893 ) ) ;
#122140 = CARTESIAN_POINT ( 'NONE',  ( 5.408770660633122063, 1.379882519126625295, -1.195542987486551301 ) ) ;
#122141 = CARTESIAN_POINT ( 'NONE',  ( -3.574546055497324737, 7.322054164722185732, 0.7998128361456341429 ) ) ;
#122142 = CARTESIAN_POINT ( 'NONE',  ( 5.397554552016216256, 7.390509292142662723, 1.443375672974065660 ) ) ;
#122143 = CARTESIAN_POINT ( 'NONE',  ( 8.224992744984721327, 12.74757530245756243, 1.040834085586084257E-14 ) ) ;
#122144 = CARTESIAN_POINT ( 'NONE',  ( -4.620296487206990932, 8.612372678375294299, 0.000000000000000000 ) ) ;
#122145 = CARTESIAN_POINT ( 'NONE',  ( 3.845709127770629010, 7.638411082374393146, 0.7998128361456321445 ) ) ;
#122146 = CARTESIAN_POINT ( 'NONE',  ( 3.230585741806197841, 6.991043475407723307, 0.7998128361456271485 ) ) ;
#122147 = ORIENTED_EDGE ( 'NONE', *, *, #160202, .T. ) ;
#122149 = CARTESIAN_POINT ( 'NONE',  ( 6.310797300923185915, -0.5409384057308598281, -1.939081195975641769 ) ) ;
#122148 = CARTESIAN_POINT ( 'NONE',  ( 2.823586671956069605, 1.020774559177588081, -1.532180179759069283 ) ) ;
#122150 = CARTESIAN_POINT ( 'NONE',  ( 2.038793776981039141, 2.199649879376049721, -0.6664975855598854748 ) ) ;
#122152 = CARTESIAN_POINT ( 'NONE',  ( 6.403176761927252159, -1.659045864033869666, 1.046607237317781269 ) ) ;
#122151 = CARTESIAN_POINT ( 'NONE',  ( 3.199361063144961825, 6.676412307070352270, -0.7216878364870267237 ) ) ;
#122153 = CARTESIAN_POINT ( 'NONE',  ( -4.543954038874438162, 8.453030145328826350, 1.040834085586084257E-14 ) ) ;
#122154 = CARTESIAN_POINT ( 'NONE',  ( 0.1833691866889655686, 7.629137130509075604, -2.653448492709729933 ) ) ;
#122155 = CARTESIAN_POINT ( 'NONE',  ( 3.920094060441734030, -1.906919942518231936, 0.1457910263855527466 ) ) ;
#122156 = CARTESIAN_POINT ( 'NONE',  ( -9.215791728987058562, 11.77484298861683598, -1.599625672291263179 ) ) ;
#122158 = ADVANCED_FACE ( 'NONE', ( #8275 ), #135369, .T. ) ;
#122157 = CARTESIAN_POINT ( 'NONE',  ( 0.2739938332866619364, -2.030697503880642518, 0.4024348779970430834 ) ) ;
#122159 = CARTESIAN_POINT ( 'NONE',  ( -7.485510208520816278, 8.866088343763324886, 1.082531754730549078 ) ) ;
#122161 = CARTESIAN_POINT ( 'NONE',  ( 1.199835987674138460, -1.870836310881810682, -0.003643258294119822160 ) ) ;
#122160 = CARTESIAN_POINT ( 'NONE',  ( 2.718400508848108466, 1.969533948853121386, 0.7019594197221010745 ) ) ;
#122162 = CARTESIAN_POINT ( 'NONE',  ( 1.880232294074701604, -0.2495702131940503166, 2.000550610736757218 ) ) ;
#122163 = CARTESIAN_POINT ( 'NONE',  ( 7.104109303880752790, 11.23195192126214970, -0.7216878364870267237 ) ) ;
#122164 = ORIENTED_EDGE ( 'NONE', *, *, #197691, .T. ) ;
#122165 = CARTESIAN_POINT ( 'NONE',  ( -1.201851678989727383E-14, 4.259375000341417028, -1.575800808251660134 ) ) ;
#122166 = CARTESIAN_POINT ( 'NONE',  ( 2.647703282711162398, 0.5884205719196273776, 1.638072370343154116 ) ) ;
#122167 = PRESENTATION_LAYER_ASSIGNMENT (  '', '', ( #59920 ) ) ;
#122168 = CARTESIAN_POINT ( 'NONE',  ( 5.495132332240461714, 5.305409230568988832, 0.7998128361456341429 ) ) ;
#122170 = CARTESIAN_POINT ( 'NONE',  ( 0.4770138163741251547, 3.005786281947454786, -1.942556692846756361 ) ) ;
#122169 = FILL_AREA_STYLE_COLOUR ( '', #179436 ) ;
#122171 = CARTESIAN_POINT ( 'NONE',  ( 2.754212737529265986, 0.5811417601193774596, 1.624163882408189652 ) ) ;
#122172 = CARTESIAN_POINT ( 'NONE',  ( 3.193114300108112147, 1.729001323093733111, 1.346577201094656395 ) ) ;
#122173 = CARTESIAN_POINT ( 'NONE',  ( 5.285833163787800437, 1.479997892162682849, 1.637210856327932618 ) ) ;
#122174 = CARTESIAN_POINT ( 'NONE',  ( -10.14891672641957499, 5.000029895416906456, -7.601366607803407227 ) ) ;
#122175 = FILL_AREA_STYLE ('',( #115732 ) ) ;
#122176 = CARTESIAN_POINT ( 'NONE',  ( 3.309609623814670165, -1.772202297075220256, -1.253863066769088874 ) ) ;
#122177 = CARTESIAN_POINT ( 'NONE',  ( 2.314841291766779108, 1.630546960418734148, 0.8213866120303781049 ) ) ;
#122178 = CARTESIAN_POINT ( 'NONE',  ( 0.7500000000000006661, 12.33333333333333570, 1.299038105676657340 ) ) ;
#122179 = CARTESIAN_POINT ( 'NONE',  ( 4.136029606254186142, 2.116781002543933088, -0.05581379417103624063 ) ) ;
#122180 = CARTESIAN_POINT ( 'NONE',  ( 6.539320575229245591, 2.459069921018588900, 2.280790101157427419 ) ) ;
#122181 = ORIENTED_EDGE ( 'NONE', *, *, #73605, .T. ) ;
#122183 = CARTESIAN_POINT ( 'NONE',  ( -1.364683531250012516, 2.551041667008089320, -0.7879004041258289570 ) ) ;
#122182 = CARTESIAN_POINT ( 'NONE',  ( 4.950848118218736715, -1.935628577297190400, -1.227853487085520001 ) ) ;
#122184 = DIRECTION ( 'NONE',  ( 0.05872483221476459958, 0.000000000000000000, 0.9982742078614211811 ) ) ;
#122185 = CARTESIAN_POINT ( 'NONE',  ( 10.53876547652418338, 11.18964789890005918, 0.7998128361456462443 ) ) ;
#122186 = CARTESIAN_POINT ( 'NONE',  ( -0.1104750535120025967, -0.004616138082884357029, -2.103378236956429337 ) ) ;
#122187 = CARTESIAN_POINT ( 'NONE',  ( -4.758548728716557541, 8.495464583570553785, 1.040834085586084257E-14 ) ) ;
#122188 = CARTESIAN_POINT ( 'NONE',  ( 3.958617665510264949, 5.641473247893851628, -1.443375672974051449 ) ) ;
#122189 =( GEOMETRIC_REPRESENTATION_CONTEXT ( 3 ) GLOBAL_UNCERTAINTY_ASSIGNED_CONTEXT ( ( #25927 ) ) GLOBAL_UNIT_ASSIGNED_CONTEXT ( ( #94783, #95855, #12423 ) ) REPRESENTATION_CONTEXT ( 'NONE', 'WORKASPACE' ) );
#122190 = CARTESIAN_POINT ( 'NONE',  ( -4.894130264408862452, 7.693273827576896373, -1.082531754730548412 ) ) ;
#122191 =( GEOMETRIC_REPRESENTATION_CONTEXT ( 3 ) GLOBAL_UNCERTAINTY_ASSIGNED_CONTEXT ( ( #148541 ) ) GLOBAL_UNIT_ASSIGNED_CONTEXT ( ( #53701, #152271, #7053 ) ) REPRESENTATION_CONTEXT ( 'NONE', 'WORKASPACE' ) );
#122192 = EDGE_CURVE ( 'NONE', #73686, #77536, #57298, .T. ) ;
#122193 = CARTESIAN_POINT ( 'NONE',  ( 6.883263157960391787, 1.253787318140922480, 2.167784446185747171 ) ) ;
#122194 = ORIENTED_EDGE ( 'NONE', *, *, #134348, .F. ) ;
#122195 = CARTESIAN_POINT ( 'NONE',  ( 5.274064633610318076, 1.777012466945230962, -0.9530095070046653571 ) ) ;
#122197 = CARTESIAN_POINT ( 'NONE',  ( 3.608308625203029862, 2.062741128266020851, 0.004805803398660184710 ) ) ;
#122196 = CARTESIAN_POINT ( 'NONE',  ( 3.825371897350130723, 7.614684313550482031, 0.7998128361456321445 ) ) ;
#122199 = CARTESIAN_POINT ( 'NONE',  ( 6.883263157960371359, 7.052674735402435502, 2.544342468817725855 ) ) ;
#122198 = CARTESIAN_POINT ( 'NONE',  ( 5.671053392266061977, 9.838255734277600695, 0.7998128361456331437 ) ) ;
#122200 = CARTESIAN_POINT ( 'NONE',  ( 6.444921918449731280, 8.612437886315108315, 1.599625672291268286 ) ) ;
#122201 = CARTESIAN_POINT ( 'NONE',  ( 3.285556943750000070, -1.684374999522043836, 0.000000000000000000 ) ) ;
#122202 = CYLINDRICAL_SURFACE ( 'NONE', #213166, 0.4000000000000010214 ) ;
#122203 = CARTESIAN_POINT ( 'NONE',  ( 6.509741685903361663, -1.029359178063901092, -1.934661654277470166 ) ) ;
#122204 = CARTESIAN_POINT ( 'NONE',  ( 3.621720349255663773, 0.2986264320336135536, 1.994071497604548382 ) ) ;
#122205 = CARTESIAN_POINT ( 'NONE',  ( 3.597050949361340511, -0.5310884314010614338, 1.763007376093472800 ) ) ;
#122206 = CARTESIAN_POINT ( 'NONE',  ( 6.830610463186557624, 6.863467050006115677, 1.040834085586084257E-14 ) ) ;
#122207 = CARTESIAN_POINT ( 'NONE',  ( 0.2699429432127123385, -1.132711312255540115, 1.300796998575669772 ) ) ;
#122208 = AXIS2_PLACEMENT_3D ( 'NONE', #139265, #207440, #124159 ) ;
#122209 = FACE_OUTER_BOUND ( 'NONE', #213508, .T. ) ;
#122210 = CARTESIAN_POINT ( 'NONE',  ( 1.389710824352110574, -0.8328434156393785814, -2.142668459815112669 ) ) ;
#122211 = CARTESIAN_POINT ( 'NONE',  ( -7.335124800193271177, 8.516399340768996851, -1.199719254218452935 ) ) ;
#122212 = CARTESIAN_POINT ( 'NONE',  ( 6.737213295527981316, -2.024711933681651477, 1.009942563148768846 ) ) ;
#122213 = CARTESIAN_POINT ( 'NONE',  ( 2.244876548131835126, 0.4624279887704956238, 2.054504457251419502 ) ) ;
#122214 = CARTESIAN_POINT ( 'NONE',  ( -6.180537922983287302, 8.303989891604203422, -1.599625672291271394 ) ) ;
#122215 = CARTESIAN_POINT ( 'NONE',  ( 6.428537391173986038, 10.65171072301167854, 0.7998128361456462443 ) ) ;
#122216 = CARTESIAN_POINT ( 'NONE',  ( 5.763624699140868834, 7.817591130454727200, -1.443375672974078761 ) ) ;
#122217 =( LENGTH_UNIT ( ) NAMED_UNIT ( * ) SI_UNIT ( .MILLI., .METRE. ) );
#122218 = CARTESIAN_POINT ( 'NONE',  ( -7.400052914960538963, 7.527816577075747695, 1.040834085586084257E-14 ) ) ;
#122219 = CARTESIAN_POINT ( 'NONE',  ( 5.138177029454829459, 8.938364267765221527, 0.7216878364870438212 ) ) ;
#122220 = CARTESIAN_POINT ( 'NONE',  ( 4.197832665289490173, 7.575126408543901846, 0.9117821302269245587 ) ) ;
#122221 =( GEOMETRIC_REPRESENTATION_CONTEXT ( 3 ) GLOBAL_UNCERTAINTY_ASSIGNED_CONTEXT ( ( #132872 ) ) GLOBAL_UNIT_ASSIGNED_CONTEXT ( ( #140026, #21939, #123843 ) ) REPRESENTATION_CONTEXT ( 'NONE', 'WORKASPACE' ) );
#122222 = CARTESIAN_POINT ( 'NONE',  ( -5.111587607552082524, 5.922272616020886282, 1.199719254218450271 ) ) ;
#122223 = CARTESIAN_POINT ( 'NONE',  ( 3.621504738650199950, 1.906737781736141280, 1.139490138724685853 ) ) ;
#122224 = CARTESIAN_POINT ( 'NONE',  ( 2.343918204863020271, 2.190988169473460090, 0.05230688499441307066 ) ) ;
#122225 = CARTESIAN_POINT ( 'NONE',  ( -6.196239896645333367, 7.187700286629718605, -1.199719254218446718 ) ) ;
#122226 = CARTESIAN_POINT ( 'NONE',  ( 6.883263157960398892, 2.970623603138923929, 2.399364662246627589 ) ) ;
#122227 = CARTESIAN_POINT ( 'NONE',  ( -4.984557751679625781, 5.844347460828191565, 1.199719254218452935 ) ) ;
#122228 = CARTESIAN_POINT ( 'NONE',  ( 5.986763597034562068, 1.890319730748804439, 0.5246630281777532323 ) ) ;
#122229 = CARTESIAN_POINT ( 'NONE',  ( -1.324925973730976203, 1.296446089449585948, 1.500000000000001998 ) ) ;
#122230 = CARTESIAN_POINT ( 'NONE',  ( 0.6823417656249899377, 2.342708333674753618, 1.181850606188767472 ) ) ;
#122231 = CARTESIAN_POINT ( 'NONE',  ( 6.610000000000026965, 7.052677709320480659, 2.598153670447616470 ) ) ;
#122233 = ORIENTED_EDGE ( 'NONE', *, *, #210306, .T. ) ;
#122232 = CARTESIAN_POINT ( 'NONE',  ( -7.049876689426121779, 7.327203680526343632, -0.7216878364870278340 ) ) ;
#122234 = CARTESIAN_POINT ( 'NONE',  ( 4.992489932941452935, -1.175987964647656536, 1.764448611491518548 ) ) ;
#122235 = CARTESIAN_POINT ( 'NONE',  ( -3.959863383643135393, 6.777535159962392086, 1.199719254218452935 ) ) ;
#122236 = ORIENTED_EDGE ( 'NONE', *, *, #54770, .F. ) ;
#122237 = CARTESIAN_POINT ( 'NONE',  ( 5.946190753372003535, 2.158995856162956084, 0.1107517376499680406 ) ) ;
#122238 = CARTESIAN_POINT ( 'NONE',  ( 4.821896187954575197, 8.777295985922343391, 0.7998128361456462443 ) ) ;
#122239 = CARTESIAN_POINT ( 'NONE',  ( 5.038538826285253514, -1.576363729006284187, 0.9512496309353534185 ) ) ;
#122240 = UNCERTAINTY_MEASURE_WITH_UNIT (LENGTH_MEASURE( 1.000000000000000082E-05 ), #116833, 'distance_accuracy_value', 'NONE');
#122241 = CARTESIAN_POINT ( 'NONE',  ( -5.892944143475336460, 6.011535633345318708, 0.2346759862181871381 ) ) ;
#122242 = CARTESIAN_POINT ( 'NONE',  ( 0.6823417656249899377, 1.905208333674752952, 1.181850606188755259 ) ) ;
#122243 = CARTESIAN_POINT ( 'NONE',  ( 0.3447215323711784740, 0.5487897507440896439, -1.651745661738156734 ) ) ;
#122244 = CARTESIAN_POINT ( 'NONE',  ( 6.827182134110222123, 7.629137130509070275, 2.410944104600701188 ) ) ;
#122245 = CARTESIAN_POINT ( 'NONE',  ( 11.80247861663003484, 13.79999999999999716, -1.695431928471867966 ) ) ;
#122246 = CARTESIAN_POINT ( 'NONE',  ( 4.065412822539622439, 0.2671453805177248508, -2.145074402785766665 ) ) ;
#122247 = CARTESIAN_POINT ( 'NONE',  ( -3.249150368769345043, 6.942425863539538611, 0.7998128361456341429 ) ) ;
#122248 = CARTESIAN_POINT ( 'NONE',  ( -8.310784975052685652, 9.758632561392040827, -1.082531754730543083 ) ) ;
#122249 = CARTESIAN_POINT ( 'NONE',  ( 3.432649856329002880, 2.108609624295390006, 0.4754391814798044069 ) ) ;
#122250 = CARTESIAN_POINT ( 'NONE',  ( 4.393795938483449071, -0.7573388051436024115, 1.820269059793070410 ) ) ;
#122251 = CARTESIAN_POINT ( 'NONE',  ( 3.954193900006929052, 1.254965027507263464, 1.196595854207074261 ) ) ;
#122252 = CARTESIAN_POINT ( 'NONE',  ( 1.224469250947546328, 2.113408192816915943, 0.5798510048089372537 ) ) ;
#122253 = CARTESIAN_POINT ( 'NONE',  ( 0.6754003219355340093, -2.174137316696134636, -0.7736760779102586083 ) ) ;
#122254 = CARTESIAN_POINT ( 'NONE',  ( 4.059881558241601240, 2.045671965140416937, -0.2483333800566180083 ) ) ;
#122255 = CARTESIAN_POINT ( 'NONE',  ( 5.952673665805181535, -1.667821083538678861, -0.9947414763863350329 ) ) ;
#122256 = CARTESIAN_POINT ( 'NONE',  ( -8.798878505144665851, 9.367705798864669475, -0.7216878364870267237 ) ) ;
#122257 = B_SPLINE_CURVE_WITH_KNOTS ( 'NONE', 3,
 ( #53244, #118306, #119374, #34842, #185361, #54315, #103066, #169122, #170182, #86810, #152876, #116172, #84675, #4454, #70524, #33788, #1265, #136641, #67324, #133468, #199471, #51113 ),
 .UNSPECIFIED., .F., .F.,
 ( 4, 2, 2, 2, 2, 2, 2, 2, 2, 2, 4 ),
 ( -5.999999999670954957E-08, 0.0006677484337924339576, 0.001335556867584864740, 0.002671173735169722618, 0.004006790602754580280, 0.005342407470339437942, 0.006678024337924295603, 0.008013641205509153265, 0.009349258073094010926, 0.01001706650688643715, 0.01068487494067886685 ),
 .UNSPECIFIED. ) ;
#122258 = CARTESIAN_POINT ( 'NONE',  ( -6.330731382938325602, 6.350551133041632212, 0.7998128361456281477 ) ) ;
#122259 = DIRECTION ( 'NONE',  ( 0.000000000000000000, 1.000000000000000000, 0.000000000000000000 ) ) ;
#122261 = ORIENTED_EDGE ( 'NONE', *, *, #24409, .T. ) ;
#122260 = CARTESIAN_POINT ( 'NONE',  ( 0.3869524901765013514, 1.970899860167981910, -11.77270853017065200 ) ) ;
#122262 = CARTESIAN_POINT ( 'NONE',  ( -8.161645285302366659, 8.624267042381978499, 1.040834085586084257E-14 ) ) ;
#122263 = CARTESIAN_POINT ( 'NONE',  ( 3.733602637680955461, -2.039903990487580643, 0.8422819887162477093 ) ) ;
#122264 = CARTESIAN_POINT ( 'NONE',  ( 1.642778471875000035, -0.2260416661887081069, -2.845375778867859751 ) ) ;
#122265 = ORIENTED_EDGE ( 'NONE', *, *, #93378, .T. ) ;
#122266 = CARTESIAN_POINT ( 'NONE',  ( 0.2857036466711966316, -1.138303949996006148, -1.472634861895638636 ) ) ;
#122267 =( BOUNDED_SURFACE ( )  B_SPLINE_SURFACE ( 3, 2, ( 
 ( #186468, #7710, #38103 ),
 ( #56485, #19702, #20753 ),
 ( #85781, #103102, #169160 ),
 ( #86848, #4491, #21808 ) ),
 .UNSPECIFIED., .F., .F., .T. ) 
 B_SPLINE_SURFACE_WITH_KNOTS ( ( 4, 4 ),
 ( 3, 3 ),
 ( 0.01133669335851669041, 0.01377857026255017818 ),
 ( 0.000000000000000000, 1.000000000000000000 ),
 .UNSPECIFIED. ) 
 GEOMETRIC_REPRESENTATION_ITEM ( )  RATIONAL_B_SPLINE_SURFACE ( (
 ( 1.000000000000000000, 0.7169883299103929630, 1.000000000000000000),
 ( 1.000000000000000000, 0.7174882367753923074, 1.000000000000000000),
 ( 1.000000000000000000, 0.7180609655871061925, 1.000000000000000000),
 ( 1.000000000000000000, 0.7187540731122933346, 1.000000000000000000) ) ) 
 REPRESENTATION_ITEM ( '' )  SURFACE ( )  );
#122268 = CARTESIAN_POINT ( 'NONE',  ( -0.1291982275798781443, -0.004298614154785855221, -2.073875112923003083 ) ) ;
#122269 = CARTESIAN_POINT ( 'NONE',  ( -1.500000000000011324, 5.160416667349487341, -0.8660254037844313801 ) ) ;
#122271 = CARTESIAN_POINT ( 'NONE',  ( -4.983945206004156248, 6.510271170337021296, -1.264942728826349949 ) ) ;
#122270 = CYLINDRICAL_SURFACE ( 'NONE', #111231, 1.250000000000000000 ) ;
#122272 = CARTESIAN_POINT ( 'NONE',  ( 6.714805130922314014, -0.1276373473727103192, 1.811824464382847832 ) ) ;
#122273 = ORIENTED_EDGE ( 'NONE', *, *, #153089, .T. ) ;
#122274 = CARTESIAN_POINT ( 'NONE',  ( 1.903268112024224523, 1.712809940758196259, 1.145777703309367457 ) ) ;
#122275 = CARTESIAN_POINT ( 'NONE',  ( 1.360316468749983576, 0.5156250003414062366, -5.204170427930421283E-15 ) ) ;
#122276 = CARTESIAN_POINT ( 'NONE',  ( -6.449928391799210736, 8.548002428564306143, -1.599625672291263179 ) ) ;
#122277 = CARTESIAN_POINT ( 'NONE',  ( 10.91877977293360047, -9.985078020775006280, -0.1443118549625480029 ) ) ;
#122278 = SURFACE_SIDE_STYLE ('',( #136313 ) ) ;
#122279 = CARTESIAN_POINT ( 'NONE',  ( 5.495132332240461714, 5.305409230568988832, 0.7998128361456341429 ) ) ;
#122280 = CARTESIAN_POINT ( 'NONE',  ( 0.4970371946629085769, 1.713755840317375601, -1.144362063176207922 ) ) ;
#122282 = CARTESIAN_POINT ( 'NONE',  ( 5.161589042655139181, 0.9124512986629171873, 1.599201395118980740 ) ) ;
#122281 = CARTESIAN_POINT ( 'NONE',  ( -3.096514578442687515, 6.188910745953249304, -0.7944190528704382359 ) ) ;
#122283 = CARTESIAN_POINT ( 'NONE',  ( 5.524057522564145728, 8.532151978711786100, 1.199719254218462483 ) ) ;
#122284 = CARTESIAN_POINT ( 'NONE',  ( -4.308458954092677651, 8.248562223075252220, -0.7998128361456362523 ) ) ;
#122285 = CARTESIAN_POINT ( 'NONE',  ( 6.966220764712121927, 6.002124920821316323, 2.500000000000000444 ) ) ;
#122286 = TOROIDAL_SURFACE ( 'NONE', #11474, 11.92000000000000171, 0.08000000000000000167 ) ;
#122287 = CARTESIAN_POINT ( 'NONE',  ( 4.406973378220558679, 1.706932345810768359, -1.398813476408675260 ) ) ;
#122288 = CARTESIAN_POINT ( 'NONE',  ( 0.5269342146079664113, 2.068330297753611546, 0.6279826202375409228 ) ) ;
#122289 = CARTESIAN_POINT ( 'NONE',  ( -5.287316719649550301, 5.270883715786984780, 0.7216878364870317197 ) ) ;
#122290 = CARTESIAN_POINT ( 'NONE',  ( 6.469024005207689498, -1.393930998056407189, 1.156871781951673395 ) ) ;
#122291 = CARTESIAN_POINT ( 'NONE',  ( 1.147673126774436225, 1.985868168208399842, -0.3494872464938902357 ) ) ;
#122292 = CARTESIAN_POINT ( 'NONE',  ( 0.000000000000000000, 13.49999999999999822, 0.000000000000000000 ) ) ;
#122293 = CARTESIAN_POINT ( 'NONE',  ( 1.687308557152231270, -1.277188091954140514, -1.910694296540839332 ) ) ;
#122294 = EDGE_CURVE ( 'NONE', #40830, #197229, #73449, .T. ) ;
#122295 = DIRECTION ( 'NONE',  ( 0.000000000000000000, 1.000000000000000000, 0.000000000000000000 ) ) ;
#122296 = CARTESIAN_POINT ( 'NONE',  ( 0.000000000000000000, 11.37999999999998302, 0.000000000000000000 ) ) ;
#122297 = LINE ( 'NONE', #172024, #192296 ) ;
#122298 = CARTESIAN_POINT ( 'NONE',  ( 1.375632740723360836, 1.111493989511678881, 1.504490780774490499 ) ) ;
#122299 = CARTESIAN_POINT ( 'NONE',  ( 2.342982756445275427, -1.756855002775299379, -0.9896843009072553432 ) ) ;
#122301 = CARTESIAN_POINT ( 'NONE',  ( 11.33772467203841572, 13.50732847981847939, 3.599999999999999201 ) ) ;
#122300 = CARTESIAN_POINT ( 'NONE',  ( 1.364683531249988757, 0.3843750003414206362, 0.000000000000000000 ) ) ;
#122303 = CARTESIAN_POINT ( 'NONE',  ( 5.250649905694958264, 0.6104557620976447385, 2.015647016877469166 ) ) ;
#122302 = CARTESIAN_POINT ( 'NONE',  ( -7.018317073368468328, 11.33978701890523233, -0.7998128361456291469 ) ) ;
#122304 = CARTESIAN_POINT ( 'NONE',  ( 6.909851844459134362, 11.21324425184434936, -0.7998128361456291469 ) ) ;
#122306 = CARTESIAN_POINT ( 'NONE',  ( -7.178152263431422320, 10.46192917639026554, 1.199719254218453823 ) ) ;
#122305 = CARTESIAN_POINT ( 'NONE',  ( 6.073126464278658432, 6.050012061272033392, 0.000000000000000000 ) ) ;
#122307 = SURFACE_SIDE_STYLE ('',( #123375 ) ) ;
#122308 = CARTESIAN_POINT ( 'NONE',  ( 4.008073073761713623, -0.7691326184188684856, 1.867817587601346307 ) ) ;
#122309 = CARTESIAN_POINT ( 'NONE',  ( -1.364683531250012516, 4.738541667008091096, -0.7879004041258300672 ) ) ;
#122310 = EDGE_CURVE ( 'NONE', #145502, #188383, #6301, .T. ) ;
#122311 = CARTESIAN_POINT ( 'NONE',  ( 6.619587925713169341, 0.3565228922877783924, -2.031493691534612012 ) ) ;
#122312 = CARTESIAN_POINT ( 'NONE',  ( 8.080296364064698977, 12.37083682481011060, -0.7216878364870328300 ) ) ;
#122313 = CARTESIAN_POINT ( 'NONE',  ( 4.024825912876791811, 2.051136489140188424, 0.6822911077620784637 ) ) ;
#122314 = CARTESIAN_POINT ( 'NONE',  ( 6.363572996767764778, 8.517530811019446091, -1.599625672291283607 ) ) ;
#122315 = CARTESIAN_POINT ( 'NONE',  ( -1.402160292154681736E-14, -0.3656249996585805295, 1.575800808251672791 ) ) ;
#122317 = CARTESIAN_POINT ( 'NONE',  ( -7.949604103952364831, -6.836271202499947464, 7.404765023120916112 ) ) ;
#122316 = CARTESIAN_POINT ( 'NONE',  ( 6.703580607314123085, 6.785541894813420072, 0.000000000000000000 ) ) ;
#122318 = CARTESIAN_POINT ( 'NONE',  ( 7.917598520256366790, 8.339545816494993602, 1.040834085586084257E-14 ) ) ;
#122320 = CARTESIAN_POINT ( 'NONE',  ( 1.608462485350599769, 8.735270501766756013, 2.463594439587641904 ) ) ;
#122319 = CARTESIAN_POINT ( 'NONE',  ( 2.330757530436095237, -1.336968151498512336, 1.710609410560095522 ) ) ;
#122322 = CARTESIAN_POINT ( 'NONE',  ( 1.382094229771430705, -0.2707140722739818650, -1.821126350552772610 ) ) ;
#122321 = CARTESIAN_POINT ( 'NONE',  ( -4.772106882330227506, 7.550913215151819458, -1.082531754730549967 ) ) ;
#122323 = CARTESIAN_POINT ( 'NONE',  ( -0.6823417656250212460, 3.801041667008085767, 1.181850606188767472 ) ) ;
#122324 = CARTESIAN_POINT ( 'NONE',  ( 3.175498511859841333, 1.392037702009111033, 1.692654053968026151 ) ) ;
#122325 = CARTESIAN_POINT ( 'NONE',  ( 6.983263157960365675, 7.629137130509066722, 2.553810918356711479 ) ) ;
#122326 = CARTESIAN_POINT ( 'NONE',  ( 3.590934319571597033, -0.4389823211032486960, -2.219365549907009960 ) ) ;
#122327 = CARTESIAN_POINT ( 'NONE',  ( -6.718228810771495141, 7.796687353110217877, 1.199719254218450271 ) ) ;
#122328 = DIRECTION ( 'NONE',  ( 0.000000000000000000, -0.000000000000000000, 1.000000000000000000 ) ) ;
#122329 = CARTESIAN_POINT ( 'NONE',  ( 6.365646016822680942, 6.829858545691475769, 0.5939985411197836740 ) ) ;
#122330 = CARTESIAN_POINT ( 'NONE',  ( -6.009258394948636914E-15, 13.18749999999999822, -1.732050807568875195 ) ) ;
#122331 = CARTESIAN_POINT ( 'NONE',  ( 4.584065335196252811, 8.362176967788721882, 0.7216878364870328300 ) ) ;
#122332 = CARTESIAN_POINT ( 'NONE',  ( 5.536323748068817885, 1.743679661707888018, 0.3015777700523143978 ) ) ;
#122333 = CARTESIAN_POINT ( 'NONE',  ( 3.492840887459470522, -1.940756296261561209, -0.5346130827820451126 ) ) ;
#122334 = CARTESIAN_POINT ( 'NONE',  ( 8.178592977541601527, 10.56477777859713463, 1.599625672291281386 ) ) ;
#122335 = CARTESIAN_POINT ( 'NONE',  ( 2.081218647941612154, -0.1023907900198107734, -2.103586654547675128 ) ) ;
#122337 = ADVANCED_FACE ( 'NONE', ( #174925 ), #212977, .T. ) ;
#122336 = CARTESIAN_POINT ( 'NONE',  ( 1.364683531249996529, 10.96354166700806942, 0.7879004041258405033 ) ) ;
#122338 = CARTESIAN_POINT ( 'NONE',  ( 1.047236342219150407, 1.738656489303032737, -0.9252727719080054980 ) ) ;
#122339 = CARTESIAN_POINT ( 'NONE',  ( -4.228163802615396705, 6.026220084508304708, -1.599625672291271394 ) ) ;
#122340 = CARTESIAN_POINT ( 'NONE',  ( 3.611473365557979598, 7.348452737196720541, -0.2779858853791586926 ) ) ;
#122342 = ORIENTED_EDGE ( 'NONE', *, *, #148379, .T. ) ;
#122341 = CARTESIAN_POINT ( 'NONE',  ( 6.117428737855862941, 1.511353622793030427, 0.9985130155200862001 ) ) ;
#122343 = CARTESIAN_POINT ( 'NONE',  ( 5.477130870240836558, 9.333810415348903433, -0.7216878364870267237 ) ) ;
#122344 = CARTESIAN_POINT ( 'NONE',  ( 1.364683531249986537, -0.3239583329919163424, 0.7879004041258500513 ) ) ;
#122345 = CARTESIAN_POINT ( 'NONE',  ( 5.207814216083940018, -1.861544245658670604, 0.1842191830812093256 ) ) ;
#122346 = AXIS2_PLACEMENT_3D ( 'NONE', #45782, #31653, #146486 ) ;
#122347 = CARTESIAN_POINT ( 'NONE',  ( 5.717656431054087385, 0.4094431674900833040, -2.029196096928844284 ) ) ;
#122348 = AXIS2_PLACEMENT_3D ( 'NONE', #124831, #188679, #26168 ) ;
#122349 = CARTESIAN_POINT ( 'NONE',  ( -5.157946788997579689E-14, 2.437500000000003553, -1.414508159514605401 ) ) ;
#122350 = CARTESIAN_POINT ( 'NONE',  ( -4.624739795592936353, 7.449261290616792763, -1.082531754730549967 ) ) ;
#122351 = CARTESIAN_POINT ( 'NONE',  ( 7.670162217029129259, 9.971608557999250166, 1.599625672291281386 ) ) ;
#122352 = CARTESIAN_POINT ( 'NONE',  ( -9.016335848287868160, 10.47781223021269170, 1.199719254218462483 ) ) ;
#122353 = CARTESIAN_POINT ( 'NONE',  ( 7.289443866002793371, 8.533381260871966134, 1.199719254218452047 ) ) ;
#122354 = EDGE_CURVE ( 'NONE', #136413, #11785, #106169, .T. ) ;
#122355 = DIRECTION ( 'NONE',  ( 0.000000000000000000, 1.000000000000000000, 0.000000000000000000 ) ) ;
#122356 = CARTESIAN_POINT ( 'NONE',  ( -1.364683531250014514, -0.2197916663252438285, 0.7879004041258379498 ) ) ;
#122357 = CARTESIAN_POINT ( 'NONE',  ( -1.500000000000013101, 1.670833333333355153, 0.8660254037844403729 ) ) ;
#122359 = CARTESIAN_POINT ( 'NONE',  ( 3.988069740714122791, 7.804498464141805592, 0.7998128361456321445 ) ) ;
#122358 = CARTESIAN_POINT ( 'NONE',  ( 4.914483161888778540, 0.7490505147796695518, 1.813437088826752142 ) ) ;
#122360 = CARTESIAN_POINT ( 'NONE',  ( 2.214220036344019871, -1.617569417291262690, -1.203170845901546215 ) ) ;
#122361 = CARTESIAN_POINT ( 'NONE',  ( 11.55950211276791251, 13.88000000000000078, -3.221476510067114329 ) ) ;
#122362 = CIRCLE ( 'NONE', #153346, 9.523431457505068920 ) ;
#122363 = CARTESIAN_POINT ( 'NONE',  ( 0.9783777488623355278, -2.139296967303818686, -0.4750931833387496694 ) ) ;
#122364 = PRESENTATION_STYLE_ASSIGNMENT (( #23684 ) ) ;
#122365 = CARTESIAN_POINT ( 'NONE',  ( 1.774454573425466863, -1.774572579973210384, -0.5916213571805841731 ) ) ;
#122366 = CARTESIAN_POINT ( 'NONE',  ( -1.001543065824772872E-14, 5.071875000341421469, 1.575800808251672791 ) ) ;
#122367 = CARTESIAN_POINT ( 'NONE',  ( 4.201435496602879738, 1.796340046740346086, -0.9091319694144882613 ) ) ;
#122368 = CARTESIAN_POINT ( 'NONE',  ( -7.645908563102897126, 11.00764485934031889, 1.199719254218453823 ) ) ;
#122370 = CARTESIAN_POINT ( 'NONE',  ( 3.779011003814860548, 1.787463462570267447, -1.134484337778138174 ) ) ;
#122369 = CARTESIAN_POINT ( 'NONE',  ( -5.341549334104202629, 7.254893527920112994, 1.443375672974064550 ) ) ;
#122371 = DIRECTION ( 'NONE',  ( 0.000000000000000000, 1.000000000000000000, 0.000000000000000000 ) ) ;
#122372 = CARTESIAN_POINT ( 'NONE',  ( 4.773920332862017446, -2.031068740936771366, 0.4005940302675218834 ) ) ;
#122373 = CARTESIAN_POINT ( 'NONE',  ( 7.028976294042106332, 7.165170195996068969, 0.000000000000000000 ) ) ;
#122375 = CARTESIAN_POINT ( 'NONE',  ( 6.720655732516647163, -0.004400176169771369272, 2.173773060281408931 ) ) ;
#122374 = CARTESIAN_POINT ( 'NONE',  ( 1.681308932615958041, 1.444198878393717411, 1.512019500502481018 ) ) ;
#122377 = ORIENTED_EDGE ( 'NONE', *, *, #197814, .F. ) ;
#122376 = CARTESIAN_POINT ( 'NONE',  ( 6.159193757800505153, -1.567253032978152660, -0.9359774744091067245 ) ) ;
#122378 = CARTESIAN_POINT ( 'NONE',  ( 7.613066949273408213, 8.840665181362512115, -1.199719254218441611 ) ) ;
#122379 = CARTESIAN_POINT ( 'NONE',  ( -6.078132937628113908, 5.985576603521232109, 1.040834085586084257E-14 ) ) ;
#122380 = CARTESIAN_POINT ( 'NONE',  ( 5.327714171786221975, 6.335452698179637743, -1.103974704194911283 ) ) ;
#122381 = CARTESIAN_POINT ( 'NONE',  ( -9.811677024507259759, 4.107325997343203028, 6.339424533126782002 ) ) ;
#122382 = CARTESIAN_POINT ( 'NONE',  ( 6.249945625775433555, 10.23542763013927726, -0.7216878364870267237 ) ) ;
#122383 = CARTESIAN_POINT ( 'NONE',  ( -1.913843809498108950, 3.268536626279731738, 0.4294081188992993070 ) ) ;
#122384 = CARTESIAN_POINT ( 'NONE',  ( 5.865855438783555087, 0.5507134639845879809, -1.831277125143706552 ) ) ;
#122385 = CARTESIAN_POINT ( 'NONE',  ( -8.857554428429624593, 9.228235009456373206, 0.7998128361456462443 ) ) ;
#122386 = CARTESIAN_POINT ( 'NONE',  ( 6.356075086708249167, 6.309842444114747373, -0.7998128361456281477 ) ) ;
#122387 = CARTESIAN_POINT ( 'NONE',  ( -9.479415819240319507, -6.570271182191716797, 0.2417854191286431531 ) ) ;
#122388 = FACE_BOUND ( 'NONE', #171565, .T. ) ;
#122389 = CARTESIAN_POINT ( 'NONE',  ( 4.857899112398166075, 4.561970474086296079, 1.040834085586084257E-14 ) ) ;
#122390 = VERTEX_POINT ( 'NONE', #39559 ) ;
#122391 = CARTESIAN_POINT ( 'NONE',  ( 6.433220217788329087, -1.621194592471734364, -1.198847091081943539 ) ) ;
#122392 = CARTESIAN_POINT ( 'NONE',  ( 3.231779075379113131, 6.036511184309971689, 0.9899555337401855226 ) ) ;
#122393 = CARTESIAN_POINT ( 'NONE',  ( -3.001735798205259265, 6.389591682482198109, -0.7455002297410243672 ) ) ;
#122394 = CARTESIAN_POINT ( 'NONE',  ( 0.1394461523057474728, 0.7845381482947767493, -1.808261586923729736 ) ) ;
#122395 = CARTESIAN_POINT ( 'NONE',  ( -4.772106882330234612, 6.590544000850479200, -1.443375672974053447 ) ) ;
#122396 = CARTESIAN_POINT ( 'NONE',  ( 2.683624340501134853, 5.218313266304903664, -1.199719254218446718 ) ) ;
#122397 = CARTESIAN_POINT ( 'NONE',  ( 4.030098220014290078, 1.090402053431119622, 1.639822181875214557 ) ) ;
#122398 = CARTESIAN_POINT ( 'NONE',  ( 4.517203946846011675, -1.842441744247227842, 0.8197884948388589610 ) ) ;
#122399 = CARTESIAN_POINT ( 'NONE',  ( -5.181187258716735577, 9.196468901811520880, 0.7998128361456481317 ) ) ;
#122400 = CARTESIAN_POINT ( 'NONE',  ( 1.469576158976824144E-15, 18.91999999999999815, 12.00000000000000178 ) ) ;
#122401 = CARTESIAN_POINT ( 'NONE',  ( 4.418054252288761141, 1.349281245414082342, -1.726737887558588591 ) ) ;
#122402 = CARTESIAN_POINT ( 'NONE',  ( 0.000000000000000000, -0.2000000000000057288, 0.000000000000000000 ) ) ;
#122403 = CARTESIAN_POINT ( 'NONE',  ( 2.731371607455813422, -1.798138232897347644, 0.6916047562727283271 ) ) ;
#122404 = CARTESIAN_POINT ( 'NONE',  ( -9.158696461231359720, 10.64389961198009615, 1.199719254218462483 ) ) ;
#122405 = CARTESIAN_POINT ( 'NONE',  ( -0.1298852118743892559, 2.894271690123681573, -2.215574276383952768 ) ) ;
#122406 = FACE_OUTER_BOUND ( 'NONE', #137608, .T. ) ;
#122407 = DIRECTION ( 'NONE',  ( 0.000000000000000000, -1.000000000000000000, 0.000000000000000000 ) ) ;
#122408 = CARTESIAN_POINT ( 'NONE',  ( 4.310602774141044868, 7.116454772218158809, -1.199719254218452047 ) ) ;
#122409 = EDGE_LOOP ( 'NONE', ( #69919, #114856, #84782, #198444 ) ) ;
#122410 = CARTESIAN_POINT ( 'NONE',  ( 4.746763178560261309, 5.670883475476017566, 1.082531754730549078 ) ) ;
#122411 = ORIENTED_EDGE ( 'NONE', *, *, #157331, .F. ) ;
#122413 = CARTESIAN_POINT ( 'NONE',  ( 3.141273780804701765, 0.05169848057553745602, 2.012594475454997145 ) ) ;
#122412 = CARTESIAN_POINT ( 'NONE',  ( 5.724118993814841794, 1.776208094789998304, 0.4848738846057951135 ) ) ;
#122414 = CARTESIAN_POINT ( 'NONE',  ( 5.642068729656325665, -0.04839715497878017969, -2.298027403377851385 ) ) ;
#122416 = CARTESIAN_POINT ( 'NONE',  ( 3.080726782406420838, 1.750568488035513681, 0.6316850995219197573 ) ) ;
#122415 = CARTESIAN_POINT ( 'NONE',  ( 10.62873463776380056, 9.799999999999998934, -3.200000000000001510 ) ) ;
#122418 = CARTESIAN_POINT ( 'NONE',  ( 1.642778471875001811, -0.6927083328553753638, 2.845375778867859751 ) ) ;
#122417 = ADVANCED_BREP_SHAPE_REPRESENTATION ( '', ( #86932, #200407 ), #155604 ) ;
#122419 = CARTESIAN_POINT ( 'NONE',  ( 0.000000000000000000, 9.799999999999982947, 0.000000000000000000 ) ) ;
#122420 = CARTESIAN_POINT ( 'NONE',  ( -11.84668730067608600, 10.89999999999998259, 1.399999999999998579 ) ) ;
#122421 = CARTESIAN_POINT ( 'NONE',  ( -6.826694039680798021, 7.923230120171105284, -1.199719254218446718 ) ) ;
#122422 = EDGE_CURVE ( 'NONE', #135209, #12134, #76329, .T. ) ;
#122423 = CARTESIAN_POINT ( 'NONE',  ( -5.641601317062259646, 5.754492089426966217, -0.7216878364870338292 ) ) ;
#122424 = CARTESIAN_POINT ( 'NONE',  ( 6.269093502906415871, 2.000459608610676288, -0.6076830679577133187 ) ) ;
#122425 = CARTESIAN_POINT ( 'NONE',  ( 6.182154858151487353, 6.314861544039274577, -0.7216878364870257245 ) ) ;
#122426 = ORIENTED_EDGE ( 'NONE', *, *, #102711, .F. ) ;
#122427 = PLANE ( 'NONE',  #15410 ) ;
#122428 = DIRECTION ( 'NONE',  ( 0.000000000000000000, 0.000000000000000000, -1.000000000000000000 ) ) ;
#122429 = CARTESIAN_POINT ( 'NONE',  ( 0.8030139110496161692, 1.490934425176414502, 1.053415343471690857 ) ) ;
#122430 = CARTESIAN_POINT ( 'NONE',  ( -4.466521540698216164, 7.298359999868178960, -1.199719254218452047 ) ) ;
#122431 = MECHANICAL_DESIGN_GEOMETRIC_PRESENTATION_REPRESENTATION (  '', ( #94684 ), #28961 ) ;
#122432 = CARTESIAN_POINT ( 'NONE',  ( 2.127222352579770881, 0.3811697317757706815, 1.691523546451817683 ) ) ;
#122433 = CYLINDRICAL_SURFACE ( 'NONE', #46659, 0.4000000000000010214 ) ;
#122434 = CARTESIAN_POINT ( 'NONE',  ( -6.124532705071231931, 8.168374127381657246, -1.599625672291263179 ) ) ;
#122435 = CARTESIAN_POINT ( 'NONE',  ( 6.727182134110200273, 7.629137130509069387, 2.789055895399249696 ) ) ;
#122436 = CARTESIAN_POINT ( 'NONE',  ( 6.895391736652770831, -1.943277935985653349, 0.9682779983983346161 ) ) ;
#122437 = CARTESIAN_POINT ( 'NONE',  ( 5.953692858212231265, 0.5253669772854427933, -1.748464709795935157 ) ) ;
#122438 = CARTESIAN_POINT ( 'NONE',  ( 3.116010788575247936, 1.952738871351952232, -0.1875660449981580158 ) ) ;
#122439 = CARTESIAN_POINT ( 'NONE',  ( 1.224999999999989209, -1.083333332650529224, 0.7072540797572777205 ) ) ;
#122440 = CARTESIAN_POINT ( 'NONE',  ( -7.641992139597101108, 12.06740792950531649, 0.7998128361456481317 ) ) ;
#122441 = CARTESIAN_POINT ( 'NONE',  ( 6.751070424600909448, 9.963667031088037973, -1.199719254218441611 ) ) ;
#122442 = CARTESIAN_POINT ( 'NONE',  ( 3.369896858953733698, 0.5134250039646214292, -2.057278921464212207 ) ) ;
#122443 = LINE ( 'NONE', #26960, #114049 ) ;
#122444 = CARTESIAN_POINT ( 'NONE',  ( -1.499999999999997780, 4.400000000000021672, 1.214306433183764966E-14 ) ) ;
#122445 = AXIS2_PLACEMENT_3D ( 'NONE', #163206, #180509, #32129 ) ;
#122446 = CARTESIAN_POINT ( 'NONE',  ( 1.885682352965558639, -1.950755244972163904, 0.6936349442826782452 ) ) ;
#122448 = CARTESIAN_POINT ( 'NONE',  ( -1.364683531250000748, -0.9281249996585805295, 0.000000000000000000 ) ) ;
#122447 = DIRECTION ( 'NONE',  ( 0.000000000000000000, 0.000000000000000000, 1.000000000000000000 ) ) ;
#122450 = VERTEX_POINT ( 'NONE', #8119 ) ;
#122449 = CARTESIAN_POINT ( 'NONE',  ( 4.828890449103202975, 1.532327986240004103, -1.608379539844583705 ) ) ;
#122451 = CARTESIAN_POINT ( 'NONE',  ( 1.723655420059172050, 2.274453554295458702, 0.3322429970207661509 ) ) ;
#122453 = CARTESIAN_POINT ( 'NONE',  ( 0.3913574919355842785, -1.795980968407092426, 0.7896611536716554580 ) ) ;
#122452 = CARTESIAN_POINT ( 'NONE',  ( 7.944714827928033962, 12.21265836598400689, 0.7216878364870438212 ) ) ;
#122455 = CARTESIAN_POINT ( 'NONE',  ( -3.474999999999998312, -0.3208333333333319715, 2.006292185433951047 ) ) ;
#122454 = CARTESIAN_POINT ( 'NONE',  ( 4.634908411025333130, 6.500755460986618495, 1.599625672291268286 ) ) ;
#122456 = CARTESIAN_POINT ( 'NONE',  ( 1.445103857048100515, 8.688264192037886247, 2.625611233228254182 ) ) ;
#122457 = CARTESIAN_POINT ( 'NONE',  ( 6.216338285296751920, 1.720575329815833943, 0.6561210673821931127 ) ) ;
#122458 = VERTEX_POINT ( 'NONE', #72031 ) ;
#122459 = CARTESIAN_POINT ( 'NONE',  ( 3.469446951953614189E-15, 0.7598076211376182387, 6.938893903907228378E-15 ) ) ;
#122460 = ADVANCED_FACE ( 'NONE', ( #140301 ), #2343, .T. ) ;
#122461 = CARTESIAN_POINT ( 'NONE',  ( 2.953266587970606150, -1.684550232849800544, 0.9053361341156559439 ) ) ;
#122462 = CARTESIAN_POINT ( 'NONE',  ( -0.2102771530458225069, 7.629137130509110243, -2.803678522703976661 ) ) ;
#122463 = CARTESIAN_POINT ( 'NONE',  ( 3.610098185430905104, -0.6985691267104906510, -1.577150584296799440 ) ) ;
#122464 = CARTESIAN_POINT ( 'NONE',  ( 2.747280062631300535, 0.2910806042949847239, -1.995268371848608835 ) ) ;
#122465 = CARTESIAN_POINT ( 'NONE',  ( 3.481312804724666421, -2.296076454524886845, -0.1115701876132721843 ) ) ;
#122466 = CARTESIAN_POINT ( 'NONE',  ( 3.409705294423628352, -0.4451680670645007387, 2.218022689048837481 ) ) ;
#122467 = CARTESIAN_POINT ( 'NONE',  ( 6.656868561830338038, -1.629224735911166233, 1.334343933791133141 ) ) ;
#122468 = CARTESIAN_POINT ( 'NONE',  ( -5.966997003790232235, 7.094489604910957148, -1.082531754730549967 ) ) ;
#122469 = CARTESIAN_POINT ( 'NONE',  ( 4.534285406439878763, 1.735348426437629765, 0.3461848140887160974 ) ) ;
#122471 = CARTESIAN_POINT ( 'NONE',  ( 1.377341666110833529, 2.116387791839238641, -0.8810097948994728423 ) ) ;
#122470 = CARTESIAN_POINT ( 'NONE',  ( 6.013923656113508542, 9.173938811177871244, -1.199719254218452047 ) ) ;
#122472 = CARTESIAN_POINT ( 'NONE',  ( 6.105383947169263692, -1.826632712061267094, 0.2301338403083788009 ) ) ;
#122473 = CARTESIAN_POINT ( 'NONE',  ( -3.460355519985875983, 5.060167411448709629, 1.599625672291267398 ) ) ;
#122474 = CARTESIAN_POINT ( 'NONE',  ( 5.384801694919699067, 1.933943663793664225, -1.030698541907522081 ) ) ;
#122475 = DIRECTION ( 'NONE',  ( 0.000000000000000000, 0.000000000000000000, -1.000000000000000000 ) ) ;
#122476 = CARTESIAN_POINT ( 'NONE',  ( -5.973748133451506348, 15.46936577441865168, 10.41719235512011998 ) ) ;
#122477 = CARTESIAN_POINT ( 'NONE',  ( 5.846161131210033446, -0.9342735719010831774, 1.847668428805064655 ) ) ;
#122478 = CARTESIAN_POINT ( 'NONE',  ( 0.3742329010679063539, -2.001858617179689492, -0.2420261300371470137 ) ) ;
#122479 = CARTESIAN_POINT ( 'NONE',  ( -0.7500000000000249800, -1.277083332650516656, 1.299038105676659116 ) ) ;
#122480 = CARTESIAN_POINT ( 'NONE',  ( 4.318917837333097864, 1.761897194459721927, 0.7795765077616281236 ) ) ;
#122481 = CARTESIAN_POINT ( 'NONE',  ( 0.6823417656249934904, 10.69270833367473550, 1.181850606188764807 ) ) ;
#122482 = CARTESIAN_POINT ( 'NONE',  ( -4.311129659465605002, 4.131998812239033647, 0.7216878364870317197 ) ) ;
#122483 = CARTESIAN_POINT ( 'NONE',  ( 1.688022500292500228, 2.124017718264622268, -0.6504838024826449239 ) ) ;
#122485 = ORIENTED_EDGE ( 'NONE', *, *, #85855, .F. ) ;
#122484 = DIRECTION ( 'NONE',  ( 0.000000000000000000, -1.000000000000000000, 0.000000000000000000 ) ) ;
#122487 = CARTESIAN_POINT ( 'NONE',  ( 5.680503174445848735, 5.729601246382692636, 1.040834085586084257E-14 ) ) ;
#122486 = CARTESIAN_POINT ( 'NONE',  ( -10.95308175811721085, 11.29999999999998117, 1.799999999999999600 ) ) ;
#122488 = CARTESIAN_POINT ( 'NONE',  ( 4.403700966340357681, 4.032072637018845107, -0.7998128361456211532 ) ) ;
#122489 = CARTESIAN_POINT ( 'NONE',  ( -5.382223794500848868, 5.381608636446845395, -0.7216878364870227269 ) ) ;
#122490 = CARTESIAN_POINT ( 'NONE',  ( 1.499999999999989120, 6.280000000000042881, 2.500000000000003997 ) ) ;
#122491 = CARTESIAN_POINT ( 'NONE',  ( 11.46886997981669509, 8.378336224489386197, 3.378633107758532095 ) ) ;
#122492 = CARTESIAN_POINT ( 'NONE',  ( 10.01911233037457905, 11.75168114260095109, 1.082531754730548412 ) ) ;
#122493 = CARTESIAN_POINT ( 'NONE',  ( 1.433958818539453395, 1.165882187713672247, 1.577721859592796205 ) ) ;
#122494 = CARTESIAN_POINT ( 'NONE',  ( -1.402160292154681736E-14, 2.009375000341422801, -1.575800808251660134 ) ) ;
#122495 = EDGE_CURVE ( 'NONE', #20303, #50054, #147298, .T. ) ;
#122496 = CARTESIAN_POINT ( 'NONE',  ( 4.217276354152451390, 3.814577256132954730, 1.214306433183764966E-14 ) ) ;
#122497 = AXIS2_PLACEMENT_3D ( 'NONE', #162850, #146615, #114164 ) ;
#122498 = CARTESIAN_POINT ( 'NONE',  ( 6.320756440275016708, -1.388331291134708767, 1.386421665916007795 ) ) ;
#122499 = CARTESIAN_POINT ( 'NONE',  ( -9.657485491635913633, 10.16148791653038330, 1.040834085586084257E-14 ) ) ;
#122500 = CARTESIAN_POINT ( 'NONE',  ( -3.416291520519271874, 6.929497840673697340, 1.040834085586084257E-14 ) ) ;
#122501 = CARTESIAN_POINT ( 'NONE',  ( 6.789893189004300389, -0.9291300992274166282, 1.949920244826188309 ) ) ;
#122503 = VERTEX_POINT ( 'NONE', #106751 ) ;
#122502 = CARTESIAN_POINT ( 'NONE',  ( -7.054319997812058318, 7.124461507069184130, 1.040834085586084257E-14 ) ) ;
#122504 = CARTESIAN_POINT ( 'NONE',  ( -1.364683531250010295, 5.488541667008087543, -0.7879004041258300672 ) ) ;
#122505 = CARTESIAN_POINT ( 'NONE',  ( 0.9834252619641962179, 1.251819791611600285, 1.390119989509101650 ) ) ;
#122506 = CARTESIAN_POINT ( 'NONE',  ( 6.784571902810725419, -1.680486618648807218, 0.4264331113166124343 ) ) ;
#122507 = AXIS2_PLACEMENT_3D ( 'NONE', #126098, #74066, #192058 ) ;
#122509 = CARTESIAN_POINT ( 'NONE',  ( 4.177398808104064720, 1.432170664236757540, 1.658919600136643524 ) ) ;
#122508 = CARTESIAN_POINT ( 'NONE',  ( 0.6801582343749865700, 2.307291667008083635, -1.178068619123879834 ) ) ;
#122510 = CARTESIAN_POINT ( 'NONE',  ( 4.067613405475267285, 0.2862205578705340203, -2.289715105617713409 ) ) ;
#122511 = CARTESIAN_POINT ( 'NONE',  ( 0.1982117360312448395, -2.060432452642831702, -0.05102901230808094130 ) ) ;
#122512 = CARTESIAN_POINT ( 'NONE',  ( 2.572129589083424150, -1.858482343604623610, -0.5632287606567585314 ) ) ;
#122513 = CARTESIAN_POINT ( 'NONE',  ( -5.707619481228832115, 6.721606151930833661, -1.082531754730543971 ) ) ;
#122514 = PLANE ( 'NONE',  #161246 ) ;
#122515 = CARTESIAN_POINT ( 'NONE',  ( 5.062787373817618786, 0.6179034821891697948, 2.028544477791139222 ) ) ;
#122516 = DIRECTION ( 'NONE',  ( 7.387867266669436732E-31, -1.000000000000000000, -8.546850786086424434E-32 ) ) ;
#122517 = CARTESIAN_POINT ( 'NONE',  ( 3.674454069786535548, 1.462445212485608437, 1.388486266691544957 ) ) ;
#122518 = CARTESIAN_POINT ( 'NONE',  ( -5.721177634842498527, 5.777054783512106440, 0.000000000000000000 ) ) ;
#122519 = CARTESIAN_POINT ( 'NONE',  ( -7.282664789195997912, 8.525472337930658284, 1.199719254218452047 ) ) ;
#122520 = CARTESIAN_POINT ( 'NONE',  ( 9.911173986789782120, 11.52179005846497972, -1.199719254218440723 ) ) ;
#122521 = CARTESIAN_POINT ( 'NONE',  ( 0.8205984872286451459, 1.685833220154912881, 0.7012733028506010768 ) ) ;
#122522 = CARTESIAN_POINT ( 'NONE',  ( -6.017840079619296567, 8.114175741012878973, -1.599625672291271394 ) ) ;
#122523 = CARTESIAN_POINT ( 'NONE',  ( -4.132202957115018727, 8.042930226601317401, 0.000000000000000000 ) ) ;
#122524 = CARTESIAN_POINT ( 'NONE',  ( -11.73082749631449140, 4.534045925630191931, 5.066687987500840151 ) ) ;
#122525 = ORIENTED_EDGE ( 'NONE', *, *, #168972, .T. ) ;
#122526 = CARTESIAN_POINT ( 'NONE',  ( 5.120021580010623907, -1.100570584753908454, -1.742215132906791641 ) ) ;
#122527 = CARTESIAN_POINT ( 'NONE',  ( -6.414416072596845986, 8.576847732820027659, -1.443375672974066548 ) ) ;
#122528 = UNCERTAINTY_MEASURE_WITH_UNIT (LENGTH_MEASURE( 1.000000000000000082E-05 ), #55190, 'distance_accuracy_value', 'NONE');
#122529 = CARTESIAN_POINT ( 'NONE',  ( 6.604230223188150894, 9.758666789477915771, -1.082531754730548412 ) ) ;
#122530 = CARTESIAN_POINT ( 'NONE',  ( -3.307299406729781399, 5.945934176904983381, -1.199719254218452935 ) ) ;
#122531 = CARTESIAN_POINT ( 'NONE',  ( -8.448702279610222021, 13.00856975952063088, 1.040834085586084257E-14 ) ) ;
#122532 = CARTESIAN_POINT ( 'NONE',  ( 5.162762804107727810, 0.5884847259931770269, 1.932018068032066438 ) ) ;
#122534 = VERTEX_POINT ( 'NONE', #10254 ) ;
#122533 = CARTESIAN_POINT ( 'NONE',  ( 5.426523936546859161, -0.9972995744461101708, -1.984925452567573023 ) ) ;
#122535 = CARTESIAN_POINT ( 'NONE',  ( -4.625266680917477835, 5.425174544939014964, -1.199719254218453823 ) ) ;
#122536 = CARTESIAN_POINT ( 'NONE',  ( 4.632082037363250748, 8.555846143565791095, -0.7998128361456231517 ) ) ;
#122537 = CARTESIAN_POINT ( 'NONE',  ( 4.399328490915206835, 1.653984737846543540, 1.229246434344443806 ) ) ;
#122538 = CARTESIAN_POINT ( 'NONE',  ( 3.551407868487792552, -1.352154898762620849, 1.496051317864898866 ) ) ;
#122539 = ORIENTED_EDGE ( 'NONE', *, *, #49979, .F. ) ;
#122540 = CARTESIAN_POINT ( 'NONE',  ( 2.920214025141053327, 6.445393704534057022, 0.4458799699700779495 ) ) ;
#122541 = CARTESIAN_POINT ( 'NONE',  ( 4.227444969362701421, 3.826440640544909400, 1.214306433183764966E-14 ) ) ;
#122543 = ORIENTED_EDGE ( 'NONE', *, *, #87783, .F. ) ;
#122542 = CARTESIAN_POINT ( 'NONE',  ( -5.908321080505254841, 10.11506803722328129, 0.7998128361456291469 ) ) ;
#122544 = CARTESIAN_POINT ( 'NONE',  ( 4.653539691347775786, 8.417882268172059312, -0.4891605808478947104 ) ) ;
#122545 = CARTESIAN_POINT ( 'NONE',  ( 4.253279712585047001, -1.993766238088546361, -0.2985801555873274227 ) ) ;
#122546 = CARTESIAN_POINT ( 'NONE',  ( 3.363068133243895197, 1.796009578954290253, -0.4044003374430102382 ) ) ;
#122547 = DIRECTION ( 'NONE',  ( 1.000000000000000000, 0.000000000000000000, 0.000000000000000000 ) ) ;
#122548 = CARTESIAN_POINT ( 'NONE',  ( 1.717812883538033297, -0.2792282863031622653, 2.290681961221084695 ) ) ;
#122549 = CARTESIAN_POINT ( 'NONE',  ( 5.571474780572990504, 5.464751763615448787, 0.7998128361456352531 ) ) ;
#122550 = ADVANCED_FACE ( 'NONE', ( #126233, #89397 ), #40648, .F. ) ;
#122551 = CARTESIAN_POINT ( 'NONE',  ( 4.253314833958360630, -1.794556715717060769, -1.204719293387515267 ) ) ;
#122552 = CARTESIAN_POINT ( 'NONE',  ( 8.934986926605834157, 10.38290515491702770, -1.199719254218446718 ) ) ;
#122553 = CARTESIAN_POINT ( 'NONE',  ( -4.225337428953291230, 8.081310767087481750, 0.7998128361456341429 ) ) ;
#122554 = CARTESIAN_POINT ( 'NONE',  ( 3.726148964702048705, -2.024938297411133625, -1.087335920097615594 ) ) ;
#122555 = CARTESIAN_POINT ( 'NONE',  ( 10.39230484541330313, 3.499999999999989342, 5.999999999999906741 ) ) ;
#122556 = CARTESIAN_POINT ( 'NONE',  ( 2.043623373375623942, 0.7184291972081280342, -1.727395513401897453 ) ) ;
#122557 = CARTESIAN_POINT ( 'NONE',  ( 6.825078400183526739, -0.0002198122173602961866, 1.955566246027613531 ) ) ;
#122559 = CARTESIAN_POINT ( 'NONE',  ( -6.454563648557663846, 9.688018802362710957, -1.199719254218452047 ) ) ;
#122558 = CARTESIAN_POINT ( 'NONE',  ( -0.6823417656249969321, 4.217708333674755394, -1.181850606188749264 ) ) ;
#122561 = CARTESIAN_POINT ( 'NONE',  ( 2.051678093609669240, -1.773579625386853875, -1.313098587465796774 ) ) ;
#122560 = CARTESIAN_POINT ( 'NONE',  ( -4.954615070790188369, 7.867802451642154082, -1.199719254218452047 ) ) ;
#122562 = CARTESIAN_POINT ( 'NONE',  ( -1.436717785781610024, 7.422226822640078048, -4.237127798884826824 ) ) ;
#122563 = CARTESIAN_POINT ( 'NONE',  ( 5.789495288235341874, 6.713164910151406595, 1.199719254218462483 ) ) ;
#122564 = CARTESIAN_POINT ( 'NONE',  ( -5.925076824372040640, 6.871343368977510302, 1.199719254218450271 ) ) ;
#122565 = CARTESIAN_POINT ( 'NONE',  ( -8.024185963717894055, -5.166862990899638852, 7.524604700374177391 ) ) ;
#122566 = CARTESIAN_POINT ( 'NONE',  ( 6.491095702449441340, 1.715375089605765124, -0.9715357305846801239 ) ) ;
#122567 = CARTESIAN_POINT ( 'NONE',  ( 5.426528828858072195, 1.378586375901286187, -1.850541897242431677 ) ) ;
#122569 = EDGE_CURVE ( 'NONE', #162878, #98728, #209506, .T. ) ;
#122568 = CARTESIAN_POINT ( 'NONE',  ( 6.830517471914854255, -1.143533572366756124, 1.468690548319721900 ) ) ;
#122570 = CARTESIAN_POINT ( 'NONE',  ( 2.641531011850445143, 1.887532825382558066, -0.8318756707885038848 ) ) ;
#122571 = CARTESIAN_POINT ( 'NONE',  ( 7.307481608085759639, 7.627742752295940676, 1.040834085586084257E-14 ) ) ;
#122572 = CARTESIAN_POINT ( 'NONE',  ( 7.828907357248368726, 8.098423103070084395, 0.7998128361456281477 ) ) ;
#122573 = CARTESIAN_POINT ( 'NONE',  ( 6.277061933002769045, 10.26706332190449622, 0.7216878364870438212 ) ) ;
#122574 = CARTESIAN_POINT ( 'NONE',  ( 0.6823417656249882723, 2.988541667008084879, -1.181850606188754593 ) ) ;
#122575 = CARTESIAN_POINT ( 'NONE',  ( -11.04536101718726293, 12.59409062111168609, -1.100000000000000311 ) ) ;
#122576 = CARTESIAN_POINT ( 'NONE',  ( 4.324687812634882000, 7.028924300507257250, 1.082531754730558626 ) ) ;
#122577 = CARTESIAN_POINT ( 'NONE',  ( 5.266168369200141086, -2.161202989243858674, 0.2077703183603739345 ) ) ;
#122578 = APPLICATION_CONTEXT ( 'automotive_design' ) ;
#122580 = CARTESIAN_POINT ( 'NONE',  ( 5.056134578334451568, -1.329838508726857382, 1.273713382018211382 ) ) ;
#122579 = DIRECTION ( 'NONE',  ( 0.000000000000000000, 0.000000000000000000, -1.000000000000000000 ) ) ;
#122581 = CARTESIAN_POINT ( 'NONE',  ( 9.516228778038653857, -8.176227079964613509, -0.3870642018030908682 ) ) ;
#122582 = CARTESIAN_POINT ( 'NONE',  ( 0.2999999999999842792, 3.975028841772351829, 0.9637995837462106641 ) ) ;
#122583 = CARTESIAN_POINT ( 'NONE',  ( 0.4033012769992084245, -0.5052730135347225371, 1.800932346938296069 ) ) ;
#122584 = CARTESIAN_POINT ( 'NONE',  ( 0.7732102150014728004, -2.130643883221981838, -0.7610950190743612787 ) ) ;
#122585 = CARTESIAN_POINT ( 'NONE',  ( -4.081306271799089558, 7.708262650413779227, 0.6970576149333465032 ) ) ;
#122586 = DIRECTION ( 'NONE',  ( 0.000000000000000000, -1.000000000000000000, 0.000000000000000000 ) ) ;
#122587 = CARTESIAN_POINT ( 'NONE',  ( 5.669760509565840323, 7.437725440679550992, 1.325564871123290356 ) ) ;
#122588 = CARTESIAN_POINT ( 'NONE',  ( 11.86145016429273191, 13.40000000000000036, 1.099999999999996758 ) ) ;
#122589 = CARTESIAN_POINT ( 'NONE',  ( 1.762210296550786204, -1.254468555733399660, 1.248734745320427830 ) ) ;
#122590 = CARTESIAN_POINT ( 'NONE',  ( 6.533844907621704223, -1.952130696095262463, 0.4912315161729706725 ) ) ;
#122592 = CARTESIAN_POINT ( 'NONE',  ( 3.567908551050925858, -0.9411222629213971125, 1.668380548182837542 ) ) ;
#122591 = CARTESIAN_POINT ( 'NONE',  ( -10.15522075183580419, 11.80651128435196462, 1.199719254218462483 ) ) ;
#122593 = CARTESIAN_POINT ( 'NONE',  ( -1.499999999999997780, 4.150000000000021672, 1.214306433183764966E-14 ) ) ;
#122594 = CARTESIAN_POINT ( 'NONE',  ( 3.982825254072485777, 1.869399454171687180, 0.6202158817144760583 ) ) ;
#122595 = CARTESIAN_POINT ( 'NONE',  ( 0.3168469074051638024, -0.7203255543706194031, -1.994627023381766673 ) ) ;
#122596 = CARTESIAN_POINT ( 'NONE',  ( -4.308793891044708779, 3.921347715840572956, 1.214306433183764966E-14 ) ) ;
#122597 = CARTESIAN_POINT ( 'NONE',  ( 3.326877442632663939, 0.04465521416292458912, 1.870282673472216439 ) ) ;
#122599 = ORIENTED_EDGE ( 'NONE', *, *, #30637, .T. ) ;
#122598 = CARTESIAN_POINT ( 'NONE',  ( 6.234932630344998117, 0.1766075427261544484, 1.715814389380666327 ) ) ;
#122601 = CARTESIAN_POINT ( 'NONE',  ( 2.738383840280328663, 5.178236332760252303, 1.082531754730548412 ) ) ;
#122600 = CARTESIAN_POINT ( 'NONE',  ( 2.192262590105994668, -0.9421081357594159877, 1.995820444975453745 ) ) ;
#122602 = CARTESIAN_POINT ( 'NONE',  ( -0.6823417656250212460, 3.363541667008085323, 1.181850606188767472 ) ) ;
#122603 = CARTESIAN_POINT ( 'NONE',  ( 6.373494408814909917, -0.2414686440028299685, 1.946897059556201848 ) ) ;
#122604 = CARTESIAN_POINT ( 'NONE',  ( 7.995557903757111617, 10.35123685918189729, 1.599625672291281386 ) ) ;
#122605 = CARTESIAN_POINT ( 'NONE',  ( -10.50487009249003378, 11.15010328419353947, 0.7998128361456462443 ) ) ;
#122606 = CARTESIAN_POINT ( 'NONE',  ( 0.000000000000000000, 5.939655416065874327, 0.000000000000000000 ) ) ;
#122607 = CARTESIAN_POINT ( 'NONE',  ( 0.1747926744264677867, 0.7439089246787933263, -1.939883394317852616 ) ) ;
#122608 = MECHANICAL_DESIGN_GEOMETRIC_PRESENTATION_REPRESENTATION (  '', ( #67119 ), #23408 ) ;
#122609 = CARTESIAN_POINT ( 'NONE',  ( -7.626802973668077357, -6.615717645447081630, -7.927630635717592078 ) ) ;
#122610 = EDGE_LOOP ( 'NONE', ( #32374, #49383, #200713, #72257 ) ) ;
#122611 = CARTESIAN_POINT ( 'NONE',  ( 2.963400493335893948, 1.747644659881589568, 1.109742091278065113 ) ) ;
#122612 = CARTESIAN_POINT ( 'NONE',  ( -0.7500000000000215383, 3.691666666666690411, 1.299038105676671107 ) ) ;
#122613 = CARTESIAN_POINT ( 'NONE',  ( 4.150767584078112193, 7.994312614733129152, 0.7998128361456321445 ) ) ;
#122614 = CARTESIAN_POINT ( 'NONE',  ( -6.454776619733716636, 6.787828609132271929, -0.3692292702514640146 ) ) ;
#122616 = EDGE_CURVE ( 'NONE', #120076, #69400, #132944, .T. ) ;
#122615 = CARTESIAN_POINT ( 'NONE',  ( 0.4694063198951373694, -1.707435420315214003, -1.078448885650341582 ) ) ;
#122617 = CARTESIAN_POINT ( 'NONE',  ( 1.499999999999999556, 7.809254910141758543, 3.635752117236003667 ) ) ;
#122618 = CARTESIAN_POINT ( 'NONE',  ( 0.6823417656249917140, 4.342708333674755394, 1.181850606188765695 ) ) ;
#122619 = EDGE_CURVE ( 'NONE', #173996, #137701, #145999, .T. ) ;
#122621 = CARTESIAN_POINT ( 'NONE',  ( 8.676855123066012254, 11.14608361504227574, -1.443375672974052559 ) ) ;
#122620 = CARTESIAN_POINT ( 'NONE',  ( 0.07459516483343266169, 4.098104556601829707, -2.310507343083552989 ) ) ;
#122622 = CARTESIAN_POINT ( 'NONE',  ( 5.518907608433407219, 2.013924273726455549, -0.09612181791086168992 ) ) ;
#122623 = CARTESIAN_POINT ( 'NONE',  ( 5.770691199759951040, -0.2880491948782157308, -1.893834403066462446 ) ) ;
#122624 = LINE ( 'NONE', #152890, #20508 ) ;
#122625 = CARTESIAN_POINT ( 'NONE',  ( 3.685266855566126321, 1.588411730319793769, 1.510178839762461811 ) ) ;
#122626 = CARTESIAN_POINT ( 'NONE',  ( -0.7500000000000006661, 1.889583334016155192, -1.299038105676652011 ) ) ;
#122627 = CARTESIAN_POINT ( 'NONE',  ( 2.795058504854182946, -0.1448928079688660830, -1.906987441340234568 ) ) ;
#122628 = CARTESIAN_POINT ( 'NONE',  ( -4.543954038874438162, 8.453030145328826350, 1.040834085586084257E-14 ) ) ;
#122629 = CARTESIAN_POINT ( 'NONE',  ( 4.107757354816228279, 6.775838766385488654, -1.082531754730548412 ) ) ;
#122631 = CARTESIAN_POINT ( 'NONE',  ( -0.1234324464992678227, -0.4448297287729073846, -1.973926538189611835 ) ) ;
#122630 = CARTESIAN_POINT ( 'NONE',  ( 3.582479189645107809, 7.343285104996937207, -0.3223619143407419063 ) ) ;
#122632 = CARTESIAN_POINT ( 'NONE',  ( 0.6823417656249969321, 10.83854166700806765, -1.181850606188757036 ) ) ;
#122634 = CARTESIAN_POINT ( 'NONE',  ( -6.119526231721793330, 8.232809585132461194, 1.599625672291263179 ) ) ;
#122633 = CARTESIAN_POINT ( 'NONE',  ( 5.689076433642084041, 1.658752129386225516, 1.432425853890168188 ) ) ;
#122636 = ORIENTED_EDGE ( 'NONE', *, *, #55551, .T. ) ;
#122635 = CARTESIAN_POINT ( 'NONE',  ( 3.170621359714973941, -1.593115903276512757, -0.6614109595024783017 ) ) ;
#122637 = CARTESIAN_POINT ( 'NONE',  ( 6.011998765391792787, -0.7129019540204998284, 1.997330473063135381 ) ) ;
#122638 = CARTESIAN_POINT ( 'NONE',  ( 7.308008492965924141, 8.484763649003774333, -1.199719254218451159 ) ) ;
#122639 = CARTESIAN_POINT ( 'NONE',  ( 5.148345644887269756, 7.029489223833707001, -1.599625672291256295 ) ) ;
#122640 = DIRECTION ( 'NONE',  ( 1.000000000000000000, -5.578564026256504688E-16, 0.000000000000000000 ) ) ;
#122641 = CARTESIAN_POINT ( 'NONE',  ( 0.6253529088778920775, 0.1960189665039281104, -1.952063659030291998 ) ) ;
#122642 = CARTESIAN_POINT ( 'NONE',  ( 5.681030059326015014, 6.586622143090519188, -1.199719254218445830 ) ) ;
#122643 = CARTESIAN_POINT ( 'NONE',  ( 2.039928227386953008, 3.162178953954597471, -11.45750328113830108 ) ) ;
#122644 = ORIENTED_EDGE ( 'NONE', *, *, #187034, .T. ) ;
#122645 = CARTESIAN_POINT ( 'NONE',  ( 9.499700864329909678, -7.154544010627095219, 0.07538891330675402680 ) ) ;
#122646 = ORIENTED_EDGE ( 'NONE', *, *, #192009, .T. ) ;
#122647 = CARTESIAN_POINT ( 'NONE',  ( 3.158660791640830467, 0.4427227019567353539, 1.756387338163778233 ) ) ;
#122648 = ORIENTED_EDGE ( 'NONE', *, *, #64465, .T. ) ;
#122649 = CARTESIAN_POINT ( 'NONE',  ( 8.516493047678546091, 13.08765898893368629, -0.7998128361456352531 ) ) ;
#122650 = CARTESIAN_POINT ( 'NONE',  ( 6.249382461256315580, 6.255644057745969988, -0.7998128361456481317 ) ) ;
#122651 = CARTESIAN_POINT ( 'NONE',  ( 3.773895570499671503, 1.797357569013877887, -0.2251608728849313346 ) ) ;
#122652 = CARTESIAN_POINT ( 'NONE',  ( 0.5723387408578806124, 3.454750211409410632, 0.3125093782470996229 ) ) ;
#122653 = CARTESIAN_POINT ( 'NONE',  ( -8.023115266309158500, -5.166862915010145052, 7.407835137441773021 ) ) ;
#122654 = CARTESIAN_POINT ( 'NONE',  ( 5.039007818866061861, 6.552116822607409574, 1.229770346242751389 ) ) ;
#122656 = CARTESIAN_POINT ( 'NONE',  ( -0.6823417656250003738, 14.40104166700806232, 1.181850606188754593 ) ) ;
#122655 = CARTESIAN_POINT ( 'NONE',  ( 5.213276571848306951, -1.572085989900060765, -0.9957144527335654027 ) ) ;
#122657 = CARTESIAN_POINT ( 'NONE',  ( 2.812013442917372430, 1.061847183940438422, -1.594151112820214822 ) ) ;
#122658 = CARTESIAN_POINT ( 'NONE',  ( 0.8502975112493587062, 0.5252643332615304361, 1.748389446526978031 ) ) ;
#122659 = AXIS2_PLACEMENT_3D ( 'NONE', #67206, #165810, #136522 ) ;
#122660 = DIRECTION ( 'NONE',  ( 1.000000000000000000, -0.000000000000000000, -0.000000000000000000 ) ) ;
#122661 = CARTESIAN_POINT ( 'NONE',  ( -11.19364298753552411, 5.612864353363596237, -3.868560769348357464 ) ) ;
#122662 = CARTESIAN_POINT ( 'NONE',  ( 5.324837791525375508, 7.612559486139466536, 1.234112182050936646 ) ) ;
#122663 = CARTESIAN_POINT ( 'NONE',  ( -11.44779965693287416, 10.10313923201287700, 3.599999932275866676 ) ) ;
#122664 = CARTESIAN_POINT ( 'NONE',  ( -1.608462485350604876, 8.735270501766756013, -2.463594439587629914 ) ) ;
#122665 = CARTESIAN_POINT ( 'NONE',  ( 1.737499999999999378, -2.522916665710750461, -3.009438278150925683 ) ) ;
#122666 = AXIS2_PLACEMENT_3D ( 'NONE', #92230, #75947, #155070 ) ;
#122667 = CARTESIAN_POINT ( 'NONE',  ( 8.120970824905713314, 8.576813505252564696, 1.040834085586084257E-14 ) ) ;
#122668 = CARTESIAN_POINT ( 'NONE',  ( -3.093231602212184850, 6.760520635889515795, -0.7998128361456281477 ) ) ;
#122669 = CARTESIAN_POINT ( 'NONE',  ( 11.86145016429273369, 12.59412591486744759, -1.100000000000002087 ) ) ;
#122670 = CARTESIAN_POINT ( 'NONE',  ( 1.640690513341718670, -1.765443103004183056, 1.119499978516135252 ) ) ;
#122671 = CARTESIAN_POINT ( 'NONE',  ( 6.458035534591947346, 1.921153000004784284, -0.1426463852419664891 ) ) ;
#122672 = CARTESIAN_POINT ( 'NONE',  ( -5.199715606040888005, 6.025088614257851027, -1.199719254218446718 ) ) ;
#122673 = CARTESIAN_POINT ( 'NONE',  ( 2.432394421669949569, 1.770131964307398498, 0.4459858026567494194 ) ) ;
#122674 = CARTESIAN_POINT ( 'NONE',  ( 3.826972293661185187, 2.095320012007126476, 0.6930106488920934060 ) ) ;
#122675 = CARTESIAN_POINT ( 'NONE',  ( 11.96212011828584387, 12.27187554950052295, 0.9569185076417748848 ) ) ;
#122676 = CARTESIAN_POINT ( 'NONE',  ( 0.7031954830387620037, 1.685401770928725007, -0.9037484838233383888 ) ) ;
#122677 = CARTESIAN_POINT ( 'NONE',  ( 1.310928286630644646, -1.554615626247756177, 1.209165358520351674 ) ) ;
#122678 = CARTESIAN_POINT ( 'NONE',  ( 3.526839302598220982, -1.793260235690095072, 0.7459913709994684394 ) ) ;
#122679 = ORIENTED_EDGE ( 'NONE', *, *, #70772, .T. ) ;
#122680 = DIRECTION ( 'NONE',  ( 0.000000000000000000, 0.000000000000000000, -1.000000000000000000 ) ) ;
#122682 = CARTESIAN_POINT ( 'NONE',  ( 6.561375291409637711, 1.546756896810308035, 1.034385502077879382 ) ) ;
#122681 = CARTESIAN_POINT ( 'NONE',  ( -5.829079699232685208, 5.765290835385048496, 0.000000000000000000 ) ) ;
#122683 = CARTESIAN_POINT ( 'NONE',  ( 3.549202351727371862, 7.362762853649070571, -0.7998128361456362523 ) ) ;
#122684 = CARTESIAN_POINT ( 'NONE',  ( 0.2883962233416060283, -9.094943692057521289, -9.630124952822544770 ) ) ;
#122685 = CARTESIAN_POINT ( 'NONE',  ( -6.961139734775127152, 5.290451655907111750, 1.299555808129863194E-14 ) ) ;
#122686 = CARTESIAN_POINT ( 'NONE',  ( -4.586401103172829785, 8.572828063668767484, 0.7998128361456281477 ) ) ;
#122687 = CARTESIAN_POINT ( 'NONE',  ( 2.736070936638954176, 2.175344985778558726, 0.2654339622269741295 ) ) ;
#122688 = FACE_OUTER_BOUND ( 'NONE', #184404, .T. ) ;
#122689 = ORIENTED_EDGE ( 'NONE', *, *, #71412, .F. ) ;
#122690 = CARTESIAN_POINT ( 'NONE',  ( 7.038618024149998043, 8.240751112043669835, -1.199719254218452047 ) ) ;
#122692 =( BOUNDED_CURVE ( )  B_SPLINE_CURVE ( 2, ( #206257, #170556, #158594, #25376, #23222, #73047, #56816, #122986, #187867 ),
 .UNSPECIFIED., .F., .T. ) 
 B_SPLINE_CURVE_WITH_KNOTS ( ( 3, 2, 2, 2, 3 ),
 ( 0.2291666666666666574, 0.2361111111111111049, 0.2500000000000000000, 0.2638888888888888951, 0.2708333333333333703 ),
 .UNSPECIFIED. ) 
 CURVE ( )  GEOMETRIC_REPRESENTATION_ITEM ( )  RATIONAL_B_SPLINE_CURVE ( ( 0.9330127018922194093, 0.9330127018922194093, 1.000000000000000000, 0.8660254037844387076, 1.000000000000000000, 0.8660254037844387076, 1.000000000000000000, 0.9330127018922190762, 0.9330127018922194093 ) ) 
 REPRESENTATION_ITEM ( '' )  );
#122691 = FACE_OUTER_BOUND ( 'NONE', #21253, .T. ) ;
#122693 = CARTESIAN_POINT ( 'NONE',  ( 4.002439121739418404, -0.5745171773131328985, -1.733004836422600725 ) ) ;
#122694 = CARTESIAN_POINT ( 'NONE',  ( 0.000000000000000000, 12.21999999999998288, 0.000000000000000000 ) ) ;
#122695 = CARTESIAN_POINT ( 'NONE',  ( -10.31739171031960822, 11.13930453823545186, 1.040834085586084257E-14 ) ) ;
#122696 = CARTESIAN_POINT ( 'NONE',  ( -4.594589183792981757, 8.486487934283967860, 0.2047448450237729367 ) ) ;
#122697 = CARTESIAN_POINT ( 'NONE',  ( -0.02968770228139894218, 7.629137130509075604, -2.426318643530885222 ) ) ;
#122698 = CARTESIAN_POINT ( 'NONE',  ( 4.030043484472041193, 1.001115284758803625, -1.580040089582811280 ) ) ;
#122699 = CARTESIAN_POINT ( 'NONE',  ( 8.076906825439115423, 10.44614393447756129, -1.599625672291262513 ) ) ;
#122700 = CARTESIAN_POINT ( 'NONE',  ( 2.490742943097464135, -0.3295026218355610603, -1.897965567226393979 ) ) ;
#122701 = CARTESIAN_POINT ( 'NONE',  ( 6.631700630569578259, 1.878258136613653040, -0.5663492180864730940 ) ) ;
#122702 = CARTESIAN_POINT ( 'NONE',  ( -1.364683531250010295, 8.942708333674731946, 0.7879004041258445001 ) ) ;
#122703 = CARTESIAN_POINT ( 'NONE',  ( -4.876128802409253282, 8.840567369452784874, 0.7998128361456481317 ) ) ;
#122704 = CARTESIAN_POINT ( 'NONE',  ( 3.659811400685081040, 6.357198169852855685, -1.199719254218446718 ) ) ;
#122705 = CARTESIAN_POINT ( 'NONE',  ( -5.492461626867567226, 6.540864998501174199, 1.082531754730549078 ) ) ;
#122706 = CARTESIAN_POINT ( 'NONE',  ( -0.07047696482224277692, -1.639844204322737697, -1.338861086256079913 ) ) ;
#122707 = VECTOR ( 'NONE', #53699, 1000.000000000000000 ) ;
#122708 = CARTESIAN_POINT ( 'NONE',  ( -1.225000000000040057, 0.5833333340161186431, 0.7072540797572817173 ) ) ;
#122709 = CARTESIAN_POINT ( 'NONE',  ( -2.657034918598345730, 5.083329257464595408, -1.082531754730543971 ) ) ;
#122710 = CARTESIAN_POINT ( 'NONE',  ( 4.610256228194366201, 2.069909489248497714, -0.04556564433023241323 ) ) ;
#122712 = CARTESIAN_POINT ( 'NONE',  ( -1.364683531250012516, 2.092708333674750953, 0.7879004041258379498 ) ) ;
#122711 = CARTESIAN_POINT ( 'NONE',  ( -0.04178991631376138827, -1.644041690304678616, -0.8291446804715857377 ) ) ;
#122713 = VERTEX_POINT ( 'NONE', #196487 ) ;
#122714 = CARTESIAN_POINT ( 'NONE',  ( 5.608098314261791728, -0.05969564267381716194, 2.298051806275173359 ) ) ;
#122715 = CARTESIAN_POINT ( 'NONE',  ( 6.968527767744109980, 7.232296605230681408, 0.7216878364870317197 ) ) ;
#122717 = CARTESIAN_POINT ( 'NONE',  ( 1.224999999999963896, 1.374999999999987343, -4.857225732735059864E-14 ) ) ;
#122716 = CARTESIAN_POINT ( 'NONE',  ( 5.099275172515607579, 5.121778254122544283, -0.7216878364870458196 ) ) ;
#122718 = CARTESIAN_POINT ( 'NONE',  ( 0.1645876019286318381, -1.492192613954560265, 1.740154187221523818 ) ) ;
#122719 = CARTESIAN_POINT ( 'NONE',  ( -5.752402313948099533, 9.933162809573264695, -0.7998128361456362523 ) ) ;
#122720 = CARTESIAN_POINT ( 'NONE',  ( 5.384693163835662766, 1.711646917711911353, -0.9173020705802971131 ) ) ;
#122721 = ORIENTED_EDGE ( 'NONE', *, *, #16450, .F. ) ;
#122723 = CARTESIAN_POINT ( 'NONE',  ( 8.554831740098649107, 11.96409221588171157, 1.082531754730546636 ) ) ;
#122722 = AXIS2_PLACEMENT_3D ( 'NONE', #164113, #11438, #195545 ) ;
#122724 = EDGE_LOOP ( 'NONE', ( #143650, #151789, #12119, #142422, #192508, #181419, #181587 ) ) ;
#122725 = CARTESIAN_POINT ( 'NONE',  ( 6.117437049485344502, 1.593764408019750389, 1.056661447057717362 ) ) ;
#122726 = CARTESIAN_POINT ( 'NONE',  ( 5.542203953035277131, 0.8216685229280199509, 1.841735684200429990 ) ) ;
#122728 =( NAMED_UNIT ( * ) SI_UNIT ( $, .STERADIAN. ) SOLID_ANGLE_UNIT ( ) );
#122727 = CARTESIAN_POINT ( 'NONE',  ( -8.696665468161981494, 12.23352791524263239, -1.199719254218446718 ) ) ;
#122729 = CARTESIAN_POINT ( 'NONE',  ( 1.001543065824772753E-15, -1.509374999522041794, 3.793834371823811669 ) ) ;
#122731 = CARTESIAN_POINT ( 'NONE',  ( 1.621574733132331358, -0.9795727578338263575, -1.473812506242745179 ) ) ;
#122730 = CARTESIAN_POINT ( 'NONE',  ( 2.378955762007132435, 1.911079870108543410, -0.8480884496332024014 ) ) ;
#122732 = CARTESIAN_POINT ( 'NONE',  ( 6.381482430641396419, -0.5404875331735843336, -1.942542459342583294 ) ) ;
#122734 = CARTESIAN_POINT ( 'NONE',  ( 4.031398662939575495, -1.579512745870830237, -1.661420017294244156 ) ) ;
#122733 =( NAMED_UNIT ( * ) SI_UNIT ( $, .STERADIAN. ) SOLID_ANGLE_UNIT ( ) );
#122735 = CARTESIAN_POINT ( 'NONE',  ( 2.571852248423611709, -1.665254919270848344, -0.5056227470447529626 ) ) ;
#122736 = CARTESIAN_POINT ( 'NONE',  ( 3.032219910950674890, 6.689340329417765574, 0.7998128361456321445 ) ) ;
#122737 = CARTESIAN_POINT ( 'NONE',  ( 6.561219994370630637, 6.619454513046008515, 0.000000000000000000 ) ) ;
#122738 = CARTESIAN_POINT ( 'NONE',  ( 1.668881318695322413, -0.6185640615885504845, -1.619952590838618312 ) ) ;
#122739 = CARTESIAN_POINT ( 'NONE',  ( 0.6801582343749674742, 1.755208333674734833, 1.178068619123803451 ) ) ;
#122740 = CARTESIAN_POINT ( 'NONE',  ( 1.170091191536073660, -0.8321358839059491697, -1.664716676500255010 ) ) ;
#122741 = CARTESIAN_POINT ( 'NONE',  ( 2.787735123443566110, -2.026669663610313865, 0.7793237752812106622 ) ) ;
#122742 = CARTESIAN_POINT ( 'NONE',  ( 4.635998460869027227, 7.496083073400806818, -1.199719254218452047 ) ) ;
#122743 = CARTESIAN_POINT ( 'NONE',  ( 3.696500153570709379, 1.422608671726926177, -1.429447704489300364 ) ) ;
#122744 = CARTESIAN_POINT ( 'NONE',  ( 2.750000000000001332, 1.574424887750340441E-13, 2.052068128417947612 ) ) ;
#122745 =( BOUNDED_SURFACE ( )  B_SPLINE_SURFACE ( 1, 2, ( 
 ( #142951, #99499, #148255, #16079, #149308, #114739, #33421, #50739, #889, #166628, #115799, #18220, #83225, #180737, #100557, #196985, #164493, #17149, #181787, #65887, #66956, #165556, #48624, #82162, #32364, #214256, #132035, #49674, #116865, #133095, #98428, #198045, #199093, #182867, #34483, #15543, #47024, #130466, #97906, #148770, #212681, #115264, #67479, #147713, #131501, #129411, #146667, #162896, #197505, #83756, #16607, #96849, #79499, #80568, #30769, #165012, #195394, #48099, #133625, #13424, #1417, #82688, #199627, #34999, #339, #51273, #66412, #132557, #196456, #114211, #149848, #117397, #145618, #183394, #211614, #179146, #14479, #213731, #65354, #100018, #33943, #198556, #161836, #166082, #64322, #180209, #63250, #31831, #113139, #163967, #81628, #49148, #50205, #116323, #181257, #32884, #98961, #182314, #17670, #20722, #88967, #69473, #203736, #106318, #6606, #123679, #153958, #41292, #22853, #3404, #205888, #189641, #36990, #187507, #87884, #136648, #171259, #5524, #57521, #135580, #139857, #201602, #53250, #4460, #72687, #71605, #168070, #155022, #70530, #39136, #121537, #21775, #119381, #202673, #104142, #138782, #54321, #105219, #73762, #137716, #55382, #185367, #152882, #169128, #204802, #90034, #56453, #103073, #85749, #86816, #120462, #122613, #186434, #38072, #19670, #151831, #7678, #188576, #170189, #40208, #172342, #23930, #156093, #78024, #75898, #142002, #29284, #161427, #173422, #13010, #157167, #124738, #190697, #93242, #159276, #45551, #193903, #176603, #107400, #111667, #42358, #174492, #145205, #92181, #62836, #158231, #59643, #10875, #94308, #110602, #192827, #108470, #177674, #26069, #208017, #44485, #76950, #128998, #79087, #143075, #160349, #28215, #11951, #144148, #211211, #9822, #210140, #61784, #125801, #209068, #191763, #127950, #60705, #43419, #126869, #95378, #194975, #25004, #91106, #27136, #109543, #8759, #74840, #140940, #206954, #175547, #58583, #180850, #134273, #33534, #97496, #132148, #214368, #114850, #146258, #15136, #197096, #99606, #163553, #65998, #166744, #32472, #16193, #14066, #31420, #47687, #82274, #182981, #115913, #196055, #178743, #179801, #130062, #49787, #80153, #147306, #18338, #112733, #100666, #181899, #84419, #46611, #165672, #150508, #17261, #83337, #81224, #213332, #34598, #2069, #30356, #68140, #96443, #63906, #113799, #98544, #164608, #199209, #133205, #149422, #162494, #50856, #64957, #131109, #212271, #48737, #148369, #198154, #1005, #67069, #116981, #203472, #71341, #3137, #72417, #135327, #86554, #137457, #186171, #155829, #106057, #37805, #38873, #55126, #121271, #187246, #23672, #52981, #170999, #22597, #168865, #103880, #119117, #88704, #169928, #152618, #21512, #154762, #104958, #6345, #138518, #120195, #202405, #87624, #153695, #70273, #151570, #5264, #36723, #185096, #204542, #101737, #56190, #122351, #188308, #7413, #39950, #73495, #172079, #35658, #89782, #200281, #69207, #51932, #118056, #20468, #184041, #167806, #19405, #85484, #201341, #102809, #4205, #136389, #54060, #123421, #109279, #189383, #206694, #205619, #141749, #25807, #43166, #208811, #77760, #176343, #27951, #94044, #95106, #207756, #174233, #111403, #91916, #124478, #160084, #58322, #11686, #75642, #143882, #157976, #74575, #110340, #59383, #191500, #60443, #139596, #90841, #125538, #209875, #175288, #140678, #9565, #26874, #92977, #159023, #126601, #61514, #127679, #193639, #190435, #45281, #177405, #42095, #29022, #108210, #8493, #173159, #161154, #156904, #12741, #57259, #41026, #107135, #24740, #114101, #180092, #81520, #147598, #53284, #37022, #121571, #123713, #189675, #103106, #41325, #137754, #70565, #72723, #54360, #107435, #205923, #187542, #185404, #39172, #38108, #136684, #173459, #170229, #55417, #156132, #120501, #4496, #57556, #104180, #5560, #169164, #20759, #87918, #25039, #91139, #119417, #40244, #21813, #203773, #202709, #186472, #152918, #23967, #153992, #71641, #105256, #157196, #188612, #138817, #140978, #86853, #171297, #22888, #89004, #155057, #204838, #6644, #56490, #122649, #74872, #106355, #172378, #90069, #7714, #73797, #139892 ),
 ( #8793, #193939, #43456, #160385, #112770, #192863, #176638, #174527, #191795, #208050, #28250, #129038, #61818, #142034, #124772, #125836, #75933, #210178, #26105, #93275, #178782, #58616, #46647, #127986, #30395, #80191, #45586, #96481, #111703, #177710, #175581, #27171, #195014, #162528, #190731, #14101, #42394, #9857, #59677, #44519, #110636, #145241, #79125, #29320, #206987, #211246, #109577, #159313, #108503, #10910, #92217, #76986, #143112, #94343, #95414, #161466, #78061, #209104, #62871, #60742, #126904, #144186, #11985, #158268, #13046, #132183, #199245, #149458, #67104, #83375, #184075, #213369, #117017, #183014, #114887, #198189, #64991, #34631, #49824, #98583, #115949, #100702, #1041, #166778, #18374, #66036, #148406, #181939, #33569, #16228, #97535, #99641, #197134, #131145, #133240, #47725, #165708, #84451, #50892, #101770, #17297, #19436, #150539, #196092, #35694, #167838, #15175, #2103, #68177, #180886, #134308, #200315, #51966, #48773, #214405, #118090, #32508, #163592, #146296, #164645, #82312, #130098, #113841, #212308, #63943, #179837, #31458, #81262, #147341, #169961, #20502, #102843, #185132, #56224, #4237, #54094, #36758, #89816, #6380, #104990, #173191, #85516, #203506, #168900, #121304, #103915, #171031, #55157, #53016, #70307, #107166, #154793, #22627, #135359, #88737, #57290, #120231, #122386, #172113, #69241, #187279, #201375, #152654, #151602, #87658, #186205, #38906, #72451, #23707, #188343, #39982, #106091, #41059, #153727, #37839, #123453, #21547, #136423, #155861, #202439, #7449, #5296, #73528, #71376, #86588, #138551, #137490, #204574, #139630, #3170, #205653, #189415, #119150, #93008, #25836, #43194, #60473, #126630, #26903, #192594, #159052, #12772, #59412, #91944, #77791, #29053, #75671, #95136, #158006, #108239, #58353, #141778, #42126, #174263, #142837, #62600, #9594, #74606, #11717, #208843, #112493, #207785, #24771, #8525, #10645, #161186, #78846, #140710, #144966, #109307, #125569, #44248, #191530, #210972, #177436, #76720, #156936, #110370, #175317, #176375, #143912, #27981, #94075, #160115, #209906, #124508, #61543, #127710, #193670, #190467, #128763, #45313, #111432, #90874, #206725, #194737, #46374, #214143, #196872, #197926, #148141, #146025, #97263, #200059, #33300, #49553, #13840, #115679, #150276, #147081, #767, #50623, #162254, #65769, #79916, #31190, #30114, #180620, #64734, #82048, #181673, #116749, #66833, #132976, #198978, #134051, #32244, #213103, #1846, #130878, #163317, #182748, #14899, #34366, #114629, #100440, #48509, #113566, #17034, #98315, #15964, #99385, #178504, #129831, #164380, #166511, #131916, #179571, #165437, #83111, #149192, #18102, #84189, #67905, #51710, #96204, #80993, #212035, #63677, #195814, #47451, #184875, #201115, #151341, #168640, #135101, #52756, #21298, #155605, #102579, #167579, #104730, #87404, #205397, #118891, #117830, #101509, #185944, #188085, #39715, #19178, #105823, #202179, #36501, #137234, #20242, #171849, #55968, #37577, #85253, #103659, #86328, #152399, #23444, #3978, #119967, #6119, #70047, #68983, #122121, #136161, #53836, #2910, #169708, #153469, #89554, #7189, #183821, #5042, #71118, #72187, #203256, #54899, #73262, #121052, #187018, #38651, #170777, #22366, #139366, #88479, #154538, #138296, #204311, #141532, #206471, #74355, #156680, #27733, #190218, #25586, #8272, #61300, #192344, #76474, #144729, #57036, #175070, #140459, #92760, #75420, #142585, #26657, #24512, #41877, #78607, #126384, #208593, #106910, #60225, #28804, #91697, #93827, #143665, #40803, #158804, #172935, #124259, #123203, #59160, #157750, #10401, #44002, #209659, #159868, #11472, #77543, #12535, #125318, #9348, #94889, #207540, #107988, #127462, #174016, #193433, #191277, #45077, #42944, #58100, #110121, #109052, #176133, #111186, #189164, #177189, #160941, #90622, #64500, #211799, #14664, #32007, #98089, #212864, #164142, #130642, #198732, #30954, #63435, #49327, #517, #47212, #66585, #129587, #79680, #29878, #113326, #13605, #145793, #114388, #34119, #195574, #46139, #197682, #180383, #83930, #179333, #210740, #194495, #196635, #132728 ) ),
 .UNSPECIFIED., .F., .F., .T. ) 
 B_SPLINE_SURFACE_WITH_KNOTS ( ( 2, 2 ),
 ( 3, 2, 2, 2, 2, 2, 2, 2, 2, 2, 2, 2, 2, 2, 2, 2, 2, 2, 2, 2, 2, 2, 2, 2, 2, 2, 2, 2, 2, 2, 2, 2, 2, 2, 2, 2, 2, 2, 2, 2, 2, 2, 2, 2, 2, 2, 2, 2, 2, 2, 2, 2, 2, 2, 2, 2, 2, 2, 2, 2, 2, 2, 2, 2, 2, 2, 2, 2, 2, 2, 2, 2, 2, 2, 2, 2, 2, 2, 2, 2, 2, 2, 2, 2, 2, 2, 2, 2, 2, 2, 2, 2, 2, 2, 2, 2, 2, 2, 2, 2, 2, 2, 2, 2, 2, 2, 2, 2, 2, 2, 2, 2, 2, 2, 2, 2, 2, 2, 2, 2, 2, 2, 2, 2, 2, 2, 2, 2, 2, 2, 2, 2, 2, 2, 2, 2, 2, 2, 2, 2, 2, 2, 2, 2, 2, 2, 2, 2, 2, 2, 2, 2, 2, 2, 2, 2, 2, 2, 2, 2, 2, 2, 2, 2, 2, 2, 2, 2, 2, 2, 2, 2, 2, 2, 2, 2, 2, 2, 2, 2, 2, 2, 2, 2, 2, 2, 2, 2, 2, 2, 2, 2, 2, 2, 2, 2, 2, 2, 2, 2, 2, 2, 2, 2, 2, 2, 2, 2, 2, 2, 2, 2, 2, 2, 2, 2, 2, 2, 2, 2, 2, 2, 2, 2, 2, 2, 2, 2, 2, 2, 2, 2, 2, 2, 2, 2, 2, 2, 2, 2, 3 ),
 ( 0.000000000000000000, 1.000000000000000000 ),
 ( 0.000000000000000000, 0.004166666666666666609, 0.008333333333333333218, 0.01250000000000000069, 0.01666666666666666644, 0.02083333333333333218, 0.02500000000000000139, 0.02916666666666666713, 0.03333333333333333287, 0.03749999999999999861, 0.04166666666666666435, 0.04583333333333333010, 0.05000000000000000278, 0.05416666666666666852, 0.05833333333333333426, 0.06250000000000000000, 0.06666666666666666574, 0.07083333333333333148, 0.07499999999999999722, 0.07916666666666666297, 0.08333333333333332871, 0.08749999999999999445, 0.09166666666666666019, 0.09583333333333333981, 0.1000000000000000056, 0.1041666666666666713, 0.1083333333333333370, 0.1125000000000000028, 0.1166666666666666685, 0.1208333333333333343, 0.1250000000000000000, 0.1291666666666666796, 0.1333333333333333315, 0.1375000000000000111, 0.1416666666666666630, 0.1458333333333333426, 0.1499999999999999944, 0.1541666666666666741, 0.1583333333333333259, 0.1625000000000000056, 0.1666666666666666574, 0.1708333333333333370, 0.1749999999999999889, 0.1791666666666666685, 0.1833333333333333204, 0.1875000000000000000, 0.1916666666666666796, 0.1958333333333333315, 0.2000000000000000111, 0.2041666666666666630, 0.2083333333333333426, 0.2124999999999999944, 0.2166666666666666741, 0.2208333333333333259, 0.2250000000000000056, 0.2291666666666666574, 0.2333333333333333370, 0.2374999999999999889, 0.2416666666666666685, 0.2458333333333333204, 0.2500000000000000000, 0.2541666666666666519, 0.2583333333333333592, 0.2625000000000000111, 0.2666666666666666630, 0.2708333333333333148, 0.2750000000000000222, 0.2791666666666666741, 0.2833333333333333259, 0.2874999999999999778, 0.2916666666666666852, 0.2958333333333333370, 0.2999999999999999889, 0.3041666666666666408, 0.3083333333333333481, 0.3125000000000000000, 0.3166666666666666519, 0.3208333333333333592, 0.3250000000000000111, 0.3291666666666666630, 0.3333333333333333148, 0.3375000000000000222, 0.3416666666666666741, 0.3458333333333333259, 0.3499999999999999778, 0.3541666666666666852, 0.3583333333333333370, 0.3624999999999999889, 0.3666666666666666408, 0.3708333333333333481, 0.3750000000000000000, 0.3791666666666666519, 0.3833333333333333592, 0.3875000000000000111, 0.3916666666666666630, 0.3958333333333333148, 0.4000000000000000222, 0.4041666666666666741, 0.4083333333333333259, 0.4124999999999999778, 0.4166666666666666852, 0.4208333333333333370, 0.4249999999999999889, 0.4291666666666666408, 0.4333333333333333481, 0.4375000000000000000, 0.4416666666666666519, 0.4458333333333333592, 0.4500000000000000111, 0.4541666666666666630, 0.4583333333333333148, 0.4625000000000000222, 0.4666666666666666741, 0.4708333333333333259, 0.4749999999999999778, 0.4791666666666666852, 0.4833333333333333370, 0.4874999999999999889, 0.4916666666666666408, 0.4958333333333333481, 0.5000000000000000000, 0.5041666666666666519, 0.5083333333333333037, 0.5124999999999999556, 0.5166666666666667185, 0.5208333333333333703, 0.5250000000000000222, 0.5291666666666666741, 0.5333333333333333259, 0.5374999999999999778, 0.5416666666666666297, 0.5458333333333332815, 0.5500000000000000444, 0.5541666666666666963, 0.5583333333333333481, 0.5625000000000000000, 0.5666666666666666519, 0.5708333333333333037, 0.5749999999999999556, 0.5791666666666667185, 0.5833333333333333703, 0.5875000000000000222, 0.5916666666666666741, 0.5958333333333333259, 0.5999999999999999778, 0.6041666666666666297, 0.6083333333333332815, 0.6125000000000000444, 0.6166666666666666963, 0.6208333333333333481, 0.6250000000000000000, 0.6291666666666666519, 0.6333333333333333037, 0.6374999999999999556, 0.6416666666666667185, 0.6458333333333333703, 0.6500000000000000222, 0.6541666666666666741, 0.6583333333333333259, 0.6624999999999999778, 0.6666666666666666297, 0.6708333333333332815, 0.6750000000000000444, 0.6791666666666666963, 0.6833333333333333481, 0.6875000000000000000, 0.6916666666666666519, 0.6958333333333333037, 0.6999999999999999556, 0.7041666666666667185, 0.7083333333333333703, 0.7125000000000000222, 0.7166666666666666741, 0.7208333333333333259, 0.7249999999999999778, 0.7291666666666666297, 0.7333333333333332815, 0.7375000000000000444, 0.7416666666666666963, 0.7458333333333333481, 0.7500000000000000000, 0.7541666666666666519, 0.7583333333333333037, 0.7624999999999999556, 0.7666666666666667185, 0.7708333333333333703, 0.7750000000000000222, 0.7791666666666666741, 0.7833333333333333259, 0.7874999999999999778, 0.7916666666666666297, 0.7958333333333332815, 0.8000000000000000444, 0.8041666666666666963, 0.8083333333333333481, 0.8125000000000000000, 0.8166666666666666519, 0.8208333333333333037, 0.8249999999999999556, 0.8291666666666667185, 0.8333333333333333703, 0.8375000000000000222, 0.8416666666666666741, 0.8458333333333333259, 0.8499999999999999778, 0.8541666666666666297, 0.8583333333333332815, 0.8625000000000000444, 0.8666666666666666963, 0.8708333333333333481, 0.8750000000000000000, 0.8791666666666666519, 0.8833333333333333037, 0.8874999999999999556, 0.8916666666666667185, 0.8958333333333333703, 0.9000000000000000222, 0.9041666666666666741, 0.9083333333333333259, 0.9124999999999999778, 0.9166666666666666297, 0.9208333333333332815, 0.9250000000000000444, 0.9291666666666666963, 0.9333333333333333481, 0.9375000000000000000, 0.9416666666666666519, 0.9458333333333333037, 0.9499999999999999556, 0.9541666666666667185, 0.9583333333333333703, 0.9625000000000000222, 0.9666666666666666741, 0.9708333333333333259, 0.9749999999999999778, 0.9791666666666666297, 0.9833333333333332815, 0.9875000000000000444, 0.9916666666666666963, 0.9958333333333333481, 1.000000000000000000 ),
 .UNSPECIFIED. ) 
 GEOMETRIC_REPRESENTATION_ITEM ( )  RATIONAL_B_SPLINE_SURFACE ( (
 ( 1.000000000000000000, 0.8660254037844387076, 1.000000000000000000, 0.8660254037844387076, 1.000000000000000000, 0.8660254037844387076, 1.000000000000000000, 0.8660254037844387076, 1.000000000000000000, 0.8660254037844387076, 1.000000000000000000, 0.8660254037844387076, 1.000000000000000000, 0.8660254037844387076, 1.000000000000000000, 0.8660254037844387076, 1.000000000000000000, 0.8660254037844387076, 1.000000000000000000, 0.8660254037844387076, 1.000000000000000000, 0.8660254037844387076, 1.000000000000000000, 0.8660254037844387076, 1.000000000000000000, 0.8660254037844387076, 1.000000000000000000, 0.8660254037844387076, 1.000000000000000000, 0.8660254037844387076, 1.000000000000000000, 0.8660254037844387076, 1.000000000000000000, 0.8660254037844387076, 1.000000000000000000, 0.8660254037844387076, 1.000000000000000000, 0.8660254037844387076, 1.000000000000000000, 0.8660254037844387076, 1.000000000000000000, 0.8660254037844387076, 1.000000000000000000, 0.8660254037844387076, 1.000000000000000000, 0.8660254037844387076, 1.000000000000000000, 0.8660254037844387076, 1.000000000000000000, 0.8660254037844387076, 1.000000000000000000, 0.8660254037844387076, 1.000000000000000000, 0.8660254037844387076, 1.000000000000000000, 0.8660254037844387076, 1.000000000000000000, 0.8660254037844387076, 1.000000000000000000, 0.8660254037844387076, 1.000000000000000000, 0.8660254037844387076, 1.000000000000000000, 0.8660254037844387076, 1.000000000000000000, 0.8660254037844387076, 1.000000000000000000, 0.8660254037844387076, 1.000000000000000000, 0.8660254037844387076, 1.000000000000000000, 0.8660254037844387076, 1.000000000000000000, 0.8660254037844387076, 1.000000000000000000, 0.8660254037844387076, 1.000000000000000000, 0.8660254037844387076, 1.000000000000000000, 0.8660254037844387076, 1.000000000000000000, 0.8660254037844387076, 1.000000000000000000, 0.8660254037844387076, 1.000000000000000000, 0.8660254037844387076, 1.000000000000000000, 0.8660254037844387076, 1.000000000000000000, 0.8660254037844387076, 1.000000000000000000, 0.8660254037844387076, 1.000000000000000000, 0.8660254037844387076, 1.000000000000000000, 0.8660254037844387076, 1.000000000000000000, 0.8660254037844387076, 1.000000000000000000, 0.8660254037844387076, 1.000000000000000000, 0.8660254037844387076, 1.000000000000000000, 0.8660254037844387076, 1.000000000000000000, 0.8660254037844387076, 1.000000000000000000, 0.8660254037844387076, 1.000000000000000000, 0.8660254037844387076, 1.000000000000000000, 0.8660254037844387076, 1.000000000000000000, 0.8660254037844387076, 1.000000000000000000, 0.8660254037844387076, 1.000000000000000000, 0.8660254037844387076, 1.000000000000000000, 0.8660254037844387076, 1.000000000000000000, 0.8660254037844387076, 1.000000000000000000, 0.8660254037844387076, 1.000000000000000000, 0.8660254037844387076, 1.000000000000000000, 0.8660254037844387076, 1.000000000000000000, 0.8660254037844387076, 1.000000000000000000, 0.8660254037844387076, 1.000000000000000000, 0.8660254037844387076, 1.000000000000000000, 0.8660254037844387076, 1.000000000000000000, 0.8660254037844387076, 1.000000000000000000, 0.8660254037844387076, 1.000000000000000000, 0.8660254037844387076, 1.000000000000000000, 0.8660254037844387076, 1.000000000000000000, 0.8660254037844387076, 1.000000000000000000, 0.8660254037844387076, 1.000000000000000000, 0.8660254037844387076, 1.000000000000000000, 0.8660254037844387076, 1.000000000000000000, 0.8660254037844387076, 1.000000000000000000, 0.8660254037844387076, 1.000000000000000000, 0.8660254037844387076, 1.000000000000000000, 0.8660254037844387076, 1.000000000000000000, 0.8660254037844387076, 1.000000000000000000, 0.8660254037844387076, 1.000000000000000000, 0.8660254037844387076, 1.000000000000000000, 0.8660254037844387076, 1.000000000000000000, 0.8660254037844387076, 1.000000000000000000, 0.8660254037844387076, 1.000000000000000000, 0.8660254037844387076, 1.000000000000000000, 0.8660254037844387076, 1.000000000000000000, 0.8660254037844387076, 1.000000000000000000, 0.8660254037844387076, 1.000000000000000000, 0.8660254037844387076, 1.000000000000000000, 0.8660254037844387076, 1.000000000000000000, 0.8660254037844387076, 1.000000000000000000, 0.8660254037844387076, 1.000000000000000000, 0.8660254037844387076, 1.000000000000000000, 0.8660254037844387076, 1.000000000000000000, 0.8660254037844387076, 1.000000000000000000, 0.8660254037844387076, 1.000000000000000000, 0.8660254037844387076, 1.000000000000000000, 0.8660254037844387076, 1.000000000000000000, 0.8660254037844387076, 1.000000000000000000, 0.8660254037844387076, 1.000000000000000000, 0.8660254037844387076, 1.000000000000000000, 0.8660254037844387076, 1.000000000000000000, 0.8660254037844387076, 1.000000000000000000, 0.8660254037844387076, 1.000000000000000000, 0.8660254037844387076, 1.000000000000000000, 0.8660254037844387076, 1.000000000000000000, 0.8660254037844387076, 1.000000000000000000, 0.8660254037844387076, 1.000000000000000000, 0.8660254037844387076, 1.000000000000000000, 0.8660254037844387076, 1.000000000000000000, 0.8660254037844387076, 1.000000000000000000, 0.8660254037844387076, 1.000000000000000000, 0.8660254037844387076, 1.000000000000000000, 0.8660254037844387076, 1.000000000000000000, 0.8660254037844387076, 1.000000000000000000, 0.8660254037844387076, 1.000000000000000000, 0.8660254037844387076, 1.000000000000000000, 0.8660254037844387076, 1.000000000000000000, 0.8660254037844387076, 1.000000000000000000, 0.8660254037844387076, 1.000000000000000000, 0.8660254037844387076, 1.000000000000000000, 0.8660254037844387076, 1.000000000000000000, 0.8660254037844387076, 1.000000000000000000, 0.8660254037844387076, 1.000000000000000000, 0.8660254037844387076, 1.000000000000000000, 0.8660254037844387076, 1.000000000000000000, 0.8660254037844387076, 1.000000000000000000, 0.8660254037844387076, 1.000000000000000000, 0.8660254037844387076, 1.000000000000000000, 0.8660254037844387076, 1.000000000000000000, 0.8660254037844387076, 1.000000000000000000, 0.8660254037844387076, 1.000000000000000000, 0.8660254037844387076, 1.000000000000000000, 0.8660254037844387076, 1.000000000000000000, 0.8660254037844387076, 1.000000000000000000, 0.8660254037844387076, 1.000000000000000000, 0.8660254037844387076, 1.000000000000000000, 0.8660254037844387076, 1.000000000000000000, 0.8660254037844387076, 1.000000000000000000, 0.8660254037844387076, 1.000000000000000000, 0.8660254037844387076, 1.000000000000000000, 0.8660254037844387076, 1.000000000000000000, 0.8660254037844387076, 1.000000000000000000, 0.8660254037844387076, 1.000000000000000000, 0.8660254037844387076, 1.000000000000000000, 0.8660254037844387076, 1.000000000000000000, 0.8660254037844387076, 1.000000000000000000, 0.8660254037844387076, 1.000000000000000000, 0.8660254037844387076, 1.000000000000000000, 0.8660254037844387076, 1.000000000000000000, 0.8660254037844387076, 1.000000000000000000, 0.8660254037844387076, 1.000000000000000000, 0.8660254037844387076, 1.000000000000000000, 0.8660254037844387076, 1.000000000000000000, 0.8660254037844387076, 1.000000000000000000, 0.8660254037844387076, 1.000000000000000000, 0.8660254037844387076, 1.000000000000000000, 0.8660254037844387076, 1.000000000000000000, 0.8660254037844387076, 1.000000000000000000, 0.8660254037844387076, 1.000000000000000000, 0.8660254037844387076, 1.000000000000000000, 0.8660254037844387076, 1.000000000000000000, 0.8660254037844387076, 1.000000000000000000, 0.8660254037844387076, 1.000000000000000000, 0.8660254037844387076, 1.000000000000000000, 0.8660254037844387076, 1.000000000000000000, 0.8660254037844387076, 1.000000000000000000, 0.8660254037844387076, 1.000000000000000000, 0.8660254037844387076, 1.000000000000000000, 0.8660254037844387076, 1.000000000000000000, 0.8660254037844387076, 1.000000000000000000, 0.8660254037844387076, 1.000000000000000000, 0.8660254037844387076, 1.000000000000000000, 0.8660254037844387076, 1.000000000000000000, 0.8660254037844387076, 1.000000000000000000, 0.8660254037844387076, 1.000000000000000000, 0.8660254037844387076, 1.000000000000000000, 0.8660254037844387076, 1.000000000000000000, 0.8660254037844387076, 1.000000000000000000, 0.8660254037844387076, 1.000000000000000000, 0.8660254037844387076, 1.000000000000000000, 0.8660254037844387076, 1.000000000000000000, 0.8660254037844387076, 1.000000000000000000, 0.8660254037844387076, 1.000000000000000000, 0.8660254037844387076, 1.000000000000000000, 0.8660254037844387076, 1.000000000000000000, 0.8660254037844387076, 1.000000000000000000, 0.8660254037844387076, 1.000000000000000000, 0.8660254037844387076, 1.000000000000000000, 0.8660254037844387076, 1.000000000000000000, 0.8660254037844387076, 1.000000000000000000, 0.8660254037844387076, 1.000000000000000000, 0.8660254037844387076, 1.000000000000000000, 0.8660254037844387076, 1.000000000000000000, 0.8660254037844387076, 1.000000000000000000, 0.8660254037844387076, 1.000000000000000000, 0.8660254037844387076, 1.000000000000000000, 0.8660254037844387076, 1.000000000000000000, 0.8660254037844387076, 1.000000000000000000, 0.8660254037844387076, 1.000000000000000000, 0.8660254037844387076, 1.000000000000000000, 0.8660254037844387076, 1.000000000000000000, 0.8660254037844387076, 1.000000000000000000, 0.8660254037844387076, 1.000000000000000000, 0.8660254037844387076, 1.000000000000000000, 0.8660254037844387076, 1.000000000000000000, 0.8660254037844387076, 1.000000000000000000, 0.8660254037844387076, 1.000000000000000000, 0.8660254037844387076, 1.000000000000000000, 0.8660254037844387076, 1.000000000000000000, 0.8660254037844387076, 1.000000000000000000, 0.8660254037844387076, 1.000000000000000000, 0.8660254037844387076, 1.000000000000000000, 0.8660254037844387076, 1.000000000000000000, 0.8660254037844387076, 1.000000000000000000, 0.8660254037844387076, 1.000000000000000000, 0.8660254037844387076, 1.000000000000000000, 0.8660254037844387076, 1.000000000000000000, 0.8660254037844387076, 1.000000000000000000, 0.8660254037844387076, 1.000000000000000000, 0.8660254037844387076, 1.000000000000000000, 0.8660254037844387076, 1.000000000000000000, 0.8660254037844387076, 1.000000000000000000, 0.8660254037844387076, 1.000000000000000000, 0.8660254037844387076, 1.000000000000000000, 0.8660254037844387076, 1.000000000000000000, 0.8660254037844387076, 1.000000000000000000, 0.8660254037844387076, 1.000000000000000000, 0.8660254037844387076, 1.000000000000000000, 0.8660254037844387076, 1.000000000000000000, 0.8660254037844387076, 1.000000000000000000, 0.8660254037844387076, 1.000000000000000000, 0.8660254037844387076, 1.000000000000000000, 0.8660254037844387076, 1.000000000000000000, 0.8660254037844387076, 1.000000000000000000, 0.8660254037844387076, 1.000000000000000000, 0.8660254037844387076, 1.000000000000000000, 0.8660254037844387076, 1.000000000000000000),
 ( 1.000000000000000000, 0.8660254037844387076, 1.000000000000000000, 0.8660254037844387076, 1.000000000000000000, 0.8660254037844387076, 1.000000000000000000, 0.8660254037844387076, 1.000000000000000000, 0.8660254037844387076, 1.000000000000000000, 0.8660254037844387076, 1.000000000000000000, 0.8660254037844387076, 1.000000000000000000, 0.8660254037844387076, 1.000000000000000000, 0.8660254037844387076, 1.000000000000000000, 0.8660254037844387076, 1.000000000000000000, 0.8660254037844387076, 1.000000000000000000, 0.8660254037844387076, 1.000000000000000000, 0.8660254037844387076, 1.000000000000000000, 0.8660254037844387076, 1.000000000000000000, 0.8660254037844387076, 1.000000000000000000, 0.8660254037844387076, 1.000000000000000000, 0.8660254037844387076, 1.000000000000000000, 0.8660254037844387076, 1.000000000000000000, 0.8660254037844387076, 1.000000000000000000, 0.8660254037844387076, 1.000000000000000000, 0.8660254037844387076, 1.000000000000000000, 0.8660254037844387076, 1.000000000000000000, 0.8660254037844387076, 1.000000000000000000, 0.8660254037844387076, 1.000000000000000000, 0.8660254037844387076, 1.000000000000000000, 0.8660254037844387076, 1.000000000000000000, 0.8660254037844387076, 1.000000000000000000, 0.8660254037844387076, 1.000000000000000000, 0.8660254037844387076, 1.000000000000000000, 0.8660254037844387076, 1.000000000000000000, 0.8660254037844387076, 1.000000000000000000, 0.8660254037844387076, 1.000000000000000000, 0.8660254037844387076, 1.000000000000000000, 0.8660254037844387076, 1.000000000000000000, 0.8660254037844387076, 1.000000000000000000, 0.8660254037844387076, 1.000000000000000000, 0.8660254037844387076, 1.000000000000000000, 0.8660254037844387076, 1.000000000000000000, 0.8660254037844387076, 1.000000000000000000, 0.8660254037844387076, 1.000000000000000000, 0.8660254037844387076, 1.000000000000000000, 0.8660254037844387076, 1.000000000000000000, 0.8660254037844387076, 1.000000000000000000, 0.8660254037844387076, 1.000000000000000000, 0.8660254037844387076, 1.000000000000000000, 0.8660254037844387076, 1.000000000000000000, 0.8660254037844387076, 1.000000000000000000, 0.8660254037844387076, 1.000000000000000000, 0.8660254037844387076, 1.000000000000000000, 0.8660254037844387076, 1.000000000000000000, 0.8660254037844387076, 1.000000000000000000, 0.8660254037844387076, 1.000000000000000000, 0.8660254037844387076, 1.000000000000000000, 0.8660254037844387076, 1.000000000000000000, 0.8660254037844387076, 1.000000000000000000, 0.8660254037844387076, 1.000000000000000000, 0.8660254037844387076, 1.000000000000000000, 0.8660254037844387076, 1.000000000000000000, 0.8660254037844387076, 1.000000000000000000, 0.8660254037844387076, 1.000000000000000000, 0.8660254037844387076, 1.000000000000000000, 0.8660254037844387076, 1.000000000000000000, 0.8660254037844387076, 1.000000000000000000, 0.8660254037844387076, 1.000000000000000000, 0.8660254037844387076, 1.000000000000000000, 0.8660254037844387076, 1.000000000000000000, 0.8660254037844387076, 1.000000000000000000, 0.8660254037844387076, 1.000000000000000000, 0.8660254037844387076, 1.000000000000000000, 0.8660254037844387076, 1.000000000000000000, 0.8660254037844387076, 1.000000000000000000, 0.8660254037844387076, 1.000000000000000000, 0.8660254037844387076, 1.000000000000000000, 0.8660254037844387076, 1.000000000000000000, 0.8660254037844387076, 1.000000000000000000, 0.8660254037844387076, 1.000000000000000000, 0.8660254037844387076, 1.000000000000000000, 0.8660254037844387076, 1.000000000000000000, 0.8660254037844387076, 1.000000000000000000, 0.8660254037844387076, 1.000000000000000000, 0.8660254037844387076, 1.000000000000000000, 0.8660254037844387076, 1.000000000000000000, 0.8660254037844387076, 1.000000000000000000, 0.8660254037844387076, 1.000000000000000000, 0.8660254037844387076, 1.000000000000000000, 0.8660254037844387076, 1.000000000000000000, 0.8660254037844387076, 1.000000000000000000, 0.8660254037844387076, 1.000000000000000000, 0.8660254037844387076, 1.000000000000000000, 0.8660254037844387076, 1.000000000000000000, 0.8660254037844387076, 1.000000000000000000, 0.8660254037844387076, 1.000000000000000000, 0.8660254037844387076, 1.000000000000000000, 0.8660254037844387076, 1.000000000000000000, 0.8660254037844387076, 1.000000000000000000, 0.8660254037844387076, 1.000000000000000000, 0.8660254037844387076, 1.000000000000000000, 0.8660254037844387076, 1.000000000000000000, 0.8660254037844387076, 1.000000000000000000, 0.8660254037844387076, 1.000000000000000000, 0.8660254037844387076, 1.000000000000000000, 0.8660254037844387076, 1.000000000000000000, 0.8660254037844387076, 1.000000000000000000, 0.8660254037844387076, 1.000000000000000000, 0.8660254037844387076, 1.000000000000000000, 0.8660254037844387076, 1.000000000000000000, 0.8660254037844387076, 1.000000000000000000, 0.8660254037844387076, 1.000000000000000000, 0.8660254037844387076, 1.000000000000000000, 0.8660254037844387076, 1.000000000000000000, 0.8660254037844387076, 1.000000000000000000, 0.8660254037844387076, 1.000000000000000000, 0.8660254037844387076, 1.000000000000000000, 0.8660254037844387076, 1.000000000000000000, 0.8660254037844387076, 1.000000000000000000, 0.8660254037844387076, 1.000000000000000000, 0.8660254037844387076, 1.000000000000000000, 0.8660254037844387076, 1.000000000000000000, 0.8660254037844387076, 1.000000000000000000, 0.8660254037844387076, 1.000000000000000000, 0.8660254037844387076, 1.000000000000000000, 0.8660254037844387076, 1.000000000000000000, 0.8660254037844387076, 1.000000000000000000, 0.8660254037844387076, 1.000000000000000000, 0.8660254037844387076, 1.000000000000000000, 0.8660254037844387076, 1.000000000000000000, 0.8660254037844387076, 1.000000000000000000, 0.8660254037844387076, 1.000000000000000000, 0.8660254037844387076, 1.000000000000000000, 0.8660254037844387076, 1.000000000000000000, 0.8660254037844387076, 1.000000000000000000, 0.8660254037844387076, 1.000000000000000000, 0.8660254037844387076, 1.000000000000000000, 0.8660254037844387076, 1.000000000000000000, 0.8660254037844387076, 1.000000000000000000, 0.8660254037844387076, 1.000000000000000000, 0.8660254037844387076, 1.000000000000000000, 0.8660254037844387076, 1.000000000000000000, 0.8660254037844387076, 1.000000000000000000, 0.8660254037844387076, 1.000000000000000000, 0.8660254037844387076, 1.000000000000000000, 0.8660254037844387076, 1.000000000000000000, 0.8660254037844387076, 1.000000000000000000, 0.8660254037844387076, 1.000000000000000000, 0.8660254037844387076, 1.000000000000000000, 0.8660254037844387076, 1.000000000000000000, 0.8660254037844387076, 1.000000000000000000, 0.8660254037844387076, 1.000000000000000000, 0.8660254037844387076, 1.000000000000000000, 0.8660254037844387076, 1.000000000000000000, 0.8660254037844387076, 1.000000000000000000, 0.8660254037844387076, 1.000000000000000000, 0.8660254037844387076, 1.000000000000000000, 0.8660254037844387076, 1.000000000000000000, 0.8660254037844387076, 1.000000000000000000, 0.8660254037844387076, 1.000000000000000000, 0.8660254037844387076, 1.000000000000000000, 0.8660254037844387076, 1.000000000000000000, 0.8660254037844387076, 1.000000000000000000, 0.8660254037844387076, 1.000000000000000000, 0.8660254037844387076, 1.000000000000000000, 0.8660254037844387076, 1.000000000000000000, 0.8660254037844387076, 1.000000000000000000, 0.8660254037844387076, 1.000000000000000000, 0.8660254037844387076, 1.000000000000000000, 0.8660254037844387076, 1.000000000000000000, 0.8660254037844387076, 1.000000000000000000, 0.8660254037844387076, 1.000000000000000000, 0.8660254037844387076, 1.000000000000000000, 0.8660254037844387076, 1.000000000000000000, 0.8660254037844387076, 1.000000000000000000, 0.8660254037844387076, 1.000000000000000000, 0.8660254037844387076, 1.000000000000000000, 0.8660254037844387076, 1.000000000000000000, 0.8660254037844387076, 1.000000000000000000, 0.8660254037844387076, 1.000000000000000000, 0.8660254037844387076, 1.000000000000000000, 0.8660254037844387076, 1.000000000000000000, 0.8660254037844387076, 1.000000000000000000, 0.8660254037844387076, 1.000000000000000000, 0.8660254037844387076, 1.000000000000000000, 0.8660254037844387076, 1.000000000000000000, 0.8660254037844387076, 1.000000000000000000, 0.8660254037844387076, 1.000000000000000000, 0.8660254037844387076, 1.000000000000000000, 0.8660254037844387076, 1.000000000000000000, 0.8660254037844387076, 1.000000000000000000, 0.8660254037844387076, 1.000000000000000000, 0.8660254037844387076, 1.000000000000000000, 0.8660254037844387076, 1.000000000000000000, 0.8660254037844387076, 1.000000000000000000, 0.8660254037844387076, 1.000000000000000000, 0.8660254037844387076, 1.000000000000000000, 0.8660254037844387076, 1.000000000000000000, 0.8660254037844387076, 1.000000000000000000, 0.8660254037844387076, 1.000000000000000000, 0.8660254037844387076, 1.000000000000000000, 0.8660254037844387076, 1.000000000000000000, 0.8660254037844387076, 1.000000000000000000, 0.8660254037844387076, 1.000000000000000000, 0.8660254037844387076, 1.000000000000000000, 0.8660254037844387076, 1.000000000000000000, 0.8660254037844387076, 1.000000000000000000, 0.8660254037844387076, 1.000000000000000000, 0.8660254037844387076, 1.000000000000000000, 0.8660254037844387076, 1.000000000000000000, 0.8660254037844387076, 1.000000000000000000, 0.8660254037844387076, 1.000000000000000000, 0.8660254037844387076, 1.000000000000000000, 0.8660254037844387076, 1.000000000000000000, 0.8660254037844387076, 1.000000000000000000, 0.8660254037844387076, 1.000000000000000000, 0.8660254037844387076, 1.000000000000000000, 0.8660254037844387076, 1.000000000000000000, 0.8660254037844387076, 1.000000000000000000, 0.8660254037844387076, 1.000000000000000000, 0.8660254037844387076, 1.000000000000000000, 0.8660254037844387076, 1.000000000000000000, 0.8660254037844387076, 1.000000000000000000, 0.8660254037844387076, 1.000000000000000000, 0.8660254037844387076, 1.000000000000000000, 0.8660254037844387076, 1.000000000000000000, 0.8660254037844387076, 1.000000000000000000, 0.8660254037844387076, 1.000000000000000000, 0.8660254037844387076, 1.000000000000000000, 0.8660254037844387076, 1.000000000000000000, 0.8660254037844387076, 1.000000000000000000, 0.8660254037844387076, 1.000000000000000000, 0.8660254037844387076, 1.000000000000000000, 0.8660254037844387076, 1.000000000000000000, 0.8660254037844387076, 1.000000000000000000, 0.8660254037844387076, 1.000000000000000000, 0.8660254037844387076, 1.000000000000000000, 0.8660254037844387076, 1.000000000000000000, 0.8660254037844387076, 1.000000000000000000, 0.8660254037844387076, 1.000000000000000000, 0.8660254037844387076, 1.000000000000000000, 0.8660254037844387076, 1.000000000000000000, 0.8660254037844387076, 1.000000000000000000, 0.8660254037844387076, 1.000000000000000000) ) ) 
 REPRESENTATION_ITEM ( '' )  SURFACE ( )  );
#122746 = CARTESIAN_POINT ( 'NONE',  ( 1.499999999999989120, 2.556250000682817713, 1.214306433183764966E-14 ) ) ;
#122747 = CARTESIAN_POINT ( 'NONE',  ( 1.219610691686360049, -1.880083933147856934, 0.4191893400790832613 ) ) ;
#122748 = CARTESIAN_POINT ( 'NONE',  ( -0.6823417656250039265, 14.06770833367473195, -1.181850606188755259 ) ) ;
#122749 = CARTESIAN_POINT ( 'NONE',  ( 4.060924178622978609, 0.5945426864985210447, 2.140278595106285042 ) ) ;
#122750 = ORIENTED_EDGE ( 'NONE', *, *, #33691, .T. ) ;
#122751 = CARTESIAN_POINT ( 'NONE',  ( 0.6124999999999793943, 2.479166667349472331, -1.060881119635965764 ) ) ;
#122752 = CARTESIAN_POINT ( 'NONE',  ( 0.7499999999999867883, -0.1833333333333131421, -1.299038105676652899 ) ) ;
#122753 = CARTESIAN_POINT ( 'NONE',  ( 8.274553823041976841, 8.548067636504127265, 1.040834085586084257E-14 ) ) ;
#122754 = CARTESIAN_POINT ( 'NONE',  ( 0.6823417656249882723, 0.1760416670080894308, -1.181850606188749264 ) ) ;
#122755 = EDGE_CURVE ( 'NONE', #58812, #1871, #109318, .T. ) ;
#122756 = CARTESIAN_POINT ( 'NONE',  ( 0.6279475770487872310, -0.3202071342675495425, 2.197987568497254074 ) ) ;
#122757 = CARTESIAN_POINT ( 'NONE',  ( 4.861744986159981075, -0.5251177144562025889, 1.890194517805739771 ) ) ;
#122758 = CARTESIAN_POINT ( 'NONE',  ( 8.093854517678360949, 12.38665467069271386, 1.040834085586084257E-14 ) ) ;
#122759 = EDGE_CURVE ( 'NONE', #67094, #5587, #63110, .T. ) ;
#122760 = CARTESIAN_POINT ( 'NONE',  ( -1.355680771150862052, 3.764352529171857142, -0.6419739358886606961 ) ) ;
#122761 = CARTESIAN_POINT ( 'NONE',  ( 5.483742561420515749, 1.513553928502100465, 1.681752807289581986 ) ) ;
#122762 = CLOSED_SHELL ( 'NONE', ( #116185, #189849, #153001, #68577, #74162, #52834, #133317, #164766, #28088, #42907, #65210, #3770, #171652, #69891, #7540, #125806, #3603, #197146, #187447, #72771, #69625 ) ) ;
#122763 = CARTESIAN_POINT ( 'NONE',  ( -4.665414256878301025, 6.536345614481700927, -1.443375672974066548 ) ) ;
#122764 = CARTESIAN_POINT ( 'NONE',  ( 2.945816691342293847, 1.456820166381930015, 1.460492231956188824 ) ) ;
#122765 = CARTESIAN_POINT ( 'NONE',  ( -6.728924311084075960, 6.744833205886536120, 1.040834085586084257E-14 ) ) ;
#122766 = CARTESIAN_POINT ( 'NONE',  ( 1.499999999999987121, 2.577083334016147198, -0.8660254037844262731 ) ) ;
#122767 = CARTESIAN_POINT ( 'NONE',  ( -1.364683531250012516, 4.801041667008083991, -0.7879004041258300672 ) ) ;
#122768 = CARTESIAN_POINT ( 'NONE',  ( 4.587079231881330266, 1.671727914585485530, -0.8392916717318499309 ) ) ;
#122769 = CARTESIAN_POINT ( 'NONE',  ( 3.287501071874948000, 1.364548152031169082, -1.070007228145404943 ) ) ;
#122770 = CARTESIAN_POINT ( 'NONE',  ( 3.368457041919175055, 0.03905506635776007096, -1.740168019110074793 ) ) ;
#122771 = CARTESIAN_POINT ( 'NONE',  ( 0.6094042559229868594, -0.3290114652876909296, 2.268531362689259812 ) ) ;
#122772 = CARTESIAN_POINT ( 'NONE',  ( 1.290363523627102049, -0.9912053058820711193, 1.971723787660728977 ) ) ;
#122773 = CARTESIAN_POINT ( 'NONE',  ( 4.564062515778636531, -1.364536961465147913, 1.584173057036510013 ) ) ;
#122774 = CARTESIAN_POINT ( 'NONE',  ( 5.841732304440537149, 1.939831336911639781, 0.09320031894976579800 ) ) ;
#122776 = ORIENTED_EDGE ( 'NONE', *, *, #108161, .F. ) ;
#122775 = DIRECTION ( 'NONE',  ( 0.000000000000000000, 0.000000000000000000, 1.000000000000000000 ) ) ;
#122777 = CARTESIAN_POINT ( 'NONE',  ( 0.4400775573648734174, -1.704940109561555950, -1.076314675215600314 ) ) ;
#122778 = CARTESIAN_POINT ( 'NONE',  ( 1.090261293813089560, 1.267680250814690934, 1.699812782343253170 ) ) ;
#122779 = CARTESIAN_POINT ( 'NONE',  ( -11.89197369110780045, 12.30000000000000604, -0.8056055387119882560 ) ) ;
#122780 = CARTESIAN_POINT ( 'NONE',  ( -7.980945979938748103, 12.46285407657057220, 0.000000000000000000 ) ) ;
#122781 = CARTESIAN_POINT ( 'NONE',  ( 8.118635056484817980, 8.366162408854107113, 0.7998128361456481317 ) ) ;
#122782 = LINE ( 'NONE', #155189, #94482 ) ;
#122783 = CARTESIAN_POINT ( 'NONE',  ( 4.019992336727182369, -0.9402185374879183932, -1.564826772493657536 ) ) ;
#122784 = ORIENTED_EDGE ( 'NONE', *, *, #64259, .F. ) ;
#122785 = CARTESIAN_POINT ( 'NONE',  ( -7.014364370223741929, 9.276787413384745662, -1.599625672291271394 ) ) ;
#122786 = MECHANICAL_DESIGN_GEOMETRIC_PRESENTATION_REPRESENTATION (  '', ( #91471 ), #25736 ) ;
#122787 = CARTESIAN_POINT ( 'NONE',  ( -2.844178363816758814, 6.540234867753325076, -0.7998128361456481317 ) ) ;
#122788 = CARTESIAN_POINT ( 'NONE',  ( 3.285556943750000070, -2.121874999522044281, 0.000000000000000000 ) ) ;
#122789 = CARTESIAN_POINT ( 'NONE',  ( -6.561256274009600986, 9.742217188731485678, -1.199719254218440723 ) ) ;
#122790 = CARTESIAN_POINT ( 'NONE',  ( 2.197526642425628118, 1.844980167888200961, -0.8223984085018556378 ) ) ;
#122791 = CARTESIAN_POINT ( 'NONE',  ( 6.176841753231244958, -2.093540797633717254, -0.6980159708611932690 ) ) ;
#122792 = CARTESIAN_POINT ( 'NONE',  ( -4.930325137224961907, 5.781076077297750970, -1.199719254218453823 ) ) ;
#122793 = ADVANCED_FACE ( 'NONE', ( #162929 ), #27576, .T. ) ;
#122794 = CARTESIAN_POINT ( 'NONE',  ( 2.781907013001069906, -1.067198605185412763, -1.524341717138616215 ) ) ;
#122795 = CARTESIAN_POINT ( 'NONE',  ( 2.544126380858701797, 6.119897877643793116, 0.7998128361456462443 ) ) ;
#122796 = DIRECTION ( 'NONE',  ( 0.000000000000000000, 0.000000000000000000, -1.000000000000000000 ) ) ;
#122797 = ORIENTED_EDGE ( 'NONE', *, *, #127726, .T. ) ;
#122798 = CARTESIAN_POINT ( 'NONE',  ( -4.066556009095094737, 6.831733546331167695, 1.199719254218464037 ) ) ;
#122799 = CARTESIAN_POINT ( 'NONE',  ( -7.486073373039941359, 11.88550270185529278, -0.7998128361456291469 ) ) ;
#122800 = CARTESIAN_POINT ( 'NONE',  ( 5.461492464141177727, 0.3521552718798379722, -1.791230276788812414 ) ) ;
#122802 = CARTESIAN_POINT ( 'NONE',  ( -3.992976280936286759, 7.825322551632388546, 0.2949607357299148802 ) ) ;
#122801 = CARTESIAN_POINT ( 'NONE',  ( -4.492547798081878874, 6.334668079219206049, 1.599625672291263179 ) ) ;
#122803 = CARTESIAN_POINT ( 'NONE',  ( 6.435676556713933572, 6.878741676577107889, -0.7109887800627444632 ) ) ;
#122804 = CARTESIAN_POINT ( 'NONE',  ( 0.2273701076888709205, -1.544753302685021534, -0.7874640570253422789 ) ) ;
#122805 = CARTESIAN_POINT ( 'NONE',  ( 0.2689661900789627746, 0.9977586965290600185, 1.425695987021274647 ) ) ;
#122806 = CARTESIAN_POINT ( 'NONE',  ( 5.268348002110199602, 1.133478272989609348, 2.010090980756351176 ) ) ;
#122807 = CARTESIAN_POINT ( 'NONE',  ( 3.881377115262159894, 7.750300077773022878, 0.7998128361456271485 ) ) ;
#122808 = CARTESIAN_POINT ( 'NONE',  ( 0.7025034608351670151, -0.6919086601019829308, -1.941309234904058600 ) ) ;
#122809 = CARTESIAN_POINT ( 'NONE',  ( 6.681470773436232413, 6.689470745297396270, -0.7998128361456281477 ) ) ;
#122810 = CARTESIAN_POINT ( 'NONE',  ( 6.011119390975155241, 2.295276066174879670, 0.1220560631845988148 ) ) ;
#122811 = CARTESIAN_POINT ( 'NONE',  ( 4.183485216215318658, 3.563207579971337413, 2.499999999999998668 ) ) ;
#122813 = AXIS2_PLACEMENT_3D ( 'NONE', #34478, #52870, #200165 ) ;
#122812 = CARTESIAN_POINT ( 'NONE',  ( -6.099189001301292379, 8.209082816308541197, 1.599625672291263179 ) ) ;
#122814 = CARTESIAN_POINT ( 'NONE',  ( 5.700035372616791385, -1.870836310086241294, 0.001406584917262864625 ) ) ;
#122815 = PRESENTATION_LAYER_ASSIGNMENT (  '', '', ( #198903 ) ) ;
#122817 = CARTESIAN_POINT ( 'NONE',  ( -4.553559489343377287, 6.405848385690952718, -1.599625672291271394 ) ) ;
#122816 = CARTESIAN_POINT ( 'NONE',  ( 3.357576282340120066, -1.451192137084562628, -1.245647637661301044 ) ) ;
#122818 = CARTESIAN_POINT ( 'NONE',  ( 5.057340365224886725, -1.863002784048470639, -1.182737378625432489 ) ) ;
#122819 = CARTESIAN_POINT ( 'NONE',  ( 4.891875743818586919, -2.106850654347144580, 0.2108507618673941542 ) ) ;
#122820 = CARTESIAN_POINT ( 'NONE',  ( -1.225000000000016076, 0.8333333340161279690, 0.7072540797572857141 ) ) ;
#122821 = CARTESIAN_POINT ( 'NONE',  ( 6.983263157960335477, 4.692686028926381425, 2.608776679625654182 ) ) ;
#122822 = CARTESIAN_POINT ( 'NONE',  ( 5.275531169048895741, 7.248148678680751189, -1.443375672974078761 ) ) ;
#122823 = CARTESIAN_POINT ( 'NONE',  ( -4.787437638956927977, 7.639075441208117212, -1.082531754730549967 ) ) ;
#122824 = CARTESIAN_POINT ( 'NONE',  ( 5.654972079148370412, 0.4136758123431219514, 2.079573305287989449 ) ) ;
#122825 = CARTESIAN_POINT ( 'NONE',  ( 2.380262917520099553, 1.419673959206497527, 1.819133949716137844 ) ) ;
#122827 = EDGE_CURVE ( 'NONE', #55688, #23953, #9018, .T. ) ;
#122826 = CARTESIAN_POINT ( 'NONE',  ( 3.385159196556942085, 0.04556868695702701727, 1.961494628812537444 ) ) ;
#122828 = CARTESIAN_POINT ( 'NONE',  ( 7.253312916980332758, -6.796015482748900105, 7.253312916980308778 ) ) ;
#122829 = CARTESIAN_POINT ( 'NONE',  ( 6.508646177561060675, 0.6413444998595011493, 1.960425241914983907 ) ) ;
#122830 = CARTESIAN_POINT ( 'NONE',  ( 4.392478581147586603, 4.226905887534702977, -0.7216878364870188411 ) ) ;
#122831 = CARTESIAN_POINT ( 'NONE',  ( 5.578253857379852576, 5.472660686556754861, -0.7998128361456481317 ) ) ;
#122832 = ORIENTED_EDGE ( 'NONE', *, *, #142608, .F. ) ;
#122833 = CARTESIAN_POINT ( 'NONE',  ( 6.034388706570055660, 0.6371486477873434806, 1.913263546360920220 ) ) ;
#122834 = CARTESIAN_POINT ( 'NONE',  ( -9.484092147959342967, 11.02352791316275216, 1.199719254218462483 ) ) ;
#122835 = CIRCLE ( 'NONE', #129619, 2.000000000000006217 ) ;
#122836 = LINE ( 'NONE', #23071, #21096 ) ;
#122837 = CARTESIAN_POINT ( 'NONE',  ( 1.780376006863694904, -1.203675225865230569, -1.806662255390781180 ) ) ;
#122838 = DIRECTION ( 'NONE',  ( 0.000000000000000000, 0.000000000000000000, 1.000000000000000000 ) ) ;
#122839 = CARTESIAN_POINT ( 'NONE',  ( 0.3168469074051638024, -0.7203255543706194031, -1.994627023381766673 ) ) ;
#122840 = CARTESIAN_POINT ( 'NONE',  ( 1.499999999999989120, 2.306250000682817713, 1.214306433183764966E-14 ) ) ;
#122841 = CARTESIAN_POINT ( 'NONE',  ( -5.601541066505636657, 14.53093293999984681, -10.62175398270116489 ) ) ;
#122842 = DIRECTION ( 'NONE',  ( 0.6483454320283812411, 0.000000000000000000, -0.7613463080411777550 ) ) ;
#122843 = CARTESIAN_POINT ( 'NONE',  ( 5.869365784521903606, 7.282179437329668659, 1.264975801879052453 ) ) ;
#122844 = CARTESIAN_POINT ( 'NONE',  ( 1.018906392562862528, 1.903027849223213330, 0.7912521351585340978 ) ) ;
#122846 = CARTESIAN_POINT ( 'NONE',  ( 6.727182134110193168, 4.701113012587437190, 2.373661997258198486 ) ) ;
#122845 = CARTESIAN_POINT ( 'NONE',  ( -8.805130697071332335, 12.36007068230351358, 1.199719254218462483 ) ) ;
#122847 = CARTESIAN_POINT ( 'NONE',  ( 1.364683531249988757, 0.6343750003414208027, 0.000000000000000000 ) ) ;
#122848 = FILL_AREA_STYLE_COLOUR ( '', #98091 ) ;
#122849 = EDGE_CURVE ( 'NONE', #62256, #63949, #46963, .T. ) ;
#122850 = EDGE_LOOP ( 'NONE', ( #172818, #17030, #137030, #208122, #172646, #207245, #32606, #139778 ) ) ;
#122851 = CARTESIAN_POINT ( 'NONE',  ( 3.545477442914763078, -1.765841875850767906, 0.7343832577718925059 ) ) ;
#122852 = CARTESIAN_POINT ( 'NONE',  ( 5.067173336470212064, 0.1711322554274422036, -1.761558580727173862 ) ) ;
#122853 = PRESENTATION_LAYER_ASSIGNMENT (  '', '', ( #153990 ) ) ;
#122854 = CARTESIAN_POINT ( 'NONE',  ( 4.538947565524982686, 8.517465603079630299, 0.000000000000000000 ) ) ;
#122855 = CARTESIAN_POINT ( 'NONE',  ( -3.846762897975357198, 5.510976019103107859, -1.599625672291256295 ) ) ;
#122856 = CARTESIAN_POINT ( 'NONE',  ( 0.5799530485631685384, 0.8934014309100688500, 1.575905833579164694 ) ) ;
#122858 = CARTESIAN_POINT ( 'NONE',  ( 6.169544653506280341, 1.324940883694783578, 1.383738526680919012 ) ) ;
#122857 = CARTESIAN_POINT ( 'NONE',  ( -6.661184041420952440, -7.246166700180828535, 6.773376349083141790 ) ) ;
#122859 = CARTESIAN_POINT ( 'NONE',  ( 0.5024991115675537801, 2.064720838319131779, 0.1538615064654233477 ) ) ;
#122860 = CARTESIAN_POINT ( 'NONE',  ( 1.364683531249988757, -0.3031249996585799744, 0.000000000000000000 ) ) ;
#122861 = CARTESIAN_POINT ( 'NONE',  ( 5.805500895539822181, -0.4530025297027094888, 1.814837910242727226 ) ) ;
#122862 = CARTESIAN_POINT ( 'NONE',  ( 2.455445036260803349, 0.4872311372507812655, -1.759406031448563557 ) ) ;
#122864 = CARTESIAN_POINT ( 'NONE',  ( 5.606371582794006159, 7.377293116531995487, 1.238817421570908905 ) ) ;
#122863 = CARTESIAN_POINT ( 'NONE',  ( 6.270183524512255246, 1.130759168108757873, 1.895055401287759178 ) ) ;
#122865 = CARTESIAN_POINT ( 'NONE',  ( -0.6823417656250246877, 0.5510416670080897639, 1.181850606188755259 ) ) ;
#122866 = CARTESIAN_POINT ( 'NONE',  ( 3.578633024105078331, 1.310608547571969540, -1.592757226543355165 ) ) ;
#122867 = CARTESIAN_POINT ( 'NONE',  ( -6.204827856548512877, 10.39071626594860476, -0.7998128361456291469 ) ) ;
#122868 = CARTESIAN_POINT ( 'NONE',  ( 9.413438726589914651, 9.876766690643398405, 0.000000000000000000 ) ) ;
#122869 = CARTESIAN_POINT ( 'NONE',  ( 4.355193658487812591, 6.104145239700998538, -1.599625672291255185 ) ) ;
#122870 = CARTESIAN_POINT ( 'NONE',  ( 0.4741787938652639034, 1.244221353789766837, 1.767418780601250017 ) ) ;
#122871 = CARTESIAN_POINT ( 'NONE',  ( 6.426242046702522082, 1.060841730010402495, 1.777776562702712226 ) ) ;
#122872 = CARTESIAN_POINT ( 'NONE',  ( -1.402160292154681736E-14, -0.2406249996585799189, -1.575800808251665908 ) ) ;
#122873 = CARTESIAN_POINT ( 'NONE',  ( 3.532649767544591590, 2.108058052951222283, 0.4773693597190583060 ) ) ;
#122876 = EDGE_CURVE ( 'NONE', #75032, #53161, #43567, .T. ) ;
#122875 = CARTESIAN_POINT ( 'NONE',  ( 2.576550507925364109, 1.283677811227203147, -1.483670167215108693 ) ) ;
#122874 = CARTESIAN_POINT ( 'NONE',  ( 3.791669620513484773, 1.900943035724310448, -0.6826196560621737852 ) ) ;
#122877 = CARTESIAN_POINT ( 'NONE',  ( 6.720655732516663150, 7.051555433583626353, 2.871889998671435240 ) ) ;
#122878 = CIRCLE ( 'NONE', #112468, 0.07999999999999986289 ) ;
#122879 = ADVANCED_FACE ( 'NONE', ( #163996 ), #193279, .F. ) ;
#122882 = CARTESIAN_POINT ( 'NONE',  ( 6.643132081016124069, 7.813037518349371879, 1.082531754730558626 ) ) ;
#122881 = CARTESIAN_POINT ( 'NONE',  ( 1.642778471875001811, -3.492708332855375630, 2.845375778867859751 ) ) ;
#122880 = PLANE ( 'NONE',  #55929 ) ;
#122883 = CARTESIAN_POINT ( 'NONE',  ( -7.618755976236585958, 7.853246491889623648, 0.000000000000000000 ) ) ;
#122884 = CARTESIAN_POINT ( 'NONE',  ( 2.466030083290056130, -1.032479112849067793, 1.731996155473938259 ) ) ;
#122885 = CARTESIAN_POINT ( 'NONE',  ( -4.416205349749324327, 6.175325546172740765, 1.599625672291267398 ) ) ;
#122886 = CARTESIAN_POINT ( 'NONE',  ( 1.499999999999989120, 5.577083334016153415, -0.8660254037844323793 ) ) ;
#122887 = CARTESIAN_POINT ( 'NONE',  ( 6.240485052285455581, 1.095381943021833449, -1.567431287326017886 ) ) ;
#122888 = CARTESIAN_POINT ( 'NONE',  ( -2.656508033273816238, 5.186677574539687363, -1.199719254218446718 ) ) ;
#122889 = CARTESIAN_POINT ( 'NONE',  ( 4.758548728272192108, 7.535095368750792666, -1.082531754730549078 ) ) ;
#122891 = CARTESIAN_POINT ( 'NONE',  ( 3.901970389206737444, -1.039011544341267745, -1.727992587138134306 ) ) ;
#122890 = CARTESIAN_POINT ( 'NONE',  ( -6.683806541412756985, 10.74159869838281622, -0.7216878364870267237 ) ) ;
#122892 = CARTESIAN_POINT ( 'NONE',  ( -1.201851678989727383E-14, 3.962500000000022116, 1.732050807568877637 ) ) ;
#122893 = CARTESIAN_POINT ( 'NONE',  ( -8.012344526598182026E-15, 15.10937500034140157, -1.575800808251669460 ) ) ;
#122894 = CARTESIAN_POINT ( 'NONE',  ( 6.774431772926147843, -1.055741295204252195, 1.364281925921766447 ) ) ;
#122895 = CARTESIAN_POINT ( 'NONE',  ( 7.038618024149998043, 8.240751112043669835, -1.199719254218452047 ) ) ;
#122896 = CARTESIAN_POINT ( 'NONE',  ( 8.541273586929342798, 11.94827437051752206, -1.082531754730543083 ) ) ;
#122897 = CARTESIAN_POINT ( 'NONE',  ( 10.91804381884011121, -9.954640477432047163, -0.1905751637469971504 ) ) ;
#122898 = CARTESIAN_POINT ( 'NONE',  ( 4.710133486059870478, -0.7981590245086762625, -1.691823354513532163 ) ) ;
#122899 = FACE_OUTER_BOUND ( 'NONE', #34699, .T. ) ;
#122900 = CARTESIAN_POINT ( 'NONE',  ( 1.815371668717490339, -1.773540675419151169, -1.067758146248848128 ) ) ;
#122901 = CARTESIAN_POINT ( 'NONE',  ( -6.983858524370814003, 9.241197259889665006, 1.443375672974064550 ) ) ;
#122902 = ORIENTED_EDGE ( 'NONE', *, *, #131609, .T. ) ;
#122903 = CARTESIAN_POINT ( 'NONE',  ( 3.984117037569365305, 5.741498858621315371, 1.599625672291261402 ) ) ;
#122904 = CARTESIAN_POINT ( 'NONE',  ( 0.4390776481996219727, -1.704952938511293814, -1.076296438737800454 ) ) ;
#122905 = CARTESIAN_POINT ( 'NONE',  ( -0.2051949539778260834, -0.1395167590549877823, -1.781371329038708096 ) ) ;
#122906 = CARTESIAN_POINT ( 'NONE',  ( 3.065552130021340194, 6.590578228417936835, 0.000000000000000000 ) ) ;
#122907 = CARTESIAN_POINT ( 'NONE',  ( -0.1888596022590736112, -6.708723052947947352, -10.87247189006428272 ) ) ;
#122908 = CARTESIAN_POINT ( 'NONE',  ( 8.229436053370676518, 9.663725486096376827, 1.082531754730558626 ) ) ;
#122909 = CARTESIAN_POINT ( 'NONE',  ( 7.751511138711133064, 10.06651563329490529, -1.599625672291262513 ) ) ;
#122911 = CARTESIAN_POINT ( 'NONE',  ( 5.888286034446420736, -0.6943482264498787027, -1.785519067699488982 ) ) ;
#122910 = CARTESIAN_POINT ( 'NONE',  ( -6.338600509588822263, 7.353787668397130162, -1.199719254218446718 ) ) ;
#122912 = CARTESIAN_POINT ( 'NONE',  ( -1.115562610750309283E-14, 11.34375000068279604, 1.500000000000001554 ) ) ;
#122913 = CARTESIAN_POINT ( 'NONE',  ( -2.599325408948150784, -3.206724562287903257, 2.073009253707752464 ) ) ;
#122914 = DIRECTION ( 'NONE',  ( 0.000000000000000000, 1.000000000000000000, 0.000000000000000000 ) ) ;
#122916 = ORIENTED_EDGE ( 'NONE', *, *, #3680, .T. ) ;
#122915 = CARTESIAN_POINT ( 'NONE',  ( 5.504247177468190699, 5.523969249908757817, 0.7216878364870317197 ) ) ;
#122917 = CARTESIAN_POINT ( 'NONE',  ( -8.026063749610061748, 9.426457798375635022, -1.082531754730543971 ) ) ;
#122918 = CARTESIAN_POINT ( 'NONE',  ( 3.256853613824191029, -1.637998819981079990, 1.410756932016984155 ) ) ;
#122919 = CARTESIAN_POINT ( 'NONE',  ( -5.008811405605897882, 4.808311159487113073, 0.7998128361456281477 ) ) ;
#122920 = CARTESIAN_POINT ( 'NONE',  ( 8.014278199453778839, 8.522615118883788199, 0.000000000000000000 ) ) ;
#122921 = CARTESIAN_POINT ( 'NONE',  ( 1.266058358664986949, 0.6103625328083387425, -2.030891291126469600 ) ) ;
#122922 = CARTESIAN_POINT ( 'NONE',  ( 6.334959139596201716, 0.1821375521317940283, 1.816452708017932238 ) ) ;
#122923 = CARTESIAN_POINT ( 'NONE',  ( 0.9835902346791641770, 1.320712255264442803, 1.463733941802777716 ) ) ;
#122924 = CARTESIAN_POINT ( 'NONE',  ( 3.252119977711815491, 0.8557668478980616777, -1.710280963351323846 ) ) ;
#122925 = ORIENTED_EDGE ( 'NONE', *, *, #3337, .T. ) ;
#122926 = CARTESIAN_POINT ( 'NONE',  ( -11.55950211276791251, 9.719999999999998863, -3.221476510067115662 ) ) ;
#122928 = EDGE_CURVE ( 'NONE', #30243, #64100, #65357, .T. ) ;
#122927 = CARTESIAN_POINT ( 'NONE',  ( 5.301205566836260985, -1.690247886301226909, 1.010757534590230433 ) ) ;
#122929 = CARTESIAN_POINT ( 'NONE',  ( 0.6384921070224542916, -1.665899481912515245, 0.9977595643581302909 ) ) ;
#122930 = ORIENTED_EDGE ( 'NONE', *, *, #143526, .F. ) ;
#122931 = CARTESIAN_POINT ( 'NONE',  ( -6.069210040772897052, 7.109775131437022999, -1.199719254218453823 ) ) ;
#122933 = CARTESIAN_POINT ( 'NONE',  ( 5.959260761812961604, -1.790568634313693730, 1.135864312162476297 ) ) ;
#122932 = CARTESIAN_POINT ( 'NONE',  ( -3.623772196602547346, 7.449761006003425834, 0.000000000000000000 ) ) ;
#122934 = CARTESIAN_POINT ( 'NONE',  ( 5.031484404002878996, 7.923796667095108326, 1.082531754730548412 ) ) ;
#122936 = ORIENTED_EDGE ( 'NONE', *, *, #56061, .T. ) ;
#122935 = CARTESIAN_POINT ( 'NONE',  ( 5.233030847706650057, 1.768443763404730307, 0.7281017474275592871 ) ) ;
#122937 = CARTESIAN_POINT ( 'NONE',  ( 0.5345543961663907773, 1.132513062451316221, -1.893880525681296723 ) ) ;
#122938 = CARTESIAN_POINT ( 'NONE',  ( 7.786489011997303145, -5.767087321559190016, 7.770158002572460809 ) ) ;
#122939 = CARTESIAN_POINT ( 'NONE',  ( 6.551439491213440824, -1.797098368391306655, 0.9074013689854224518 ) ) ;
#122940 = CARTESIAN_POINT ( 'NONE',  ( 0.000000000000000000, 13.49999999999999822, -1.500000000000000222 ) ) ;
#122941 = FACE_OUTER_BOUND ( 'NONE', #93460, .T. ) ;
#122942 = DIRECTION ( 'NONE',  ( 3.330669073875479482E-16, -3.330669073875479482E-16, -1.000000000000000000 ) ) ;
#122943 = CARTESIAN_POINT ( 'NONE',  ( 2.102089431743926706, 0.7944251937819692966, -1.912079865474418439 ) ) ;
#122944 = CARTESIAN_POINT ( 'NONE',  ( -4.876128802409253282, 8.840567369452784874, 0.7998128361456481317 ) ) ;
#122945 = CARTESIAN_POINT ( 'NONE',  ( -4.629329830860687167, 8.351765225447314478, -0.3187335059142253346 ) ) ;
#122946 = CARTESIAN_POINT ( 'NONE',  ( 0.1632417891470130944, -1.931755829615459996, -0.9703963252955111196 ) ) ;
#122947 = CARTESIAN_POINT ( 'NONE',  ( 4.937140493670735708, 8.911747675924535983, -0.7998128361456281477 ) ) ;
#122948 = CARTESIAN_POINT ( 'NONE',  ( -11.40750169882514520, 7.888053100162446540, 3.733381924586108624 ) ) ;
#122949 = CARTESIAN_POINT ( 'NONE',  ( 5.750066545971570520, 5.881034856487848295, -0.7216878364870458196 ) ) ;
#122950 = DIRECTION ( 'NONE',  ( -0.000000000000000000, 1.000000000000000000, -0.000000000000000000 ) ) ;
#122951 = DIRECTION ( 'NONE',  ( 1.000000000000000000, 0.000000000000000000, 0.000000000000000000 ) ) ;
#122952 = CARTESIAN_POINT ( 'NONE',  ( -1.402160292154681736E-14, 13.48437500034139269, 1.575800808251682339 ) ) ;
#122954 = CARTESIAN_POINT ( 'NONE',  ( -5.420227550413282636, 9.545625585449309725, 0.7998128361456291469 ) ) ;
#122953 = CARTESIAN_POINT ( 'NONE',  ( 6.925078400183573457, 0.5887076473912872254, 1.908330883025354030 ) ) ;
#122956 = CARTESIAN_POINT ( 'NONE',  ( 4.412597608232919022, -1.071937594435016683, -1.363045487976799475 ) ) ;
#122955 = TOROIDAL_SURFACE ( 'NONE', #29489, 9.580000000000001847, 0.08000000000000000167 ) ;
#122957 = CARTESIAN_POINT ( 'NONE',  ( -3.632695093457760649, 6.325562478087638496, -1.199719254218452047 ) ) ;
#122958 = CARTESIAN_POINT ( 'NONE',  ( 1.956005403265232978, -0.7013823251572397499, 1.947930506816720087 ) ) ;
#122959 = CARTESIAN_POINT ( 'NONE',  ( 3.989952538763715140, -2.111419002029162328, 0.1578513319024783257 ) ) ;
#122960 = AXIS2_PLACEMENT_3D ( 'NONE', #56031, #122184, #141590 ) ;
#122961 = CARTESIAN_POINT ( 'NONE',  ( 7.884230021546724920, 9.157022099014721306, 1.199719254218462483 ) ) ;
#122962 = CARTESIAN_POINT ( 'NONE',  ( 1.364683531249990311, 3.884375000341417028, 1.214306433183764966E-14 ) ) ;
#122963 = CARTESIAN_POINT ( 'NONE',  ( 1.832793114640043131, -1.868399652882225981, -0.6228533014895777375 ) ) ;
#122964 = CARTESIAN_POINT ( 'NONE',  ( 6.064713176501767222, 6.047104440226040545, 0.4075101515045934097 ) ) ;
#122965 = CARTESIAN_POINT ( 'NONE',  ( 0.08795244648929222142, 1.102731429460445334, 1.562230693318837238 ) ) ;
#122966 = CARTESIAN_POINT ( 'NONE',  ( 4.066585926679040064, -2.138228679320841152, -0.8265488639036464580 ) ) ;
#122967 = CARTESIAN_POINT ( 'NONE',  ( 1.998415063578623085, -0.4859047700337820741, -1.759764234465097221 ) ) ;
#122968 = CARTESIAN_POINT ( 'NONE',  ( 6.201928923608456046, 6.200281597156833691, 0.7998128361456352531 ) ) ;
#122969 = CARTESIAN_POINT ( 'NONE',  ( 7.280365300414074703, 7.596107060012304402, -0.7216878364870257245 ) ) ;
#122970 = CARTESIAN_POINT ( 'NONE',  ( -8.532158741701643123, 8.848606708273724308, 0.7998128361456462443 ) ) ;
#122971 = EDGE_CURVE ( 'NONE', #25151, #210539, #83398, .T. ) ;
#122972 = CARTESIAN_POINT ( 'NONE',  ( 2.654543897082308312, 1.998474955683330334, 0.2423782132614532570 ) ) ;
#122973 = CARTESIAN_POINT ( 'NONE',  ( 3.256644689873238629, -0.5649923015349536115, -1.878667693404307171 ) ) ;
#122974 = CARTESIAN_POINT ( 'NONE',  ( -8.993135964566285168, 9.386413468282476913, -0.7998128361456291469 ) ) ;
#122975 = CARTESIAN_POINT ( 'NONE',  ( -5.280010757518168063, 8.247430752824802980, -1.199719254218446718 ) ) ;
#122976 = CARTESIAN_POINT ( 'NONE',  ( 0.07536363704233049743, 2.002983476668462881, -2.558365315478607904 ) ) ;
#122978 = CARTESIAN_POINT ( 'NONE',  ( 4.750734298983296355, -1.420434005603900429, 1.055588576545069657 ) ) ;
#122977 = CARTESIAN_POINT ( 'NONE',  ( 6.210894578592706772, -0.2570060295814159401, 2.074700711848826096 ) ) ;
#122979 = DIRECTION ( 'NONE',  ( 0.000000000000000000, -1.000000000000000000, 0.000000000000000000 ) ) ;
#122980 = CARTESIAN_POINT ( 'NONE',  ( 0.6740948890744530297, -1.214310170130480593, 1.824057261183717582 ) ) ;
#122981 = CARTESIAN_POINT ( 'NONE',  ( 6.140530580581591735, -1.466303750465405065, 0.9370796520578956734 ) ) ;
#122982 = EDGE_CURVE ( 'NONE', #135497, #129718, #24488, .T. ) ;
#122983 = CARTESIAN_POINT ( 'NONE',  ( 7.052212457402625922, 11.37933163361175382, -0.7998128361456291469 ) ) ;
#122984 = CARTESIAN_POINT ( 'NONE',  ( -6.966220764712169000, 6.002124920821316323, -2.420000000000000373 ) ) ;
#122985 = CARTESIAN_POINT ( 'NONE',  ( 6.416599408848439268, -1.497502150434773194, -1.744030381972218047 ) ) ;
#122986 = CARTESIAN_POINT ( 'NONE',  ( -0.9311234436981480345, -1.428119629485601338, -3.475000000000001421 ) ) ;
#122987 = CARTESIAN_POINT ( 'NONE',  ( 5.835191860132536767, -1.097891704307648597, 1.341895879554096727 ) ) ;
#122988 = CARTESIAN_POINT ( 'NONE',  ( 1.471597369358583318, 0.1596246592955492538, -2.201166978212334424 ) ) ;
#122989 = CARTESIAN_POINT ( 'NONE',  ( 6.250449712397290192, -2.160098187209258835, -0.2192636458223720386 ) ) ;
#122990 = FACE_OUTER_BOUND ( 'NONE', #127258, .T. ) ;
#122991 = CARTESIAN_POINT ( 'NONE',  ( 1.516979485257620608, 0.2134662686405098542, 2.106589464619255558 ) ) ;
#122993 = PRESENTATION_LAYER_ASSIGNMENT (  '', '', ( #64155 ) ) ;
#122992 = CARTESIAN_POINT ( 'NONE',  ( 2.593750000000001776, -1.895863743164140525, -0.7852924748298559798 ) ) ;
#122994 = CARTESIAN_POINT ( 'NONE',  ( 6.727182134110178069, 2.947419669445831669, 2.641212418657997496 ) ) ;
#122995 = CARTESIAN_POINT ( 'NONE',  ( 4.207974007929848881, -1.921269893987355593, 0.1410920886178046452 ) ) ;
#122996 = CARTESIAN_POINT ( 'NONE',  ( 0.7509959265504009274, 2.189410886431830239, 0.3742058002541984729 ) ) ;
#122997 = ORIENTED_EDGE ( 'NONE', *, *, #153215, .F. ) ;
#122998 = CARTESIAN_POINT ( 'NONE',  ( -0.7499999999999972244, 4.108333333333360038, -1.299038105676652011 ) ) ;
#122999 = CARTESIAN_POINT ( 'NONE',  ( 5.345992642490140057, 5.131412925860272090, 1.040834085586084257E-14 ) ) ;
#123000 = CARTESIAN_POINT ( 'NONE',  ( 5.632522751473472589, 8.658694745772667289, -1.199719254218440723 ) ) ;
#123001 = EDGE_CURVE ( 'NONE', #207703, #162811, #103248, .T. ) ;
#123002 = CARTESIAN_POINT ( 'NONE',  ( 3.387547421374631273, 0.05309406834838430178, -2.220816570709438498 ) ) ;
#123003 = CARTESIAN_POINT ( 'NONE',  ( -9.341204650135658483, 10.00041963468749984, 1.040834085586084257E-14 ) ) ;
#123004 = PRESENTATION_STYLE_ASSIGNMENT (( #104528 ) ) ;
#123005 = CARTESIAN_POINT ( 'NONE',  ( 6.724481002698112775, 8.868313807946373473, -1.443375672974057666 ) ) ;
#123006 = EDGE_CURVE ( 'NONE', #129569, #180365, #169308, .T. ) ;
#123007 = CARTESIAN_POINT ( 'NONE',  ( -9.042925270190641740, 11.57316545335434199, 1.443375672974064550 ) ) ;
#123008 = CARTESIAN_POINT ( 'NONE',  ( 5.072158865288222351, 8.931619419562697004, 0.7216878364870317197 ) ) ;
#123009 = B_SPLINE_CURVE_WITH_KNOTS ( 'NONE', 3,
 ( #207557, #75438, #7208, #24533, #40821, #205418, #123220, #90641, #176153, #44022 ),
 .UNSPECIFIED., .F., .F.,
 ( 4, 3, 3, 4 ),
 ( 9.838398445787047234E-17, 3.125150876928134587E-05, 6.280292424941480802E-05, 9.436683654567485139E-05 ),
 .UNSPECIFIED. ) ;
#123010 =( GEOMETRIC_REPRESENTATION_CONTEXT ( 3 ) GLOBAL_UNCERTAINTY_ASSIGNED_CONTEXT ( ( #82142 ) ) GLOBAL_UNIT_ASSIGNED_CONTEXT ( ( #47430, #14877, #63657 ) ) REPRESENTATION_CONTEXT ( 'NONE', 'WORKASPACE' ) );
#123011 = CARTESIAN_POINT ( 'NONE',  ( 1.793592486599729252, 1.492254607734722072, -1.356300734917381678 ) ) ;
#123013 = CARTESIAN_POINT ( 'NONE',  ( 0.4267248635717044158, -1.349908593859616257, 1.559510075185864153 ) ) ;
#123012 = CARTESIAN_POINT ( 'NONE',  ( 6.903072767652295383, 11.20533532890304684, 1.040834085586084257E-14 ) ) ;
#123014 = CARTESIAN_POINT ( 'NONE',  ( -11.48243876534946217, 11.29999999999998117, 3.199999999999997957 ) ) ;
#123015 = CARTESIAN_POINT ( 'NONE',  ( 7.648208051440442468, 8.095533279534887328, 0.000000000000000000 ) ) ;
#123016 = CARTESIAN_POINT ( 'NONE',  ( 6.567905868640212752, -1.062476624526029312, 1.378933096211315101 ) ) ;
#123017 =( LENGTH_UNIT ( ) NAMED_UNIT ( * ) SI_UNIT ( .MILLI., .METRE. ) );
#123018 = CARTESIAN_POINT ( 'NONE',  ( -1.364683531250012516, 2.238541667008087988, -0.7879004041258289570 ) ) ;
#123019 = CARTESIAN_POINT ( 'NONE',  ( 1.510649146982666613, 1.557664219135522110, 0.8400682108315477015 ) ) ;
#123020 = CARTESIAN_POINT ( 'NONE',  ( 0.05336153386781630759, -1.314994204386025434, 1.528742563917218078 ) ) ;
#123021 = CARTESIAN_POINT ( 'NONE',  ( 0.2746299231596514012, 1.718356743839201561, -0.6618312839273902126 ) ) ;
#123022 = CARTESIAN_POINT ( 'NONE',  ( 3.984120879971131401, -2.267471576223866414, -0.3361144993852988594 ) ) ;
#123023 = CARTESIAN_POINT ( 'NONE',  ( 2.273173984786102775, 1.132353773513800510, 1.451651336590239927 ) ) ;
#123024 = AXIS2_PLACEMENT_3D ( 'NONE', #66870, #187054, #38686 ) ;
#123025 = CARTESIAN_POINT ( 'NONE',  ( 10.26082332744404368, 10.86538205830655279, -0.7998128361456281477 ) ) ;
#123026 = CARTESIAN_POINT ( 'NONE',  ( 0.000000000000000000, 15.00000000000000000, 0.000000000000000000 ) ) ;
#123027 = CARTESIAN_POINT ( 'NONE',  ( 3.399243825379614226, 1.438455020490635450, 1.123966471122700650 ) ) ;
#123028 = CARTESIAN_POINT ( 'NONE',  ( 3.867814693791224112, -0.2004342644464084944, -2.006446243107910199 ) ) ;
#123029 = CARTESIAN_POINT ( 'NONE',  ( -8.642432853707342488, 12.17025653171218558, 1.199719254218462483 ) ) ;
#123031 = CARTESIAN_POINT ( 'NONE',  ( -2.021340551328828283, -3.469446951953614189E-15, -0.2879360613984097150 ) ) ;
#123030 = CARTESIAN_POINT ( 'NONE',  ( 3.661208364039827856, -1.994111792441630726, -1.068896079077549910 ) ) ;
#123032 = CARTESIAN_POINT ( 'NONE',  ( 5.034254431704021648, 1.084988065057530982, -1.804815602348212256 ) ) ;
#123033 = CARTESIAN_POINT ( 'NONE',  ( 7.947120472790364154, 14.95225098152464582, 9.881210053433072460 ) ) ;
#123034 = CARTESIAN_POINT ( 'NONE',  ( 2.207561477879273593, -1.661462528888792090, -1.235070534849058266 ) ) ;
#123035 = CARTESIAN_POINT ( 'NONE',  ( 3.867100128395839942, 5.534702787927018974, -1.599625672291255185 ) ) ;
#123036 = CARTESIAN_POINT ( 'NONE',  ( 0.6801582343749865700, 0.08854166700808518975, -1.178068619123869398 ) ) ;
#123037 = CARTESIAN_POINT ( 'NONE',  ( 6.217454246653871586, 1.762742247767977055, 1.178343227268910276 ) ) ;
#123038 = CONTEXT_DEPENDENT_SHAPE_REPRESENTATION ( #155693, #147571 ) ;
#123040 = CARTESIAN_POINT ( 'NONE',  ( 1.084454569787800304, -1.879374161238209773, -0.4228483607967240543 ) ) ;
#123039 = CARTESIAN_POINT ( 'NONE',  ( -10.32861409551237486, 10.94447128771960287, 1.040834085586084257E-14 ) ) ;
#123041 = UNCERTAINTY_MEASURE_WITH_UNIT (LENGTH_MEASURE( 1.000000000000000082E-05 ), #21195, 'distance_accuracy_value', 'NONE');
#123042 = CARTESIAN_POINT ( 'NONE',  ( -4.411198876399886615, 6.239761003923544713, -1.599625672291271394 ) ) ;
#123043 = CARTESIAN_POINT ( 'NONE',  ( 8.341290820905593151, 10.75459192918846618, 1.599625672291281386 ) ) ;
#123044 = CARTESIAN_POINT ( 'NONE',  ( 4.543390873910903238, 7.354354215321133204, 1.082531754730548412 ) ) ;
#123045 = CARTESIAN_POINT ( 'NONE',  ( 4.662511749779700843, 6.863130753939731932, 1.222702295491843616 ) ) ;
#123046 = CARTESIAN_POINT ( 'NONE',  ( -1.500000000000001110, 9.552083334016128191, 0.8660254037844418162 ) ) ;
#123047 = CARTESIAN_POINT ( 'NONE',  ( -5.766295404513795297, 5.621766148221195358, 0.7998128361456341429 ) ) ;
#123048 = CARTESIAN_POINT ( 'NONE',  ( 1.125557598851456786, 1.962289056045916524, 1.041162070263027761 ) ) ;
#123049 = CARTESIAN_POINT ( 'NONE',  ( 1.835132634908468452, 0.2055991040930336133, 2.095883127255711464 ) ) ;
#123050 = CARTESIAN_POINT ( 'NONE',  ( -3.318713740295064163, 7.093859473644694269, 0.000000000000000000 ) ) ;
#123051 = CARTESIAN_POINT ( 'NONE',  ( 8.599949509769960088, 8.927695937686774386, 1.040834085586084257E-14 ) ) ;
#123052 = CARTESIAN_POINT ( 'NONE',  ( 6.104338052012460381, 1.858797879379699536, 0.09248701691148655812 ) ) ;
#123053 = CARTESIAN_POINT ( 'NONE',  ( 5.940443861082012944, 10.08226827123770697, 0.7998128361456462443 ) ) ;
#123054 = CARTESIAN_POINT ( 'NONE',  ( -6.943184063974175757, 9.193743722760251202, -1.443375672974066548 ) ) ;
#123055 = CARTESIAN_POINT ( 'NONE',  ( -7.700668062882059850, 11.92793714009701311, -0.7216878364870267237 ) ) ;
#123056 = CARTESIAN_POINT ( 'NONE',  ( 0.01804983835817890528, -0.5593552815991027494, 2.045460531183339814 ) ) ;
#123057 = CARTESIAN_POINT ( 'NONE',  ( -7.923814432544069142, 8.209148024248356990, 0.000000000000000000 ) ) ;
#123059 = CARTESIAN_POINT ( 'NONE',  ( 3.191801227909254912, -1.315628469008291557, -1.455533501494077342 ) ) ;
#123058 = CARTESIAN_POINT ( 'NONE',  ( -0.6801582343750420812, 2.713541667008087632, 1.178068619123787908 ) ) ;
#123060 = CARTESIAN_POINT ( 'NONE',  ( 2.536181837661064087, 1.019768383293401248, -1.906060392209196763 ) ) ;
#123061 = CARTESIAN_POINT ( 'NONE',  ( 0.9953642579336658969, -1.841430844361633845, 2.783310008858119066E-05 ) ) ;
#123063 = CARTESIAN_POINT ( 'NONE',  ( -5.297426666345223190, 6.395294968284933823, -1.134026229594787383 ) ) ;
#123062 = CARTESIAN_POINT ( 'NONE',  ( -4.122561227007127016, 6.967349310553715647, 1.199719254218452935 ) ) ;
#123064 = CARTESIAN_POINT ( 'NONE',  ( 0.6823417656249899377, 1.592708333674752730, 1.181850606188755259 ) ) ;
#123065 = CARTESIAN_POINT ( 'NONE',  ( 3.978220273661048356, -0.1731065449946489199, -1.731690827559639878 ) ) ;
#123066 = CARTESIAN_POINT ( 'NONE',  ( 5.287316719649520991, 8.151991358691011769, -1.082531754730549078 ) ) ;
#123067 = CARTESIAN_POINT ( 'NONE',  ( -11.77618483200234500, 4.711409542047888976, 4.977076041189349098 ) ) ;
#123068 = CARTESIAN_POINT ( 'NONE',  ( 0.9015118058452382677, 1.767791302423503685, 1.243857928393626633 ) ) ;
#123069 = MECHANICAL_DESIGN_GEOMETRIC_PRESENTATION_REPRESENTATION (  '', ( #1856 ), #209365 ) ;
#123070 = CARTESIAN_POINT ( 'NONE',  ( 2.091172504846372959, 1.163092143266548639, -1.646586049616038494 ) ) ;
#123071 = CARTESIAN_POINT ( 'NONE',  ( -0.09005296632882617280, -9.916958724994124452, -10.99963137851696082 ) ) ;
#123072 = CARTESIAN_POINT ( 'NONE',  ( 0.3566080023540801336, 0.8287714912002723811, 1.996717379258300840 ) ) ;
#123073 = CARTESIAN_POINT ( 'NONE',  ( 2.219545571343143120, -1.912749475042923475, 0.4771270530836198565 ) ) ;
#123074 = DIRECTION ( 'NONE',  ( 0.6507913734559658270, -0.7592566023652989049, 0.000000000000000000 ) ) ;
#123076 = ORIENTED_EDGE ( 'NONE', *, *, #133615, .F. ) ;
#123075 = CARTESIAN_POINT ( 'NONE',  ( -5.641601317062248988, 6.714861303728305586, -1.082531754730549967 ) ) ;
#123077 = CARTESIAN_POINT ( 'NONE',  ( -5.275531169048901958, 8.208517892982092334, -1.082531754730549967 ) ) ;
#123078 = CARTESIAN_POINT ( 'NONE',  ( 5.761288931164342486, 5.686201605971993978, -0.7998128361456481317 ) ) ;
#123079 = CARTESIAN_POINT ( 'NONE',  ( -6.967964602780620353, 7.093989889524320525, 0.000000000000000000 ) ) ;
#123080 = CARTESIAN_POINT ( 'NONE',  ( 2.121745675717867652, -0.4403476065239861903, 1.970919799026500607 ) ) ;
#123081 = LINE ( 'NONE', #24379, #104338 ) ;
#123082 = CARTESIAN_POINT ( 'NONE',  ( 5.790114358714919973, -1.044397830967594976, 2.057800239056095659 ) ) ;
#123084 = EDGE_CURVE ( 'NONE', #57555, #121388, #192259, .T. ) ;
#123083 = DIRECTION ( 'NONE',  ( 0.000000000000000000, 0.06195440338563660415, 0.9980789807931683688 ) ) ;
#123085 = CARTESIAN_POINT ( 'NONE',  ( 3.309375504473045293, -1.601080850277468715, -1.133301831143386007 ) ) ;
#123086 = CARTESIAN_POINT ( 'NONE',  ( 7.723341061279088038, 12.16231500480096983, -0.7998128361456291469 ) ) ;
#123087 = CARTESIAN_POINT ( 'NONE',  ( 0.1764080092822375156, 1.496053712750060383, 1.352152247781977179 ) ) ;
#123088 = ORIENTED_EDGE ( 'NONE', *, *, #144045, .T. ) ;
#123089 = CARTESIAN_POINT ( 'NONE',  ( 2.888026961012623239, -2.114693475102703779, 0.1087559668010943809 ) ) ;
#123091 = CARTESIAN_POINT ( 'NONE',  ( -6.531277313481209212, 8.642909503859968368, 1.599625672291283607 ) ) ;
#123090 = LINE ( 'NONE', #170661, #211493 ) ;
#123092 = CARTESIAN_POINT ( 'NONE',  ( 1.833694255977034615, 1.820935426717207317, 0.2711280389895084353 ) ) ;
#123093 = VERTEX_POINT ( 'NONE', #37171 ) ;
#123094 = CARTESIAN_POINT ( 'NONE',  ( -8.839026081105473054, 12.39961529701003684, -1.199719254218446718 ) ) ;
#123095 = CARTESIAN_POINT ( 'NONE',  ( 2.352382916832110649, 2.704376054464898704, 2.456006149337789157 ) ) ;
#123096 = CARTESIAN_POINT ( 'NONE',  ( 4.570628194609677841, 0.8141925398062774821, 1.958264201954627026 ) ) ;
#123097 = CARTESIAN_POINT ( 'NONE',  ( 0.4976878544296211015, -0.6176706345307936274, -1.734562967469073236 ) ) ;
#123098 = CARTESIAN_POINT ( 'NONE',  ( -1.001543065824772872E-14, 5.243750000682815937, 1.732050807568877637 ) ) ;
#123099 = CARTESIAN_POINT ( 'NONE',  ( 8.450809820019639318, 8.753699632978056755, -0.7998128361456291469 ) ) ;
#123100 = CARTESIAN_POINT ( 'NONE',  ( 6.363572996767764778, 8.517530811019446091, -1.599625672291283607 ) ) ;
#123101 = CARTESIAN_POINT ( 'NONE',  ( 4.868464682339723737, -1.349271924330990080, 1.557713215823807174 ) ) ;
#123103 = CARTESIAN_POINT ( 'NONE',  ( 0.9953642579336658969, -1.841430844361633845, 2.783310008858119066E-05 ) ) ;
#123102 = CARTESIAN_POINT ( 'NONE',  ( -7.063961727919978451, 8.200042423116789436, 1.199719254218450271 ) ) ;
#123104 = CARTESIAN_POINT ( 'NONE',  ( -1.364683531250012516, 4.988541667008084879, -0.7879004041258300672 ) ) ;
#123105 = CARTESIAN_POINT ( 'NONE',  ( -5.966965883657915803, 5.998778352662823998, -0.3115505981291895043 ) ) ;
#123106 = CARTESIAN_POINT ( 'NONE',  ( -9.499615238232420822, -9.906571760739462107, 0.08550182772145856203 ) ) ;
#123107 = PLANE ( 'NONE',  #42504 ) ;
#123108 = CARTESIAN_POINT ( 'NONE',  ( 1.190363680384380229, -0.9894552095768920363, 1.972713631218452557 ) ) ;
#123109 = CARTESIAN_POINT ( 'NONE',  ( 4.306154650063803935, -2.256721687276264099, 0.1609511959119753199 ) ) ;
#123110 = CARTESIAN_POINT ( 'NONE',  ( -6.873620692448438874, 10.96304854125777695, 0.000000000000000000 ) ) ;
#123111 = CARTESIAN_POINT ( 'NONE',  ( 3.252039308394638173, 0.8100161731663655384, -1.620448113725055483 ) ) ;
#123112 = CARTESIAN_POINT ( 'NONE',  ( 3.678834806144789749, 1.615436204272060472, -1.029439157428935658 ) ) ;
#123113 = CARTESIAN_POINT ( 'NONE',  ( 5.793440749948310042, -1.873300974885267589, 0.8818263447485861217 ) ) ;
#123114 = CARTESIAN_POINT ( 'NONE',  ( -1.364683531250012516, 4.801041667008083991, -0.7879004041258300672 ) ) ;
#123115 = CARTESIAN_POINT ( 'NONE',  ( 3.080892710809614243, -0.1436740641204778401, -1.966277672030048107 ) ) ;
#123116 = CARTESIAN_POINT ( 'NONE',  ( 0.6395170938602061650, -1.359983930408629194, -1.364592209491755082 ) ) ;
#123117 = CARTESIAN_POINT ( 'NONE',  ( 3.942156681999692491, 1.861596489644477437, 0.1839347620080991341 ) ) ;
#123118 = CARTESIAN_POINT ( 'NONE',  ( 2.684532350912737009, -1.185368471958246905, 1.979860261248457931 ) ) ;
#123119 = CARTESIAN_POINT ( 'NONE',  ( 3.543253484755361615, 1.683469864222198797, -0.7936445362404942472 ) ) ;
#123120 = CARTESIAN_POINT ( 'NONE',  ( -0.6823417656250212460, 3.801041667008085767, 1.181850606188767472 ) ) ;
#123121 = AXIS2_PLACEMENT_3D ( 'NONE', #156684, #53025, #206474 ) ;
#123122 = CARTESIAN_POINT ( 'NONE',  ( -5.284980951228653190, 5.060232619388524533, 0.000000000000000000 ) ) ;
#123123 = CARTESIAN_POINT ( 'NONE',  ( 6.368579470117202490, 8.453095353268645695, 1.599625672291281386 ) ) ;
#123124 = CARTESIAN_POINT ( 'NONE',  ( -6.518203450479830963, 5.167241622962448488, -2.437504649502885368 ) ) ;
#123125 = CARTESIAN_POINT ( 'NONE',  ( 0.7507728315698600774, 0.6134373412659529512, 2.014746520763583959 ) ) ;
#123126 = CARTESIAN_POINT ( 'NONE',  ( 3.009546912109283934, 6.454962464195385330, 0.000000000000000000 ) ) ;
#123128 = CARTESIAN_POINT ( 'NONE',  ( 0.4019237886466847653, 8.823664549684627545, 1.499999999999997113 ) ) ;
#123127 = CARTESIAN_POINT ( 'NONE',  ( -0.6823417656249969321, 5.030208333674755394, -1.181850606188749264 ) ) ;
#123129 = CARTESIAN_POINT ( 'NONE',  ( 1.406531590435019963, 4.363011334059644142, -0.01155683023987031516 ) ) ;
#123130 = CARTESIAN_POINT ( 'NONE',  ( 1.863691559860299884, -1.706161385809309650, -1.259181899442491037 ) ) ;
#123131 = FILL_AREA_STYLE ('',( #210391 ) ) ;
#123133 = ADVANCED_FACE ( 'NONE', ( #51299 ), #207566, .T. ) ;
#123132 = CARTESIAN_POINT ( 'NONE',  ( 1.072527844217635584, 0.8224262283116140493, 1.844967818783457725 ) ) ;
#123134 = CARTESIAN_POINT ( 'NONE',  ( -1.402160292154681736E-14, 0.5718750003414239114, 1.575800808251672791 ) ) ;
#123135 = CARTESIAN_POINT ( 'NONE',  ( -2.331639231870358930, 5.664070170583284103, -0.7216878364870267237 ) ) ;
#123136 = CARTESIAN_POINT ( 'NONE',  ( 4.473300617505036492, 7.306268922809479704, -1.199719254218452047 ) ) ;
#123137 = CARTESIAN_POINT ( 'NONE',  ( 1.194844697948213463, -0.5240009448631496314, -2.097013730318515456 ) ) ;
#123140 = CARTESIAN_POINT ( 'NONE',  ( 3.958617665510264949, 5.641473247893851628, -1.443375672974051449 ) ) ;
#123139 = CARTESIAN_POINT ( 'NONE',  ( 6.825078400183556049, 7.053092130845653784, 2.453807127456457238 ) ) ;
#123138 = CARTESIAN_POINT ( 'NONE',  ( 4.525389411911321602, 8.501647757197021704, -0.7998128361456381397 ) ) ;
#123141 = CARTESIAN_POINT ( 'NONE',  ( -5.517242166118370150, 5.401480380085008193, 0.7998128361456281477 ) ) ;
#123142 = CARTESIAN_POINT ( 'NONE',  ( 6.016814611094169152, 0.2024578496369993375, 2.006372135924570088 ) ) ;
#123143 = CARTESIAN_POINT ( 'NONE',  ( -9.354762803749327560, 10.01623748057011376, 0.7216878364870438212 ) ) ;
#123144 = ADVANCED_FACE ( 'NONE', ( #98990 ), #143920, .T. ) ;
#123145 = CARTESIAN_POINT ( 'NONE',  ( -0.04112450405316381286, -1.960553898366865555, -0.9795403211517728082 ) ) ;
#123146 = DIRECTION ( 'NONE',  ( -1.000000000000000000, -8.267061968666011278E-31, 1.224646799147343593E-16 ) ) ;
#123148 = CARTESIAN_POINT ( 'NONE',  ( 0.6823417656249969321, 11.02604166700806765, -1.181850606188757036 ) ) ;
#123147 = CARTESIAN_POINT ( 'NONE',  ( 6.719591497160966931, -2.098179372288328182, 0.5198544864785522579 ) ) ;
#123149 = CARTESIAN_POINT ( 'NONE',  ( -10.99777869561574661, 5.379318780083400142, 4.807744692366845207 ) ) ;
#123151 = CARTESIAN_POINT ( 'NONE',  ( 0.8256309606260933132, 0.7751641160983432366, -1.751937020314651150 ) ) ;
#123150 = CARTESIAN_POINT ( 'NONE',  ( -4.568734577680880093, 7.313645526394248364, -1.082531754730548412 ) ) ;
#123152 = CARTESIAN_POINT ( 'NONE',  ( 1.364683531249988757, 1.196875000341421469, 0.000000000000000000 ) ) ;
#123153 = CARTESIAN_POINT ( 'NONE',  ( 0.000000000000000000, 1.000000000000000888, -11.49999999999998934 ) ) ;
#123154 = CARTESIAN_POINT ( 'NONE',  ( -1.850000000000000089, 2.265596578422597184E-16, 1.540743955509788682E-30 ) ) ;
#123155 = CARTESIAN_POINT ( 'NONE',  ( 3.017853972043908151, -0.8504761986376055960, -1.500546066986796490 ) ) ;
#123156 = CARTESIAN_POINT ( 'NONE',  ( 5.713835393516482952, 5.630839145382857680, 0.7998128361456352531 ) ) ;
#123157 = CARTESIAN_POINT ( 'NONE',  ( 0.7019891895669374549, -0.5885738721268447549, -1.669159149975569578 ) ) ;
#123158 = CARTESIAN_POINT ( 'NONE',  ( 4.313639225654395837, -0.3805011380913872476, 2.173570407251994574 ) ) ;
#123159 = ORIENTED_EDGE ( 'NONE', *, *, #127553, .F. ) ;
#123160 = CARTESIAN_POINT ( 'NONE',  ( 9.205623113554628034, 9.842241175342985926, 0.7216878364870458196 ) ) ;
#123161 = CARTESIAN_POINT ( 'NONE',  ( -5.887983850084758330, 10.09134126839936840, 0.7998128361456291469 ) ) ;
#123163 = CARTESIAN_POINT ( 'NONE',  ( 3.603138812553498216, -0.1455146663824242736, 2.011206757212272933 ) ) ;
#123162 = CARTESIAN_POINT ( 'NONE',  ( 4.231183009085410340, 1.939187816756043237, 0.8583030597293441755 ) ) ;
#123164 = ORIENTED_EDGE ( 'NONE', *, *, #111400, .F. ) ;
#123165 = CARTESIAN_POINT ( 'NONE',  ( 4.655245641445829641, 6.524482229810530498, 1.599625672291269396 ) ) ;
#123166 = VERTEX_POINT ( 'NONE', #50231 ) ;
#123167 = CARTESIAN_POINT ( 'NONE',  ( 1.797508989346347619, -0.6330400025267440833, 1.760413054629046625 ) ) ;
#123168 = EDGE_CURVE ( 'NONE', #177320, #156205, #202316, .T. ) ;
#123169 = CARTESIAN_POINT ( 'NONE',  ( -10.45358220256320436, 1.000000000000000888, 5.892590188894342162 ) ) ;
#123170 = LINE ( 'NONE', #142551, #88260 ) ;
#123171 = DIRECTION ( 'NONE',  ( 0.000000000000000000, 0.000000000000000000, -1.000000000000000000 ) ) ;
#123172 = DIRECTION ( 'NONE',  ( 0.000000000000000000, 1.000000000000000000, 0.000000000000000000 ) ) ;
#123173 = CARTESIAN_POINT ( 'NONE',  ( -1.364683531250012516, 2.801041667008090652, -0.7879004041258289570 ) ) ;
#123174 =( NAMED_UNIT ( * ) PLANE_ANGLE_UNIT ( ) SI_UNIT ( $, .RADIAN. ) );
#123175 = STYLED_ITEM ( 'NONE', ( #191132 ), #140161 ) ;
#123176 = CARTESIAN_POINT ( 'NONE',  ( 6.482206841109512396, 9.616306177052839743, -1.082531754730548412 ) ) ;
#123177 = CARTESIAN_POINT ( 'NONE',  ( -4.990809943606294929, 4.995235487061662205, -0.7216878364870338292 ) ) ;
#123178 = CARTESIAN_POINT ( 'NONE',  ( -6.445975688654487001, 6.485002823043819475, -0.7998128361456362523 ) ) ;
#123179 = CARTESIAN_POINT ( 'NONE',  ( 4.043311264919998038, 0.1072909356813686044, 2.118029240109862155 ) ) ;
#123181 = CARTESIAN_POINT ( 'NONE',  ( -10.50659947519749693, 5.359800460605414152, -5.105385958519358169 ) ) ;
#123180 = CARTESIAN_POINT ( 'NONE',  ( -0.02948999725182251466, 0.2504340119564217870, -1.961592983597350459 ) ) ;
#123182 = CARTESIAN_POINT ( 'NONE',  ( 5.589129042188730523, 1.739749244469630529, -0.9270521019464451618 ) ) ;
#123183 = CARTESIAN_POINT ( 'NONE',  ( -1.402160292154681736E-14, 0.5718750003414239114, 1.575800808251672791 ) ) ;
#123184 = CARTESIAN_POINT ( 'NONE',  ( 0.6857920578585029459, 1.939116618559855842, -0.5408100507186993644 ) ) ;
#123185 = ORIENTED_EDGE ( 'NONE', *, *, #7576, .F. ) ;
#123186 = CARTESIAN_POINT ( 'NONE',  ( 0.1580148589572556717, 1.223040929162301449, 1.728066982087714809 ) ) ;
#123187 = DIRECTION ( 'NONE',  ( 0.000000000000000000, 1.000000000000000000, -8.546850786086437571E-32 ) ) ;
#123188 = CARTESIAN_POINT ( 'NONE',  ( 1.574760213118006735, 1.391939136705011348, -1.532762857463897843 ) ) ;
#123189 = CARTESIAN_POINT ( 'NONE',  ( 5.123001941117305336, 7.070197912760590064, 1.599625672291268286 ) ) ;
#123190 = CARTESIAN_POINT ( 'NONE',  ( 6.086684617892325733, 6.065829907154645539, -0.7998128361456481317 ) ) ;
#123192 = CARTESIAN_POINT ( 'NONE',  ( 6.518772930072240790, 6.499656594706071822, -0.7998128361456281477 ) ) ;
#123191 = CARTESIAN_POINT ( 'NONE',  ( 3.873056903084231450, 1.968474739099084436, -0.7045419632574521085 ) ) ;
#123193 = CARTESIAN_POINT ( 'NONE',  ( 5.691390622686558487, 9.861982503101517139, 0.7998128361456341429 ) ) ;
#123196 = VERTEX_POINT ( 'NONE', #82721 ) ;
#123195 = CARTESIAN_POINT ( 'NONE',  ( 1.488595082971344352, -1.720062743487455581, -0.5684112265044569678 ) ) ;
#123194 = CARTESIAN_POINT ( 'NONE',  ( 2.203868028057700990, -1.825262823911228072, 0.04193083753635528516 ) ) ;
#123197 = CARTESIAN_POINT ( 'NONE',  ( 5.057340365224886725, -1.863002784048470639, -1.182737378625432489 ) ) ;
#123198 = DIRECTION ( 'NONE',  ( -1.000000000000000000, -3.135042426464105837E-15, 0.000000000000000000 ) ) ;
#123199 = CARTESIAN_POINT ( 'NONE',  ( 4.383934217864794647, 1.438874268414831015, 1.673263306058408340 ) ) ;
#123200 = CARTESIAN_POINT ( 'NONE',  ( 5.960781091502512119, 10.10599504006161986, 0.7998128361456462443 ) ) ;
#123201 = CARTESIAN_POINT ( 'NONE',  ( -5.911983611117388904, 6.103112485921549535, -0.7233604532801055642 ) ) ;
#123202 = CARTESIAN_POINT ( 'NONE',  ( 3.193911838225035105, 1.215006091714765368, 1.476655219734591906 ) ) ;
#123203 = CARTESIAN_POINT ( 'NONE',  ( 9.368847842243145152, 10.88907622316056312, 1.199719254218453823 ) ) ;
#123204 = CARTESIAN_POINT ( 'NONE',  ( 4.984861949208964305, 1.980195279717174905, 0.6042863919064264122 ) ) ;
#123205 = CARTESIAN_POINT ( 'NONE',  ( 0.07999999999999327094, -8.407420853759283830, 10.99970695577496294 ) ) ;
#123206 = CARTESIAN_POINT ( 'NONE',  ( 5.935146830689759234, -1.586316731616247200, -1.512381816529739353 ) ) ;
#123207 = CARTESIAN_POINT ( 'NONE',  ( 5.959663945170571075, 7.214374732172471383, -1.219933935757764099 ) ) ;
#123208 = VERTEX_POINT ( 'NONE', #33970 ) ;
#123209 = CARTESIAN_POINT ( 'NONE',  ( -11.84668730067608600, 13.39999999999998259, 1.399999999999998579 ) ) ;
#123210 = CARTESIAN_POINT ( 'NONE',  ( 4.329849954717849947, 6.144853928627882489, 1.599625672291262513 ) ) ;
#123211 = CARTESIAN_POINT ( 'NONE',  ( -3.285556943750000070, -0.8929624362542626370, 0.2544620058384380323 ) ) ;
#123212 = CYLINDRICAL_SURFACE ( 'NONE', #181482, 2.000000000000000000 ) ;
#123213 = CARTESIAN_POINT ( 'NONE',  ( -6.548225005720456515, 10.58342024007512983, 0.000000000000000000 ) ) ;
#123214 = CARTESIAN_POINT ( 'NONE',  ( 4.598150373690133463, 5.393538853173795111, -1.199719254218452047 ) ) ;
#123215 = CARTESIAN_POINT ( 'NONE',  ( 5.840704046183605946, -2.018525344099521668, -0.4591754850708437696 ) ) ;
#123216 = CARTESIAN_POINT ( 'NONE',  ( 4.688067719671657585, -0.9068681981775075229, 1.699704011162524120 ) ) ;
#123217 = CARTESIAN_POINT ( 'NONE',  ( 1.405875298092047698, -1.122519365368032984, -1.674874950958963549 ) ) ;
#123218 = CARTESIAN_POINT ( 'NONE',  ( -10.29471871147821282, 10.90492667301307605, -0.7998128361456291469 ) ) ;
#123219 = CARTESIAN_POINT ( 'NONE',  ( 2.925527285498711549, 6.635141943048991742, 0.7998128361456281477 ) ) ;
#123220 = CARTESIAN_POINT ( 'NONE',  ( -4.202365068134823467, 3.977385433202452969, -0.5578299018209158522 ) ) ;
#123221 = CARTESIAN_POINT ( 'NONE',  ( 0.9201892814816803323, 1.302667801055312990, -1.762099327409505811 ) ) ;
#123222 = CARTESIAN_POINT ( 'NONE',  ( 5.109893933574640279, -1.816543354971979163, 0.1824992186492402357 ) ) ;
#123223 = CARTESIAN_POINT ( 'NONE',  ( 5.316205630334249754, 7.295602216847000498, -1.443375672974078761 ) ) ;
#123224 = CARTESIAN_POINT ( 'NONE',  ( 10.40996301719436090, 11.03937836301526687, 0.000000000000000000 ) ) ;
#123225 = CARTESIAN_POINT ( 'NONE',  ( -4.796552484184649856, 8.818004674849227342, -0.7998128361456362523 ) ) ;
#123226 = CARTESIAN_POINT ( 'NONE',  ( 3.357615597678655917, 7.068968630600412695, 0.7998128361456321445 ) ) ;
#123227 = CARTESIAN_POINT ( 'NONE',  ( 5.228604516725597229, 6.129068686715179126, -1.199719254218450271 ) ) ;
#123228 = ORIENTED_EDGE ( 'NONE', *, *, #207043, .T. ) ;
#123230 = CARTESIAN_POINT ( 'NONE',  ( 6.539320575229251808, 0.004279804010676873348, 1.996977849922920267 ) ) ;
#123229 = CARTESIAN_POINT ( 'NONE',  ( 2.261056740009634414, 1.805359621025553363, -0.3608742708730780513 ) ) ;
#123231 = CARTESIAN_POINT ( 'NONE',  ( 1.687308557152231270, -1.277188091954140514, -1.910694296540839332 ) ) ;
#123232 = CARTESIAN_POINT ( 'NONE',  ( 6.702011072381410806, 0.7537920952922130269, -1.811353739714548272 ) ) ;
#123233 = CARTESIAN_POINT ( 'NONE',  ( -5.799137018343247796, 7.788745826199009237, -1.599625672291256295 ) ) ;
#123234 = CARTESIAN_POINT ( 'NONE',  ( -6.781144757626059061, -7.161464053357560644, 6.776370306708066948 ) ) ;
#123235 = CARTESIAN_POINT ( 'NONE',  ( -3.002240950422295995, 5.590032644546251817, -1.199719254218452935 ) ) ;
#123236 = CARTESIAN_POINT ( 'NONE',  ( 0.4146172280090759665, 0.7909515328246279342, 1.913518691844050323 ) ) ;
#123237 = CARTESIAN_POINT ( 'NONE',  ( -4.496464221587651799, 5.274905009054215554, 1.199719254218452935 ) ) ;
#123239 = CARTESIAN_POINT ( 'NONE',  ( 0.6724591444495706671, -1.759989063064151038, -0.6342292696241008665 ) ) ;
#123238 = CARTESIAN_POINT ( 'NONE',  ( 3.105106965723201551, -0.4054212715494521224, 2.050880055191468543 ) ) ;
#123240 = CARTESIAN_POINT ( 'NONE',  ( 1.704453651327157537, -1.458331393932917885, -1.392334588655015803 ) ) ;
#123241 = CARTESIAN_POINT ( 'NONE',  ( 8.188761592974039161, 10.57664116326830595, -1.443375672974063439 ) ) ;
#123242 = VERTEX_POINT ( 'NONE', #166109 ) ;
#123243 = CARTESIAN_POINT ( 'NONE',  ( 1.364683531249988535, 4.717708333674755394, -0.7879004041258300672 ) ) ;
#123244 = CARTESIAN_POINT ( 'NONE',  ( 2.120290817172516551, 0.0009401564262049438847, 1.740626721131139698 ) ) ;
#123245 = CARTESIAN_POINT ( 'NONE',  ( 5.986088515633498197, 6.942523675449257858, -1.199719254218446718 ) ) ;
#123247 = CARTESIAN_POINT ( 'NONE',  ( 0.3975484427966501366, 2.885820281855256741, -1.961872594692045890 ) ) ;
#123246 = CARTESIAN_POINT ( 'NONE',  ( -5.608757509019083543, 5.629766575900002401, -2.420000000000000373 ) ) ;
#123248 = CARTESIAN_POINT ( 'NONE',  ( 2.912419603134624779, 1.249142870932816507, -1.189721958963300130 ) ) ;
#123249 = CARTESIAN_POINT ( 'NONE',  ( 2.419692422129790632, -1.264489869534379141, -1.789777738334753732 ) ) ;
#123250 = CARTESIAN_POINT ( 'NONE',  ( 5.619807753665406302, -2.153844256707802440, 0.4802137346974973409 ) ) ;
#123251 = CARTESIAN_POINT ( 'NONE',  ( -9.645406396194509568, 4.042443384815813445, -6.587269312116742270 ) ) ;
#123252 = CARTESIAN_POINT ( 'NONE',  ( 2.606498238493897279, 2.170487999849361138, 0.05724136673956359972 ) ) ;
#123253 = CARTESIAN_POINT ( 'NONE',  ( 1.365546509989667534, 1.798985258052044900, -0.3101867277976525505 ) ) ;
#123254 = CARTESIAN_POINT ( 'NONE',  ( 1.536181705502183137, 8.701161256998862115, -2.509509933406538273 ) ) ;
#123255 = CARTESIAN_POINT ( 'NONE',  ( 4.434827806327999333, -1.698493238601869182, 1.263996378755541938 ) ) ;
#123256 = CARTESIAN_POINT ( 'NONE',  ( 3.834746474454188013E-15, 12.09375000068279604, 1.500000000000001554 ) ) ;
#123257 = VERTEX_POINT ( 'NONE', #17695 ) ;
#123259 = CARTESIAN_POINT ( 'NONE',  ( 0.6823417656249899377, 0.6552083336747518416, 1.181850606188755259 ) ) ;
#123258 = CARTESIAN_POINT ( 'NONE',  ( 4.318134875187846333, 1.410584032999320225, -1.806939822960533348 ) ) ;
#123260 = DIRECTION ( 'NONE',  ( 0.000000000000000000, 0.000000000000000000, 1.000000000000000000 ) ) ;
#123261 = CARTESIAN_POINT ( 'NONE',  ( 4.704842999142070603, 5.447737239542574272, -1.199719254218452047 ) ) ;
#123262 = EDGE_CURVE ( 'NONE', #140594, #114917, #109597, .T. ) ;
#123263 = CARTESIAN_POINT ( 'NONE',  ( 6.604121268705382519, -0.9518609934017449037, 2.004712419625443776 ) ) ;
#123264 = CARTESIAN_POINT ( 'NONE',  ( -4.907688418466881863, 8.669460888279271416, 0.7216878364870458196 ) ) ;
#123265 = AXIS2_PLACEMENT_3D ( 'NONE', #68913, #150209, #182680 ) ;
#123266 = CARTESIAN_POINT ( 'NONE',  ( 3.795919822146273326, 5.451659097302528068, -1.443375672974051449 ) ) ;
#123267 = CARTESIAN_POINT ( 'NONE',  ( -5.816084710138169633, 8.768887347594400694, 1.082531754730548412 ) ) ;
#123268 =( BOUNDED_CURVE ( )  B_SPLINE_CURVE ( 2, ( #157241, #24007, #91181 ),
 .UNSPECIFIED., .F., .T. ) 
 B_SPLINE_CURVE_WITH_KNOTS ( ( 3, 3 ),
 ( 0.000000000000000000, 0.002450381106065499439 ),
 .UNSPECIFIED. ) 
 CURVE ( )  GEOMETRIC_REPRESENTATION_ITEM ( )  RATIONAL_B_SPLINE_CURVE ( ( 1.000000000000000000, 0.9212106833777522485, 0.9350920161047693302 ) ) 
 REPRESENTATION_ITEM ( '' )  );
#123269 = CARTESIAN_POINT ( 'NONE',  ( 5.099275172515607579, 5.121778254122544283, -0.7216878364870458196 ) ) ;
#123271 = VERTEX_POINT ( 'NONE', #7859 ) ;
#123270 =( GEOMETRIC_REPRESENTATION_CONTEXT ( 3 ) GLOBAL_UNCERTAINTY_ASSIGNED_CONTEXT ( ( #886 ) ) GLOBAL_UNIT_ASSIGNED_CONTEXT ( ( #29913, #16816, #211832 ) ) REPRESENTATION_CONTEXT ( 'NONE', 'WORKASPACE' ) );
#123272 = CARTESIAN_POINT ( 'NONE',  ( 4.781875055470904634, 1.674888562130649960, -1.122497055794105192 ) ) ;
#123274 = CARTESIAN_POINT ( 'NONE',  ( 2.887610015510627459, -1.926180996541780877, 0.7380674418178012619 ) ) ;
#123273 = CARTESIAN_POINT ( 'NONE',  ( 4.741601036477289810, 6.554953847355395880, 1.599625672291267398 ) ) ;
#123276 = CARTESIAN_POINT ( 'NONE',  ( -0.1409997244345879974, 6.947781918643359589, -2.595319453918026653 ) ) ;
#123275 = CARTESIAN_POINT ( 'NONE',  ( -5.182812566104885832, 7.844509203380741980, -1.320274515446249408 ) ) ;
#123277 = CARTESIAN_POINT ( 'NONE',  ( 3.214691819771663628, 6.764574533126651801, -0.7216878364870338292 ) ) ;
#123278 = CARTESIAN_POINT ( 'NONE',  ( 0.000000000000000000, -3.346874999522042149, -3.793834371823813001 ) ) ;
#123279 =( NAMED_UNIT ( * ) PLANE_ANGLE_UNIT ( ) SI_UNIT ( $, .RADIAN. ) );
#123280 = CARTESIAN_POINT ( 'NONE',  ( 5.789076383285488347, 1.657349226701849476, 1.433863557930945332 ) ) ;
#123281 = CARTESIAN_POINT ( 'NONE',  ( 3.129529892704606464, 0.4926417352555876872, 1.955172657653013957 ) ) ;
#123282 = CARTESIAN_POINT ( 'NONE',  ( 2.770863647982471534, 1.747605724785822767, -0.5798694457997202178 ) ) ;
#123283 = CARTESIAN_POINT ( 'NONE',  ( 6.114890974963323345, 7.092793211334054604, 1.199719254218462483 ) ) ;
#123284 = CARTESIAN_POINT ( 'NONE',  ( 6.528339890195161921, 1.048227956652090231, -1.494441373796271622 ) ) ;
#123285 = CARTESIAN_POINT ( 'NONE',  ( -6.714312387265696458, 8.856450423275211037, 1.599625672291283607 ) ) ;
#123286 = CARTESIAN_POINT ( 'NONE',  ( 6.350461102289020054, 0.7023508724467423248, 2.150821023316491498 ) ) ;
#123287 = CARTESIAN_POINT ( 'NONE',  ( 2.156984414944181694, -1.627247350590403707, 1.336999143475733121 ) ) ;
#123288 = CARTESIAN_POINT ( 'NONE',  ( -4.288121723672178476, 8.224835454251337552, -0.7998128361456362523 ) ) ;
#123289 = CARTESIAN_POINT ( 'NONE',  ( 7.588813295347141441, 9.876701482703580837, -1.599625672291262513 ) ) ;
#123290 = CARTESIAN_POINT ( 'NONE',  ( 7.471952054462756010, 7.889901283060952508, 0.7216878364870267237 ) ) ;
#123291 = CARTESIAN_POINT ( 'NONE',  ( -6.144869935491728441, 8.192100896205577243, -1.599625672291263179 ) ) ;
#123292 = CARTESIAN_POINT ( 'NONE',  ( 7.931156673870037643, 8.355363662377600420, -0.7216878364870267237 ) ) ;
#123293 = CARTESIAN_POINT ( 'NONE',  ( 4.048816217420559305, 7.761621341895022397, 0.4883610165275272808 ) ) ;
#123294 = CARTESIAN_POINT ( 'NONE',  ( -3.574546055497324737, 7.322054164722185732, 0.7998128361456341429 ) ) ;
#123296 = CARTESIAN_POINT ( 'NONE',  ( 4.500347021246276391, -1.045864285740649935, 1.959767921951799829 ) ) ;
#123295 = CARTESIAN_POINT ( 'NONE',  ( 2.285534418239891785, 0.09939759515392716793, -2.118372479656557061 ) ) ;
#123297 = CARTESIAN_POINT ( 'NONE',  ( 2.062683196291382082, -2.004346222996217897, -0.8864330828558324438 ) ) ;
#123298 = CARTESIAN_POINT ( 'NONE',  ( 0.7685542157043163680, 1.090964843879228097, 1.918292034055509632 ) ) ;
#123299 = CARTESIAN_POINT ( 'NONE',  ( -3.935609729716867289, 7.813571461303467913, 0.7998128361456352531 ) ) ;
#123300 = CARTESIAN_POINT ( 'NONE',  ( 4.809014631063706524, -1.576880339463518022, 1.167019128429528374 ) ) ;
#123301 = CARTESIAN_POINT ( 'NONE',  ( 9.890836756369282057, 11.49806328964105617, -1.199719254218440723 ) ) ;
#123302 = DIRECTION ( 'NONE',  ( 0.000000000000000000, 0.000000000000000000, -1.000000000000000000 ) ) ;
#123303 = CARTESIAN_POINT ( 'NONE',  ( -0.6823417656250003738, 2.467708333674753618, -1.181850606188749264 ) ) ;
#123305 = CARTESIAN_POINT ( 'NONE',  ( -7.212574532790110737, 7.517017831117667193, -0.7216878364870278340 ) ) ;
#123304 = AXIS2_PLACEMENT_3D ( 'NONE', #99898, #168097, #115143 ) ;
#123306 = CARTESIAN_POINT ( 'NONE',  ( 3.463236921083117981, -1.731491641549892435, 1.224000437801611163 ) ) ;
#123307 = CARTESIAN_POINT ( 'NONE',  ( -2.810282979782591006, 6.500690253046801814, 0.000000000000000000 ) ) ;
#123308 = CARTESIAN_POINT ( 'NONE',  ( 5.313408243115379292, -0.3210861823062813314, 2.137610926513198617 ) ) ;
#123309 = CARTESIAN_POINT ( 'NONE',  ( 4.511176471348508521, -1.804767551675333204, 0.3638508048048467169 ) ) ;
#123310 = CARTESIAN_POINT ( 'NONE',  ( -5.788012183699196456, 6.074875824575221017, 0.5810633148162994699 ) ) ;
#123311 = CARTESIAN_POINT ( 'NONE',  ( -1.364683531250012516, 1.342708333674755616, 0.7879004041258379498 ) ) ;
#123312 = CARTESIAN_POINT ( 'NONE',  ( 0.2041417395101949583, 1.512754574849054956, 0.8604388899705726068 ) ) ;
#123313 = CARTESIAN_POINT ( 'NONE',  ( 6.827182134110178602, 3.710826266403470797, 2.225597045202745594 ) ) ;
#123314 = CARTESIAN_POINT ( 'NONE',  ( 2.385871846325007706, 5.727341554113725586, -0.7216878364870267237 ) ) ;
#123315 = CARTESIAN_POINT ( 'NONE',  ( 11.53271246284126406, 7.258204413557574064, -3.348426109308498155 ) ) ;
#123316 = VECTOR ( 'NONE', #116072, 1000.000000000000000 ) ;
#123317 = CARTESIAN_POINT ( 'NONE',  ( 4.153314892778156242, -1.795761387672462961, -1.203114871582221079 ) ) ;
#123318 = CARTESIAN_POINT ( 'NONE',  ( -5.274285450916075035, 6.112086766612214284, 1.199719254218450271 ) ) ;
#123319 = CARTESIAN_POINT ( 'NONE',  ( 6.063827332385394620, 1.649827434358666967, -1.158513616066357832 ) ) ;
#123320 = CARTESIAN_POINT ( 'NONE',  ( -6.832946231163084860, 10.91559500309152675, 0.000000000000000000 ) ) ;
#123321 = CARTESIAN_POINT ( 'NONE',  ( 3.942369626403975147, 2.151062187213080623, 0.2142938780915065733 ) ) ;
#123322 = CARTESIAN_POINT ( 'NONE',  ( 4.270748893545842861, -1.838291250766799223, -0.7124064801689540261 ) ) ;
#123323 = CARTESIAN_POINT ( 'NONE',  ( 0.2752733618501881363, 2.042644424557562122, -0.7945232813236638991 ) ) ;
#123324 = CARTESIAN_POINT ( 'NONE',  ( 0.6226543773679366067, -1.237902357568532841, -1.947274881911696953 ) ) ;
#123325 = CARTESIAN_POINT ( 'NONE',  ( 3.989569841107299286, 1.489977244407629131, 1.423887585670815747 ) ) ;
#123326 = CARTESIAN_POINT ( 'NONE',  ( 5.442900063589676485, -1.533566843616997133, -1.191469007954217618 ) ) ;
#123327 = CARTESIAN_POINT ( 'NONE',  ( -8.649738815394339753, 9.193709494155953621, 1.040834085586084257E-14 ) ) ;
#123328 = AXIS2_PLACEMENT_3D ( 'NONE', #182264, #146614, #16554 ) ;
#123329 = CARTESIAN_POINT ( 'NONE',  ( -7.119966945832006289, 8.335658187339330283, 1.199719254218452047 ) ) ;
#123330 = DIRECTION ( 'NONE',  ( -0.000000000000000000, -1.000000000000000000, -0.000000000000000000 ) ) ;
#123331 = ORIENTED_EDGE ( 'NONE', *, *, #125522, .T. ) ;
#123332 = CARTESIAN_POINT ( 'NONE',  ( -8.148087131688692253, 9.568818410800712826, -1.082531754730543083 ) ) ;
#123333 = CARTESIAN_POINT ( 'NONE',  ( 1.835297179245497068, 0.2165863673247066801, 2.196102686035047213 ) ) ;
#123334 = CARTESIAN_POINT ( 'NONE',  ( 3.285556943750000070, -3.171874999522043215, 0.000000000000000000 ) ) ;
#123335 = VERTEX_POINT ( 'NONE', #187681 ) ;
#123336 = CARTESIAN_POINT ( 'NONE',  ( 6.983263157960366563, -0.003091553303710344557, 1.945923119799706669 ) ) ;
#123337 = CARTESIAN_POINT ( 'NONE',  ( -0.1290005225502433017, 0.6921039065478848951, -2.255494067288220439 ) ) ;
#123338 = CARTESIAN_POINT ( 'NONE',  ( 1.499999999999990896, 5.306250000682820378, 1.214306433183764966E-14 ) ) ;
#123339 = CARTESIAN_POINT ( 'NONE',  ( 4.499531974119707733, 7.248992493261455117, -1.273121237324711386 ) ) ;
#123341 = DIRECTION ( 'NONE',  ( 0.9982742078614211811, 0.000000000000000000, -0.05872483221476467591 ) ) ;
#123340 = CARTESIAN_POINT ( 'NONE',  ( 9.495347311156807635, -6.857257212219900921, -1.861063089699362494E-15 ) ) ;
#123342 = CARTESIAN_POINT ( 'NONE',  ( 11.94654170777226376, 13.65174326158935791, 1.134972293687618539 ) ) ;
#123343 = ORIENTED_EDGE ( 'NONE', *, *, #170700, .F. ) ;
#123344 = CARTESIAN_POINT ( 'NONE',  ( 2.711851390082948399, -2.038666671984638690, 0.3009093235433103475 ) ) ;
#123345 = CARTESIAN_POINT ( 'NONE',  ( 1.360316468749973584, 0.7864583336747016373, -0.7853790794159161148 ) ) ;
#123346 = CARTESIAN_POINT ( 'NONE',  ( -7.528855374290365887, 7.678086112960552434, -0.7998128361456291469 ) ) ;
#123347 = FILL_AREA_STYLE_COLOUR ( '', #27315 ) ;
#123348 = CARTESIAN_POINT ( 'NONE',  ( 5.820528018968444961, 5.685037531751635953, 0.7998128361456341429 ) ) ;
#123349 = CARTESIAN_POINT ( 'NONE',  ( 0.6376604129620618844, -1.456937097490097255, -1.457867103223365213 ) ) ;
#123351 = CARTESIAN_POINT ( 'NONE',  ( 5.003375819710620398, -1.831856422778654681, 0.1858995714831001289 ) ) ;
#123350 = DIRECTION ( 'NONE',  ( 0.000000000000000000, 0.000000000000000000, 1.000000000000000000 ) ) ;
#123352 = CARTESIAN_POINT ( 'NONE',  ( 7.253775878511261155, 8.421492265473332850, 1.199719254218462483 ) ) ;
#123353 =( BOUNDED_CURVE ( )  B_SPLINE_CURVE ( 2, ( #84619, #200483, #67274, #213530, #66203, #165877, #181057 ),
 .UNSPECIFIED., .F., .T. ) 
 B_SPLINE_CURVE_WITH_KNOTS ( ( 3, 2, 2, 3 ),
 ( 0.3962798098108560874, 0.3988095238095238360, 0.4047619047619047672, 0.4072916187605991611 ),
 .UNSPECIFIED. ) 
 CURVE ( )  GEOMETRIC_REPRESENTATION_ITEM ( )  RATIONAL_B_SPLINE_CURVE ( ( 0.9345202395942615592, 0.9430618748659230777, 1.000000000000000000, 0.8660254037844387076, 1.000000000000000000, 0.9430618748653227801, 0.9345202395940813700 ) ) 
 REPRESENTATION_ITEM ( '' )  );
#123354 = CARTESIAN_POINT ( 'NONE',  ( -5.981082042284069367, 7.006959133200059142, 1.199719254218452935 ) ) ;
#123356 = VERTEX_POINT ( 'NONE', #206063 ) ;
#123355 = CARTESIAN_POINT ( 'NONE',  ( -0.2409995289980003397, 4.087843961663322645, -2.555282842491034323 ) ) ;
#123357 = CARTESIAN_POINT ( 'NONE',  ( 4.600333186373093852, -2.206333364838486411, -0.05604163552313382035 ) ) ;
#123358 = CARTESIAN_POINT ( 'NONE',  ( 0.7202740732663616141, -1.155732025818452913, -1.826486478054230256 ) ) ;
#123359 = CARTESIAN_POINT ( 'NONE',  ( -5.097502569058210753, 7.930541516334467467, -1.082531754730549967 ) ) ;
#123360 = CARTESIAN_POINT ( 'NONE',  ( 6.411931881972196610E-05, -0.8997486769052507327, 1.687471195204979457 ) ) ;
#123361 = CARTESIAN_POINT ( 'NONE',  ( 0.5148617154710420918, 0.1531739628206352510, 2.010800830040265996 ) ) ;
#123362 = CARTESIAN_POINT ( 'NONE',  ( 5.980555156959511898, 9.991415093179179863, -0.7216878364870458196 ) ) ;
#123363 = CARTESIAN_POINT ( 'NONE',  ( 9.398334472548928176, 13.71816428308574842, -7.461477588779884762 ) ) ;
#123364 = DIRECTION ( 'NONE',  ( 0.000000000000000000, 1.000000000000000000, 0.000000000000000000 ) ) ;
#123365 = CARTESIAN_POINT ( 'NONE',  ( 0.000000000000000000, -0.5000000000000005551, 0.000000000000000000 ) ) ;
#123366 = CARTESIAN_POINT ( 'NONE',  ( 0.3384655940862451029, 0.3152513238553408814, 1.843739016257638141 ) ) ;
#123367 = CARTESIAN_POINT ( 'NONE',  ( 2.571500236035813902, 1.429449181443824823, 1.422607194786096541 ) ) ;
#123369 = CARTESIAN_POINT ( 'NONE',  ( -4.467832636417345071, 7.566084030862750609, 0.9469059386725534599 ) ) ;
#123368 = CARTESIAN_POINT ( 'NONE',  ( 1.364683531249986537, 1.113541667008082658, 0.7879004041258500513 ) ) ;
#123371 = CARTESIAN_POINT ( 'NONE',  ( 4.213572796808015219, -0.3603392467595716298, 2.074844637031019623 ) ) ;
#123370 = CARTESIAN_POINT ( 'NONE',  ( -8.178592977541617515, 10.56477777859713463, 1.599625672291295375 ) ) ;
#123372 = CARTESIAN_POINT ( 'NONE',  ( 7.741869408603235136, 8.990934717247309749, 1.199719254218462483 ) ) ;
#123374 = CARTESIAN_POINT ( 'NONE',  ( -7.666245793523398078, 11.03137162816423356, 1.199719254218453823 ) ) ;
#123373 = CARTESIAN_POINT ( 'NONE',  ( 4.050854035433010480, 7.948023151305657841, 0.000000000000000000 ) ) ;
#123375 = SURFACE_STYLE_FILL_AREA ( #204496 ) ;
#123377 = EDGE_CURVE ( 'NONE', #157191, #33058, #108644, .T. ) ;
#123376 = CARTESIAN_POINT ( 'NONE',  ( 4.131121313247118287, 1.848376352210901574, 0.8146727144991843250 ) ) ;
#123378 = CARTESIAN_POINT ( 'NONE',  ( -0.6823417656250212460, 4.551041667008086655, 1.181850606188767472 ) ) ;
#123379 = CARTESIAN_POINT ( 'NONE',  ( 8.432808358020015049, 11.82173160345663376, 1.082531754730546636 ) ) ;
#123380 = CARTESIAN_POINT ( 'NONE',  ( 4.446650332099550518, 0.5718123500428309303, 2.084546224624775679 ) ) ;
#123381 = CARTESIAN_POINT ( 'NONE',  ( 4.850785098639300408, 8.881276058379668825, -0.7998128361456481317 ) ) ;
#123382 = CARTESIAN_POINT ( 'NONE',  ( 1.364683531249986537, -0.8239583329919186738, 0.7879004041258500513 ) ) ;
#123384 =( NAMED_UNIT ( * ) SI_UNIT ( $, .STERADIAN. ) SOLID_ANGLE_UNIT ( ) );
#123383 = CARTESIAN_POINT ( 'NONE',  ( 5.182959862174088883, 9.268813282503625572, 0.7998128361456331437 ) ) ;
#123385 = CARTESIAN_POINT ( 'NONE',  ( 8.609064354553323639, 10.10662517080946543, -1.082531754730543083 ) ) ;
#123387 = CARTESIAN_POINT ( 'NONE',  ( -8.881784197001254049E-17, 4.500000000000002665, 1.600000000000005196 ) ) ;
#123386 = CARTESIAN_POINT ( 'NONE',  ( 1.820994678651502330, -1.536134449795123480, 1.534618252339227329 ) ) ;
#123389 = CARTESIAN_POINT ( 'NONE',  ( 2.067674361007607597, -1.131582805410412673, 1.452419944642673100 ) ) ;
#123388 = CARTESIAN_POINT ( 'NONE',  ( -4.107757355260591936, 7.736207981205250661, 1.040834085586084257E-14 ) ) ;
#123390 = ADVANCED_FACE ( 'NONE', ( #91286 ), #56631, .F. ) ;
#123391 = CARTESIAN_POINT ( 'NONE',  ( -0.6823417656250212460, 1.801041667008083991, 1.181850606188755259 ) ) ;
#123392 = CARTESIAN_POINT ( 'NONE',  ( 3.737968522918270864, 2.181131050170285857, 0.2133239450496857148 ) ) ;
#123393 = CARTESIAN_POINT ( 'NONE',  ( 6.883263157960366918, 2.950764357809147143, 2.606098932787728639 ) ) ;
#123394 = CARTESIAN_POINT ( 'NONE',  ( 4.170984489290855635, -2.109804223432755865, -0.8175660662063081174 ) ) ;
#123395 = CARTESIAN_POINT ( 'NONE',  ( -7.802881099864745984, 9.062115023719057305, -1.199719254218446718 ) ) ;
#123396 = CARTESIAN_POINT ( 'NONE',  ( 1.364683531249988535, 4.967708333674756283, -0.7879004041258300672 ) ) ;
#123397 = CARTESIAN_POINT ( 'NONE',  ( 6.486339200172205999, 6.751434215916642501, 0.1376000389162572446 ) ) ;
#123398 = CARTESIAN_POINT ( 'NONE',  ( -1.500000000000008216, 14.24999999999999822, 3.469446951953614189E-15 ) ) ;
#123399 = CARTESIAN_POINT ( 'NONE',  ( 4.584065335196261692, 7.401807753487379848, 1.082531754730549078 ) ) ;
#123400 = CARTESIAN_POINT ( 'NONE',  ( 5.008955365368598756, 1.539791945809299012, 0.8722439129504773181 ) ) ;
#123401 = CARTESIAN_POINT ( 'NONE',  ( 8.609591239877852686, 10.00327685373437347, -1.199719254218445830 ) ) ;
#123402 = CARTESIAN_POINT ( 'NONE',  ( 0.6398468662271715734, -1.489381099377089512, -1.489160694218383485 ) ) ;
#123404 = CARTESIAN_POINT ( 'NONE',  ( -1.201851678989727383E-14, 0.9625000000000237810, 1.732050807568877637 ) ) ;
#123403 = CARTESIAN_POINT ( 'NONE',  ( 1.364683531249996529, 10.21354166700806587, 0.7879004041258405033 ) ) ;
#123405 = CARTESIAN_POINT ( 'NONE',  ( 0.6429344911094649895, -0.2373986304471594755, -1.955105650238073478 ) ) ;
#123406 = CARTESIAN_POINT ( 'NONE',  ( -4.995253251992230581, 4.792493313604505367, 0.000000000000000000 ) ) ;
#123407 = CARTESIAN_POINT ( 'NONE',  ( -10.91970695577495754, -5.907420853759267843, -0.07999999999999847511 ) ) ;
#123409 = VERTEX_POINT ( 'NONE', #173612 ) ;
#123408 = CARTESIAN_POINT ( 'NONE',  ( 5.519718948577209794, -0.4320008574366646648, 1.759211659423996155 ) ) ;
#123410 = CARTESIAN_POINT ( 'NONE',  ( 5.816084710582486217, 9.729256562414162701, 1.040834085586084257E-14 ) ) ;
#123411 = CARTESIAN_POINT ( 'NONE',  ( 8.723781775389312543, 12.26516360700784958, -1.199719254218446718 ) ) ;
#123413 = CARTESIAN_POINT ( 'NONE',  ( 4.557402362779487959, 0.4096945884842878027, -1.825068887194372991 ) ) ;
#123412 = CIRCLE ( 'NONE', #54051, 7.424569270082293393 ) ;
#123414 = CARTESIAN_POINT ( 'NONE',  ( 2.517010073631369860, 6.088262185878572375, -0.7998128361456281477 ) ) ;
#123415 = CARTESIAN_POINT ( 'NONE',  ( 4.487213805514509879, 0.09639557921744396074, 2.068113308821089902 ) ) ;
#123416 = CARTESIAN_POINT ( 'NONE',  ( 1.224999999999955014, 1.895833333333312831, -0.7072540797573217963 ) ) ;
#123417 = ADVANCED_FACE ( 'NONE', ( #73944, #55562 ), #24108, .F. ) ;
#123418 = CARTESIAN_POINT ( 'NONE',  ( -5.763624699140894592, 5.896852701852039580, -0.7216878364870338292 ) ) ;
#123419 = SURFACE_STYLE_FILL_AREA ( #57258 ) ;
#123420 = AXIS2_PLACEMENT_3D ( 'NONE', #62154, #113101, #30729 ) ;
#123421 = CARTESIAN_POINT ( 'NONE',  ( 6.916630921265960019, 11.22115317478565188, 0.7998128361456462443 ) ) ;
#123422 = CARTESIAN_POINT ( 'NONE',  ( -9.775592450653132204, 11.36361159963886891, -1.199719254218441611 ) ) ;
#123423 = CARTESIAN_POINT ( 'NONE',  ( 7.018280793729500644, 8.217024343219755167, -1.199719254218452047 ) ) ;
#123424 = CARTESIAN_POINT ( 'NONE',  ( 4.779848517908583894, 4.883929213520019630, -0.7538207499340529028 ) ) ;
#123425 = CARTESIAN_POINT ( 'NONE',  ( -1.402160292154681736E-14, -0.1781249996585796136, 1.575800808251672791 ) ) ;
#123426 = CARTESIAN_POINT ( 'NONE',  ( -1.500000000000015099, 0.6291666666666863028, -0.8660254037844313801 ) ) ;
#123427 = CARTESIAN_POINT ( 'NONE',  ( 3.631260574587381829, 0.05062604155347744800, -1.961386756325018021 ) ) ;
#123428 = CARTESIAN_POINT ( 'NONE',  ( 1.598982282203027516, 0.9961506480390787122, -1.752761228829377904 ) ) ;
#123429 = CARTESIAN_POINT ( 'NONE',  ( -0.1108833634137010027, 1.377173795795206157, -2.152720132533675113 ) ) ;
#123430 = CARTESIAN_POINT ( 'NONE',  ( -4.953446695184517523, 4.881368687244443727, 0.2706067644340372502 ) ) ;
#123431 = DIRECTION ( 'NONE',  ( 0.000000000000000000, 0.000000000000000000, -1.000000000000000000 ) ) ;
#123432 = CARTESIAN_POINT ( 'NONE',  ( 1.739302498465819191, -1.351291084634953066, -1.293660915597586003 ) ) ;
#123433 = CARTESIAN_POINT ( 'NONE',  ( -1.364683531250010295, 5.488541667008087543, -0.7879004041258300672 ) ) ;
#123434 = CARTESIAN_POINT ( 'NONE',  ( 4.465094144989894431, -1.614439531090381408, 1.202519638469838226 ) ) ;
#123435 = CARTESIAN_POINT ( 'NONE',  ( -7.458957065812611198, 11.85386701009007204, 0.7998128361456481317 ) ) ;
#123437 = CARTESIAN_POINT ( 'NONE',  ( 2.864987086846816577, -0.1587241086147250513, -2.111353475082369702 ) ) ;
#123436 = CARTESIAN_POINT ( 'NONE',  ( -6.127922243696855453, 7.211959374810172463, 1.082531754730549967 ) ) ;
#123438 = CARTESIAN_POINT ( 'NONE',  ( -1.500000000000025091, 4.952083334016149863, 0.8660254037844322683 ) ) ;
#123439 = CARTESIAN_POINT ( 'NONE',  ( 4.932118098221458524, 1.189261692661430114, 1.694535115018414917 ) ) ;
#123440 = CARTESIAN_POINT ( 'NONE',  ( 6.343235766347262938, 8.493804042195527870, -1.599625672291281386 ) ) ;
#123442 = CARTESIAN_POINT ( 'NONE',  ( 6.720655732516665815, 6.034026441762381232, 2.768628153821062199 ) ) ;
#123441 = CARTESIAN_POINT ( 'NONE',  ( 6.720655732516684466, -0.001531948155393536137, 2.073773125298985054 ) ) ;
#123444 = VERTEX_POINT ( 'NONE', #141124 ) ;
#123443 = CARTESIAN_POINT ( 'NONE',  ( 6.018537349360657984, 1.224031959697377658, -1.354583942311540667 ) ) ;
#123445 = CARTESIAN_POINT ( 'NONE',  ( 7.567422294721922960, 11.98040977715095323, 0.7998128361456462443 ) ) ;
#123446 = CARTESIAN_POINT ( 'NONE',  ( 7.985752187169497418, -6.863172033215938050, -7.565242077046494096 ) ) ;
#123447 = CARTESIAN_POINT ( 'NONE',  ( -11.95360554405576359, 13.60444996502587500, 1.059413164304729538 ) ) ;
#123448 = CARTESIAN_POINT ( 'NONE',  ( -11.27970626620888517, 5.059847508428347851, 5.788342990380983544 ) ) ;
#123449 = CARTESIAN_POINT ( 'NONE',  ( 8.405692050348340771, 8.908988268268968724, 1.040834085586084257E-14 ) ) ;
#123450 = CARTESIAN_POINT ( 'NONE',  ( -8.012344526598182026E-15, 12.10937500034140157, -1.575800808251669460 ) ) ;
#123451 = CARTESIAN_POINT ( 'NONE',  ( -0.02317427319796245069, -1.617030479356797334, -0.8165419217573687272 ) ) ;
#123452 = CARTESIAN_POINT ( 'NONE',  ( -7.811469059767924605, 12.26513100303794168, -0.7998128361456281477 ) ) ;
#123453 = CARTESIAN_POINT ( 'NONE',  ( 4.496500501226593727, 8.397667684739696270, 0.7998128361456462443 ) ) ;
#123454 = CARTESIAN_POINT ( 'NONE',  ( 0.6801582343749831283, 2.755208333674742605, 1.178068619123796568 ) ) ;
#123455 = CARTESIAN_POINT ( 'NONE',  ( 2.860407222358963608, 5.320596945185329218, 1.082531754730548412 ) ) ;
#123456 = CARTESIAN_POINT ( 'NONE',  ( -1.500000000000001110, 12.30208333401612641, 0.8660254037844418162 ) ) ;
#123457 = CARTESIAN_POINT ( 'NONE',  ( 2.184835310096557404, 5.700724961754617404, 1.040834085586084257E-14 ) ) ;
#123458 = EDGE_LOOP ( 'NONE', ( #169688, #168594, #120371, #178895 ) ) ;
#123459 = COLOUR_RGB ( '', 0.09019608, 0.27058824, 0.51372549) ;
#123460 = CARTESIAN_POINT ( 'NONE',  ( -4.938913097128142304, 8.984092056616635347, -0.7998128361456362523 ) ) ;
#123461 = CARTESIAN_POINT ( 'NONE',  ( 5.097279880301520905, -0.2930512725940071506, 1.994873791649566463 ) ) ;
#123462 = CARTESIAN_POINT ( 'NONE',  ( -3.672734859294646270E-15, -9.746166700180790343, -9.579665964948869572 ) ) ;
#123463 = SURFACE_STYLE_USAGE ( .BOTH. , #141790 ) ;
#123464 = CARTESIAN_POINT ( 'NONE',  ( -6.492003545397249553, 6.763960095814848472, -0.1687977717132038147 ) ) ;
#123465 = CARTESIAN_POINT ( 'NONE',  ( -4.121315508874255684, 7.752025827087861920, -0.7216878364870267237 ) ) ;
#123466 = CARTESIAN_POINT ( 'NONE',  ( 4.518945272056516416, 4.166524327021037699, 0.7998128361456341429 ) ) ;
#123467 = CARTESIAN_POINT ( 'NONE',  ( 2.887507918447276722, -1.839357967585793840, 0.7044240162308276210 ) ) ;
#123468 = CARTESIAN_POINT ( 'NONE',  ( 4.165638788432171502, 1.319243065725501873, 1.525032742243138451 ) ) ;
#123469 = CARTESIAN_POINT ( 'NONE',  ( -6.205881626753225966, 8.263281202677319470, 1.599625672291283607 ) ) ;
#123470 = CARTESIAN_POINT ( 'NONE',  ( 6.727182134110194944, 2.413774403037728167, 2.569658639860139093 ) ) ;
#123471 = CIRCLE ( 'NONE', #151067, 0.08000000000000040412 ) ;
#123472 = CARTESIAN_POINT ( 'NONE',  ( 4.365290731249091394, 2.125951747006165959, -0.5312598475561494116 ) ) ;
#123473 = SURFACE_STYLE_USAGE ( .BOTH. , #173210 ) ;
#123474 = CARTESIAN_POINT ( 'NONE',  ( 3.223571483072392940, -1.856993652095505487, 0.5122080487700955143 ) ) ;
#123475 = CARTESIAN_POINT ( 'NONE',  ( -9.671043645249580933, 10.17730576241299900, 0.7998128361456462443 ) ) ;
#123476 = CARTESIAN_POINT ( 'NONE',  ( 0.4999999999999848455, 3.949999999999953548, -0.4500000000000250466 ) ) ;
#123477 = CARTESIAN_POINT ( 'NONE',  ( 0.1755611466353626804, -0.002217706044341590139, -2.244164702216360663 ) ) ;
#123478 = CARTESIAN_POINT ( 'NONE',  ( 1.466069532605751007E-15, 14.48154074412737558, 12.00000000000000178 ) ) ;
#123479 = CARTESIAN_POINT ( 'NONE',  ( 4.313465427442102929, 8.184126765324453601, 0.7998128361456462443 ) ) ;
#123480 = CARTESIAN_POINT ( 'NONE',  ( -6.725651841507101381, -7.791858861492833910, 6.710064404886642464 ) ) ;
#123481 = CARTESIAN_POINT ( 'NONE',  ( 4.584065335196271462, 5.481069324884694005, 1.082531754730549078 ) ) ;
#123482 = ORIENTED_EDGE ( 'NONE', *, *, #178819, .T. ) ;
#123484 = CARTESIAN_POINT ( 'NONE',  ( 2.701816853162309684, 1.425160482578791354, 1.422027561765064174 ) ) ;
#123483 = CARTESIAN_POINT ( 'NONE',  ( 6.251489360189885325, 1.835807759842246423, -0.1425652098738516838 ) ) ;
#123485 = CARTESIAN_POINT ( 'NONE',  ( 5.308124166105086417, -1.975000179191854111, 1.175378216249231222 ) ) ;
#123487 = CARTESIAN_POINT ( 'NONE',  ( 3.731172809088632025, 0.04972793443442201367, -1.860468898575567520 ) ) ;
#123486 = CARTESIAN_POINT ( 'NONE',  ( 10.50000000000000178, 10.09159113040219502, -3.600000000000000977 ) ) ;
#123488 = CARTESIAN_POINT ( 'NONE',  ( 0.000000000000000000, 2.800000000000024691, 1.214306433183764966E-14 ) ) ;
#123489 = DIRECTION ( 'NONE',  ( 0.000000000000000000, -0.7999999999972235987, -0.6000000000037019054 ) ) ;
#123490 = CARTESIAN_POINT ( 'NONE',  ( -5.682838942422375084, 9.781729199468104596, 0.000000000000000000 ) ) ;
#123491 = CARTESIAN_POINT ( 'NONE',  ( -3.363831509966360489, 6.938570838353784076, -0.7216878364870458196 ) ) ;
#123492 = CARTESIAN_POINT ( 'NONE',  ( 6.286679179808664308, 1.818834136932646839, -1.030939041669608924 ) ) ;
#123493 = CARTESIAN_POINT ( 'NONE',  ( 6.168596704537822717, 6.299043698156668647, 1.040834085586084257E-14 ) ) ;
#123494 = EDGE_LOOP ( 'NONE', ( #58317, #124950, #199642, #39194 ) ) ;
#123495 = CARTESIAN_POINT ( 'NONE',  ( 5.586571952581918410, 5.815697052094486175, 0.6573761775866425738 ) ) ;
#123497 = CARTESIAN_POINT ( 'NONE',  ( 3.181359600701000989, 6.863336634126477875, 0.000000000000000000 ) ) ;
#123496 = CARTESIAN_POINT ( 'NONE',  ( 0.4809368265653533037, 3.139971263792666445, -0.4000000000000023537 ) ) ;
#123498 = CARTESIAN_POINT ( 'NONE',  ( 5.900961842893762466, 1.406060569669766114, -0.9988219321918601068 ) ) ;
#123499 = CARTESIAN_POINT ( 'NONE',  ( -5.331380718671772101, 7.243030143248949670, -1.599625672291256295 ) ) ;
#123500 = CARTESIAN_POINT ( 'NONE',  ( 0.9142546942676577082, -1.099255453910731983, -1.341178637715144673 ) ) ;
#123501 = CARTESIAN_POINT ( 'NONE',  ( -6.414416072596883289, 6.656109304217317835, -0.7216878364870141782 ) ) ;
#123502 = CARTESIAN_POINT ( 'NONE',  ( 1.387358672534390935, 7.315968950353690659, -4.254625267138188782 ) ) ;
#123503 = CARTESIAN_POINT ( 'NONE',  ( 0.000000000000000000, 0.03624871340549007392, 6.250000000000000000 ) ) ;
#123504 = CARTESIAN_POINT ( 'NONE',  ( 5.454042025912737124, -0.7881617977381920603, 2.023119649181570168 ) ) ;
#123505 = CARTESIAN_POINT ( 'NONE',  ( 5.285714101943871590, 1.228958891529348785, 1.350286652578087665 ) ) ;
#123506 = CARTESIAN_POINT ( 'NONE',  ( 2.535929169054650156, 1.202975682259961765, 1.549578550289295586 ) ) ;
#123507 = FACE_OUTER_BOUND ( 'NONE', #35845, .T. ) ;
#123508 = CARTESIAN_POINT ( 'NONE',  ( -9.829825065107822724, 11.42688298316931572, 1.199719254218462483 ) ) ;
#123509 = CARTESIAN_POINT ( 'NONE',  ( 8.423693512792301163, 8.722063941212843119, 0.7998128361456481317 ) ) ;
#123510 = ADVANCED_FACE ( 'NONE', ( #26245 ), #155202, .F. ) ;
#123511 = CARTESIAN_POINT ( 'NONE',  ( 3.879626234357834047, 0.2581020070546445888, -2.104639248629774251 ) ) ;
#123512 =( NAMED_UNIT ( * ) PLANE_ANGLE_UNIT ( ) SI_UNIT ( $, .RADIAN. ) );
#123513 = CARTESIAN_POINT ( 'NONE',  ( -5.762678113124475310, 6.090388861115007657, -0.6347866013659544393 ) ) ;
#123514 = CARTESIAN_POINT ( 'NONE',  ( 2.166927730644189420, 1.536898783757352005, -1.387270004372019416 ) ) ;
#123516 = CARTESIAN_POINT ( 'NONE',  ( -1.500000000000001110, 15.05208333401613174, 0.8660254037844419273 ) ) ;
#123515 = CYLINDRICAL_SURFACE ( 'NONE', #162134, 0.07999999999999993228 ) ;
#123518 = ORIENTED_EDGE ( 'NONE', *, *, #157520, .F. ) ;
#123517 = CARTESIAN_POINT ( 'NONE',  ( 3.985193088136604889, -2.072824570928345711, -0.7989420372410382942 ) ) ;
#123519 = CARTESIAN_POINT ( 'NONE',  ( 1.618275512070939115, 0.2312369868452644750, 2.287056861988717493 ) ) ;
#123521 = CARTESIAN_POINT ( 'NONE',  ( 0.2682999959267086676, -0.8333247372044670920, -1.774235371720728649 ) ) ;
#123520 = CARTESIAN_POINT ( 'NONE',  ( 10.39874063200158893, 11.23421161353111586, 0.000000000000000000 ) ) ;
#123523 = CARTESIAN_POINT ( 'NONE',  ( -1.642778471875000035, -3.667708332855373676, -2.845375778867859751 ) ) ;
#123522 = CARTESIAN_POINT ( 'NONE',  ( 3.555981428534177091, 7.370671776590375757, 0.7998128361456271485 ) ) ;
#123524 = DIRECTION ( 'NONE',  ( -1.000000000000000000, -0.000000000000000000, -0.000000000000000000 ) ) ;
#123525 = CARTESIAN_POINT ( 'NONE',  ( 6.392148736875968851, -0.4980823202534767624, -1.772533436741857260 ) ) ;
#123526 = CARTESIAN_POINT ( 'NONE',  ( -5.775621779818983725, 6.082434804166422460, -0.6095328524017195049 ) ) ;
#123527 = CARTESIAN_POINT ( 'NONE',  ( -0.2106725631049838343, 0.7236243445625335502, -2.087119268998542942 ) ) ;
#123528 = CARTESIAN_POINT ( 'NONE',  ( 2.854212618329458717, 0.5792176767629078071, 1.624745991979989812 ) ) ;
#123529 = CARTESIAN_POINT ( 'NONE',  ( 1.798064920797682653, -0.9548589541341389042, -1.776165177175797583 ) ) ;
#123530 =( BOUNDED_SURFACE ( )  B_SPLINE_SURFACE ( 3, 2, ( 
 ( #203607, #21645, #84550 ),
 ( #101871, #87752, #166880 ),
 ( #153829, #121407, #5399 ),
 ( #55260, #105093, #138655 ) ),
 .UNSPECIFIED., .F., .F., .T. ) 
 B_SPLINE_SURFACE_WITH_KNOTS ( ( 4, 4 ),
 ( 3, 3 ),
 ( 1.570796326794896114, 2.200856270471036158 ),
 ( 0.000000000000000000, 1.000000000000000000 ),
 .UNSPECIFIED. ) 
 GEOMETRIC_REPRESENTATION_ITEM ( )  RATIONAL_B_SPLINE_SURFACE ( (
 ( 1.000000000000000000, 0.7071067811865544561, 1.000000000000000000),
 ( 1.000000000000000000, 0.7517196685950666701, 1.000000000000000000),
 ( 1.000000000000000000, 0.7917671131335243251, 1.000000000000000000),
 ( 1.000000000000000000, 0.8226529996948415135, 1.000000000000000000) ) ) 
 REPRESENTATION_ITEM ( '' )  SURFACE ( )  );
#123531 = CARTESIAN_POINT ( 'NONE',  ( 3.093345431676647994, 1.942085262481594965, -1.160266548027958367 ) ) ;
#123532 = CARTESIAN_POINT ( 'NONE',  ( 4.811209553025526553, 1.832079168721172380, 1.038602630702612384 ) ) ;
#123533 = CARTESIAN_POINT ( 'NONE',  ( -5.302647476720585118, 9.200522799567075083, 0.000000000000000000 ) ) ;
#123534 = CARTESIAN_POINT ( 'NONE',  ( 3.514700139928600198, 1.598748483301600354, 0.7592613872578843903 ) ) ;
#123536 = CARTESIAN_POINT ( 'NONE',  ( 5.970342212645192603, -2.175549559325986149, -0.7227481681704952532 ) ) ;
#123535 = CARTESIAN_POINT ( 'NONE',  ( 7.713663051532233972, 7.963971413067895355, -0.7998128361456341429 ) ) ;
#123537 = CARTESIAN_POINT ( 'NONE',  ( 5.349485151062911115, 1.838858031828109363, -0.09410559872920226665 ) ) ;
#123538 = CARTESIAN_POINT ( 'NONE',  ( -3.086452525405351643, 6.752611712948207057, 0.7998128361456341429 ) ) ;
#123539 = UNCERTAINTY_MEASURE_WITH_UNIT (LENGTH_MEASURE( 1.000000000000000082E-05 ), #102807, 'distance_accuracy_value', 'NONE');
#123540 = CARTESIAN_POINT ( 'NONE',  ( 6.017560223340764125, -1.214513600917455083, -1.823921334435735231 ) ) ;
#123541 = CARTESIAN_POINT ( 'NONE',  ( -4.243865776277440993, 4.909930479533815451, -1.199719254218446718 ) ) ;
#123542 = CARTESIAN_POINT ( 'NONE',  ( -9.920930332858638678, -7.768188185258915190, 0.4648879685169945430 ) ) ;
#123543 = CARTESIAN_POINT ( 'NONE',  ( 6.285608408418759119, -1.950803066209889636, 0.6937918898708083093 ) ) ;
#123544 = CARTESIAN_POINT ( 'NONE',  ( -0.04763828917917976857, -1.313539345393003321, 1.530161206715647149 ) ) ;
#123545 = CARTESIAN_POINT ( 'NONE',  ( -1.500000000000001332, -0.8187499993171781787, 0.000000000000000000 ) ) ;
#123546 = CARTESIAN_POINT ( 'NONE',  ( 4.020081831311307141, -0.9914672019816127557, -1.651657144357060014 ) ) ;
#123547 = CARTESIAN_POINT ( 'NONE',  ( -0.6823417656250039265, 10.56770833367473550, -1.181850606188755259 ) ) ;
#123548 = CARTESIAN_POINT ( 'NONE',  ( -2.725000000000000089, 0.000000000000000000, 0.000000000000000000 ) ) ;
#123549 = CARTESIAN_POINT ( 'NONE',  ( 6.363548717301088509, -1.704009271243651868, -1.262090224194649446 ) ) ;
#123551 = ORIENTED_EDGE ( 'NONE', *, *, #175718, .T. ) ;
#123550 = CARTESIAN_POINT ( 'NONE',  ( 2.835626683552519012, 6.459981564119914310, 0.000000000000000000 ) ) ;
#123553 =( LENGTH_UNIT ( ) NAMED_UNIT ( * ) SI_UNIT ( .MILLI., .METRE. ) );
#123552 = CARTESIAN_POINT ( 'NONE',  ( -4.258669648468323743, 6.061810238003387141, 1.443375672974065660 ) ) ;
#123554 = CARTESIAN_POINT ( 'NONE',  ( 9.028840231696797503, 12.62106513936658203, -1.199719254218446718 ) ) ;
#123555 = DIRECTION ( 'NONE',  ( -0.6483454320283799088, 0.000000000000000000, 0.7613463080411786432 ) ) ;
#123556 = CARTESIAN_POINT ( 'NONE',  ( -5.983791420057156252, 7.107340751733106643, 1.079986564815892613 ) ) ;
#123557 = CARTESIAN_POINT ( 'NONE',  ( 11.83077207345802506, 7.766074702148943132, -1.743650018162308912 ) ) ;
#123558 = CARTESIAN_POINT ( 'NONE',  ( -1.448815997565382929, 7.903552007303741966, 10.65195286442484424 ) ) ;
#123559 = CARTESIAN_POINT ( 'NONE',  ( 1.310910670669521272, -1.548711629584406113, 1.204245502051364936 ) ) ;
#123560 = CARTESIAN_POINT ( 'NONE',  ( 1.364683531249988535, 1.676041667008085101, 0.7879004041258500513 ) ) ;
#123561 = CARTESIAN_POINT ( 'NONE',  ( -1.500000000000043299, 3.670833333333355153, 0.8660254037844216102 ) ) ;
#123562 = CIRCLE ( 'NONE', #185610, 11.92000000000000171 ) ;
#123563 = CARTESIAN_POINT ( 'NONE',  ( 0.4497679408741364071, 1.527348849510310247, 1.386460675282843447 ) ) ;
#123564 = CARTESIAN_POINT ( 'NONE',  ( -8.809047120577080392, 11.30030761213851953, 1.599625672291269396 ) ) ;
#123565 = CARTESIAN_POINT ( 'NONE',  ( -4.243338890952892406, 7.894386439512932618, -0.7216878364870257245 ) ) ;
#123566 = CARTESIAN_POINT ( 'NONE',  ( 0.5676901151186209971, 0.2185747425910676001, -2.251950761720759253 ) ) ;
#123568 = ORIENTED_EDGE ( 'NONE', *, *, #202457, .F. ) ;
#123567 = CARTESIAN_POINT ( 'NONE',  ( -4.381256195510448315, 8.263215994737505454, 1.040834085586084257E-14 ) ) ;
#123570 = EDGE_CURVE ( 'NONE', #146015, #19327, #145621, .T. ) ;
#123569 = CARTESIAN_POINT ( 'NONE',  ( 0.7499999999999885647, -1.235416665983847473, 1.299038105676657340 ) ) ;
#123571 = CARTESIAN_POINT ( 'NONE',  ( 1.774454573425466863, -1.774572579973210384, -0.5916213571805841731 ) ) ;
#123572 = CARTESIAN_POINT ( 'NONE',  ( 0.2461560209003906818, 1.715711078377361032, -0.2512605247984560086 ) ) ;
#123574 = CARTESIAN_POINT ( 'NONE',  ( 4.142245973918059043, 0.5854081421233224836, 2.111838497463234710 ) ) ;
#123573 = CARTESIAN_POINT ( 'NONE',  ( -0.6801582343750213200, 1.348958333674710186, -1.178068619123886718 ) ) ;
#123575 = CARTESIAN_POINT ( 'NONE',  ( 4.331326240856082421, 0.1090238329626690705, 2.305124713103424483 ) ) ;
#123576 = CARTESIAN_POINT ( 'NONE',  ( 6.591097270071800907, 1.795350502275098403, -1.011519373207786288 ) ) ;
#123577 = CARTESIAN_POINT ( 'NONE',  ( 2.396341059777199689, 1.559625748545325319, -1.156842939599848741 ) ) ;
#123578 = CARTESIAN_POINT ( 'NONE',  ( -6.358410854684796831, 6.520493539994793863, -0.7216878364870267237 ) ) ;
#123579 = FACE_OUTER_BOUND ( 'NONE', #29833, .T. ) ;
#123580 = CARTESIAN_POINT ( 'NONE',  ( 4.851869265964163347, -1.501451181749386743, -1.497782127133556518 ) ) ;
#123581 = CARTESIAN_POINT ( 'NONE',  ( 3.990861413484114273, -2.010826503599131065, 0.1511389102963680842 ) ) ;
#123582 = CARTESIAN_POINT ( 'NONE',  ( -6.033015167956818026, 6.140865238812146742, -0.7216878364870267237 ) ) ;
#123583 = CARTESIAN_POINT ( 'NONE',  ( -6.851666526859749418, 9.086973262793417661, -1.599625672291271394 ) ) ;
#123584 = CARTESIAN_POINT ( 'NONE',  ( 10.07387183015377197, 11.71160420905630062, -1.199719254218440723 ) ) ;
#123585 = CARTESIAN_POINT ( 'NONE',  ( 0.4514209555319322331, 0.5758240286459560542, -1.732582669633643047 ) ) ;
#123586 = CARTESIAN_POINT ( 'NONE',  ( -4.613517410400161722, 8.604463755433990002, -0.7998128361456362523 ) ) ;
#123587 = CARTESIAN_POINT ( 'NONE',  ( -0.04160626335162843220, 15.48012587866529444, 11.99061301703373772 ) ) ;
#123588 = CARTESIAN_POINT ( 'NONE',  ( -9.669761313225400556, 3.035266360176858136, 6.558537842936834394 ) ) ;
#123589 = VERTEX_POINT ( 'NONE', #140039 ) ;
#123590 = CARTESIAN_POINT ( 'NONE',  ( 5.524313221898556669, 1.229557446212639071, -1.653754484787550494 ) ) ;
#123591 = CARTESIAN_POINT ( 'NONE',  ( -5.926322542504864899, 8.967774495347393682, -1.082531754730549967 ) ) ;
#123592 = CARTESIAN_POINT ( 'NONE',  ( 7.973603738168424826, 8.475161580717541554, 0.000000000000000000 ) ) ;
#123593 = CARTESIAN_POINT ( 'NONE',  ( -4.090809663021341969, 5.795697244990093644, 1.599625672291267398 ) ) ;
#123594 = CARTESIAN_POINT ( 'NONE',  ( -9.110189153378817295, 12.71597221466224603, 1.199719254218462483 ) ) ;
#123595 = CARTESIAN_POINT ( 'NONE',  ( 4.090493647085408746, -1.161108546167070488, 1.652349136562575760 ) ) ;
#123597 = ORIENTED_EDGE ( 'NONE', *, *, #146492, .F. ) ;
#123596 = CARTESIAN_POINT ( 'NONE',  ( 5.672587799981195111, 0.8983335965149964464, 2.031727793752806210 ) ) ;
#123599 = CARTESIAN_POINT ( 'NONE',  ( 8.785320351975350661, 9.351887953500479966, -0.7216878364870197293 ) ) ;
#123598 = CARTESIAN_POINT ( 'NONE',  ( -7.910256278930404505, 8.193330178365746619, -0.7998128361456362523 ) ) ;
#123600 = CARTESIAN_POINT ( 'NONE',  ( 4.957477724091233995, 8.935474444748447098, -0.7998128361456281477 ) ) ;
#123601 = CARTESIAN_POINT ( 'NONE',  ( 4.662995224183227982, -1.840047010505897029, -0.9283316357228312832 ) ) ;
#123602 = CARTESIAN_POINT ( 'NONE',  ( 3.850232551101364642, 0.2440307281281335339, -2.001511205109906655 ) ) ;
#123603 = ORIENTED_EDGE ( 'NONE', *, *, #59652, .F. ) ;
#123604 = CARTESIAN_POINT ( 'NONE',  ( 1.907692715643306114, 3.236394383240543959, -0.4609675857477724681 ) ) ;
#123605 = CARTESIAN_POINT ( 'NONE',  ( 4.704842999142070603, 5.447737239542574272, -1.199719254218452047 ) ) ;
#123606 = CIRCLE ( 'NONE', #151191, 6.959052028703005099 ) ;
#123608 = EDGE_LOOP ( 'NONE', ( #72991, #45646, #143114, #138432 ) ) ;
#123607 = CARTESIAN_POINT ( 'NONE',  ( -5.759181390754928742, 9.941071732514568993, 0.000000000000000000 ) ) ;
#123609 = CARTESIAN_POINT ( 'NONE',  ( 5.488371254093075358, 7.473176909139983337, -1.250075884424824757 ) ) ;
#123610 = CARTESIAN_POINT ( 'NONE',  ( 3.901720107437017582, 0.2930258228103881923, 1.994564303527603499 ) ) ;
#123611 = CARTESIAN_POINT ( 'NONE',  ( 2.747807751077631977, 0.6205313035267927546, 1.733543155639664990 ) ) ;
#123612 = CARTESIAN_POINT ( 'NONE',  ( 4.492294583948199360, 8.028511867738709284, 2.499999999999656719 ) ) ;
#123613 = CARTESIAN_POINT ( 'NONE',  ( 1.559632053384899741, -1.981161107035840141, -1.183202272445786907 ) ) ;
#123614 = CARTESIAN_POINT ( 'NONE',  ( 5.408776937209000657, 5.274937613024121674, 0.7998128361456352531 ) ) ;
#123615 = CARTESIAN_POINT ( 'NONE',  ( 4.024825912876791811, 2.051136489140188424, 0.6822911077620784637 ) ) ;
#123616 = CARTESIAN_POINT ( 'NONE',  ( 9.772729797352075920, 10.29593960653257234, -0.7998128361456281477 ) ) ;
#123617 = CARTESIAN_POINT ( 'NONE',  ( -5.551173829791513192, 8.563787670477010394, 1.199719254218452047 ) ) ;
#123618 = PRESENTATION_LAYER_ASSIGNMENT (  '', '', ( #120187 ) ) ;
#123619 = CARTESIAN_POINT ( 'NONE',  ( 3.743815364168050053, -2.214071480395309433, -0.6165714402358390966 ) ) ;
#123620 = CARTESIAN_POINT ( 'NONE',  ( 1.224999999999947020, 2.354166666666674512, 0.7072540797573039217 ) ) ;
#123621 = CARTESIAN_POINT ( 'NONE',  ( 2.852262661058731386, 0.6285613048715790185, 1.762029509812724992 ) ) ;
#123622 = CARTESIAN_POINT ( 'NONE',  ( 6.262572880032761802, -1.394454384559177695, 1.393866484745357459 ) ) ;
#123624 = CARTESIAN_POINT ( 'NONE',  ( -7.910256278930404505, 8.193330178365746619, -0.7998128361456362523 ) ) ;
#123623 = CARTESIAN_POINT ( 'NONE',  ( 0.6823417656249899377, 5.176041667008086655, -1.181850606188754593 ) ) ;
#123626 = CARTESIAN_POINT ( 'NONE',  ( 0.1357705729100426029, -2.015811560716780360, 0.8986578214904348272 ) ) ;
#123625 = CARTESIAN_POINT ( 'NONE',  ( -5.819474248763749635, 7.812472595022922128, -1.599625672291256295 ) ) ;
#123627 = CARTESIAN_POINT ( 'NONE',  ( -1.403499169902657995, 7.376709478543001630, -4.304123474984410613 ) ) ;
#123628 = CARTESIAN_POINT ( 'NONE',  ( 5.087333953625774008, 6.958308917361963886, 1.599625672291267398 ) ) ;
#123629 = CARTESIAN_POINT ( 'NONE',  ( -4.388035272317281077, 8.271124917678806199, 0.7998128361456481317 ) ) ;
#123630 = CIRCLE ( 'NONE', #95888, 1.500000000000000222 ) ;
#123631 = CARTESIAN_POINT ( 'NONE',  ( -0.04765083308772119497, -6.900199406649610623, -9.605391220871888791 ) ) ;
#123632 = CARTESIAN_POINT ( 'NONE',  ( 6.315303677655929704, -0.2418685481465185916, 1.956520841371222952 ) ) ;
#123633 = CARTESIAN_POINT ( 'NONE',  ( 5.778008146871475681, 1.369946362297723264, 1.856932335381543897 ) ) ;
#123634 = CARTESIAN_POINT ( 'NONE',  ( 6.584420904419787668, 1.070383488754884649, -1.522209605261907406 ) ) ;
#123635 = CARTESIAN_POINT ( 'NONE',  ( 3.063389470891558997, 1.739959455442946279, 1.107334787568447165 ) ) ;
#123636 = CARTESIAN_POINT ( 'NONE',  ( 7.483737605063422116, 7.833374748769873719, -0.7216878364870257245 ) ) ;
#123637 = CARTESIAN_POINT ( 'NONE',  ( 7.666209513884374438, 7.908608952478760834, 0.7998128361456281477 ) ) ;
#123638 = CARTESIAN_POINT ( 'NONE',  ( 7.931156673870037643, 8.355363662377600420, -0.7216878364870267237 ) ) ;
#123639 = CARTESIAN_POINT ( 'NONE',  ( 1.364683531249988535, 3.926041667008087543, 0.7879004041258500513 ) ) ;
#123640 = CARTESIAN_POINT ( 'NONE',  ( -11.07131242353766254, 12.30000000000000249, -0.8043462106219255725 ) ) ;
#123641 = CARTESIAN_POINT ( 'NONE',  ( 5.626270559546821204, 6.626699076635176766, 1.082531754730560403 ) ) ;
#123642 = CARTESIAN_POINT ( 'NONE',  ( 5.652828992512394457, -0.5219723807755486389, -2.107401415877676598 ) ) ;
#123644 = CARTESIAN_POINT ( 'NONE',  ( 5.425302022954732628, -1.172690680311109901, -1.419496581506813904 ) ) ;
#123643 = CARTESIAN_POINT ( 'NONE',  ( 2.680963302754415079, 0.4788041664859938318, -0.1016165050511480955 ) ) ;
#123645 = ADVANCED_FACE ( 'NONE', ( #156275 ), #121717, .F. ) ;
#123647 = CARTESIAN_POINT ( 'NONE',  ( 6.620655732516647518, 0.007553340620044743381, 1.826407896915738238 ) ) ;
#123646 = CARTESIAN_POINT ( 'NONE',  ( 1.364683531249990311, 5.613541667008087543, 0.7879004041258500513 ) ) ;
#123648 = CARTESIAN_POINT ( 'NONE',  ( 6.497619750234602698, -2.191128968173004843, 0.05151875470104508997 ) ) ;
#123649 = CARTESIAN_POINT ( 'NONE',  ( 0.7373108528737730705, -1.318359053027039263, -1.327247110734230962 ) ) ;
#123650 = CARTESIAN_POINT ( 'NONE',  ( 0.6325467830279264403, 1.161941506187497364, -1.941124190868536603 ) ) ;
#123651 = CARTESIAN_POINT ( 'NONE',  ( -4.565105001785453531, 7.177652750280781646, 1.346018956990787885 ) ) ;
#123652 = FACE_OUTER_BOUND ( 'NONE', #144440, .T. ) ;
#123653 = CARTESIAN_POINT ( 'NONE',  ( 6.587573780899039555, 6.778200402807202707, -0.2451836268814889253 ) ) ;
#123654 = CARTESIAN_POINT ( 'NONE',  ( -4.407809337774280856, 7.196175756495025055, 1.082531754730549967 ) ) ;
#123655 = CARTESIAN_POINT ( 'NONE',  ( 0.2934254677693093338, 1.784247535656303230, -0.6883866973072181317 ) ) ;
#123656 = CARTESIAN_POINT ( 'NONE',  ( 1.621574733132331358, -0.9795727578338263575, -1.473812506242745179 ) ) ;
#123657 = CARTESIAN_POINT ( 'NONE',  ( 5.971345465650553130, -1.727703365644253086, -1.033000238237492763 ) ) ;
#123659 = CARTESIAN_POINT ( 'NONE',  ( 3.427252967507479209, -1.452606091845513037, -1.248918174067833009 ) ) ;
#123658 = CARTESIAN_POINT ( 'NONE',  ( -4.406036734316900905, 5.203092947200234519, -1.082531754730543971 ) ) ;
#123660 = CARTESIAN_POINT ( 'NONE',  ( 2.333974999846879061, 5.874721266463329705, -0.7998128361456291469 ) ) ;
#123661 = CARTESIAN_POINT ( 'NONE',  ( 4.721133488271325618, -1.758435714881977141, -0.8873337903104687729 ) ) ;
#123662 = CARTESIAN_POINT ( 'NONE',  ( 6.222917004181202749, 1.493787235515126044, -1.359621011941100743 ) ) ;
#123663 = CARTESIAN_POINT ( 'NONE',  ( -2.948008335967658322, 5.526761261015804116, 1.199719254218462483 ) ) ;
#123664 = CARTESIAN_POINT ( 'NONE',  ( 2.781945002432617997, -0.9632652739061451364, 1.603442845774772474 ) ) ;
#123666 = EDGE_LOOP ( 'NONE', ( #40534, #189743, #160496, #163807, #123159 ) ) ;
#123665 = CARTESIAN_POINT ( 'NONE',  ( 4.775862138867135620, 0.9967549737653296216, 1.407514542897546850 ) ) ;
#123668 = CARTESIAN_POINT ( 'NONE',  ( 3.985733972737593778, 6.633478153960411738, -1.082531754730548412 ) ) ;
#123667 = CARTESIAN_POINT ( 'NONE',  ( 2.807470779205251343, 1.864772411128329477, 1.179945617918669143 ) ) ;
#123669 = CARTESIAN_POINT ( 'NONE',  ( -1.364683531250012516, 3.051041667008083547, -0.7879004041258289570 ) ) ;
#123670 = CARTESIAN_POINT ( 'NONE',  ( 6.795372052238223048, -1.752927774724974297, 0.8811163259476795240 ) ) ;
#123671 = CARTESIAN_POINT ( 'NONE',  ( 7.401861798056875053, 10.72292363345333399, -1.199719254218441611 ) ) ;
#123672 = CARTESIAN_POINT ( 'NONE',  ( -3.929058411375401683, -1.000000000000000888, -0.7500000000000006661 ) ) ;
#123673 = CARTESIAN_POINT ( 'NONE',  ( -0.2104748580754413345, 7.629137130509052511, -2.703678718140525739 ) ) ;
#123674 = CARTESIAN_POINT ( 'NONE',  ( -4.578903193113314174, 6.365139696764064325, 1.599625672291267175 ) ) ;
#123675 = DIRECTION ( 'NONE',  ( 0.000000000000000000, 1.000000000000000000, 0.000000000000000000 ) ) ;
#123676 = ORIENTED_EDGE ( 'NONE', *, *, #182811, .F. ) ;
#123677 = CARTESIAN_POINT ( 'NONE',  ( 2.400909748719297188, 0.4512941399696759337, 2.020426262116347349 ) ) ;
#123678 = CARTESIAN_POINT ( 'NONE',  ( 1.499999999999987121, 3.045833333333353377, -0.8660254037844262731 ) ) ;
#123679 = CARTESIAN_POINT ( 'NONE',  ( 4.578903193113299963, 6.365139696764064325, 1.599625672291267398 ) ) ;
#123680 = CARTESIAN_POINT ( 'NONE',  ( 4.634908411025333130, 6.500755460986618495, 1.599625672291268286 ) ) ;
#123681 = CARTESIAN_POINT ( 'NONE',  ( 0.2233145766990596859, 1.758413993963375610, 0.9933387185240820649 ) ) ;
#123682 = FACE_OUTER_BOUND ( 'NONE', #58238, .T. ) ;
#123683 = B_SPLINE_CURVE_WITH_KNOTS ( 'NONE', 3,
 ( #210302, #62996, #66157, #192987, #161589, #15297, #82436, #129166, #195143, #31582, #162649, #213488, #61942, #44641, #46778, #110756, #97656, #164767, #163715, #130216, #181010, #32631, #128100, #194058, #45711, #47851, #197254, #112892, #111830, #29448, #48893, #178904, #95539, #113962, #13176, #79254, #30518, #96599, #14222, #98708, #84578, #101899, #167963, #118212, #1168, #17419, #83502, #116070, #117141, #200439, #33692, #152782, #67233, #35822, #100821, #151729, #20624, #133367, #52085, #102968, #183144, #185261, #70432, #184199, #150665, #19569, #2227, #86712, #149584, #199373, #3301, #68303, #134436, #182060, #34748, #4363, #166906, #51019, #135478, #202568, #18499, #169026, #85644, #132302, #36885, #69370, #136549, #201500, #53146, #165834, #119277, #49950, #198309, #99768, #33308, #115688, #178510, #14907, #130886, #65777, #149200, #113575, #196880, #47460, #81001, #62606, #48517, #181681, #114639, #112500, #177444, #83120, #179577, #32253, #95142, #98323, #29059, #775, #66841, #99393, #165446, #161192, #17041, #15972, #180631, #12780, #31199, #164388, #97273, #147089, #128768, #82058, #132985, #148150, #30122, #78853, #198986, #163327, #214151, #144974, #129839, #131927, #213112, #197937, #64744, #49563, #210979, #111440, #46382, #194744, #96211, #195820, #162262, #13849, #79925, #146032, #212041, #63683, #201126, #103669, #20253, #22377, #3988, #102592, #35439, #72196, #153478, #200067, #70057, #86337, #1853, #187027, #150286, #116757, #18110, #136168, #5050, #2919, #183830, #34374, #21306, #50631, #117838, #154547, #100447, #182756, #84196, #138305, #203264, #166520, #152408, #202186, #119975, #53844, #101516, #67913, #134059, #51718, #19188, #185955, #167587, #170786, #85263, #54910, #121061, #151350, #88488, #118899, #184883, #36508, #135110, #38661, #6128, #37587, #168649, #169717, #87414, #104739, #68992, #52764, #71126, #137242, #28441, #11104, #30590, #209293, #208238, #13253, #212507, #43649, #129241, #109765, #96674, #126021, #193061, #110821, #59870, #12180, #144376, #60941, #112964, #78252, #210375, #127097, #146487, #44714, #211441, #62015, #76122, #195214, #108691, #178976, #29516, #128171, #26292, #176828, #194133, #94533, #160572, #142225, #45783, #124960, #111900, #177903, #174719, #14296, #80391, #95609, #92407, #162725, #161658, #79324, #145441, #63073, #46850, #158446, #190922, #191983, #42586, #10046, #143302, #175773, #93467, #27366, #159506, #77180, #165, #117215, #33764, #166981, #180032, #64148, #16431, #101970, #51091, #35893, #183214, #165907, #200511, #84650, #66232, #130290, #31654, #17491, #18572, #82509, #197329, #47926, #34818, #50022, #115088, #1241, #48971, #181084, #164839, #32702, #97730, #65181, #132380, #151799, #98784, #83578, #131335, #81460, #147538, #114038, #148596, #99842, #163788, #168038, #198381, #149660, #116146, #100894, #118283, #182134, #67301, #134507, #133441, #199448, #150739, #2300, #68376, #52156, #184268, #19641, #213559, #15367, #85712, #196279, #169095, #121504, #104110, #123649, #87856, #86785, #106289, #91073, #136617, #7646, #202642, #3374, #156058, #56422, #57488, #70501, #187476, #73731, #186404, #38041, #204769, #20694, #122583, #152854, #4432, #188545, #6575, #54292, #120429, #139827, #22822, #39106, #170159, #189611, #153928, #21747, #172309 ),
 .UNSPECIFIED., .F., .F.,
 ( 4, 1, 1, 1, 1, 1, 1, 1, 1, 1, 1, 1, 1, 1, 1, 1, 1, 1, 1, 1, 1, 1, 1, 1, 1, 1, 1, 1, 1, 1, 1, 1, 1, 1, 1, 1, 1, 1, 1, 1, 1, 1, 1, 1, 1, 1, 1, 1, 1, 1, 1, 1, 1, 1, 1, 1, 1, 1, 1, 1, 1, 1, 1, 1, 1, 1, 1, 1, 1, 1, 1, 1, 1, 1, 1, 1, 1, 1, 1, 1, 1, 1, 1, 1, 1, 1, 1, 1, 1, 1, 1, 1, 1, 1, 1, 1, 1, 1, 1, 1, 1, 1, 1, 1, 1, 1, 1, 1, 1, 1, 1, 1, 1, 1, 1, 1, 1, 1, 1, 1, 1, 1, 1, 1, 1, 1, 1, 1, 1, 1, 1, 1, 1, 1, 1, 1, 1, 1, 1, 1, 1, 1, 1, 1, 1, 1, 1, 1, 1, 1, 1, 1, 1, 1, 1, 1, 1, 1, 1, 1, 1, 1, 1, 1, 1, 1, 1, 1, 1, 1, 1, 1, 1, 1, 1, 1, 1, 1, 1, 1, 1, 1, 1, 1, 1, 1, 1, 1, 1, 1, 1, 1, 1, 1, 1, 1, 1, 1, 1, 1, 1, 1, 1, 1, 1, 1, 1, 1, 1, 1, 1, 1, 1, 1, 1, 1, 1, 1, 1, 1, 1, 1, 1, 1, 1, 1, 1, 1, 1, 1, 1, 1, 1, 1, 1, 1, 1, 1, 1, 1, 1, 1, 1, 1, 1, 1, 1, 1, 1, 1, 1, 1, 1, 1, 1, 1, 1, 1, 1, 1, 1, 1, 1, 1, 1, 1, 1, 1, 1, 1, 1, 1, 1, 1, 1, 1, 1, 1, 1, 1, 1, 1, 1, 1, 1, 1, 1, 1, 1, 1, 1, 1, 1, 1, 1, 1, 1, 1, 1, 1, 1, 1, 1, 1, 1, 1, 1, 1, 1, 1, 1, 1, 1, 1, 1, 1, 1, 1, 1, 1, 1, 1, 1, 1, 1, 1, 1, 1, 1, 1, 1, 1, 1, 1, 1, 1, 1, 1, 1, 1, 1, 1, 1, 1, 1, 1, 1, 1, 1, 1, 1, 1, 1, 1, 1, 1, 1, 1, 1, 1, 1, 1, 1, 1, 1, 1, 1, 1, 1, 1, 1, 1, 1, 1, 1, 1, 1, 1, 1, 1, 1, 1, 1, 1, 4 ),
 ( 0.000000000000000000, 0.002600154539856827565, 0.005208839490340733125, 0.007813275572638063438, 0.01041576435696154809, 0.01302135854728175661, 0.01562456786780599440, 0.01822932761385693060, 0.02083324874646079461, 0.02343713590986815087, 0.02604192363554110393, 0.02864519953128016536, 0.03125045858075606309, 0.03385359029894085409, 0.03645870005206112291, 0.03906221013386886737, 0.04166657361863843057, 0.04427092160485841116, 0.04687444683368256759, 0.04947954930481244379, 0.05208268618576387260, 0.05468794662449812799, 0.05729120536831356497, 0.05989601299138836571, 0.06249988999545372931, 0.06510378435733490954, 0.06770858081828938502, 0.07031184975024351580, 0.07291710771924506118, 0.07552024060328325905, 0.07812534933470290099, 0.08072885870519988516, 0.08333322157114708695, 0.08593756915452624434, 0.08854109358761537429, 0.09114619558392741960, 0.09374933183658358538, 0.09635459170495851156, 0.09895784999447977681, 0.1015626569530685003, 0.1041665336043751944, 0.1067704272253022224, 0.1093752232910748662, 0.1119784915631429623, 0.1145837490571069844, 0.1171868814509031548, 0.1197919896162490533, 0.1223954986480551566, 0.1249998608471283579, 0.1276042081199000311, 0.1302077318846941445, 0.1328128334964322199, 0.1354159692195129883, 0.1380212286176593917, 0.1406244865514671982, 0.1432292929439143159, 0.1458331693420142072, 0.1484370623210626572, 0.1510418580899855479, 0.1536451258019158050, 0.1562503829188521542, 0.1588535149221727560, 0.1614586226195926788, 0.1640621314121666618, 0.1666664930431534797, 0.1692708401040713406, 0.1718743633000545112, 0.1744794646253388370, 0.1770825999186152189, 0.1796878589445308205, 0.1822911166222762891, 0.1848959225469683498, 0.1874997987909985397, 0.1901036912273387502, 0.1927084867977703619, 0.1953117540492253223, 0.1979170108871138589, 0.2005201425997050479, 0.2031252499273119572, 0.2057287585800815777, 0.2083331197417381819, 0.2109374666895270922, 0.2135409894161511279, 0.2161460905530729892, 0.2187492255162853672, 0.2213544842679382729, 0.2239577417892439637, 0.2265625473445374016, 0.2291664235336075273, 0.2317703155263790282, 0.2343751109966507595, 0.2369783778872631419, 0.2395836345440564008, 0.2421867660656364940, 0.2447918731215153465, 0.2473953817338825356, 0.2499997425249363969, 0.2526040894582959329, 0.2552076118149841921, 0.2578127128616094499, 0.2604158475944712281, 0.2630211061698037311, 0.2656243636342671688, 0.2682291689184919115, 0.2708330451516883230, 0.2734369368000036937, 0.2760417322684234342, 0.2786449988978000336, 0.2812502554714267355, 0.2838533869016899303, 0.2864584937839013135, 0.2890620024552456591, 0.2916663629743991848, 0.2942707099920074398, 0.2968742320781582733, 0.2994793331325310004, 0.3020824677347322962, 0.3046877262316646240, 0.3072909837388622112, 0.3098957888503254821, 0.3124996652267145181, 0.3151035566296633839, 0.3177083521945192612, 0.3203116186622446127, 0.3229168752506134110, 0.3255200066892336430, 0.3281251134958176330, 0.3307286223255002655, 0.3333329826714347410, 0.3359373298719517953, 0.3385408517869427647, 0.3411459529470890484, 0.3437490875183005223, 0.3463543460347343617, 0.3489576036842249041, 0.3515624087212146920, 0.3541662853398466204, 0.3567701765964986227, 0.3593749723560626386, 0.3619782387617029862, 0.3645834954627060198, 0.3671866270093405715, 0.3697917338383204244, 0.3723952429256875973, 0.3749996031970665444, 0.3776039506791386557, 0.3802074725223298923, 0.3828125738862612759, 0.3854157085261381011, 0.3880209671599602617, 0.3906242250512887426, 0.3932290301120778819, 0.3958329070719905363, 0.3984367982813996067, 0.4010415943339316058, 0.4036448607770379837, 0.4062501176885546794, 0.4088532494428480657, 0.4114583563922335485, 0.4140618658366201910, 0.4166662261320933647, 0.4192705739943561327, 0.4218740958650940009, 0.4244791975308115917, 0.4270823323389966175, 0.4296875911880828069, 0.4322908494207843844, 0.4348956546036337745, 0.4374995320038561619, 0.4401034232650644085, 0.4427082197088152427, 0.4453114862889279713, 0.4479167435088288185, 0.4505198755704162283, 0.4531249827382076711, 0.4557284926389418844, 0.4583328530571487147, 0.4609372013982309668, 0.4635407233958523388, 0.4661458254613498609, 0.4687489605374778323, 0.4713542196996960976, 0.4739574783732994345, 0.4765622837764619812, 0.4791661617160185016, 0.4817700531280592058, 0.4843748500612748420, 0.4869781168779269698, 0.4895833745040767959, 0.4921865069725880892, 0.4947916144567798824, 0.4973951249131855490, 0.4999994855527590265, 0.5026038344712867589, 0.5052073566951218453, 0.5078124592583899144, 0.5104155947020908579, 0.5130208542753056378, 0.5156241134893367883, 0.5182289192110610676, 0.5208327977889742888, 0.5234366894508762913, 0.5260414869718011976, 0.5286447541245218318, 0.5312500122547839654, 0.5338531452298473923, 0.5364582531284315392, 0.5390617642398328746, 0.5416661251994032700, 0.5442704747940029231, 0.5468739973433798252, 0.5494791005024090014, 0.5520822364133124438, 0.5546874964953879550, 0.5572907563493740835, 0.5598955624879079496, 0.5624994418032033261, 0.5651033338139942463, 0.5677081320208752224, 0.5703113996091939697, 0.5729166583414331271, 0.5755197919226788805, 0.5781249003336490500, 0.5807284121993739889, 0.5833327735775721834, 0.5859371239468746939, 0.5885406469211225122, 0.5911457507739076300, 0.5937488872516457628, 0.5963541479404496082, 0.5989574085339228748, 0.6015622151875171797, 0.6041660953392257172, 0.6067699877979360057, 0.6093747867890261238, 0.6119780549124759217, 0.6145833143445629254, 0.6171864486316270826, 0.6197915576529816617, 0.6223950703723655220, 0.6249994322678273928, 0.6276037835104713025, 0.6302073070089242446, 0.6328124116534677990, 0.6354155487976793637, 0.6380208101910863627, 0.6406240716235875876, 0.6432288788904997334, 0.6458327599776627626, 0.6484366529833293091, 0.6510414528568908565, 0.6536447216150126360, 0.6562499818448275235, 0.6588531169373553764, 0.6614582266671018562, 0.6640617403394915019, 0.6666661028508605868, 0.6692704550654967610, 0.6718739791874978051, 0.6744790847218130603, 0.6770822226321474568, 0.6796874848280434200, 0.6822907471991253026, 0.6848955551776233497, 0.6874994372992955238, 0.6901033309509650993, 0.6927081318052739078, 0.6953114012976200353, 0.6979166624230551674, 0.7005197984207056638, 0.7031249089568636368, 0.7057284236816204759, 0.7083327869075525252, 0.7109371401928469281, 0.7135406650377511539, 0.7161457715598668061, 0.7187489103359874232, 0.7213541734322722609, 0.7239574368415039318, 0.7265622456298695964, 0.7291661288851226663, 0.7317700232818561412, 0.7343748252152053624, 0.7369780955413426371, 0.7395833576603073611, 0.7421864946627563242, 0.7447916061033615920, 0.7473951219798656842, 0.7499994860190324353, 0.7526038404736700160, 0.7552073661408488237, 0.7578124737488122209, 0.7604156134903999886, 0.7630208775849919300, 0.7656241421319622820, 0.7682289518284949326, 0.7708328363164217434, 0.7734367315572975299, 0.7760415346680002990, 0.7786448059275148381, 0.7812500691379388185, 0.7838532072448821664, 0.7864583196879902927, 0.7890618368156444573, 0.7916662017667361884, 0.7942705574894247667, 0.7968740840782696511, 0.7994791928701499018, 0.8020823336769073997, 0.8046875988677468783, 0.8072908646520678966, 0.8098956753550886623, 0.8124995611748068169, 0.8151034573589240884, 0.8177082617453185209, 0.8203115340378186460, 0.8229167984376549727, 0.8255199377488137147, 0.8281250512925039109, 0.8307285697707365024, 0.8333329357324672504, 0.8359372928219411802, 0.8385408204318668401, 0.8411459305057594760, 0.8437490724774151518, 0.8463543388624672481, 0.8489576059837783406, 0.8515624177916331083, 0.8541663050422881875, 0.8567702022687715413, 0.8593750080292236193, 0.8619782814543437421, 0.8645835471415733720, 0.8671866877566964948, 0.8697918024990743957, 0.8723953224273439666, 0.8749996894984543028, 0.8776040480534781363, 0.8802075767839265819, 0.8828126882379567775, 0.8854158314742670566, 0.8880210991515266050, 0.8906243677094983768, 0.8932291807205616774, 0.8958330695013316802, 0.8984369678693342465, 0.9010417751022415933, 0.9036450497596462128, 0.9062503168322812996, 0.9088534588511494317, 0.9114585748903522022, 0.9140620963681507227, 0.9166664646474114164, 0.9192708247667824573, 0.9218743547172278952, 0.9244794676495572405, 0.9270826122503010858, 0.9296878813177945622, 0.9322911514121841048, 0.9348959657248061550, 0.9374998561347748227, 0.9401037557438677306, 0.9427085645475906661, 0.9453118405358371668, 0.9479171090940153865, 0.9505202526155902554, 0.9531253700418979014, 0.9557288931959170286, 0.9583332627756006028, 0.9609376244112938226, 0.9635411559431285022, 0.9661462708106475228, 0.9687494151757961580, 0.9713546862302190332, 0.9739579640138142924, 0.9765627705390533819, 0.9791666547386930208, 0.9817705986233274951, 0.9843753609709087193, 0.9869785915570626900, 0.9895841932699848131, 0.9921866851465583892, 0.9947911401134668097, 0.9973998225951543617, 1.000000000000000000 ),
 .UNSPECIFIED. ) ;
#123684 = CARTESIAN_POINT ( 'NONE',  ( -1.201851678989727383E-14, 3.446875000341421469, -1.575800808251660134 ) ) ;
#123686 = CARTESIAN_POINT ( 'NONE',  ( 9.571693261567961741, 11.22969222899322617, 1.082531754730548412 ) ) ;
#123685 = CARTESIAN_POINT ( 'NONE',  ( 6.777797683793751915, -1.903277019102869616, 0.4755351429900215310 ) ) ;
#123687 = CARTESIAN_POINT ( 'NONE',  ( 5.184922634274871989, -1.076153828860962225, -1.704676470440001701 ) ) ;
#123688 = CARTESIAN_POINT ( 'NONE',  ( 4.979654327277899917, -0.6834858053395581612, 1.789849564252174119 ) ) ;
#123689 = CARTESIAN_POINT ( 'NONE',  ( 6.539320575229274901, 4.692178491785949923, 2.665866134390063813 ) ) ;
#123690 = CARTESIAN_POINT ( 'NONE',  ( 2.208753784402537335, 1.959192758111829136, 0.9821998110004713789 ) ) ;
#123692 = AXIS2_PLACEMENT_3D ( 'NONE', #20600, #33665, #52061 ) ;
#123691 = CARTESIAN_POINT ( 'NONE',  ( -0.7500000000000215383, 2.222916667349486453, 1.299038105676671107 ) ) ;
#123693 = CARTESIAN_POINT ( 'NONE',  ( 2.355592738034977263, -1.419685808644566949, -1.281520755053264349 ) ) ;
#123694 = CARTESIAN_POINT ( 'NONE',  ( -5.555090253297260361, 7.504024600312024340, 1.599625672291269396 ) ) ;
#123696 = CARTESIAN_POINT ( 'NONE',  ( 0.3160300859305562593, 1.034144755472726995, -1.730879882831819705 ) ) ;
#123695 = CARTESIAN_POINT ( 'NONE',  ( 1.613391111044842492E-15, 14.84205778326404612, 11.68011747745297590 ) ) ;
#123697 = CARTESIAN_POINT ( 'NONE',  ( 1.364683531249996529, 10.27604166700806765, 0.7879004041258405033 ) ) ;
#123699 = CARTESIAN_POINT ( 'NONE',  ( -6.954406449166956605, 7.078172043641714595, -0.7998128361456362523 ) ) ;
#123698 = CARTESIAN_POINT ( 'NONE',  ( 5.935146830689759234, -1.586316731616247200, -1.512381816529739353 ) ) ;
#123701 = ORIENTED_EDGE ( 'NONE', *, *, #65889, .F. ) ;
#123700 = CARTESIAN_POINT ( 'NONE',  ( 2.994803049195310596, 1.480226043003279424, -0.8850232739186939535 ) ) ;
#123702 = CARTESIAN_POINT ( 'NONE',  ( 6.310795917644286490, -0.5669512758468171487, -2.043305014803979525 ) ) ;
#123703 = CARTESIAN_POINT ( 'NONE',  ( 5.671388329218120639, 5.511041227042920099, 1.040834085586084257E-14 ) ) ;
#123704 = CARTESIAN_POINT ( 'NONE',  ( -0.3000000000000051514, 3.322650755865477645, -0.5865692111443002732 ) ) ;
#123705 = CARTESIAN_POINT ( 'NONE',  ( 0.6605093422152423788, -0.6574743052488278838, -1.848563176889833626 ) ) ;
#123706 = DIRECTION ( 'NONE',  ( 0.000000000000000000, 1.000000000000000000, 0.000000000000000000 ) ) ;
#123707 = CARTESIAN_POINT ( 'NONE',  ( 6.356075086708249167, 6.309842444114747373, -0.7998128361456281477 ) ) ;
#123708 = CARTESIAN_POINT ( 'NONE',  ( 0.1399997263885795207, 2.876830203203218694, -2.488333633689450597 ) ) ;
#123709 = ORIENTED_EDGE ( 'NONE', *, *, #103355, .T. ) ;
#123710 = ORIENTED_EDGE ( 'NONE', *, *, #9209, .T. ) ;
#123711 = CARTESIAN_POINT ( 'NONE',  ( 2.807043740381453656, 1.552634882062135624, -0.9328946631028020020 ) ) ;
#123712 = ORIENTED_EDGE ( 'NONE', *, *, #132981, .T. ) ;
#123713 = CARTESIAN_POINT ( 'NONE',  ( 9.915090410295563927, 10.46202698829998567, -0.7998128361456281477 ) ) ;
#123714 = CARTESIAN_POINT ( 'NONE',  ( 5.761288931164342486, 5.686201605971993978, -0.7998128361456481317 ) ) ;
#123715 = EDGE_CURVE ( 'NONE', #12133, #45181, #119081, .T. ) ;
#123716 = CARTESIAN_POINT ( 'NONE',  ( 3.404753564208697014, -0.3562933990706117493, -1.775892323017129737 ) ) ;
#123717 = CARTESIAN_POINT ( 'NONE',  ( 7.973603738168424826, 8.475161580717541554, 0.000000000000000000 ) ) ;
#123718 = CARTESIAN_POINT ( 'NONE',  ( 5.892592298951464969, 5.976936425253049912, 0.01597356071081010298 ) ) ;
#123720 = CARTESIAN_POINT ( 'NONE',  ( 1.364683531249996529, 14.21354166700806942, 0.7879004041258405033 ) ) ;
#123719 = CARTESIAN_POINT ( 'NONE',  ( 5.301151097710674165, -1.596257866726397134, 0.9565186216247966167 ) ) ;
#123721 = CARTESIAN_POINT ( 'NONE',  ( 2.899894056866093361, -0.9465274319002868753, -1.665356295385928442 ) ) ;
#123722 = CARTESIAN_POINT ( 'NONE',  ( 1.043660158496478196, 0.7440559408637310579, -1.667260813828251642 ) ) ;
#123723 = CARTESIAN_POINT ( 'NONE',  ( 4.781538967055604772, 8.149846084806789293, 0.7984123896064146964 ) ) ;
#123724 = CARTESIAN_POINT ( 'NONE',  ( -10.93365108933372198, 4.740440605563193799, -4.433365903526399698 ) ) ;
#123725 = AXIS2_PLACEMENT_3D ( 'NONE', #161234, #193721, #45364 ) ;
#123726 = CARTESIAN_POINT ( 'NONE',  ( 5.748548729368831545, 7.266256959964179529, 1.200940202139972435 ) ) ;
#123727 = CARTESIAN_POINT ( 'NONE',  ( 8.961696533999443659, 14.59015583931033611, 8.974872064516899783 ) ) ;
#123728 = DIRECTION ( 'NONE',  ( 0.6507913734559640506, -0.7592566023653004592, 0.000000000000000000 ) ) ;
#123729 = DIRECTION ( 'NONE',  ( 0.000000000000000000, 1.000000000000000000, 0.000000000000000000 ) ) ;
#123730 = CARTESIAN_POINT ( 'NONE',  ( 7.293923454472087897, 8.572294120714675003, 1.082531754730558626 ) ) ;
#123731 = CARTESIAN_POINT ( 'NONE',  ( 6.104353324094977218, 1.967046249225043342, 0.1001853051637753428 ) ) ;
#123732 = CARTESIAN_POINT ( 'NONE',  ( -2.415323921528888196, 5.969628341758991930, 0.7998128361456341429 ) ) ;
#123733 = FILL_AREA_STYLE_COLOUR ( '', #87051 ) ;
#123734 = CARTESIAN_POINT ( 'NONE',  ( 1.148509085094330029, -1.646982989033857869, 1.287593708729701802 ) ) ;
#123735 = CARTESIAN_POINT ( 'NONE',  ( 6.440456187458303283, 1.905530750978209120, 0.2820203164855574207 ) ) ;
#123736 = CARTESIAN_POINT ( 'NONE',  ( -5.311043488251275591, 7.219303374425030562, -1.599625672291256295 ) ) ;
#123737 = CARTESIAN_POINT ( 'NONE',  ( 2.871877888313049354, 0.9750061419492547232, 1.543211660213184899 ) ) ;
#123738 = CARTESIAN_POINT ( 'NONE',  ( 2.912931060594741162, 1.598032330669514778, -1.522282275181946032 ) ) ;
#123739 = DIRECTION ( 'NONE',  ( -0.7806247498001170904, 4.926614671774123060E-13, 0.6249999999996038724 ) ) ;
#123740 = CARTESIAN_POINT ( 'NONE',  ( 0.6328886395040033142, 1.767934563615305432, 0.7296191750566642931 ) ) ;
#123741 = CARTESIAN_POINT ( 'NONE',  ( 1.574589453129974004, 1.325232347829819135, -1.457171473731319278 ) ) ;
#123742 = CARTESIAN_POINT ( 'NONE',  ( 2.278764488077251738, 1.774667200368160280, -0.7891824313753895703 ) ) ;
#123743 = ORIENTED_EDGE ( 'NONE', *, *, #87019, .T. ) ;
#123744 = CARTESIAN_POINT ( 'NONE',  ( 3.128205532383693921, 2.800000000000115730, 2.480558432692051340 ) ) ;
#123746 = CARTESIAN_POINT ( 'NONE',  ( 6.596546450148484730, 1.840605976333910654, 0.2736291870141689397 ) ) ;
#123745 = CARTESIAN_POINT ( 'NONE',  ( -6.005335696210345020, 5.970922831858983315, 0.7998128361456281477 ) ) ;
#123747 = CARTESIAN_POINT ( 'NONE',  ( 4.736594563127852098, 6.619389305106191834, -1.599625672291273171 ) ) ;
#123748 = FACE_OUTER_BOUND ( 'NONE', #9712, .T. ) ;
#123749 = CARTESIAN_POINT ( 'NONE',  ( 9.911173986789782120, 11.52179005846497972, -1.199719254218440723 ) ) ;
#123750 = CARTESIAN_POINT ( 'NONE',  ( -5.692444392891315097, 7.734547439830227411, -1.599625672291271394 ) ) ;
#123751 = CARTESIAN_POINT ( 'NONE',  ( 2.156058135970494227, 0.9403143569667195001, 1.979733194660021622 ) ) ;
#123752 = CARTESIAN_POINT ( 'NONE',  ( 4.229780737783593203, 4.037091736943370535, -0.7216878364870188411 ) ) ;
#123753 = CARTESIAN_POINT ( 'NONE',  ( 6.363572996767764778, 8.517530811019446091, -1.599625672291283607 ) ) ;
#123754 = CARTESIAN_POINT ( 'NONE',  ( 6.471393748265519719, 5.229711127717882491, -2.419999999999995044 ) ) ;
#123756 = CARTESIAN_POINT ( 'NONE',  ( 6.016814611094169152, 0.2024578496369993375, 2.006372135924570088 ) ) ;
#123755 = CARTESIAN_POINT ( 'NONE',  ( 2.543341688579534576, -1.352695106659363766, -1.226303905950577366 ) ) ;
#123757 = CARTESIAN_POINT ( 'NONE',  ( -8.622622508611375025, 12.04318144581317895, 1.082531754730560403 ) ) ;
#123758 = AXIS2_PLACEMENT_3D ( 'NONE', #175213, #156824, #6263 ) ;
#123759 = CARTESIAN_POINT ( 'NONE',  ( -4.638114411034067963, 8.432649648999159808, -0.4721908680582111995 ) ) ;
#123760 = LINE ( 'NONE', #188660, #39676 ) ;
#123761 = CARTESIAN_POINT ( 'NONE',  ( 7.214910300766615769, 11.56914578420308715, -0.7998128361456291469 ) ) ;
#123762 = CARTESIAN_POINT ( 'NONE',  ( 2.209485269003717445, -0.4220890577730853632, 1.879544223609790565 ) ) ;
#123763 = CARTESIAN_POINT ( 'NONE',  ( 6.227397112613878960, 0.1477489091250457076, -1.956280406615627854 ) ) ;
#123764 = CIRCLE ( 'NONE', #158318, 0.05000000000000059258 ) ;
#123765 = CARTESIAN_POINT ( 'NONE',  ( -0.7500000000000006661, 15.45833333333333037, -1.299038105676657340 ) ) ;
#123766 = CARTESIAN_POINT ( 'NONE',  ( -5.879432169820529630, 10.01108796476595764, -0.7998128361456221525 ) ) ;
#123767 = CARTESIAN_POINT ( 'NONE',  ( 4.090809663021327758, 5.795697244990093644, 1.599625672291267398 ) ) ;
#123768 = EDGE_CURVE ( 'NONE', #127784, #144032, #907, .T. ) ;
#123769 = CARTESIAN_POINT ( 'NONE',  ( -4.543390873910949423, 6.393985001019784953, 1.443375672974058777 ) ) ;
#123770 = CARTESIAN_POINT ( 'NONE',  ( 8.530051201292206287, 13.10347683481629488, 0.000000000000000000 ) ) ;
#123771 = CARTESIAN_POINT ( 'NONE',  ( 11.86239285000045740, 13.87999999999998302, 1.812080536912751061 ) ) ;
#123772 = CARTESIAN_POINT ( 'NONE',  ( 5.313363446356571984, -1.745981802610725442, -1.112170280247841703 ) ) ;
#123774 = CARTESIAN_POINT ( 'NONE',  ( 0.6823417656249882723, 2.488541667008084435, -1.181850606188749264 ) ) ;
#123773 = CARTESIAN_POINT ( 'NONE',  ( -0.05938221139379848412, -1.422385081007140117, -1.168950373246782526 ) ) ;
#123775 = CARTESIAN_POINT ( 'NONE',  ( 5.695955869756449630, 2.025510559372576402, 1.086827626776807554 ) ) ;
#123776 = CARTESIAN_POINT ( 'NONE',  ( 6.155038550924139429, 9.164333495178082600, 1.082531754730558626 ) ) ;
#123778 = CARTESIAN_POINT ( 'NONE',  ( 1.499999999999990896, 4.556250000682819490, 1.214306433183764966E-14 ) ) ;
#123777 = CARTESIAN_POINT ( 'NONE',  ( 4.394251184604957672, 8.140727125432173139, -0.7216878364870357165 ) ) ;
#123779 = CARTESIAN_POINT ( 'NONE',  ( 6.550320078384911149, -1.775227793318678415, 1.449923619939506025 ) ) ;
#123780 = CARTESIAN_POINT ( 'NONE',  ( -1.162044386198238935E-15, 0.3125000000000180411, 1.224999999999967004 ) ) ;
#123781 = AXIS2_PLACEMENT_3D ( 'NONE', #71194, #21374, #138373 ) ;
#123782 = CARTESIAN_POINT ( 'NONE',  ( -7.208094944320834863, 8.438474185576302133, -1.199719254218452047 ) ) ;
#123783 = CARTESIAN_POINT ( 'NONE',  ( 4.892492844921223494, 1.613610725055414141, -1.080192228897313145 ) ) ;
#123784 = ORIENTED_EDGE ( 'NONE', *, *, #141919, .F. ) ;
#123786 = ADVANCED_FACE ( 'NONE', ( #189820 ), #120640, .T. ) ;
#123785 = CARTESIAN_POINT ( 'NONE',  ( 8.229436053370667636, 11.58446391469906267, 1.082531754730558626 ) ) ;
#123787 = EDGE_LOOP ( 'NONE', ( #51638, #195042, #78130, #130282, #54355, #145308, #42936, #60741 ) ) ;
#123788 = CARTESIAN_POINT ( 'NONE',  ( 6.082274476537278041, 0.9889857280602430967, 1.636697341158253272 ) ) ;
#123789 = CARTESIAN_POINT ( 'NONE',  ( 0.4863796390984359008, -0.2058623683223875511, -1.712490539465325146 ) ) ;
#123790 = CARTESIAN_POINT ( 'NONE',  ( 6.245327377194021423, 0.3399632236478037917, -1.987496870419297013 ) ) ;
#123792 = CARTESIAN_POINT ( 'NONE',  ( -4.014622883422336308, 5.777089012116397804, -1.443375672974066548 ) ) ;
#123791 = CARTESIAN_POINT ( 'NONE',  ( -9.826962411806732689, 10.35921099006301382, -0.7998128361456291469 ) ) ;
#123793 = CARTESIAN_POINT ( 'NONE',  ( 3.285556943750000514, -1.801041666188707424, 1.896917185911906500 ) ) ;
#123795 = CARTESIAN_POINT ( 'NONE',  ( 1.023854850961497309, 1.058662087540670704, -1.418139054142423472 ) ) ;
#123794 = CARTESIAN_POINT ( 'NONE',  ( 2.097712127064654819, -2.090152927352141532, 0.05235412406051109108 ) ) ;
#123796 = CARTESIAN_POINT ( 'NONE',  ( 11.41176686791169281, 9.840491965131443308, 3.404018756831826309 ) ) ;
#123798 = CARTESIAN_POINT ( 'NONE',  ( 3.873197071204284914, 2.158828169701370037, -0.7710026823131793661 ) ) ;
#123797 = FILL_AREA_STYLE ('',( #152998 ) ) ;
#123799 = CARTESIAN_POINT ( 'NONE',  ( 2.519154997858559231, -1.001672848371559787, -1.422942596517995817 ) ) ;
#123800 = CARTESIAN_POINT ( 'NONE',  ( 5.027376032568989572, 4.759693547618927489, 0.7998128361456341429 ) ) ;
#123801 = CARTESIAN_POINT ( 'NONE',  ( 1.224999999999969225, 0.6875000006828015930, -3.642919299551294898E-14 ) ) ;
#123802 = CARTESIAN_POINT ( 'NONE',  ( 2.442404235307413796, 1.063479746408531046, 1.369289251230455751 ) ) ;
#123803 = CARTESIAN_POINT ( 'NONE',  ( -1.360316468750048635, 2.651041667008094738, -0.7853790794159161148 ) ) ;
#123804 = CARTESIAN_POINT ( 'NONE',  ( 2.101794631558097315, 0.7159089574285321111, -1.718054499674229074 ) ) ;
#123805 = CARTESIAN_POINT ( 'NONE',  ( 2.858077868800662724, -0.6831540018236246237, 2.060947818793914532 ) ) ;
#123806 = CARTESIAN_POINT ( 'NONE',  ( 6.094553744542824170, 7.069066442510145265, 1.199719254218462483 ) ) ;
#123807 = CARTESIAN_POINT ( 'NONE',  ( 3.415250174187448362, -1.861344788686780438, 0.7762291900053899241 ) ) ;
#123808 = CARTESIAN_POINT ( 'NONE',  ( 2.968750000000002220, 0.7852924748298364399, -1.895863743164148074 ) ) ;
#123809 = CARTESIAN_POINT ( 'NONE',  ( -1.499999999999997780, 2.681250000682818158, 1.214306433183764966E-14 ) ) ;
#123810 = CARTESIAN_POINT ( 'NONE',  ( 1.096560174117457764, -0.4650716533593258761, -1.869300808490617305 ) ) ;
#123811 = CARTESIAN_POINT ( 'NONE',  ( 0.6823417656249934904, 13.69270833367473195, 1.181850606188764807 ) ) ;
#123812 = CARTESIAN_POINT ( 'NONE',  ( 4.131244869123442243, 2.031816273447330623, 0.8983479855831574268 ) ) ;
#123813 = ORIENTED_EDGE ( 'NONE', *, *, #166279, .F. ) ;
#123814 = CARTESIAN_POINT ( 'NONE',  ( -0.2108831679770961920, 2.882544375557041239, -2.385815782126240236 ) ) ;
#123815 = CARTESIAN_POINT ( 'NONE',  ( -1.500000000000001332, 0.1500000000000251132, 0.000000000000000000 ) ) ;
#123817 = EDGE_CURVE ( 'NONE', #3699, #129981, #117248, .T. ) ;
#123816 = CARTESIAN_POINT ( 'NONE',  ( 7.426115451983150706, 9.686887332112256388, -1.599625672291262513 ) ) ;
#123818 = CARTESIAN_POINT ( 'NONE',  ( -1.364683531250000748, -0.4906249996585801409, 0.000000000000000000 ) ) ;
#123819 = CARTESIAN_POINT ( 'NONE',  ( 5.818639523836858451, -0.7989930759073891053, -2.072897825184773168 ) ) ;
#123820 = CARTESIAN_POINT ( 'NONE',  ( 5.107842384611220865, 0.6171798735227496113, -1.862306164846748491 ) ) ;
#123821 = CARTESIAN_POINT ( 'NONE',  ( 9.408995418203963013, 12.00024729270324286, 1.443375672974076540 ) ) ;
#123822 = CARTESIAN_POINT ( 'NONE',  ( 5.360715614582075794, -1.643942929158914268, 1.554587190974612732 ) ) ;
#123823 = CARTESIAN_POINT ( 'NONE',  ( -5.261973015879593873, 8.192700047617899273, 1.082531754730549967 ) ) ;
#123824 = CARTESIAN_POINT ( 'NONE',  ( 2.787610149020779193, -1.925555389141724527, 0.7399787145165384050 ) ) ;
#123825 = CARTESIAN_POINT ( 'NONE',  ( -5.530836599371015794, 8.540060901653093950, 1.199719254218452047 ) ) ;
#123827 = EDGE_CURVE ( 'NONE', #79740, #85578, #130054, .T. ) ;
#123826 = CARTESIAN_POINT ( 'NONE',  ( -1.402160292154681736E-14, 2.118750000682816825, -1.732050807568863648 ) ) ;
#123828 = CARTESIAN_POINT ( 'NONE',  ( 1.364683531249988535, 4.426041667008082214, 0.7879004041258500513 ) ) ;
#123829 = CARTESIAN_POINT ( 'NONE',  ( 4.340975799156801429, -1.628549031532234403, 0.9200136957008757665 ) ) ;
#123830 = CARTESIAN_POINT ( 'NONE',  ( 4.008270194328780178, -1.657810326508919685, 0.5087727743269004899 ) ) ;
#123831 = CARTESIAN_POINT ( 'NONE',  ( 2.085156077859366519, -0.7432962182043149069, 1.573855765194108081 ) ) ;
#123832 = CARTESIAN_POINT ( 'NONE',  ( 1.242159777398026410, 2.290014686995527793, 0.1064554428192917290 ) ) ;
#123833 = CARTESIAN_POINT ( 'NONE',  ( 1.483733071427257411, 2.038639745401783721, -0.8453341458589253010 ) ) ;
#123834 = CARTESIAN_POINT ( 'NONE',  ( 4.177344015168626079, 1.367166224251268547, 1.581858325755406858 ) ) ;
#123835 = CARTESIAN_POINT ( 'NONE',  ( 6.035097030359367842, -1.408219244926838476, -1.337428300092268652 ) ) ;
#123836 = EDGE_CURVE ( 'NONE', #83914, #181742, #40146, .T. ) ;
#123838 = ORIENTED_EDGE ( 'NONE', *, *, #12024, .T. ) ;
#123837 = CARTESIAN_POINT ( 'NONE',  ( -11.01135777277262129, 10.90000000000000036, -1.400000000000001910 ) ) ;
#123839 = CARTESIAN_POINT ( 'NONE',  ( 0.2291389764034670318, 2.011204493129043591, 0.1455304468792120720 ) ) ;
#123840 = CARTESIAN_POINT ( 'NONE',  ( -4.009193028827814587, 7.297902834095492786, -0.7581239365674132813 ) ) ;
#123841 = CARTESIAN_POINT ( 'NONE',  ( -8.585337585951595685, 11.03931315507545108, -1.599625672291263179 ) ) ;
#123842 = CARTESIAN_POINT ( 'NONE',  ( 7.969495366734495434, 8.192166104145387706, 1.040834085586084257E-14 ) ) ;
#123843 =( NAMED_UNIT ( * ) SI_UNIT ( $, .STERADIAN. ) SOLID_ANGLE_UNIT ( ) );
#123844 = CARTESIAN_POINT ( 'NONE',  ( 4.248545464119923842, 0.4890907236730773766, 1.758887239191930796 ) ) ;
#123845 = CARTESIAN_POINT ( 'NONE',  ( 1.905583573826599597, 1.834846665736546756, 1.225745012653912891 ) ) ;
#123846 = ORIENTED_EDGE ( 'NONE', *, *, #93021, .F. ) ;
#123847 = CARTESIAN_POINT ( 'NONE',  ( -4.624739795592948788, 5.528522862014106920, -1.082531754730549967 ) ) ;
#123848 = CARTESIAN_POINT ( 'NONE',  ( 2.209183025140937673, 5.729130629306395051, 0.2365836213946782840 ) ) ;
#123849 = CARTESIAN_POINT ( 'NONE',  ( 1.001543065824772753E-15, -1.509374999522041794, 3.793834371823811669 ) ) ;
#123850 = CARTESIAN_POINT ( 'NONE',  ( -7.043624497499477499, 8.176315654292865887, 1.199719254218450271 ) ) ;
#123851 = CARTESIAN_POINT ( 'NONE',  ( 0.6154972907393120307, 1.653649208057221598, 1.159462664468139614 ) ) ;
#123852 = CARTESIAN_POINT ( 'NONE',  ( -4.767627293860968507, 5.591261926706423857, -1.199719254218453823 ) ) ;
#123853 = CARTESIAN_POINT ( 'NONE',  ( 2.817075279929776688, -1.616631405580427838, -0.9216590669160623639 ) ) ;
#123854 = CARTESIAN_POINT ( 'NONE',  ( 8.920375002787457319, 12.49452237230570084, 1.199719254218450271 ) ) ;
#123855 = CARTESIAN_POINT ( 'NONE',  ( -0.4254946254921331272, 3.044090126849021694, -0.4192457809173989469 ) ) ;
#123856 = CARTESIAN_POINT ( 'NONE',  ( -3.893162665418476109, 7.693773542963529444, 1.040834085586084257E-14 ) ) ;
#123857 = CARTESIAN_POINT ( 'NONE',  ( -7.811469059767924605, 12.26513100303794168, -0.7998128361456281477 ) ) ;
#123858 = CARTESIAN_POINT ( 'NONE',  ( 5.109893933574640279, -1.816543354971979163, 0.1824992186492402357 ) ) ;
#123859 = AXIS2_PLACEMENT_3D ( 'NONE', #208094, #139937, #125880 ) ;
#123861 = CARTESIAN_POINT ( 'NONE',  ( -3.975508435578610555, 7.849559089036333148, -0.01386331990411299175 ) ) ;
#123860 = CARTESIAN_POINT ( 'NONE',  ( -2.844178363816758814, 6.540234867753325076, -0.7998128361456481317 ) ) ;
#123862 = CARTESIAN_POINT ( 'NONE',  ( 6.604365638557201379, 6.767254738080503706, -0.09251035838216993545 ) ) ;
#123863 = CARTESIAN_POINT ( 'NONE',  ( 0.2448742905335095366, -1.679455039217644829, -0.4304099419733271592 ) ) ;
#123864 = CARTESIAN_POINT ( 'NONE',  ( 6.562460610575872266, -1.685528226061007162, -0.7412392050258274079 ) ) ;
#123865 = CARTESIAN_POINT ( 'NONE',  ( 4.565214137342485934, -2.059927483508086965, -1.040394749072820701 ) ) ;
#123866 = CARTESIAN_POINT ( 'NONE',  ( 5.499767588998890844, 6.445425604367387429, 1.199719254218451159 ) ) ;
#123867 = CARTESIAN_POINT ( 'NONE',  ( 0.4739915956469250014, 1.184468288027096694, 1.686179815164081219 ) ) ;
#123868 = CARTESIAN_POINT ( 'NONE',  ( 5.608269097547198712, 9.694731047113750222, -0.7998128361456281477 ) ) ;
#123869 = CARTESIAN_POINT ( 'NONE',  ( 5.466298696655274902, 1.874607906009964964, 1.329618201824170898 ) ) ;
#123870 = CARTESIAN_POINT ( 'NONE',  ( 3.039951802757222765, 2.724153688964670028, 2.451370731312843443 ) ) ;
#123872 = VECTOR ( 'NONE', #113720, 1000.000000000000000 ) ;
#123871 = CARTESIAN_POINT ( 'NONE',  ( -6.936931872047518155, 8.122117267924091166, 1.199719254218452047 ) ) ;
#123873 = CARTESIAN_POINT ( 'NONE',  ( 5.559403950928493821, 0.3636877230743483236, -1.834782481876767291 ) ) ;
#123875 = AXIS2_PLACEMENT_3D ( 'NONE', #126430, #178313, #41923 ) ;
#123874 = VECTOR ( 'NONE', #103668, 1000.000000000000000 ) ;
#123877 = CARTESIAN_POINT ( 'NONE',  ( -3.851398154733808088, 6.650992392901508232, -1.199719254218450271 ) ) ;
#123876 = CARTESIAN_POINT ( 'NONE',  ( 2.847809051801777791, -1.287500320553297994, -1.414207669007704116 ) ) ;
#123878 = CARTESIAN_POINT ( 'NONE',  ( 5.444034239667132624, 0.8972360612293399651, -2.016436982482258333 ) ) ;
#123879 = CARTESIAN_POINT ( 'NONE',  ( 4.944582029040364368, -1.531444570474638667, 1.462332997386527556 ) ) ;
#123880 = CARTESIAN_POINT ( 'NONE',  ( 0.6124999999999759526, 0.8958333340161606095, 1.060881119635896264 ) ) ;
#123881 = LINE ( 'NONE', #108669, #174992 ) ;
#123882 = CARTESIAN_POINT ( 'NONE',  ( 5.682275777458851707, 6.762314840857718501, 1.082531754730549078 ) ) ;
#123883 = CARTESIAN_POINT ( 'NONE',  ( -4.570507181138272479, 7.385989907086349504, 1.082531754730549967 ) ) ;
#123884 = CARTESIAN_POINT ( 'NONE',  ( 1.817812757297363691, -0.2812075768990837665, 2.290339019377229945 ) ) ;
#123885 = CARTESIAN_POINT ( 'NONE',  ( 3.859774877264535053, -0.5717695562157121270, 1.876676618968641019 ) ) ;
#123886 = CARTESIAN_POINT ( 'NONE',  ( -5.984998465789844069, 5.947196063035064206, 0.7998128361456282587 ) ) ;
#123887 = CARTESIAN_POINT ( 'NONE',  ( 6.157095870780715074, 1.689533437190817722, -1.182850423791491856 ) ) ;
#123888 = CARTESIAN_POINT ( 'NONE',  ( 3.009546912553647147, 5.494593250412460606, -1.082531754730543083 ) ) ;
#123889 = CARTESIAN_POINT ( 'NONE',  ( 3.040771591214902259, 6.769593633051179005, -0.7998128361456362523 ) ) ;
#123890 = ORIENTED_EDGE ( 'NONE', *, *, #200423, .F. ) ;
#123891 = CARTESIAN_POINT ( 'NONE',  ( 5.260953973667149342, -0.05432152012316109058, -2.015980820358989511 ) ) ;
#123892 = CARTESIAN_POINT ( 'NONE',  ( -8.109748439268576803, 12.61312361245537517, 0.7998128361456481317 ) ) ;
#123893 = DIRECTION ( 'NONE',  ( 0.7592566023653005702, 0.6507913734559640506, 0.000000000000000000 ) ) ;
#123894 = FACE_OUTER_BOUND ( 'NONE', #173536, .T. ) ;
#123895 = CARTESIAN_POINT ( 'NONE',  ( 2.131898410887596906, 2.078612851201648404, -0.6269345663092191767 ) ) ;
#123896 = DIRECTION ( 'NONE',  ( -0.7592566023653003482, 0.6507913734559641616, 0.000000000000000000 ) ) ;
#123897 = ADVANCED_FACE ( 'NONE', ( #142176 ), #130240, .T. ) ;
#123898 = CARTESIAN_POINT ( 'NONE',  ( -7.120083641305332556, 14.52987117624244284, -9.669683711067579068 ) ) ;
#123899 = DIRECTION ( 'NONE',  ( -1.000000000000000000, 0.000000000000000000, 0.000000000000000000 ) ) ;
#123900 = CARTESIAN_POINT ( 'NONE',  ( 5.307274686206796765, 7.744096871513173497, 1.304404211447189876 ) ) ;
#123901 = CARTESIAN_POINT ( 'NONE',  ( 1.493510409444120057, 1.558468831475682492, 1.348393839584006493 ) ) ;
#123903 = CARTESIAN_POINT ( 'NONE',  ( 6.727182134110202050, 0.5964276595885747989, 1.864301751488647962 ) ) ;
#123902 = CARTESIAN_POINT ( 'NONE',  ( -0.02244404828160087226, 0.2256878572204877031, -2.222431841814066278 ) ) ;
#123904 = CARTESIAN_POINT ( 'NONE',  ( 1.364683531249988757, 0.1343750003414204142, 0.000000000000000000 ) ) ;
#123905 = DIRECTION ( 'NONE',  ( 1.000000000000000000, -0.000000000000000000, -0.000000000000000000 ) ) ;
#123906 = ORIENTED_EDGE ( 'NONE', *, *, #80361, .T. ) ;
#123907 = CARTESIAN_POINT ( 'NONE',  ( 3.703681524037071071, 1.387051605615218008, 1.316649548728260344 ) ) ;
#123908 = B_SPLINE_CURVE_WITH_KNOTS ( 'NONE', 3,
 ( #167768, #138483, #19365, #152580, #203436, #121239, #21480, #18296, #150469, #38838 ),
 .UNSPECIFIED., .F., .F.,
 ( 4, 2, 2, 2, 4 ),
 ( 1.323043618166807713E-09, 0.0004044078111608055909, 0.0008088142992779929433, 0.001213220787395179103, 0.001617627275512365263 ),
 .UNSPECIFIED. ) ;
#123909 = PRESENTATION_LAYER_ASSIGNMENT (  '', '', ( #154890 ) ) ;
#123910 = CARTESIAN_POINT ( 'NONE',  ( 5.612081123951941919, -0.7985520710115794341, -1.579504676149855458 ) ) ;
#123911 = CARTESIAN_POINT ( 'NONE',  ( 6.119526231721748033, 8.232809585132461194, 1.599625672291269396 ) ) ;
#123912 = CARTESIAN_POINT ( 'NONE',  ( -5.576481253922474401, 5.400316305864651056, -0.7998128361456221525 ) ) ;
#123914 = CARTESIAN_POINT ( 'NONE',  ( -0.03024393743376960902, -0.9005804071154848156, 1.690789300719280908 ) ) ;
#123913 = CARTESIAN_POINT ( 'NONE',  ( -0.4875155550656232184, 6.677512024511295330, -3.385544892646772386 ) ) ;
#123915 = CARTESIAN_POINT ( 'NONE',  ( 1.499999999999985123, -0.4541666666666469010, -0.8660254037844323793 ) ) ;
#123916 = CARTESIAN_POINT ( 'NONE',  ( 0.3442982867475213871, -0.9772804826688463731, 1.825211318103404867 ) ) ;
#123917 = CARTESIAN_POINT ( 'NONE',  ( -1.364683531250000748, -1.178124999658580752, 0.000000000000000000 ) ) ;
#123918 = AXIS2_PLACEMENT_3D ( 'NONE', #181934, #162524, #146292 ) ;
#123919 = CARTESIAN_POINT ( 'NONE',  ( 5.647288160985431738, -1.475499438119257878, -1.149758287351684949 ) ) ;
#123920 = CARTESIAN_POINT ( 'NONE',  ( 2.543341688579534576, -1.352695106659363766, -1.226303905950577366 ) ) ;
#123922 = CARTESIAN_POINT ( 'NONE',  ( 6.353009478083933459, 6.838182937092724956, 0.6209923359970755952 ) ) ;
#123921 = CARTESIAN_POINT ( 'NONE',  ( 5.830760709146560750, 2.125890151018691832, 0.5921790101122563765 ) ) ;
#123923 = CARTESIAN_POINT ( 'NONE',  ( -1.364683531250014514, 0.7385416670080887647, -0.7879004041258289570 ) ) ;
#123924 = CARTESIAN_POINT ( 'NONE',  ( 2.875492298462109630, -0.2048798925258775439, 2.052495523891383566 ) ) ;
#123925 = CARTESIAN_POINT ( 'NONE',  ( -5.865874016206865882, 9.995270118883347266, 0.000000000000000000 ) ) ;
#123926 = CARTESIAN_POINT ( 'NONE',  ( 9.589694723567584234, 10.08239868711733855, -0.7998128361456281477 ) ) ;
#123927 = CARTESIAN_POINT ( 'NONE',  ( 3.330499290451325312, 7.037332938835193730, -0.7998128361456291469 ) ) ;
#123928 = CARTESIAN_POINT ( 'NONE',  ( 0.6675187767142229944, 0.2125181155594977611, -2.151144519195991922 ) ) ;
#123929 = CARTESIAN_POINT ( 'NONE',  ( 7.018280793729500644, 8.217024343219755167, -1.199719254218452047 ) ) ;
#123930 = CARTESIAN_POINT ( 'NONE',  ( 5.775854211382815073, -2.020734006234246927, 0.4499205674863211990 ) ) ;
#123931 = CARTESIAN_POINT ( 'NONE',  ( 0.6823417656249882723, -0.09479166632524876901, 1.181850606188755259 ) ) ;
#123932 = CARTESIAN_POINT ( 'NONE',  ( 3.620547430246877862, 1.374377816306590727, -1.668374205817772182 ) ) ;
#123933 = CARTESIAN_POINT ( 'NONE',  ( -4.767604096130494185, 8.184890741402179870, -0.7573865900243268445 ) ) ;
#123935 = CARTESIAN_POINT ( 'NONE',  ( 2.664445928352857429, -0.7481792696971515388, -1.813797970468238985 ) ) ;
#123934 = CARTESIAN_POINT ( 'NONE',  ( 3.070967880043346199, -1.527814596969854000, 1.321012706414641524 ) ) ;
#123936 = CARTESIAN_POINT ( 'NONE',  ( 6.620655732516655512, 0.5568428858156619921, 2.325336003765938742 ) ) ;
#123938 = CARTESIAN_POINT ( 'NONE',  ( 7.619319141200072920, 7.991553207595983643, 0.7216878364870317197 ) ) ;
#123937 = CARTESIAN_POINT ( 'NONE',  ( -1.737500000000000266, -0.4083333333333334370, -3.009438278150923907 ) ) ;
#123939 = CARTESIAN_POINT ( 'NONE',  ( -5.772739544368596043, 9.956889578397179363, -0.7998128361456362523 ) ) ;
#123940 = CARTESIAN_POINT ( 'NONE',  ( 2.571500236035813902, 1.429449181443824823, 1.422607194786096541 ) ) ;
#123942 = CARTESIAN_POINT ( 'NONE',  ( 2.000000000000011990, 2.453103989352373237E-14, 0.5999999999999970912 ) ) ;
#123941 = CARTESIAN_POINT ( 'NONE',  ( -4.205000198532790279, 8.057583998263570635, 0.7998128361456341429 ) ) ;
#123943 = CARTESIAN_POINT ( 'NONE',  ( -0.7499999999999972244, 5.389583334016151639, -1.299038105676652899 ) ) ;
#123944 = CARTESIAN_POINT ( 'NONE',  ( 5.783449990912790106, 0.1341079605299954347, -1.907733270042926810 ) ) ;
#123945 = CARTESIAN_POINT ( 'NONE',  ( 4.311129659021211147, 7.973475668925984472, 1.040834085586084257E-14 ) ) ;
#123947 = CARTESIAN_POINT ( 'NONE',  ( 2.900017720922347220, -0.9963201819552582883, -1.753021271517739343 ) ) ;
#123946 = CARTESIAN_POINT ( 'NONE',  ( -8.690413276235355866, 10.20153224610512943, 1.082531754730558626 ) ) ;
#123948 = CARTESIAN_POINT ( 'NONE',  ( 0.7499999999999902300, 3.483333333333352044, 1.299038105676669330 ) ) ;
#123949 = CARTESIAN_POINT ( 'NONE',  ( -1.364683531250014514, 13.40104166700806587, -0.7879004041258335089 ) ) ;
#123950 = CARTESIAN_POINT ( 'NONE',  ( 5.860297766850644408, 0.7031890092840873407, 1.575098903243739024 ) ) ;
#123951 = CARTESIAN_POINT ( 'NONE',  ( 7.147083253059300922, 8.367293879104554577, 1.199719254218452935 ) ) ;
#123952 = CARTESIAN_POINT ( 'NONE',  ( 9.924205255523292024, 10.68058700763975466, -0.7216878364870257245 ) ) ;
#123953 = FACE_OUTER_BOUND ( 'NONE', #201379, .T. ) ;
#123954 = CARTESIAN_POINT ( 'NONE',  ( 3.883945074633635031, -0.9243716352356041721, 1.626130415258054018 ) ) ;
#123955 =( BOUNDED_CURVE ( )  B_SPLINE_CURVE ( 2, ( #74470, #73383, #209778, #58217, #125433, #26774, #124375, #155722, #192465 ),
 .UNSPECIFIED., .F., .T. ) 
 B_SPLINE_CURVE_WITH_KNOTS ( ( 3, 2, 2, 2, 3 ),
 ( 0.5089285714285713969, 0.5119047619047618625, 0.5178571428571429047, 0.5238095238095238360, 0.5267857142857143016 ),
 .UNSPECIFIED. ) 
 CURVE ( )  GEOMETRIC_REPRESENTATION_ITEM ( )  RATIONAL_B_SPLINE_CURVE ( ( 0.9330127018922194093, 0.9330127018922194093, 1.000000000000000000, 0.8660254037844387076, 1.000000000000000000, 0.8660254037844387076, 1.000000000000000000, 0.9330127018922194093, 0.9330127018922194093 ) ) 
 REPRESENTATION_ITEM ( '' )  );
#123956 = CARTESIAN_POINT ( 'NONE',  ( -1.782949938078044916, -1.500000000000001332, 2.093702347113242102 ) ) ;
#123957 = CARTESIAN_POINT ( 'NONE',  ( 2.096617048772158487, 2.047133997803842753, 0.3078910663548983795 ) ) ;
#123958 = FACE_OUTER_BOUND ( 'NONE', #46101, .T. ) ;
#123959 = VERTEX_POINT ( 'NONE', #144329 ) ;
#123960 = CARTESIAN_POINT ( 'NONE',  ( 5.076602173674213070, 4.887400388900169368, 0.000000000000000000 ) ) ;
#123961 = CARTESIAN_POINT ( 'NONE',  ( 0.2811518721992244951, 0.1772043297433387177, -1.802849762578159876 ) ) ;
#123962 = CARTESIAN_POINT ( 'NONE',  ( 5.533136087708556694, 5.627949321847663278, 0.000000000000000000 ) ) ;
#123963 = TOROIDAL_SURFACE ( 'NONE', #203458, 0.1600000000000000033, 0.08000000000000000167 ) ;
#123964 = CARTESIAN_POINT ( 'NONE',  ( -2.535011536075347571, 5.133042487381361596, -0.9999999999999956701 ) ) ;
#123965 = ORIENTED_EDGE ( 'NONE', *, *, #164350, .T. ) ;
#123966 = CARTESIAN_POINT ( 'NONE',  ( 6.765155463094740362, 10.83650577367847667, 0.7216878364870438212 ) ) ;
#123967 = EDGE_CURVE ( 'NONE', #63091, #168104, #106878, .T. ) ;
#123968 = CARTESIAN_POINT ( 'NONE',  ( 7.065770611016287006, 11.39514947949436774, 1.040834085586084257E-14 ) ) ;
#123969 = CARTESIAN_POINT ( 'NONE',  ( 5.536718839138406345, -1.507006759595967305, 1.182436279247323085 ) ) ;
#123970 = CARTESIAN_POINT ( 'NONE',  ( -11.45842088241054668, 13.59306470877032424, 3.566211699757681597 ) ) ;
#123971 = CARTESIAN_POINT ( 'NONE',  ( -3.719872605471121751, 6.605953636083950364, 2.499999999999999556 ) ) ;
#123972 = CARTESIAN_POINT ( 'NONE',  ( 4.080641048033257334, 5.783833860837341412, 1.214306433183764966E-14 ) ) ;
#123974 = ORIENTED_EDGE ( 'NONE', *, *, #170032, .T. ) ;
#123973 = CARTESIAN_POINT ( 'NONE',  ( 4.284013352238246419, 6.021101549076499637, -1.443375672974051449 ) ) ;
#123975 = CARTESIAN_POINT ( 'NONE',  ( -7.863365906246061243, 10.19701286208565705, -1.443375672974059665 ) ) ;
#123976 = CARTESIAN_POINT ( 'NONE',  ( 2.852577672069932735, 0.7271573612388192442, 2.035869728763760378 ) ) ;
#123977 = CARTESIAN_POINT ( 'NONE',  ( -6.861835142292179057, 9.098836647464588978, 1.443375672974064550 ) ) ;
#123978 = CARTESIAN_POINT ( 'NONE',  ( 6.617788377246179188, 8.814115421577600529, -1.443375672974078761 ) ) ;
#123979 = CARTESIAN_POINT ( 'NONE',  ( -3.735435015764967837, 4.316761258935923884, -1.199719254218452047 ) ) ;
#123980 = CARTESIAN_POINT ( 'NONE',  ( 5.297797529045337406, -0.6555159417414997414, 1.704002486358429325 ) ) ;
#123981 = CARTESIAN_POINT ( 'NONE',  ( 10.75342306851627328, 8.382369863076769789, 4.797975732338054300 ) ) ;
#123982 = CARTESIAN_POINT ( 'NONE',  ( 1.124223373062693820, 1.177560201100100734, -1.580856549663816280 ) ) ;
#123983 = CARTESIAN_POINT ( 'NONE',  ( 3.621269620730773298, 1.642686141288721480, 0.9789267784374030557 ) ) ;
#123984 = VERTEX_POINT ( 'NONE', #147776 ) ;
#123985 = CARTESIAN_POINT ( 'NONE',  ( -11.49978884755372555, 9.857291788371918884, -3.429452816445187402 ) ) ;
#123986 = CARTESIAN_POINT ( 'NONE',  ( 4.879337363741727884, -0.09859167047137314122, 1.967224067494575346 ) ) ;
#123987 = ORIENTED_EDGE ( 'NONE', *, *, #55534, .T. ) ;
#123988 = CARTESIAN_POINT ( 'NONE',  ( 5.741732329385339284, 1.940029712683045915, 0.09120231522616148445 ) ) ;
#123989 = ORIENTED_EDGE ( 'NONE', *, *, #143956, .T. ) ;
#123990 = CARTESIAN_POINT ( 'NONE',  ( -3.935609729716867289, 7.813571461303467913, 0.7998128361456352531 ) ) ;
#123991 = CARTESIAN_POINT ( 'NONE',  ( -5.822300622425855110, 5.757381912443740646, 0.7998128361456281477 ) ) ;
#123992 = CARTESIAN_POINT ( 'NONE',  ( 7.526184668917440312, 8.913541880892736913, -1.082531754730548412 ) ) ;
#123994 = EDGE_LOOP ( 'NONE', ( #74460, #196379, #76317, #99441, #95446 ) ) ;
#123993 = CARTESIAN_POINT ( 'NONE',  ( 3.457576163436149486, -1.449788379102138869, -1.247086912153513749 ) ) ;
#123995 = ADVANCED_FACE ( 'NONE', ( #44956 ), #179209, .T. ) ;
#123996 = CARTESIAN_POINT ( 'NONE',  ( 1.202499378025536858, -2.206952907257493823, 0.001246274542086866404 ) ) ;
#123997 = DIRECTION ( 'NONE',  ( 1.224646799147353207E-16, 0.000000000000000000, -1.000000000000000000 ) ) ;
#123998 = CARTESIAN_POINT ( 'NONE',  ( 6.322908177684296582, 1.490210921086480234, -1.353605025193492128 ) ) ;
#123999 = DIRECTION ( 'NONE',  ( -0.5620411653108546846, 0.8271092603133013421, 3.252606517456488690E-14 ) ) ;
#124000 = DIRECTION ( 'NONE',  ( 0.000000000000000000, 0.000000000000000000, -1.000000000000000000 ) ) ;
#124001 = CARTESIAN_POINT ( 'NONE',  ( 1.592325325408463055, 1.022198633559557646, -1.800363622228559946 ) ) ;
#124002 = CARTESIAN_POINT ( 'NONE',  ( -4.903245109636583443, 8.872203061218007392, -0.7998128361456281477 ) ) ;
#124003 = CIRCLE ( 'NONE', #175882, 10.75000000000000000 ) ;
#124004 = CARTESIAN_POINT ( 'NONE',  ( -5.432786300537782331, 7.535064667520821047, -1.248352293942560642 ) ) ;
#124005 = CARTESIAN_POINT ( 'NONE',  ( 2.672702088255949078E-15, 1.937500000000013323, -1.225000000000018074 ) ) ;
#124006 = CARTESIAN_POINT ( 'NONE',  ( 4.611744806942754238, 8.532119374741881757, -0.7998128361456231517 ) ) ;
#124007 = CARTESIAN_POINT ( 'NONE',  ( 3.906157654512984134, 7.571284673658201569, -0.7216878364870338292 ) ) ;
#124008 = CARTESIAN_POINT ( 'NONE',  ( -0.01979922387982912396, -6.863887327018224127, 9.496663239505998888 ) ) ;
#124009 = CARTESIAN_POINT ( 'NONE',  ( 0.000000000000000000, -4.500000000000003553, 0.000000000000000000 ) ) ;
#124010 = CARTESIAN_POINT ( 'NONE',  ( 0.6823417656249969321, 11.83854166700806765, -1.181850606188757036 ) ) ;
#124012 = CARTESIAN_POINT ( 'NONE',  ( -6.903036488013351679, 8.082572653217566128, -1.199719254218452047 ) ) ;
#124011 = CARTESIAN_POINT ( 'NONE',  ( 6.825078400183553384, 4.701740280048592346, 2.318362489372997270 ) ) ;
#124013 = CARTESIAN_POINT ( 'NONE',  ( 5.344279299745758216, 0.3302840285365048478, -1.702201177978326818 ) ) ;
#124014 = CARTESIAN_POINT ( 'NONE',  ( -3.744022975668147790, 7.519777238254810925, -0.7998128361456281477 ) ) ;
#124016 = VECTOR ( 'NONE', #17227, 1000.000000000000000 ) ;
#124015 = VECTOR ( 'NONE', #117086, 1000.000000000000000 ) ;
#124017 = CARTESIAN_POINT ( 'NONE',  ( 1.885682352965558639, -1.950755244972163904, 0.6936349442826782452 ) ) ;
#124018 = CARTESIAN_POINT ( 'NONE',  ( 3.093478398350542946, -0.4104027421963015732, 2.076914780291692519 ) ) ;
#124019 = CARTESIAN_POINT ( 'NONE',  ( 7.637320603199683866, 7.804628880021436288, -0.7998128361456281477 ) ) ;
#124020 = CARTESIAN_POINT ( 'NONE',  ( -5.398914348987532641, 6.259949555863199677, -2.420000000000000373 ) ) ;
#124021 = CARTESIAN_POINT ( 'NONE',  ( 1.252720943002823883, -0.4733663544725670302, -1.911600023467324716 ) ) ;
#124022 = CARTESIAN_POINT ( 'NONE',  ( 5.396677706949416731, 6.496517479030419651, 1.312881173378084521 ) ) ;
#124024 = CARTESIAN_POINT ( 'NONE',  ( 0.1934256698341470238, 1.783621342183003389, -0.6902995980747894667 ) ) ;
#124023 = CARTESIAN_POINT ( 'NONE',  ( 1.737500000000001155, -1.283333333333334325, 3.009438278150922130 ) ) ;
#124025 = CARTESIAN_POINT ( 'NONE',  ( 3.363489724395284597, 2.236470799849974878, -0.5019982374358539223 ) ) ;
#124026 = CARTESIAN_POINT ( 'NONE',  ( 1.400715809426569702, 1.493624456287694580, -1.049586478250638777 ) ) ;
#124027 = CARTESIAN_POINT ( 'NONE',  ( 4.366607992053101128, 7.252070536440704096, -1.199719254218448494 ) ) ;
#124029 = EDGE_CURVE ( 'NONE', #88893, #3254, #166278, .T. ) ;
#124028 = CARTESIAN_POINT ( 'NONE',  ( 6.493992390821439642, 7.639041213122241381, -1.082531754730543971 ) ) ;
#124030 = CARTESIAN_POINT ( 'NONE',  ( -6.482770005628665011, 10.71498210654212002, 0.7998128361456481317 ) ) ;
#124031 = CARTESIAN_POINT ( 'NONE',  ( 3.093996842688331750, 1.280297628565935097, 1.553616095213964154 ) ) ;
#124032 = CARTESIAN_POINT ( 'NONE',  ( 2.992962298452767289, 0.2353761085502041883, 1.947492218917420637 ) ) ;
#124033 = CARTESIAN_POINT ( 'NONE',  ( -8.320953590485107298, 10.73086516036454618, 1.599625672291269396 ) ) ;
#124034 = CARTESIAN_POINT ( 'NONE',  ( -7.549192604710863286, 7.701812881784464437, -0.7998128361456291469 ) ) ;
#124035 = CARTESIAN_POINT ( 'NONE',  ( -15.75000000000000000, 10.90000000000000036, -3.600000000000002309 ) ) ;
#124037 = CARTESIAN_POINT ( 'NONE',  ( 5.032005376881601322, 0.9078957314892305286, -1.519088338465144128 ) ) ;
#124036 = CARTESIAN_POINT ( 'NONE',  ( 5.771452434752829319, 1.244600244801373767, 1.679635579212119145 ) ) ;
#124038 = CYLINDRICAL_SURFACE ( 'NONE', #126567, 0.07999999999999998779 ) ;
#124039 = CARTESIAN_POINT ( 'NONE',  ( 0.6389542677898361056, -1.877638805159736579, 1.129783718924075364 ) ) ;
#124040 = CARTESIAN_POINT ( 'NONE',  ( 5.665861931341662938, -1.099307624823061547, 1.349167961392354620 ) ) ;
#124041 = CARTESIAN_POINT ( 'NONE',  ( 8.158255747121103241, 10.54105100977322174, 1.599625672291281386 ) ) ;
#124042 = CARTESIAN_POINT ( 'NONE',  ( 0.000000000000000000, 7.849261790823902629, 10.24999999999998934 ) ) ;
#124043 = CARTESIAN_POINT ( 'NONE',  ( 6.451773728000877561, -2.099535003536470157, -0.9362560538537908483 ) ) ;
#124045 = ADVANCED_FACE ( 'NONE', ( #14541 ), #59545, .T. ) ;
#124044 = CARTESIAN_POINT ( 'NONE',  ( 0.1333692844072767447, 1.351132181276387678, -2.308013766563504987 ) ) ;
#124046 = CARTESIAN_POINT ( 'NONE',  ( 5.096919866207451300, 0.8898786499993548427, -1.487894112255260692 ) ) ;
#124047 = CARTESIAN_POINT ( 'NONE',  ( 5.951682048281027981, 1.640226396406889942, 1.422642917226999426 ) ) ;
#124048 = CARTESIAN_POINT ( 'NONE',  ( -0.4019237886467001974, 11.30133545031536713, 1.500000000000001998 ) ) ;
#124049 = CARTESIAN_POINT ( 'NONE',  ( 0.1634790396850393235, 1.973143002845114458, -0.7684359545688070892 ) ) ;
#124050 = CARTESIAN_POINT ( 'NONE',  ( 2.625000000000002665, -2.052068128417949833, 1.560916121760785068E-13 ) ) ;
#124051 = CARTESIAN_POINT ( 'NONE',  ( 6.727182134110242906, 2.956326135258012577, 2.541581140702349195 ) ) ;
#124052 = CARTESIAN_POINT ( 'NONE',  ( 3.961874236345910294, 1.911929771648058995, -0.2350156305768891229 ) ) ;
#124053 = CARTESIAN_POINT ( 'NONE',  ( -0.7500000000000006661, 10.73958333401613174, -1.299038105676657340 ) ) ;
#124054 = CARTESIAN_POINT ( 'NONE',  ( 1.260717678522350838, 2.218966152042425755, 0.1042569218142989779 ) ) ;
#124055 = ORIENTED_EDGE ( 'NONE', *, *, #166016, .T. ) ;
#124056 = CARTESIAN_POINT ( 'NONE',  ( -1.499999999999997780, 4.900000000000022560, 1.214306433183764966E-14 ) ) ;
#124057 = CARTESIAN_POINT ( 'NONE',  ( 4.660252114795294887, 6.460046772059735432, -1.599625672291256295 ) ) ;
#124058 = CARTESIAN_POINT ( 'NONE',  ( 6.226218857173709154, 8.287007971501239467, 1.599625672291281386 ) ) ;
#124059 = CIRCLE ( 'NONE', #96318, 1.500000000000000222 ) ;
#124060 = CARTESIAN_POINT ( 'NONE',  ( 2.737233380259511684, 2.092449130469396401, 0.7459289674271016857 ) ) ;
#124061 = CARTESIAN_POINT ( 'NONE',  ( -8.839552966430012759, 10.37552855133225904, -1.082531754730543971 ) ) ;
#124062 = DIRECTION ( 'NONE',  ( 0.000000000000000000, 0.000000000000000000, -1.000000000000000000 ) ) ;
#124063 = CARTESIAN_POINT ( 'NONE',  ( 7.307481608085759639, 7.627742752295940676, 1.040834085586084257E-14 ) ) ;
#124064 = CARTESIAN_POINT ( 'NONE',  ( -7.659993601596706725, 11.88048360193076647, -0.7216878364870267237 ) ) ;
#124065 = CARTESIAN_POINT ( 'NONE',  ( 5.994113311017540191, 9.046863725278862844, -1.082531754730548412 ) ) ;
#124066 = CARTESIAN_POINT ( 'NONE',  ( 0.9322677863709986079, -1.591319861332978425, -1.238319039483272599 ) ) ;
#124068 = CARTESIAN_POINT ( 'NONE',  ( 6.531690654341108626, 1.975040822251827644, -0.5949189890239890977 ) ) ;
#124067 = CARTESIAN_POINT ( 'NONE',  ( 9.589694723567584234, 10.08239868711733855, -0.7998128361456281477 ) ) ;
#124069 = CARTESIAN_POINT ( 'NONE',  ( 0.000000000000000000, 9.999999999999998224, 0.000000000000000000 ) ) ;
#124070 = CARTESIAN_POINT ( 'NONE',  ( 5.655159470231527763, 9.611786791996525636, -0.7216878364870458196 ) ) ;
#124072 = EDGE_CURVE ( 'NONE', #6407, #57984, #199687, .T. ) ;
#124071 = CARTESIAN_POINT ( 'NONE',  ( -2.310360766237192109, 5.468970595003730395, -0.7883092092346147828 ) ) ;
#124073 = CARTESIAN_POINT ( 'NONE',  ( -1.364683531250014514, 1.738541667008085545, -0.7879004041258289570 ) ) ;
#124074 = CARTESIAN_POINT ( 'NONE',  ( 1.229378055282577042, -1.117200307070218779, -1.372552531265440523 ) ) ;
#124075 = CARTESIAN_POINT ( 'NONE',  ( 6.486931489777390425, -1.733547045345487758, 0.05303144115107599060 ) ) ;
#124076 = CARTESIAN_POINT ( 'NONE',  ( 6.480030497237043718, -1.708793550445006248, -0.3294957622956768972 ) ) ;
#124077 = CARTESIAN_POINT ( 'NONE',  ( 4.089605575727714104, -0.8772585143675699637, 2.118060962191004037 ) ) ;
#124078 = CARTESIAN_POINT ( 'NONE',  ( -1.402160292154681736E-14, -0.6781249996585819728, 1.575800808251672791 ) ) ;
#124079 = CARTESIAN_POINT ( 'NONE',  ( 2.677489186553200007, -0.9463553590365643142, 1.579155189138586435 ) ) ;
#124080 = EDGE_CURVE ( 'NONE', #37826, #96984, #127642, .T. ) ;
#124081 = CARTESIAN_POINT ( 'NONE',  ( 8.224992744984721327, 12.74757530245756243, 1.040834085586084257E-14 ) ) ;
#124082 = CARTESIAN_POINT ( 'NONE',  ( 7.874658059456543846, 14.91651369936353433, 9.071118931273595365 ) ) ;
#124083 = CARTESIAN_POINT ( 'NONE',  ( 3.364083894888194592, 0.8197913233371353359, 1.631220078658943695 ) ) ;
#124084 = CARTESIAN_POINT ( 'NONE',  ( 4.307267641921147749, 1.238321930042911578, -1.591317616567271775 ) ) ;
#124085 = CARTESIAN_POINT ( 'NONE',  ( -8.482597663644387609, 13.04811437422715414, -0.7998128361456281477 ) ) ;
#124087 = CARTESIAN_POINT ( 'NONE',  ( -3.420250508247430155, -0.02876672507465954931, -0.2938434605158617985 ) ) ;
#124086 = CARTESIAN_POINT ( 'NONE',  ( 3.344836307015612409, 0.5477570922035517320, 2.195101814764536030 ) ) ;
#124088 = CARTESIAN_POINT ( 'NONE',  ( 5.614326327132292072, -0.9438296153482359507, -1.882684210903639022 ) ) ;
#124089 = CARTESIAN_POINT ( 'NONE',  ( 9.680359324772703999, 13.43752487939449836, 8.167046318416048223 ) ) ;
#124090 = CARTESIAN_POINT ( 'NONE',  ( 2.910663983731573090, 0.6951178490613962868, 1.950330170896700022 ) ) ;
#124091 = CARTESIAN_POINT ( 'NONE',  ( 5.054492339796319733, 4.791329239384148231, -0.7998128361456211532 ) ) ;
#124092 = CARTESIAN_POINT ( 'NONE',  ( -1.360316468750014884, 0.1927083336747308917, 0.7853790794158901356 ) ) ;
#124093 = CARTESIAN_POINT ( 'NONE',  ( 4.899148033862871010, -0.2601683324335197223, -2.104413843559429065 ) ) ;
#124095 = CARTESIAN_POINT ( 'NONE',  ( 0.5570954828270138215, -1.626785562868319435, -1.031698974670463009 ) ) ;
#124094 = CARTESIAN_POINT ( 'NONE',  ( -9.992522908471816123, 11.61669713376064372, 1.199719254218462483 ) ) ;
#124096 = CARTESIAN_POINT ( 'NONE',  ( -4.679499295372141709, 5.488445928469455559, 1.199719254218452935 ) ) ;
#124097 = CARTESIAN_POINT ( 'NONE',  ( 8.829384350997564468, 11.32403438096243775, 1.599625672291281386 ) ) ;
#124098 = CARTESIAN_POINT ( 'NONE',  ( 4.868786560638885597, 7.733982516503781213, 1.082531754730548412 ) ) ;
#124099 = CARTESIAN_POINT ( 'NONE',  ( 4.546345379095670047, 6.970243970676179401, 1.177900817425497904 ) ) ;
#124100 = CARTESIAN_POINT ( 'NONE',  ( 0.7869457366334648984, 2.800000000000024247, -1.251086691529569306 ) ) ;
#124101 = PRESENTATION_LAYER_ASSIGNMENT (  '', '', ( #2902 ) ) ;
#124102 = CARTESIAN_POINT ( 'NONE',  ( -3.228813138348844536, 6.918699094715619502, 0.7998128361456341429 ) ) ;
#124103 = CARTESIAN_POINT ( 'NONE',  ( 0.6509960782678033686, 2.189857587618043055, 0.3722473809256007793 ) ) ;
#124104 = CARTESIAN_POINT ( 'NONE',  ( 2.204260208318520764, -2.105514897310766020, 0.05069945311739902649 ) ) ;
#124105 = CARTESIAN_POINT ( 'NONE',  ( -4.034433228518296666, 6.864533312316751790, -1.199719254218450271 ) ) ;
#124106 = CARTESIAN_POINT ( 'NONE',  ( 6.889514614038635187, 11.18951748302043114, -0.7998128361456291469 ) ) ;
#124107 = CARTESIAN_POINT ( 'NONE',  ( 6.016418624437367413, 0.7528656616105857680, 1.702022903989255376 ) ) ;
#124108 = CARTESIAN_POINT ( 'NONE',  ( 8.288111976655649471, 8.563885482386732306, -0.7998128361456291469 ) ) ;
#124109 = CARTESIAN_POINT ( 'NONE',  ( -0.02319159430949970652, 0.003959926571647092407, -1.810968101872318714 ) ) ;
#124110 = CARTESIAN_POINT ( 'NONE',  ( -7.431277594066160397, 7.842447745931541370, -0.7216878364870338292 ) ) ;
#124111 = CARTESIAN_POINT ( 'NONE',  ( -7.510853912290736289, 11.70648729774046792, 0.7216878364870458196 ) ) ;
#124112 = CARTESIAN_POINT ( 'NONE',  ( 0.6332531790259123827, 1.961634380476449335, 0.8060562103610890983 ) ) ;
#124113 = FACE_OUTER_BOUND ( 'NONE', #185911, .T. ) ;
#124115 = CARTESIAN_POINT ( 'NONE',  ( 3.631260574587381829, 0.05062604155347744800, -1.961386756325018021 ) ) ;
#124114 = CARTESIAN_POINT ( 'NONE',  ( 1.224999999999943023, -0.8541666666666519747, -0.7072540797573197979 ) ) ;
#124116 = CARTESIAN_POINT ( 'NONE',  ( 1.727627455807039691, -2.035446057602477321, 0.7283451284763039490 ) ) ;
#124118 = CARTESIAN_POINT ( 'NONE',  ( -4.791002085003811750, 6.784460936665063890, -1.245152473204954591 ) ) ;
#124117 = CARTESIAN_POINT ( 'NONE',  ( -4.821859908315634158, 5.654533310236863564, 1.199719254218452935 ) ) ;
#124119 = CARTESIAN_POINT ( 'NONE',  ( -1.402160292154681736E-14, 2.196875000341423689, -1.575800808251660134 ) ) ;
#124120 = CARTESIAN_POINT ( 'NONE',  ( 3.573892692743201760, -1.677664982382242931, -0.4625120326062928111 ) ) ;
#124121 = AXIS2_PLACEMENT_3D ( 'NONE', #173391, #24974, #176574 ) ;
#124122 = CARTESIAN_POINT ( 'NONE',  ( 5.016153647376196290, 8.796003655340152605, 0.7216878364870438212 ) ) ;
#124123 = CARTESIAN_POINT ( 'NONE',  ( -11.58085191697663241, 6.132731128919016506, 5.153920277027906671 ) ) ;
#124124 = ORIENTED_EDGE ( 'NONE', *, *, #189834, .F. ) ;
#124125 = CARTESIAN_POINT ( 'NONE',  ( 2.460314346279086628, 1.556669099887195484, 1.281166478716524670 ) ) ;
#124126 = CARTESIAN_POINT ( 'NONE',  ( 6.825078400183572036, 7.051914997414900022, 2.742498282622223726 ) ) ;
#124127 = CARTESIAN_POINT ( 'NONE',  ( -2.810282979782591006, 6.500690253046801814, 0.000000000000000000 ) ) ;
#124128 = CARTESIAN_POINT ( 'NONE',  ( 2.008605748815388559, 1.462198227207864853, -1.322556311574287768 ) ) ;
#124131 = ORIENTED_EDGE ( 'NONE', *, *, #36008, .T. ) ;
#124130 = CARTESIAN_POINT ( 'NONE',  ( -5.234856708652269042, 7.200695141551334721, 1.443375672974058777 ) ) ;
#124129 = FILL_AREA_STYLE_COLOUR ( '', #180996 ) ;
#124132 = CARTESIAN_POINT ( 'NONE',  ( -6.007671464186866928, 8.102312356341712984, 1.443375672974058777 ) ) ;
#124133 = CARTESIAN_POINT ( 'NONE',  ( 6.561219994370630637, 6.619454513046008515, 0.000000000000000000 ) ) ;
#124134 = CARTESIAN_POINT ( 'NONE',  ( -4.471156797456668386, 8.438376373666578445, -0.7998128361456362523 ) ) ;
#124135 = CARTESIAN_POINT ( 'NONE',  ( 2.596358364526121676, -1.036244631391324722, 1.733413072464027316 ) ) ;
#124136 = CARTESIAN_POINT ( 'NONE',  ( 0.000000000000000000, -0.4330127018922214077, -6.500000000000000000 ) ) ;
#124137 = CARTESIAN_POINT ( 'NONE',  ( 6.247156018452869830, -1.954037266989640420, 1.227234044731172036 ) ) ;
#124138 = DIRECTION ( 'NONE',  ( 0.000000000000000000, -1.000000000000000000, 0.000000000000000000 ) ) ;
#124139 = CARTESIAN_POINT ( 'NONE',  ( 3.467582345443523728, -0.3871886708083654427, 1.922995549214156608 ) ) ;
#124140 = CARTESIAN_POINT ( 'NONE',  ( 8.398386088661320414, 11.88553530582519357, -1.199719254218446718 ) ) ;
#124141 = CARTESIAN_POINT ( 'NONE',  ( 1.055314813143366726, -1.277040974352643854, 1.560502084637045650 ) ) ;
#124142 = VERTEX_POINT ( 'NONE', #18803 ) ;
#124143 = CARTESIAN_POINT ( 'NONE',  ( 1.956417434996825522, -1.298217783395636316, 1.672616391537498526 ) ) ;
#124145 = CARTESIAN_POINT ( 'NONE',  ( -7.314787569772770226, 8.492672571945082183, -1.199719254218452935 ) ) ;
#124144 = CARTESIAN_POINT ( 'NONE',  ( -3.972702704004144714, 4.593573561881607148, 1.199719254218462483 ) ) ;
#124146 = CARTESIAN_POINT ( 'NONE',  ( 2.097363409947244683, -1.840767647902554982, 0.04455809990146220728 ) ) ;
#124147 = ORIENTED_EDGE ( 'NONE', *, *, #158591, .F. ) ;
#124148 = CARTESIAN_POINT ( 'NONE',  ( -9.972185678051314284, 11.59297036493672017, 1.199719254218462483 ) ) ;
#124149 = CARTESIAN_POINT ( 'NONE',  ( 9.977656983550911463, 11.55331835374545513, 6.672210388449995477 ) ) ;
#124150 = CARTESIAN_POINT ( 'NONE',  ( 2.742561299210785286, 1.174483946500170184, -1.765453564165630596 ) ) ;
#124151 = CARTESIAN_POINT ( 'NONE',  ( 0.4097734724025984820, 1.271762808003698009, -1.331557029818277060 ) ) ;
#124152 = CARTESIAN_POINT ( 'NONE',  ( 1.499999999999990896, 4.306250000682819490, 1.214306433183764966E-14 ) ) ;
#124153 = CARTESIAN_POINT ( 'NONE',  ( 6.103141704446003679, 10.27208242182903142, 0.7998128361456462443 ) ) ;
#124154 = CARTESIAN_POINT ( 'NONE',  ( 7.713663051532233972, 7.963971413067895355, -0.7998128361456341429 ) ) ;
#124155 = CARTESIAN_POINT ( 'NONE',  ( 4.130192093715317370, 1.105610312200686174, -1.738907380658259560 ) ) ;
#124157 = CARTESIAN_POINT ( 'NONE',  ( 1.821575194732877545, 1.059174331173462935, -1.505913648122420900 ) ) ;
#124156 = CARTESIAN_POINT ( 'NONE',  ( -6.093499974338126179, 9.196501505781426999, -1.199719254218440723 ) ) ;
#124158 = CARTESIAN_POINT ( 'NONE',  ( -1.364683531250012516, 4.738541667008091096, -0.7879004041258300672 ) ) ;
#124159 = DIRECTION ( 'NONE',  ( 0.000000000000000000, 0.000000000000000000, 1.000000000000000000 ) ) ;
#124160 = CARTESIAN_POINT ( 'NONE',  ( -8.581735480930626505E-14, -9.900000000000005684, -11.00029519899099739 ) ) ;
#124161 = AXIS2_PLACEMENT_3D ( 'NONE', #122984, #156464, #91475 ) ;
#124162 = CARTESIAN_POINT ( 'NONE',  ( 1.225528936851564721, -0.05108506852482053856, 2.206457870188942572 ) ) ;
#124163 = CARTESIAN_POINT ( 'NONE',  ( 3.409705294423628352, -0.4451680670645007387, 2.218022689048837481 ) ) ;
#124164 = CARTESIAN_POINT ( 'NONE',  ( -7.700668062882065179, 10.96756792579566664, -1.082531754730543971 ) ) ;
#124165 = CARTESIAN_POINT ( 'NONE',  ( 3.849720854566369255, -1.253557171431567863, -1.308061721885760198 ) ) ;
#124166 = CARTESIAN_POINT ( 'NONE',  ( 2.571384127028350175, 1.358050290760448364, 1.351446277617992076 ) ) ;
#124167 = CARTESIAN_POINT ( 'NONE',  ( 4.299325596424930396, -1.802881993240162961, 1.017688063649782482 ) ) ;
#124168 = CARTESIAN_POINT ( 'NONE',  ( -0.6823417656250212460, 2.613541667008084879, 1.181850606188767472 ) ) ;
#124169 = CARTESIAN_POINT ( 'NONE',  ( 2.711746521272298871, -1.950232680175187250, 0.2877518621813393018 ) ) ;
#124170 = CARTESIAN_POINT ( 'NONE',  ( 1.536025370465494921, 0.9519229637394033272, -1.674701244428679292 ) ) ;
#124171 = CARTESIAN_POINT ( 'NONE',  ( 3.432352559540859271, 1.824792983844251371, 0.4109263881779609551 ) ) ;
#124172 = CARTESIAN_POINT ( 'NONE',  ( 2.403307275528394626, 1.852421531443759539, -1.376039175078101806 ) ) ;
#124173 = CARTESIAN_POINT ( 'NONE',  ( 3.508111033888267283, 1.861241883637313688, 0.002260837353922766878 ) ) ;
#124174 = CARTESIAN_POINT ( 'NONE',  ( 1.364683531249988535, 4.155208333674753618, -0.7879004041258239610 ) ) ;
#124175 = MECHANICAL_DESIGN_GEOMETRIC_PRESENTATION_REPRESENTATION (  '', ( #92881 ), #182816 ) ;
#124176 = CARTESIAN_POINT ( 'NONE',  ( -3.750802052474980108, 7.527686161196117887, 1.040834085586084257E-14 ) ) ;
#124177 = CARTESIAN_POINT ( 'NONE',  ( 5.452350330990040739, 9.512825819463730070, 0.7998128361456462443 ) ) ;
#124178 = CARTESIAN_POINT ( 'NONE',  ( 1.499999999999996891, 8.927083334016126415, -0.8660254037844378194 ) ) ;
#124179 = CARTESIAN_POINT ( 'NONE',  ( 0.2234445423696731770, -0.1008541980360810469, 2.103780803345968398 ) ) ;
#124180 = CARTESIAN_POINT ( 'NONE',  ( 3.999292125906905859, 5.688926785023260102, 1.443375672974062551 ) ) ;
#124182 = CARTESIAN_POINT ( 'NONE',  ( 1.403499169902377552, 7.376709478543040710, 4.304123474984470121 ) ) ;
#124181 = CARTESIAN_POINT ( 'NONE',  ( 1.364683531249988535, 3.467708333674749621, -0.7879004041258239610 ) ) ;
#124183 = CARTESIAN_POINT ( 'NONE',  ( 6.731704548537910782, -1.406307105171537009, -1.641701734229366716 ) ) ;
#124184 = CARTESIAN_POINT ( 'NONE',  ( 1.582450481569739331, 1.094613367649547309, 1.816135667671102016 ) ) ;
#124185 = CARTESIAN_POINT ( 'NONE',  ( 0.2287787457191146345, 1.389782569690813929, -1.465877111898945095 ) ) ;
#124186 = CARTESIAN_POINT ( 'NONE',  ( -1.402160292154681736E-14, 1.446875000341420137, -1.575800808251659024 ) ) ;
#124187 = CARTESIAN_POINT ( 'NONE',  ( -5.260200412422213923, 6.199617238323108737, -1.082531754730544860 ) ) ;
#124188 = CARTESIAN_POINT ( 'NONE',  ( 6.471319392424407901, 6.444294134116939077, 0.7998128361456341429 ) ) ;
#124189 = CARTESIAN_POINT ( 'NONE',  ( 1.124558466181435179, 1.288545020775376804, -1.735378439385642180 ) ) ;
#124192 = CARTESIAN_POINT ( 'NONE',  ( 5.016153647376217606, 4.954526798134778254, 0.7216878364870317197 ) ) ;
#124191 = CARTESIAN_POINT ( 'NONE',  ( 6.387299765813869712, 6.624473612970537495, 0.000000000000000000 ) ) ;
#124190 = CARTESIAN_POINT ( 'NONE',  ( 3.725458348705031231, 7.568394850123006279, -1.734723475976807094E-15 ) ) ;
#124193 = CARTESIAN_POINT ( 'NONE',  ( -3.492107083971660586, 6.231819477012331632, 1.199719254218452935 ) ) ;
#124194 = CARTESIAN_POINT ( 'NONE',  ( 6.051970301643104122, 1.040788372175960541, 1.727066800951609249 ) ) ;
#124196 = CARTESIAN_POINT ( 'NONE',  ( -5.546694241322218666, 8.524874810634301525, 1.082531754730550855 ) ) ;
#124195 = CARTESIAN_POINT ( 'NONE',  ( -7.836249599018719536, 12.08611559892311504, 0.7216878364870478180 ) ) ;
#124197 = LINE ( 'NONE', #189103, #153647 ) ;
#124199 = CARTESIAN_POINT ( 'NONE',  ( 1.364683531250000748, 10.50520833367473195, -0.7879004041258355073 ) ) ;
#124198 = CARTESIAN_POINT ( 'NONE',  ( 0.8314075926023238861, 0.1693486111025067908, 2.256218002396610522 ) ) ;
#124200 = CARTESIAN_POINT ( 'NONE',  ( -10.14557902172788495, 10.73093036830436553, 1.040834085586084257E-14 ) ) ;
#124202 = CARTESIAN_POINT ( 'NONE',  ( 6.450795914701256351, -1.844717532910484570, -0.8146137538835170888 ) ) ;
#124201 = CARTESIAN_POINT ( 'NONE',  ( -6.033015167956810920, 7.101234453113482559, -1.082531754730543083 ) ) ;
#124203 = CARTESIAN_POINT ( 'NONE',  ( 1.364683531249986537, 0.7177083336747527298, -0.7879004041258239610 ) ) ;
#124204 = CARTESIAN_POINT ( 'NONE',  ( -6.662120174140259365, -7.184999792969698262, 6.772456105771886392 ) ) ;
#124205 = EDGE_CURVE ( 'NONE', #142909, #159583, #68039, .T. ) ;
#124206 = CARTESIAN_POINT ( 'NONE',  ( 10.50000000000000178, 10.90000000000000036, -3.600000000000002309 ) ) ;
#124207 = CARTESIAN_POINT ( 'NONE',  ( 3.053030289171186684, -1.410389792183571966, -0.9926723171444253868 ) ) ;
#124208 = CARTESIAN_POINT ( 'NONE',  ( 3.464990776744291345, 6.200183785247111778, 1.199719254218452047 ) ) ;
#124209 = CARTESIAN_POINT ( 'NONE',  ( 6.879836604291781121, 6.991173891287354003, -0.7998128361456341429 ) ) ;
#124210 = PRESENTATION_LAYER_ASSIGNMENT (  '', '', ( #103387 ) ) ;
#124211 = CARTESIAN_POINT ( 'NONE',  ( 1.369957856843624366, -1.128201996292097498, 1.363478919461190708 ) ) ;
#124212 = CARTESIAN_POINT ( 'NONE',  ( 2.332683495817444719, 1.313167467523576715, -1.525923137932885476 ) ) ;
#124213 = CARTESIAN_POINT ( 'NONE',  ( -2.000000000000000000, 2.428612866367544447E-14, 1.733336949948522427E-30 ) ) ;
#124214 = CARTESIAN_POINT ( 'NONE',  ( 3.663272223086514234, -1.945104670120747059, -1.042327912031751458 ) ) ;
#124215 = EDGE_LOOP ( 'NONE', ( #168297, #85213, #149687, #99800 ) ) ;
#124216 = CARTESIAN_POINT ( 'NONE',  ( 7.402388682937041331, 11.57994453016116587, 1.040834085586084257E-14 ) ) ;
#124218 = CARTESIAN_POINT ( 'NONE',  ( 2.636342400811112707, 0.6820146075395253638, 1.897692325672148073 ) ) ;
#124217 = CARTESIAN_POINT ( 'NONE',  ( 4.881546266219149999, 0.2071824046101199135, -2.110321684233848583 ) ) ;
#124220 = EDGE_LOOP ( 'NONE', ( #114373, #48117, #2917, #140337 ) ) ;
#124219 = CARTESIAN_POINT ( 'NONE',  ( 3.234412676589659252, 1.145595053071927438, -1.403395578055862902 ) ) ;
#124221 = CARTESIAN_POINT ( 'NONE',  ( 3.576318658954677598, 7.394398545414291313, 0.7998128361456281477 ) ) ;
#124222 = EDGE_CURVE ( 'NONE', #214172, #162715, #51331, .T. ) ;
#124223 = ORIENTED_EDGE ( 'NONE', *, *, #193855, .T. ) ;
#124224 = CARTESIAN_POINT ( 'NONE',  ( 1.287742131874554552, -0.8442722623961744777, 1.669378388412197767 ) ) ;
#124225 = ADVANCED_FACE ( 'NONE', ( #1473 ), #119593, .T. ) ;
#124226 = CARTESIAN_POINT ( 'NONE',  ( 6.568987803155795113, -1.671525225137669102, -0.7347104647430282576 ) ) ;
#124228 = CARTESIAN_POINT ( 'NONE',  ( 2.764735878068668384, -0.1456047134679704924, -1.910273805325033436 ) ) ;
#124227 = CARTESIAN_POINT ( 'NONE',  ( -2.442440228756222353, 6.001264033524212671, -0.7998128361456281477 ) ) ;
#124229 = DIRECTION ( 'NONE',  ( 0.000000000000000000, 0.000000000000000000, -1.000000000000000000 ) ) ;
#124230 = SURFACE_SIDE_STYLE ('',( #188051 ) ) ;
#124231 = CARTESIAN_POINT ( 'NONE',  ( -0.6823417656250003738, 1.280208333674752508, -1.181850606188749264 ) ) ;
#124232 = CARTESIAN_POINT ( 'NONE',  ( 7.187230829020129441, 8.518095734345896730, 1.082531754730549967 ) ) ;
#124233 = CARTESIAN_POINT ( 'NONE',  ( -5.506019780925599960, 5.596313630600862510, 0.7216878364870257245 ) ) ;
#124234 = CARTESIAN_POINT ( 'NONE',  ( -6.505933609711270549, 8.683618192786854095, -1.599625672291271394 ) ) ;
#124235 = CARTESIAN_POINT ( 'NONE',  ( 3.269896953881154644, 0.5115095171020591636, -2.057881918134551125 ) ) ;
#124237 = CARTESIAN_POINT ( 'NONE',  ( -10.88586298614011660, 5.812970821470938354, 6.395187734525825896 ) ) ;
#124236 = CARTESIAN_POINT ( 'NONE',  ( -0.02968770228139669398, 7.629137130509076492, -2.426318643530885222 ) ) ;
#124238 = CARTESIAN_POINT ( 'NONE',  ( 3.884019131438942285, -0.9746410142534560617, 1.713524893406521699 ) ) ;
#124239 = CARTESIAN_POINT ( 'NONE',  ( -0.08764186210430401081, -2.012836238882615980, -0.04531326932211143105 ) ) ;
#124240 = VERTEX_POINT ( 'NONE', #66471 ) ;
#124241 = CARTESIAN_POINT ( 'NONE',  ( 0.03496603831146075092, -1.697522432243668389, 1.265142316669096934 ) ) ;
#124242 = SURFACE_STYLE_USAGE ( .BOTH. , #58080 ) ;
#124243 = CARTESIAN_POINT ( 'NONE',  ( 2.014207461368537455, 2.064961549741591185, -0.1501100615294431728 ) ) ;
#124244 = CARTESIAN_POINT ( 'NONE',  ( 6.505933609711257226, 8.683618192786854095, -1.599625672291281386 ) ) ;
#124245 = ORIENTED_EDGE ( 'NONE', *, *, #65741, .F. ) ;
#124246 = CARTESIAN_POINT ( 'NONE',  ( 6.066347387471824781, 6.042103138330730872, -0.7998128361456481317 ) ) ;
#124247 = CARTESIAN_POINT ( 'NONE',  ( 5.677832469072920496, 9.846164657218904992, 0.000000000000000000 ) ) ;
#124249 = CARTESIAN_POINT ( 'NONE',  ( 4.710568305744190276, 7.583081225755162968, 1.199719254218462483 ) ) ;
#124248 = CARTESIAN_POINT ( 'NONE',  ( 3.697287448106700403, -0.6068447087972194121, 2.000623839779874125 ) ) ;
#124250 = CARTESIAN_POINT ( 'NONE',  ( 7.472478939787284169, 8.746922180287201698, 1.199719254218452935 ) ) ;
#124251 = CARTESIAN_POINT ( 'NONE',  ( 0.6975727754284127835, 1.215713746931287753, 1.343078931132860587 ) ) ;
#124252 = CARTESIAN_POINT ( 'NONE',  ( 5.725267921653402148, -0.05769419298589681389, 2.206291853148376170 ) ) ;
#124253 = CIRCLE ( 'NONE', #117263, 2.000000000000000000 ) ;
#124254 = CARTESIAN_POINT ( 'NONE',  ( 0.04006801626470013478, -6.479296433800355359, -11.00029612940780410 ) ) ;
#124255 = CARTESIAN_POINT ( 'NONE',  ( 4.137865722265689605, -1.519559189622637252, -1.600479987451455699 ) ) ;
#124256 = CARTESIAN_POINT ( 'NONE',  ( 6.448874621594486989, 10.67543749183559143, 0.7998128361456462443 ) ) ;
#124257 = CARTESIAN_POINT ( 'NONE',  ( -0.6823417656250039265, 8.630208333674733723, -1.181850606188755259 ) ) ;
#124258 = CARTESIAN_POINT ( 'NONE',  ( 2.772007568003355793, 1.902874960710929431, -0.1895390408453850317 ) ) ;
#124259 = CARTESIAN_POINT ( 'NONE',  ( 8.829384350997564468, 11.32403438096243775, 1.599625672291281386 ) ) ;
#124260 = CARTESIAN_POINT ( 'NONE',  ( 5.213363469605923228, -1.747142239327776903, -1.110534646669825376 ) ) ;
#124262 = CARTESIAN_POINT ( 'NONE',  ( 2.483474991488154870, 1.976725341044349271, -0.8753317036461552014 ) ) ;
#124261 = CARTESIAN_POINT ( 'NONE',  ( 1.541006503187393850, 8.695732182938039401, -2.510084419394968513 ) ) ;
#124263 = CARTESIAN_POINT ( 'NONE',  ( 6.462441986028243157, -2.002789442531027309, -0.8901952361822995652 ) ) ;
#124264 = ORIENTED_EDGE ( 'NONE', *, *, #114516, .F. ) ;
#124265 = EDGE_LOOP ( 'NONE', ( #171186, #79075, #8644, #214288, #44876 ) ) ;
#124266 = AXIS2_PLACEMENT_3D ( 'NONE', #51959, #202432, #83365 ) ;
#124267 = PRESENTATION_STYLE_ASSIGNMENT (( #125326 ) ) ;
#124268 = CARTESIAN_POINT ( 'NONE',  ( 9.499606442108968096, -9.900000000000019895, -0.08647222121521722094 ) ) ;
#124269 = CARTESIAN_POINT ( 'NONE',  ( 5.910428620914669473, 5.860197910680708944, 0.000000000000000000 ) ) ;
#124270 = CARTESIAN_POINT ( 'NONE',  ( -0.6823417656250003738, 15.21354166700806410, 1.181850606188754593 ) ) ;
#124271 = CARTESIAN_POINT ( 'NONE',  ( -0.2102771530458276972, -0.008943344768330967198, -2.203482896658349066 ) ) ;
#124272 = CARTESIAN_POINT ( 'NONE',  ( -6.724481002698120768, 9.828683022247721723, -1.082531754730538864 ) ) ;
#124273 = CARTESIAN_POINT ( 'NONE',  ( 5.899733120602060232, 6.912052057904395141, -1.199719254218452047 ) ) ;
#124274 = CARTESIAN_POINT ( 'NONE',  ( 5.717656431054087385, 0.4094431674900833595, -2.029196096928844284 ) ) ;
#124275 = CARTESIAN_POINT ( 'NONE',  ( 4.881433204766033818, 1.796953459403265674, -0.6949688560347905275 ) ) ;
#124276 = CARTESIAN_POINT ( 'NONE',  ( 0.4039230143318903177, -1.081087622585241714, -1.701935196855845822 ) ) ;
#124277 = CARTESIAN_POINT ( 'NONE',  ( -10.08065090696061716, 11.71951313199760136, -1.199719254218441611 ) ) ;
#124278 = CARTESIAN_POINT ( 'NONE',  ( 3.061108821635398769, 6.793320401875094561, -0.7998128361456362523 ) ) ;
#124279 = CARTESIAN_POINT ( 'NONE',  ( -4.649416048473335117, 6.918063047017545486, -1.244856393069911915 ) ) ;
#124280 = CARTESIAN_POINT ( 'NONE',  ( 6.615150229029130635, -2.225211831249251482, 0.5499996461680799476 ) ) ;
#124281 = CARTESIAN_POINT ( 'NONE',  ( 4.881388680972561289, 1.702354803207173584, -0.6601141376258444771 ) ) ;
#124282 = CARTESIAN_POINT ( 'NONE',  ( 6.726253606155519371, 7.019919760035800316, -0.7216878364870458196 ) ) ;
#124284 = ADVANCED_FACE ( 'NONE', ( #35056 ), #52395, .T. ) ;
#124283 = CARTESIAN_POINT ( 'NONE',  ( 2.372313692266983853, 5.711523707712699682, 0.7216878364870438212 ) ) ;
#124285 = CARTESIAN_POINT ( 'NONE',  ( -4.118644803501354978, 8.027112380718707030, 0.7998128361456352531 ) ) ;
#124286 = CARTESIAN_POINT ( 'NONE',  ( 4.095444919779759552, 6.935713618788495793, 1.199719254218451159 ) ) ;
#124287 = ORIENTED_EDGE ( 'NONE', *, *, #62427, .T. ) ;
#124289 = CARTESIAN_POINT ( 'NONE',  ( 5.801044709096109031, -0.2997443204828981189, -1.990672168044338886 ) ) ;
#124288 = CARTESIAN_POINT ( 'NONE',  ( 2.911469271472226339, -0.9098125248445630975, -1.600700954789348263 ) ) ;
#124290 = CARTESIAN_POINT ( 'NONE',  ( 1.195116192591906046, -1.458952948520657156, -1.775991855458454838 ) ) ;
#124291 = CARTESIAN_POINT ( 'NONE',  ( 6.262552437187629550, -0.7028992384056665932, -1.831702256219314151 ) ) ;
#124292 = CARTESIAN_POINT ( 'NONE',  ( -4.557512192488103686, 8.468847991211438497, -0.7998128361456281477 ) ) ;
#124293 = CARTESIAN_POINT ( 'NONE',  ( 10.34804403480040236, -6.705807696128828432, 9.269928574751062911E-15 ) ) ;
#124294 = CARTESIAN_POINT ( 'NONE',  ( -2.625475302540713152, 6.214804952939456228, -0.7998128361456281477 ) ) ;
#124295 = CARTESIAN_POINT ( 'NONE',  ( 0.5200892513525963157, 2.048054262204841880, -0.3022008342252607838 ) ) ;
#124296 = CARTESIAN_POINT ( 'NONE',  ( -5.334207092333882017, 5.187939460669764635, 0.7998128361456281477 ) ) ;
#124298 = CARTESIAN_POINT ( 'NONE',  ( 1.569004590881704075, 0.1408476687595125731, -1.865417194689425795 ) ) ;
#124297 = CARTESIAN_POINT ( 'NONE',  ( 2.261376066768826743, 2.049819659885134371, -0.4107522398083974791 ) ) ;
#124299 = CARTESIAN_POINT ( 'NONE',  ( 2.126327167286511166, 0.3474154575464418748, -1.985796285822030161 ) ) ;
#124300 = CARTESIAN_POINT ( 'NONE',  ( 7.619319141200051604, 11.83303006480134911, 0.7216878364870438212 ) ) ;
#124301 = ORIENTED_EDGE ( 'NONE', *, *, #143273, .T. ) ;
#124302 = CARTESIAN_POINT ( 'NONE',  ( -1.201851678989727383E-14, 3.884375000341423689, 1.575800808251672791 ) ) ;
#124303 = CARTESIAN_POINT ( 'NONE',  ( 2.524636229566870060, -1.623295675544262906, 0.6281775017502010394 ) ) ;
#124304 = CARTESIAN_POINT ( 'NONE',  ( 6.145923705696426431, 6.064665832934283962, 0.7998128361456341429 ) ) ;
#124306 = DIRECTION ( 'NONE',  ( 1.000000000000000000, 0.000000000000000000, -4.336808689942017736E-15 ) ) ;
#124305 = CARTESIAN_POINT ( 'NONE',  ( 1.250000000000037526, 8.500000000000000000, 11.02939254900286237 ) ) ;
#124307 = CARTESIAN_POINT ( 'NONE',  ( 2.824480366436402878, 1.624150206794371609, 0.5811974035451406007 ) ) ;
#124309 = EDGE_CURVE ( 'NONE', #40788, #44957, #18941, .T. ) ;
#124308 = CARTESIAN_POINT ( 'NONE',  ( 2.366952063387484095, 0.1042156695447923470, -2.189191704635709890 ) ) ;
#124310 = CARTESIAN_POINT ( 'NONE',  ( 5.742855475442601332, 0.4270144693867898300, 2.165010647329483895 ) ) ;
#124311 = CARTESIAN_POINT ( 'NONE',  ( -10.21576913194658864, 4.000029896383376027, -7.512182378973799146 ) ) ;
#124312 = CARTESIAN_POINT ( 'NONE',  ( 1.938562956190786002, -1.164097522067691903, 1.832441342696682574 ) ) ;
#124313 = CARTESIAN_POINT ( 'NONE',  ( 1.189776066567624691, -0.8228614858879386151, 1.629801898503015156 ) ) ;
#124314 = CARTESIAN_POINT ( 'NONE',  ( 3.046228577489984879, 0.9562745863303960814, 1.889201325992972080 ) ) ;
#124315 = CARTESIAN_POINT ( 'NONE',  ( 6.539320575229256249, 2.979067782826943844, 2.350490835693248126 ) ) ;
#124316 = EDGE_LOOP ( 'NONE', ( #53721, #156403 ) ) ;
#124318 = CARTESIAN_POINT ( 'NONE',  ( 0.6823417656249882723, 1.488541667008083547, -1.181850606188749264 ) ) ;
#124317 = CARTESIAN_POINT ( 'NONE',  ( 4.142302782979132125, 0.6112592793995803575, 2.209291399377455889 ) ) ;
#124319 = CARTESIAN_POINT ( 'NONE',  ( -2.091679895156829610E-15, 2.562499999999987121, 1.224999999999973888 ) ) ;
#124320 = CARTESIAN_POINT ( 'NONE',  ( 4.715538499454675403, 4.395883092318884522, 1.214306433183764966E-14 ) ) ;
#124321 = CARTESIAN_POINT ( 'NONE',  ( 6.551452540055466400, -1.985718062329771438, 0.9957849561875466993 ) ) ;
#124322 = CARTESIAN_POINT ( 'NONE',  ( -5.531363484695544841, 8.436712584578003771, 1.082531754730548412 ) ) ;
#124323 = CARTESIAN_POINT ( 'NONE',  ( 4.365362273920250225, 5.155639410070820716, 1.082531754730560403 ) ) ;
#124324 = CARTESIAN_POINT ( 'NONE',  ( -7.036318535368094373, 7.311385834125318617, 0.7216878364870317197 ) ) ;
#124325 = CARTESIAN_POINT ( 'NONE',  ( 0.07804503809599044883, -9.997560133496188328, 10.91958144425262311 ) ) ;
#124326 = ORIENTED_EDGE ( 'NONE', *, *, #72117, .F. ) ;
#124327 = CARTESIAN_POINT ( 'NONE',  ( 4.342422763466713853, 0.4390309838058319425, -1.967887491402267486 ) ) ;
#124329 = CARTESIAN_POINT ( 'NONE',  ( 3.397386871994355850, -1.821155587584430302, 0.9682287363927607471 ) ) ;
#124328 = CARTESIAN_POINT ( 'NONE',  ( 6.257251587906815793, 7.258880593101466161, 1.199719254218462483 ) ) ;
#124330 = CARTESIAN_POINT ( 'NONE',  ( 7.842465510862060896, 8.114240948952696542, 0.000000000000000000 ) ) ;
#124331 = CARTESIAN_POINT ( 'NONE',  ( 4.299344108864946890, 6.109263775132799168, -1.443375672974068769 ) ) ;
#124333 = EDGE_CURVE ( 'NONE', #66793, #89199, #118522, .T. ) ;
#124332 = CARTESIAN_POINT ( 'NONE',  ( 3.285556943750000514, -3.113541666188709645, 1.896917185911906500 ) ) ;
#124334 = LINE ( 'NONE', #174088, #96039 ) ;
#124335 = CARTESIAN_POINT ( 'NONE',  ( 6.158177532299373702, -1.552315630085840947, 1.547116483708823598 ) ) ;
#124336 = CARTESIAN_POINT ( 'NONE',  ( 3.902970337090125863, -1.038992709432768891, -1.728002613881730598 ) ) ;
#124337 = CARTESIAN_POINT ( 'NONE',  ( 3.561895345837225779, -1.234009368583251387, 1.366721199326895952 ) ) ;
#124338 = EDGE_CURVE ( 'NONE', #51191, #82895, #124939, .T. ) ;
#124339 = CARTESIAN_POINT ( 'NONE',  ( 6.632963465583686435, 8.761543347979550589, -1.599625672291262513 ) ) ;
#124340 = CARTESIAN_POINT ( 'NONE',  ( 6.282242891264209206, -0.9739734823789309992, 1.543877162560060912 ) ) ;
#124341 = CARTESIAN_POINT ( 'NONE',  ( -6.738566041191992539, 7.820414121934134322, 1.199719254218450271 ) ) ;
#124342 = CARTESIAN_POINT ( 'NONE',  ( 6.508658281791896094, 1.681912584842374159, -1.513523023287469016 ) ) ;
#124343 = CARTESIAN_POINT ( 'NONE',  ( 1.576933964714849701, -2.000244969732989819, -0.6594162861879059312 ) ) ;
#124344 = CARTESIAN_POINT ( 'NONE',  ( -5.960744811863571968, 6.983232364376142698, 1.199719254218452935 ) ) ;
#124345 = CARTESIAN_POINT ( 'NONE',  ( 6.726816770674637347, 10.99970333242910669, -0.7998128361456291469 ) ) ;
#124346 = CARTESIAN_POINT ( 'NONE',  ( 5.655159470231527763, 9.611786791996525636, -0.7216878364870458196 ) ) ;
#124347 = SHAPE_REPRESENTATION_RELATIONSHIP ( 'NONE' , 'NONE' ,  #141543, #184056 ) ;
#124348 = CARTESIAN_POINT ( 'NONE',  ( -7.386494761346872551, 7.511998731193139989, -0.7998128361456291469 ) ) ;
#124349 = CARTESIAN_POINT ( 'NONE',  ( -0.07801928546529091069, -7.184999792974072541, 9.499679989893808241 ) ) ;
#124350 = CARTESIAN_POINT ( 'NONE',  ( 7.470179451005385829, 8.777926116670192513, -1.082531754730537976 ) ) ;
#124351 = CARTESIAN_POINT ( 'NONE',  ( 4.383065840713377348, 7.132475524829186675, -1.069666325224464032 ) ) ;
#124352 = CARTESIAN_POINT ( 'NONE',  ( -4.574986769607567894, 7.424902766929059261, 1.199719254218464037 ) ) ;
#124353 = CARTESIAN_POINT ( 'NONE',  ( 3.814843914748572207, -0.6992408500761657653, -2.108525230111441218 ) ) ;
#124354 = CARTESIAN_POINT ( 'NONE',  ( 0.7443833103580774768, 0.6396484562771962423, 2.096019810003430184 ) ) ;
#124355 = CARTESIAN_POINT ( 'NONE',  ( 0.3291288957359936318, 2.113116833900237967, 0.6364493931270903682 ) ) ;
#124357 =( GEOMETRIC_REPRESENTATION_CONTEXT ( 3 ) GLOBAL_UNCERTAINTY_ASSIGNED_CONTEXT ( ( #177282 ) ) GLOBAL_UNIT_ASSIGNED_CONTEXT ( ( #210372, #133438, #83575 ) ) REPRESENTATION_CONTEXT ( 'NONE', 'WORKASPACE' ) );
#124356 = CARTESIAN_POINT ( 'NONE',  ( -4.447956913735107598, 7.346977611736363656, 1.199719254218452935 ) ) ;
#124358 = CARTESIAN_POINT ( 'NONE',  ( 4.088298575758734898, 1.051444423028622399, -1.656135347060924135 ) ) ;
#124359 = CARTESIAN_POINT ( 'NONE',  ( 9.752392566931574081, 10.27221283770866300, -0.7998128361456281477 ) ) ;
#124360 = CARTESIAN_POINT ( 'NONE',  ( -5.602744053211161201, 6.190815373437144942, 0.8771416995774529157 ) ) ;
#124361 = DIRECTION ( 'NONE',  ( -1.000000000000000000, 0.000000000000000000, 0.000000000000000000 ) ) ;
#124362 = CARTESIAN_POINT ( 'NONE',  ( 0.6823417656249882723, 1.176041667008083325, -1.181850606188749264 ) ) ;
#124363 = CARTESIAN_POINT ( 'NONE',  ( -3.024877669624710386, 6.543124691288523920, 0.000000000000000000 ) ) ;
#124365 = ORIENTED_EDGE ( 'NONE', *, *, #153278, .T. ) ;
#124364 = CARTESIAN_POINT ( 'NONE',  ( -6.914295153289458540, 7.169025221700239925, 0.7216878364870317197 ) ) ;
#124366 = CARTESIAN_POINT ( 'NONE',  ( 3.603867943843573673, 1.538443694073919898, 1.459757404076333698 ) ) ;
#124367 = CARTESIAN_POINT ( 'NONE',  ( -5.483346782084204563, 5.361935765378481378, 0.000000000000000000 ) ) ;
#124368 = CARTESIAN_POINT ( 'NONE',  ( 5.524359596833869013, 1.291058806671550485, -1.733668313432787933 ) ) ;
#124369 = CARTESIAN_POINT ( 'NONE',  ( 3.931074656914943954, -1.272613488525012659, -1.330884258478791438 ) ) ;
#124370 = CARTESIAN_POINT ( 'NONE',  ( -5.762141863986474100, 6.090740110424618159, 0.6348889758391648153 ) ) ;
#124371 = CARTESIAN_POINT ( 'NONE',  ( -1.402160292154681736E-14, 1.759375000341421469, -1.575800808251659024 ) ) ;
#124372 = CARTESIAN_POINT ( 'NONE',  ( -0.04197470322641042723, -1.553021824201283208, -0.7857045047398486526 ) ) ;
#124373 = CARTESIAN_POINT ( 'NONE',  ( 11.33772463945043718, 12.69999999999997264, 3.600000000000075140 ) ) ;
#124374 = CARTESIAN_POINT ( 'NONE',  ( 3.226477370372305753, 4.787309570232886280, 1.443375672974062551 ) ) ;
#124375 = CARTESIAN_POINT ( 'NONE',  ( 0.7500000000000006661, 11.83333333333333393, 1.299038105676657340 ) ) ;
#124376 = ADVANCED_FACE ( 'NONE', ( #169342 ), #103843, .T. ) ;
#124377 = CARTESIAN_POINT ( 'NONE',  ( 4.416967121957662279, 1.975198431823081302, 0.8787980929093119897 ) ) ;
#124378 = CARTESIAN_POINT ( 'NONE',  ( 5.571638683613604037, 1.528505562557905595, -1.314797328242120367 ) ) ;
#124379 = CARTESIAN_POINT ( 'NONE',  ( -6.982085920913410071, 11.08959130780024260, 0.7216878364870458196 ) ) ;
#124380 = CARTESIAN_POINT ( 'NONE',  ( 3.643588467267334874, -1.635511012911139650, -1.413612897787956513 ) ) ;
#124381 = CARTESIAN_POINT ( 'NONE',  ( 3.954335293022055886, 0.7064427249091516092, 1.840614667007954841 ) ) ;
#124382 =( LENGTH_UNIT ( ) NAMED_UNIT ( * ) SI_UNIT ( .MILLI., .METRE. ) );
#124383 = CARTESIAN_POINT ( 'NONE',  ( 1.044460364342413072, 0.9324277726035223868, -2.110995228001291579 ) ) ;
#124384 = CARTESIAN_POINT ( 'NONE',  ( 3.690745141589413691, -0.3983964448436724259, -2.021722667813256269 ) ) ;
#124385 = CARTESIAN_POINT ( 'NONE',  ( 5.214377421777850685, 1.795891487756570815, 0.7396389662707256729 ) ) ;
#124387 = ORIENTED_EDGE ( 'NONE', *, *, #143394, .T. ) ;
#124386 = CARTESIAN_POINT ( 'NONE',  ( -7.144783764277399030, 11.27940545839156528, 0.7216878364870458196 ) ) ;
#124388 = CARTESIAN_POINT ( 'NONE',  ( -5.444481204339554736, 8.509589284108232121, 1.199719254218454489 ) ) ;
#124389 = DIRECTION ( 'NONE',  ( -5.578564026256490882E-16, -1.000000000000000000, -9.066213480720158442E-32 ) ) ;
#124391 = VERTEX_POINT ( 'NONE', #12710 ) ;
#124390 =( NAMED_UNIT ( * ) SI_UNIT ( $, .STERADIAN. ) SOLID_ANGLE_UNIT ( ) );
#124392 = CARTESIAN_POINT ( 'NONE',  ( -6.670248387799091461, 10.72578085250020585, 0.000000000000000000 ) ) ;
#124393 = CARTESIAN_POINT ( 'NONE',  ( 2.186817281270125424, -2.164169025584137263, -0.4306803264119417607 ) ) ;
#124394 = CARTESIAN_POINT ( 'NONE',  ( 1.001543065824772753E-15, -0.3718749995220430038, 3.793834371823811669 ) ) ;
#124395 = CARTESIAN_POINT ( 'NONE',  ( 6.719590461409528537, 0.3385411321301828314, -1.932175811092277096 ) ) ;
#124396 = CARTESIAN_POINT ( 'NONE',  ( -0.02880301295726198432, 7.629137130509075604, -2.873797191217826619 ) ) ;
#124398 = B_SPLINE_CURVE_WITH_KNOTS ( 'NONE', 3,
 ( #139042, #24182, #152079, #88141 ),
 .UNSPECIFIED., .F., .F.,
 ( 4, 4 ),
 ( 0.5002441414044666024, 0.5750605836579747443 ),
 .UNSPECIFIED. ) ;
#124397 = CARTESIAN_POINT ( 'NONE',  ( 0.6170404364503330186, 3.466143782776612170, -1.902435570468861137 ) ) ;
#124400 = CARTESIAN_POINT ( 'NONE',  ( -10.99036836684472540, -7.696788179137225683, 0.4651914231089842033 ) ) ;
#124399 = CARTESIAN_POINT ( 'NONE',  ( 1.499999999999990896, 5.056250000682820378, 1.214306433183764966E-14 ) ) ;
#124401 = CARTESIAN_POINT ( 'NONE',  ( 5.648353745280480176, -1.448853643138726000, 1.135948691490688667 ) ) ;
#124402 = ORIENTED_EDGE ( 'NONE', *, *, #167734, .F. ) ;
#124403 = CARTESIAN_POINT ( 'NONE',  ( 2.588805925060005730, -0.3509353788873382229, -2.030617818815634745 ) ) ;
#124404 = CARTESIAN_POINT ( 'NONE',  ( 1.360316468749977581, 0.5364583336746844289, -0.7853790794159001276 ) ) ;
#124405 = CARTESIAN_POINT ( 'NONE',  ( -6.693975156845199059, 8.832723654451292816, 1.599625672291283607 ) ) ;
#124406 = CARTESIAN_POINT ( 'NONE',  ( -2.916975605234527702, 6.554888639415577423, 1.040834085586084257E-14 ) ) ;
#124407 = DIRECTION ( 'NONE',  ( 0.000000000000000000, -1.000000000000000000, 0.000000000000000000 ) ) ;
#124408 = PRESENTATION_LAYER_ASSIGNMENT (  '', '', ( #34312 ) ) ;
#124409 = CARTESIAN_POINT ( 'NONE',  ( 4.741601036477289810, 6.554953847355395880, 1.599625672291267398 ) ) ;
#124410 = CARTESIAN_POINT ( 'NONE',  ( 1.217730312517154800, -2.010830008989676898, 0.4507304159913956831 ) ) ;
#124412 = CARTESIAN_POINT ( 'NONE',  ( 5.231922985772964552, 1.814955821992572993, 0.3091130605668013231 ) ) ;
#124411 = CARTESIAN_POINT ( 'NONE',  ( -10.79363438595513891, 4.456531630721114468, -5.247043704664541508 ) ) ;
#124413 = CARTESIAN_POINT ( 'NONE',  ( 6.662942426112080874, 9.860851032851066122, 1.199719254218460707 ) ) ;
#124414 = CARTESIAN_POINT ( 'NONE',  ( -9.372156330827838389, 14.58101807628380264, -7.405769076522356720 ) ) ;
#124415 = CARTESIAN_POINT ( 'NONE',  ( -4.294900800479008574, 8.232744377192641849, 0.000000000000000000 ) ) ;
#124417 = ORIENTED_EDGE ( 'NONE', *, *, #84764, .F. ) ;
#124416 = CARTESIAN_POINT ( 'NONE',  ( 6.610000000000030518, 1.266345627986571021, 2.115470293623383569 ) ) ;
#124418 = CARTESIAN_POINT ( 'NONE',  ( 4.776106669258010307, 1.268914099295117781, 1.805409367619143390 ) ) ;
#124419 = CARTESIAN_POINT ( 'NONE',  ( 0.6148119136215323133, 1.491057340773978668, -1.565211586912764741 ) ) ;
#124420 = CIRCLE ( 'NONE', #30959, 0.08000000000000018208 ) ;
#124421 = CARTESIAN_POINT ( 'NONE',  ( -5.178851490740209229, 7.065079377328788546, 1.443375672974064550 ) ) ;
#124422 = CARTESIAN_POINT ( 'NONE',  ( 0.4395310841842986482, -1.815173276516975243, 0.6020934215927520317 ) ) ;
#124423 = CARTESIAN_POINT ( 'NONE',  ( 6.034394305845959927, 0.6080466156053351279, 1.816710885969755163 ) ) ;
#124424 = CARTESIAN_POINT ( 'NONE',  ( -6.385527162356468445, 10.39360608948380538, 1.040834085586084257E-14 ) ) ;
#124425 = CARTESIAN_POINT ( 'NONE',  ( 1.669710354559012622, -0.8274895997400324443, -2.144421126502197517 ) ) ;
#124426 = VECTOR ( 'NONE', #111483, 1000.000000000000000 ) ;
#124427 = CARTESIAN_POINT ( 'NONE',  ( 0.07536363704237906969, 4.084105538841027894, -2.698926661290324880 ) ) ;
#124428 = CARTESIAN_POINT ( 'NONE',  ( 5.074826771331380826, -1.382354945563003312, 1.321565576914075502 ) ) ;
#124429 = CARTESIAN_POINT ( 'NONE',  ( 11.44791656467458552, 12.30000000000000071, -3.303228920649581291 ) ) ;
#124430 = CARTESIAN_POINT ( 'NONE',  ( 0.7252172114964609007, -1.777616610744123804, 0.5828384007960025759 ) ) ;
#124431 = CARTESIAN_POINT ( 'NONE',  ( 2.923064838257955156, -1.776166165677966591, 0.9548571111624851726 ) ) ;
#124433 = CARTESIAN_POINT ( 'NONE',  ( 3.721394855333003626, -0.1548319924524182156, 2.100431540652194062 ) ) ;
#124432 = CARTESIAN_POINT ( 'NONE',  ( -9.176171038350775078, 9.599954387697719582, -0.7998128361456291469 ) ) ;
#124434 = CARTESIAN_POINT ( 'NONE',  ( 6.448874621594486989, 10.67543749183559143, 0.7998128361456462443 ) ) ;
#124436 = CARTESIAN_POINT ( 'NONE',  ( -7.609150525767646833, 9.900428251527500834, -1.599625672291263179 ) ) ;
#124435 = CARTESIAN_POINT ( 'NONE',  ( 0.7499999999999885647, -0.2666666666666442365, 1.299038105676657340 ) ) ;
#124437 = CARTESIAN_POINT ( 'NONE',  ( -5.249999999999987566, -0.9165151389911689872, 1.199999999999999734 ) ) ;
#124438 = CARTESIAN_POINT ( 'NONE',  ( 3.656514325482379757, 2.010451960178538222, 0.1936393378089220907 ) ) ;
#124439 = CARTESIAN_POINT ( 'NONE',  ( 1.364683531249990311, 4.863541667008084879, 0.7879004041258500513 ) ) ;
#124440 = CARTESIAN_POINT ( 'NONE',  ( 8.758204044747998296, 11.24099069033793974, 1.443375672974076540 ) ) ;
#124441 = CARTESIAN_POINT ( 'NONE',  ( 4.745497693432328745, -1.667575968047749546, -1.375352955852253922 ) ) ;
#124442 = CARTESIAN_POINT ( 'NONE',  ( 6.550524494058025837, 7.671308660269694712, -1.199719254218452047 ) ) ;
#124443 = EDGE_CURVE ( 'NONE', #125480, #31312, #191962, .T. ) ;
#124444 = CARTESIAN_POINT ( 'NONE',  ( -1.500000000000011324, 5.129166666666691299, -0.8660254037844313801 ) ) ;
#124445 = CARTESIAN_POINT ( 'NONE',  ( 6.261886844665240481, 8.398896966899865646, 1.599625672291268286 ) ) ;
#124446 = CARTESIAN_POINT ( 'NONE',  ( 9.219181267168295335, 9.858059021225592744, 1.040834085586084257E-14 ) ) ;
#124448 = CARTESIAN_POINT ( 'NONE',  ( 5.738313685646321716, 5.917571446856333850, 2.440166996132847377 ) ) ;
#124447 = CARTESIAN_POINT ( 'NONE',  ( 1.539757937649718800, 2.006347644133343433, -0.8302594476135690682 ) ) ;
#124450 = CARTESIAN_POINT ( 'NONE',  ( 1.100829259350871281, -0.4471758257712907247, 1.786007343351428966 ) ) ;
#124449 = CARTESIAN_POINT ( 'NONE',  ( -4.433153041988574294, 8.115836282387899558, 1.040834085586084257E-14 ) ) ;
#124451 = CARTESIAN_POINT ( 'NONE',  ( -1.201851678989727383E-14, 1.821875000341421691, 1.575800808251672791 ) ) ;
#124452 = CARTESIAN_POINT ( 'NONE',  ( 3.597391730528697540, -0.6346259394694170330, 2.097678010650514402 ) ) ;
#124453 = CARTESIAN_POINT ( 'NONE',  ( 6.883263157960404222, 3.695221384915627905, 2.468000959490519897 ) ) ;
#124454 = CARTESIAN_POINT ( 'NONE',  ( 4.276442053719103242, -1.305714526237568229, 1.847550228136185302 ) ) ;
#124455 = CARTESIAN_POINT ( 'NONE',  ( -6.181627972826976958, 9.299317504018391745, 1.199719254218452047 ) ) ;
#124456 = CARTESIAN_POINT ( 'NONE',  ( 0.6823417656249917140, 5.155208333674749177, 1.181850606188765695 ) ) ;
#124457 = CARTESIAN_POINT ( 'NONE',  ( 6.426609430950597890, 6.789993649951097332, 0.4362094596595481599 ) ) ;
#124458 = CARTESIAN_POINT ( 'NONE',  ( 1.499999999999993117, 11.85416666666666430, 0.8660254037844409281 ) ) ;
#124459 = CARTESIAN_POINT ( 'NONE',  ( 6.373741612200174878, 6.608655767087927124, 0.7216878364870328300 ) ) ;
#124460 = CARTESIAN_POINT ( 'NONE',  ( 4.692510491889085422, -0.3870912556891945577, -1.726709192852653230 ) ) ;
#124461 = COLOUR_RGB ( '', 0.66274510, 0.83137255, 0.94901961) ;
#124462 = CARTESIAN_POINT ( 'NONE',  ( 8.555358625423188812, 9.940005470203933768, 1.199719254218462483 ) ) ;
#124463 = CARTESIAN_POINT ( 'NONE',  ( 0.5871190474453058528, -0.2578297629921856293, -2.090033075799145657 ) ) ;
#124465 = CARTESIAN_POINT ( 'NONE',  ( 0.7499999999999885647, 1.566666666666688412, -1.299038105676652899 ) ) ;
#124464 = CARTESIAN_POINT ( 'NONE',  ( -0.6823417656250039265, 11.06770833367473550, -1.181850606188755259 ) ) ;
#124466 = CARTESIAN_POINT ( 'NONE',  ( 1.012081461190861065, 1.967466754592902989, -0.09309286250217158054 ) ) ;
#124467 = CARTESIAN_POINT ( 'NONE',  ( -4.930325137224961907, 5.781076077297750970, -1.199719254218453823 ) ) ;
#124468 = CARTESIAN_POINT ( 'NONE',  ( 0.2386218892466463737, -1.902018210125755004, -0.4804332253167050149 ) ) ;
#124469 = ORIENTED_EDGE ( 'NONE', *, *, #82621, .F. ) ;
#124470 = CARTESIAN_POINT ( 'NONE',  ( 6.805829924380105034, 9.923590097543378619, 1.082531754730558626 ) ) ;
#124471 = EDGE_CURVE ( 'NONE', #195242, #27525, #94012, .T. ) ;
#124472 = CARTESIAN_POINT ( 'NONE',  ( 5.278141497218024725, -1.038406966791558528, 1.555765341417144842 ) ) ;
#124473 = ORIENTED_EDGE ( 'NONE', *, *, #48815, .F. ) ;
#124474 = B_SPLINE_CURVE_WITH_KNOTS ( 'NONE', 3,
 ( #181392, #167287, #33015, #17796, #99094, #35127, #165146, #82823, #149974, #1544, #67606 ),
 .UNSPECIFIED., .F., .F.,
 ( 4, 1, 1, 1, 1, 1, 1, 1, 4 ),
 ( 0.000000000000000000, 0.2255234228546724728, 0.3973271701647976828, 0.5245128843546777997, 0.6161923999872991331, 0.6815320185768301009, 0.7298552812456317040, 0.7704940248801678271, 1.000000000000000000 ),
 .UNSPECIFIED. ) ;
#124475 = CARTESIAN_POINT ( 'NONE',  ( 4.170806909802426965, 1.467596682293986765, -1.460439952253207663 ) ) ;
#124476 = CARTESIAN_POINT ( 'NONE',  ( -1.225000000000019407, 2.500000000000009326, -1.387778780781445676E-14 ) ) ;
#124477 = CARTESIAN_POINT ( 'NONE',  ( -5.709392084686210289, 8.714688961225625974, 1.082531754730550855 ) ) ;
#124478 = CARTESIAN_POINT ( 'NONE',  ( 9.264299036839600987, 9.702770385934682551, -0.7998128361456281477 ) ) ;
#124479 = CARTESIAN_POINT ( 'NONE',  ( -10.64045162862669081, 11.30828174301964140, -0.7998128361456221525 ) ) ;
#124480 = FACE_OUTER_BOUND ( 'NONE', #138227, .T. ) ;
#124481 = CARTESIAN_POINT ( 'NONE',  ( 7.334597915313080918, 9.580116872663850813, 1.040834085586084257E-14 ) ) ;
#124482 = CARTESIAN_POINT ( 'NONE',  ( 1.364683531249986981, -1.115624999658580752, 0.000000000000000000 ) ) ;
#124483 = CARTESIAN_POINT ( 'NONE',  ( 1.499999999999989120, 0.5250000000000185629, 0.000000000000000000 ) ) ;
#124484 = CARTESIAN_POINT ( 'NONE',  ( 4.246505328441081417, -1.940195102956907336, -0.2900488188990399396 ) ) ;
#124485 = CARTESIAN_POINT ( 'NONE',  ( 2.618517346670693247, 0.5404096030681635465, -1.942243668081746311 ) ) ;
#124486 = EDGE_CURVE ( 'NONE', #54906, #182393, #86096, .T. ) ;
#124487 = FACE_OUTER_BOUND ( 'NONE', #176274, .T. ) ;
#124488 = FILL_AREA_STYLE ('',( #87636 ) ) ;
#124489 = CARTESIAN_POINT ( 'NONE',  ( 1.493192106177696044, 1.412881632968411516, 1.225925835885120829 ) ) ;
#124490 = CARTESIAN_POINT ( 'NONE',  ( -0.6823417656249969321, 4.967708333674755394, -1.181850606188749264 ) ) ;
#124491 = CARTESIAN_POINT ( 'NONE',  ( 2.513933912945048199, -0.6273889547634775576, 1.913045067402745936 ) ) ;
#124493 = CARTESIAN_POINT ( 'NONE',  ( 3.550509549652399066, -1.420143166946661317, 1.570484981737807706 ) ) ;
#124492 = CARTESIAN_POINT ( 'NONE',  ( -4.744990575102892905, 8.479646737687938085, 0.7216878364870458196 ) ) ;
#124494 = CARTESIAN_POINT ( 'NONE',  ( -2.549999999999999378, 1.000000000000000888, 1.849324200890692271 ) ) ;
#124495 = CARTESIAN_POINT ( 'NONE',  ( 4.756339170418532269, -2.069830778647030023, -0.05414847147890837487 ) ) ;
#124496 = CARTESIAN_POINT ( 'NONE',  ( 5.993586425693011144, 9.150212042353954800, -1.199719254218452047 ) ) ;
#124498 = CARTESIAN_POINT ( 'NONE',  ( 6.720655732516665815, 3.683894443391816154, 2.687682123607849416 ) ) ;
#124497 = CARTESIAN_POINT ( 'NONE',  ( 0.4684514965578719381, -1.969967889910573033, -0.7007429371770137472 ) ) ;
#124500 = EDGE_LOOP ( 'NONE', ( #25045, #168535, #97699, #22887 ) ) ;
#124499 = CARTESIAN_POINT ( 'NONE',  ( 5.825187583072056974, -0.04236064406601056098, 1.825263316621673848 ) ) ;
#124501 = CARTESIAN_POINT ( 'NONE',  ( 7.401861798056875053, 10.72292363345333399, -1.199719254218441611 ) ) ;
#124502 = CARTESIAN_POINT ( 'NONE',  ( 8.074422843257124782, -6.701288531902056533, -7.470306724222344208 ) ) ;
#124503 = MECHANICAL_DESIGN_GEOMETRIC_PRESENTATION_REPRESENTATION (  '', ( #37991 ), #186713 ) ;
#124504 = CARTESIAN_POINT ( 'NONE',  ( -9.510677803526956353, 3.006766436585398772, 6.782528980676592489 ) ) ;
#124505 = CARTESIAN_POINT ( 'NONE',  ( 1.364683531249996529, 12.52604166700806232, 0.7879004041258403923 ) ) ;
#124506 = CARTESIAN_POINT ( 'NONE',  ( 5.690081826675051246, 1.142623417513729089, 1.533212917768103534 ) ) ;
#124507 = CARTESIAN_POINT ( 'NONE',  ( -8.971744963941075568, 11.49012176272984931, 1.599625672291269396 ) ) ;
#124508 = CARTESIAN_POINT ( 'NONE',  ( 5.445571254183207088, 9.504916896522420444, -0.7998128361456281477 ) ) ;
#124509 = CARTESIAN_POINT ( 'NONE',  ( -11.86239285000045918, 11.37999999999999901, -1.812080536912753059 ) ) ;
#124510 = CARTESIAN_POINT ( 'NONE',  ( 3.728129053633592704, 4.412200653069714207, -1.082531754730543083 ) ) ;
#124511 = PLANE ( 'NONE',  #151500 ) ;
#124512 = CARTESIAN_POINT ( 'NONE',  ( 3.662674053986138656, 7.424870162959149589, 0.7998128361456321445 ) ) ;
#124513 = VERTEX_POINT ( 'NONE', #91882 ) ;
#124514 = CARTESIAN_POINT ( 'NONE',  ( -6.424584688029276514, 8.588711117491191871, 1.599625672291269396 ) ) ;
#124515 = STYLED_ITEM ( 'NONE', ( #56615 ), #12474 ) ;
#124516 = CARTESIAN_POINT ( 'NONE',  ( 5.220327442464319567, 1.987051044970666647, 0.3419161450798278157 ) ) ;
#124517 = FACE_OUTER_BOUND ( 'NONE', #114229, .T. ) ;
#124518 = CARTESIAN_POINT ( 'NONE',  ( 3.046330065665291187, 6.497876143344064381, -0.2071306710573911913 ) ) ;
#124519 = CARTESIAN_POINT ( 'NONE',  ( -6.490830876026181251, 6.764709549658621590, 0.1777360701797660314 ) ) ;
#124520 =( BOUNDED_SURFACE ( )  B_SPLINE_SURFACE ( 3, 2, ( 
 ( #161010, #49390, #99211 ),
 ( #585, #112325, #47283 ),
 ( #145863, #195647, #165260 ),
 ( #113395, #80827, #82936 ) ),
 .UNSPECIFIED., .F., .F., .T. ) 
 B_SPLINE_SURFACE_WITH_KNOTS ( ( 4, 4 ),
 ( 3, 3 ),
 ( 0.01127358803094579559, 0.01374177962974961961 ),
 ( 0.000000000000000000, 1.000000000000000000 ),
 .UNSPECIFIED. ) 
 GEOMETRIC_REPRESENTATION_ITEM ( )  RATIONAL_B_SPLINE_SURFACE ( (
 ( 1.000000000000000000, 0.6947640035331676955, 1.000000000000000000),
 ( 1.000000000000000000, 0.6955505939615566069, 1.000000000000000000),
 ( 1.000000000000000000, 0.6961913616428424545, 1.000000000000000000),
 ( 1.000000000000000000, 0.6967468848049996888, 1.000000000000000000) ) ) 
 REPRESENTATION_ITEM ( '' )  SURFACE ( )  );
#124521 = CARTESIAN_POINT ( 'NONE',  ( -5.422898255786198440, 7.349800603215774331, -1.443375672974052559 ) ) ;
#124522 = CARTESIAN_POINT ( 'NONE',  ( 10.05978679165993839, 10.83876546646586014, 0.7216878364870438212 ) ) ;
#124523 = CARTESIAN_POINT ( 'NONE',  ( 1.973436150528505406, -0.2460485697947655814, 1.953970194506114755 ) ) ;
#124524 = CARTESIAN_POINT ( 'NONE',  ( 3.181267708840180841, 1.591331833097202830, 1.238305487465785948 ) ) ;
#124525 = CARTESIAN_POINT ( 'NONE',  ( -7.263417608619167076, 9.497073181520933716, -1.599625672291263179 ) ) ;
#124526 = CARTESIAN_POINT ( 'NONE',  ( 6.727182134110239353, -0.007837387828812587484, 2.289081727344749684 ) ) ;
#124527 = CARTESIAN_POINT ( 'NONE',  ( 3.363397379774799134, 2.138023915923603635, -0.4802275100637617977 ) ) ;
#124528 = CARTESIAN_POINT ( 'NONE',  ( -5.000000000000013323, 8.499999999999996447, 0.7750000000000004663 ) ) ;
#124529 = CARTESIAN_POINT ( 'NONE',  ( 2.204012588094861780, -1.926017964255047010, 0.04517517324725479899 ) ) ;
#124530 = CARTESIAN_POINT ( 'NONE',  ( -7.995557903757128493, 10.35123685918189729, 1.599625672291295375 ) ) ;
#124531 = DIRECTION ( 'NONE',  ( 1.000000000000000000, -1.250471828332824404E-35, -1.561251128379126077E-17 ) ) ;
#124532 = CARTESIAN_POINT ( 'NONE',  ( 0.2329586101569553480, 1.399178205689523224, -2.105666472772389941 ) ) ;
#124533 = CARTESIAN_POINT ( 'NONE',  ( -4.795850251199142988, 15.51848109270388854, -11.00904932811271486 ) ) ;
#124535 = EDGE_CURVE ( 'NONE', #30915, #99612, #112433, .T. ) ;
#124534 = CARTESIAN_POINT ( 'NONE',  ( 7.151035956204054855, 10.43029348462504124, 1.199719254218460707 ) ) ;
#124536 = CARTESIAN_POINT ( 'NONE',  ( 4.961394147597008697, 7.875711374583454827, -1.199719254218452047 ) ) ;
#124537 = CARTESIAN_POINT ( 'NONE',  ( -0.6125000000000279110, 1.291666666666656305, 1.060881119635892933 ) ) ;
#124538 = CARTESIAN_POINT ( 'NONE',  ( 4.733205024946604667, 8.536173272497439513, 0.000000000000000000 ) ) ;
#124539 = EDGE_LOOP ( 'NONE', ( #102798, #185950, #78308, #106305 ) ) ;
#124541 = CARTESIAN_POINT ( 'NONE',  ( 3.457684585873057159, -1.525941150838805216, -1.313146537923309376 ) ) ;
#124540 = CARTESIAN_POINT ( 'NONE',  ( 6.304252605626877504, 1.359535501544101077, -1.241908024382516240 ) ) ;
#124542 = CARTESIAN_POINT ( 'NONE',  ( 4.411641467711771014, 0.6073606466481770161, 2.216650271500276492 ) ) ;
#124544 = CARTESIAN_POINT ( 'NONE',  ( 2.746734941909965588, -0.3128536233567563163, -1.834277165529672793 ) ) ;
#124543 = CARTESIAN_POINT ( 'NONE',  ( -0.02880301295729841352, 5.718910385480866054, -2.867850616339829628 ) ) ;
#124545 = CARTESIAN_POINT ( 'NONE',  ( -1.642778471874998480, -0.4010416661887096224, 2.845375778867863303 ) ) ;
#124546 = CARTESIAN_POINT ( 'NONE',  ( 11.94105721237523277, 10.90000000000000036, -1.187919463087249827 ) ) ;
#124547 = CARTESIAN_POINT ( 'NONE',  ( -1.123270288249902160, 2.800000000000024691, 0.7750000000000117906 ) ) ;
#124548 = CARTESIAN_POINT ( 'NONE',  ( -7.965578943228732278, 9.251929174310385307, -1.199719254218446718 ) ) ;
#124549 = CARTESIAN_POINT ( 'NONE',  ( -3.350273356352693188, 6.922752992471175482, 0.000000000000000000 ) ) ;
#124550 = CARTESIAN_POINT ( 'NONE',  ( 6.392138156072928901, -0.5583118246898631787, -2.014728688386701272 ) ) ;
#124551 = CARTESIAN_POINT ( 'NONE',  ( 7.185458225562760148, 8.445751353653788485, -1.082531754730543083 ) ) ;
#124552 = ORIENTED_EDGE ( 'NONE', *, *, #165324, .F. ) ;
#124553 = CARTESIAN_POINT ( 'NONE',  ( 0.000000000000000000, 4.000000000000002665, 0.000000000000000000 ) ) ;
#124555 = CARTESIAN_POINT ( 'NONE',  ( 4.878236342818665250, 4.585697242910212523, 1.040834085586084257E-14 ) ) ;
#124554 = CARTESIAN_POINT ( 'NONE',  ( 4.699688308863886554, 8.280832412640696916, 0.6266364797024156497 ) ) ;
#124556 = CARTESIAN_POINT ( 'NONE',  ( 6.481054518252093111, -0.09278056567359710405, -1.722521162943893014 ) ) ;
#124557 = CARTESIAN_POINT ( 'NONE',  ( -6.084912014434944894, 5.993485526462540847, -0.7998128361456291469 ) ) ;
#124558 = CARTESIAN_POINT ( 'NONE',  ( 1.933800834616914877, -1.393042465158848886, -1.032573028607612464 ) ) ;
#124559 = CARTESIAN_POINT ( 'NONE',  ( 1.734723475976807094E-15, 14.55305236562695193, 11.95586206896570580 ) ) ;
#124560 = DIRECTION ( 'NONE',  ( 0.000000000000000000, 0.000000000000000000, -1.000000000000000000 ) ) ;
#124561 = CARTESIAN_POINT ( 'NONE',  ( 6.350449713519967787, -2.159805286613075470, -0.2212482231108928721 ) ) ;
#124562 = CARTESIAN_POINT ( 'NONE',  ( 4.529811765687052016, -1.125283923072720071, -1.437579299059896343 ) ) ;
#124563 = CARTESIAN_POINT ( 'NONE',  ( 2.623818369222921554, 1.924856029493416276, -0.3778354045670463401 ) ) ;
#124564 = FILL_AREA_STYLE_COLOUR ( '', #16262 ) ;
#124565 = LINE ( 'NONE', #127773, #22829 ) ;
#124566 = CARTESIAN_POINT ( 'NONE',  ( 9.264299036839600987, 9.702770385934682551, -0.7998128361456281477 ) ) ;
#124567 = CARTESIAN_POINT ( 'NONE',  ( 4.196021508500130004, 1.385991406618786836, 1.604897850144955340 ) ) ;
#124568 = CARTESIAN_POINT ( 'NONE',  ( -2.331639231870358930, 5.664070170583284103, -0.7216878364870267237 ) ) ;
#124569 = CARTESIAN_POINT ( 'NONE',  ( 3.147653791585693028, 8.920000000000001705, 2.419999999999999485 ) ) ;
#124570 = CARTESIAN_POINT ( 'NONE',  ( -4.981332701451811396, 6.629279788159643694, -1.242877772926734625 ) ) ;
#124571 = CARTESIAN_POINT ( 'NONE',  ( 1.868117093089691760, -2.055091939184821026, 0.2493290443424806546 ) ) ;
#124573 = CARTESIAN_POINT ( 'NONE',  ( 0.6823417656249864960, -1.011458332991911568, -1.181850606188749264 ) ) ;
#124572 = CARTESIAN_POINT ( 'NONE',  ( -10.91970695577495398, -9.999999999999994671, -0.07999999999999153621 ) ) ;
#124575 = ORIENTED_EDGE ( 'NONE', *, *, #6451, .F. ) ;
#124574 = CARTESIAN_POINT ( 'NONE',  ( 3.932468528151237042, -1.142516171320803853, -1.904832733444387971 ) ) ;
#124576 = CARTESIAN_POINT ( 'NONE',  ( 1.969760627029959688, -2.255332599139341809, -0.4437108664413855763 ) ) ;
#124578 = CARTESIAN_POINT ( 'NONE',  ( 6.912941059211402894, -1.598140348199797556, 1.303530876689311224 ) ) ;
#124577 = CARTESIAN_POINT ( 'NONE',  ( 8.595506201384004896, 12.01154575404795466, 1.082531754730546636 ) ) ;
#124580 = CARTESIAN_POINT ( 'NONE',  ( -3.285556943749998737, -3.930208332855377407, 1.896917185911908499 ) ) ;
#124579 = CARTESIAN_POINT ( 'NONE',  ( 5.740951700743842423, 5.662474837148078421, -0.7998128361456481317 ) ) ;
#124581 = EDGE_CURVE ( 'NONE', #171576, #102576, #16249, .T. ) ;
#124582 = CARTESIAN_POINT ( 'NONE',  ( 1.446532937691837683E-15, 15.15766726230651606, 11.68000000000000504 ) ) ;
#124583 = FACE_OUTER_BOUND ( 'NONE', #103714, .T. ) ;
#124584 = CARTESIAN_POINT ( 'NONE',  ( -0.1106727585416019261, 5.721739388512169455, -2.597565591738408841 ) ) ;
#124585 = CARTESIAN_POINT ( 'NONE',  ( 3.223388876545678183, -1.662537434388009938, 0.4588695312727729125 ) ) ;
#124586 = CARTESIAN_POINT ( 'NONE',  ( 2.553923023464285347, 1.082840749376843270, 1.700961377887353798 ) ) ;
#124587 = CARTESIAN_POINT ( 'NONE',  ( 2.708015267422092531, 2.165615165066101966, 0.7711511238016451886 ) ) ;
#124588 = CARTESIAN_POINT ( 'NONE',  ( 3.233911077135812384, -1.516719621523674677, -1.678889276187053081 ) ) ;
#124589 = CARTESIAN_POINT ( 'NONE',  ( 5.180345272937711520, -1.170841012621581134, 1.750402278287941149 ) ) ;
#124590 = CARTESIAN_POINT ( 'NONE',  ( -5.316205630334251531, 9.216340645449683677, -0.7216878364870338292 ) ) ;
#124591 = ORIENTED_EDGE ( 'NONE', *, *, #14312, .T. ) ;
#124592 = CARTESIAN_POINT ( 'NONE',  ( 3.831107792978345472, -1.636083747181043879, 0.6751729126634566924 ) ) ;
#124593 = EDGE_CURVE ( 'NONE', #36461, #80335, #7011, .T. ) ;
#124595 = CARTESIAN_POINT ( 'NONE',  ( 6.023008118121612853, -2.159854764417634687, 0.7684156934805678185 ) ) ;
#124594 = CARTESIAN_POINT ( 'NONE',  ( 5.221298554594243413, 5.264138866547622975, -0.7216878364870458196 ) ) ;
#124596 = CARTESIAN_POINT ( 'NONE',  ( 5.894452933195245770, 1.502573388107550034, -1.063714819228026132 ) ) ;
#124597 = CARTESIAN_POINT ( 'NONE',  ( -2.462777459176719308, 6.024990802348131780, -0.7998128361456281477 ) ) ;
#124598 = CARTESIAN_POINT ( 'NONE',  ( -1.500000000000013101, 3.629166666666692187, -0.8660254037844313801 ) ) ;
#124599 = CARTESIAN_POINT ( 'NONE',  ( 6.175747540105122724, -1.175446681380667213, 1.849350104233343783 ) ) ;
#124600 = CARTESIAN_POINT ( 'NONE',  ( -4.322352044658376968, 3.937165561723182883, 0.7998128361456341429 ) ) ;
#124601 = CARTESIAN_POINT ( 'NONE',  ( -11.33772463945037146, 10.19999999999998153, 3.679999999999999272 ) ) ;
#124602 = CARTESIAN_POINT ( 'NONE',  ( 6.039524589772497620, 1.914416561877980261, -0.7887839105886890190 ) ) ;
#124603 = CARTESIAN_POINT ( 'NONE',  ( 0.6379081216283178923, 2.014007883293071899, -0.1037844182863178755 ) ) ;
#124604 =( BOUNDED_SURFACE ( )  B_SPLINE_SURFACE ( 3, 2, ( 
 ( #136416, #206719, #24765 ),
 ( #138544, #89809, #153722 ),
 ( #106084, #73521, #58347 ),
 ( #72443, #123447, #189409 ),
 ( #158000, #155854, #90867 ),
 ( #107160, #41051, #121298 ) ),
 .UNSPECIFIED., .F., .F., .F. ) 
 B_SPLINE_SURFACE_WITH_KNOTS ( ( 4, 2, 4 ),
 ( 3, 3 ),
 ( 0.000000000000000000, 0.0003754689591423960443, 0.0007509379182847920886 ),
 ( 0.000000000000000000, 1.000000000000000000 ),
 .UNSPECIFIED. ) 
 GEOMETRIC_REPRESENTATION_ITEM ( )  RATIONAL_B_SPLINE_SURFACE ( (
 ( 1.000000000000000000, 0.7071067811865399122, 1.000000000000000000),
 ( 1.000000000000000000, 0.7018599272026960767, 1.000000000000000000),
 ( 1.000000000000000000, 0.6927733177256535368, 1.000000000000000000),
 ( 1.000000000000000000, 0.6772007068877564651, 1.000000000000000000),
 ( 1.000000000000000000, 0.6709974581634203794, 1.000000000000000000),
 ( 1.000000000000000000, 0.6711954675835395401, 1.000000000000000000) ) ) 
 REPRESENTATION_ITEM ( '' )  SURFACE ( )  );
#124605 =( GEOMETRIC_REPRESENTATION_CONTEXT ( 3 ) GLOBAL_UNCERTAINTY_ASSIGNED_CONTEXT ( ( #33417 ) ) GLOBAL_UNIT_ASSIGNED_CONTEXT ( ( #37663, #43025, #142664 ) ) REPRESENTATION_CONTEXT ( 'NONE', 'WORKASPACE' ) );
#124606 = CARTESIAN_POINT ( 'NONE',  ( -1.201851678989727383E-14, 4.071875000341425022, 1.575800808251672791 ) ) ;
#124607 = CARTESIAN_POINT ( 'NONE',  ( 3.492722931844041145, -0.3765888977748827471, -1.889173544197232824 ) ) ;
#124608 = CARTESIAN_POINT ( 'NONE',  ( 0.6823417656249934904, 10.44270833367473550, 1.181850606188764807 ) ) ;
#124609 = CARTESIAN_POINT ( 'NONE',  ( -4.134873662487946966, 3.926366815765101936, 1.214306433183764966E-14 ) ) ;
#124610 = CARTESIAN_POINT ( 'NONE',  ( 0.3170205077604414945, -0.7560223448306638838, -2.088923821510160650 ) ) ;
#124612 = ORIENTED_EDGE ( 'NONE', *, *, #11740, .T. ) ;
#124611 = CARTESIAN_POINT ( 'NONE',  ( 4.415115299905642665, 5.179997933758551554, -1.199719254218450271 ) ) ;
#124614 = DIRECTION ( 'NONE',  ( 0.000000000000000000, 0.000000000000000000, -1.000000000000000000 ) ) ;
#124613 = CARTESIAN_POINT ( 'NONE',  ( 3.947104627881618200, 8.980740528188865923, 0.7749999999999996891 ) ) ;
#124615 = CARTESIAN_POINT ( 'NONE',  ( 2.703961570921634028, 5.242040035128820108, -1.199719254218446718 ) ) ;
#124616 = DIRECTION ( 'NONE',  ( -0.000000000000000000, -1.000000000000000000, -0.000000000000000000 ) ) ;
#124617 = LINE ( 'NONE', #7554, #26639 ) ;
#124618 = CARTESIAN_POINT ( 'NONE',  ( 8.023115266309142513, -5.166862915010145052, -7.407835137441765916 ) ) ;
#124619 = CARTESIAN_POINT ( 'NONE',  ( 1.644895634054041933, -0.2845770130874228365, -1.940982728367894206 ) ) ;
#124620 = CARTESIAN_POINT ( 'NONE',  ( 1.364683531249986537, 1.176041667008082658, 0.7879004041258500513 ) ) ;
#124621 = CARTESIAN_POINT ( 'NONE',  ( -0.5773502691960585853, -4.295408888567775918, 1.000000000000000888 ) ) ;
#124622 = CARTESIAN_POINT ( 'NONE',  ( 5.160583804383015227, -0.6592509027269661814, -1.847929681152965520 ) ) ;
#124623 = CARTESIAN_POINT ( 'NONE',  ( -9.494787648271923786, 9.971673765939062406, 1.040834085586084257E-14 ) ) ;
#124624 = EDGE_CURVE ( 'NONE', #89432, #87871, #171262, .T. ) ;
#124625 = CARTESIAN_POINT ( 'NONE',  ( -5.436456408955534947, 6.405249234278626247, 1.082531754730546636 ) ) ;
#124626 = CARTESIAN_POINT ( 'NONE',  ( 6.508665849870632236, 1.605377118863276387, -1.447859449074364591 ) ) ;
#124628 = ORIENTED_EDGE ( 'NONE', *, *, #194299, .F. ) ;
#124627 = CARTESIAN_POINT ( 'NONE',  ( -0.1653080603930669190, -5.324706741106404628, -10.99896775280364025 ) ) ;
#124629 = CARTESIAN_POINT ( 'NONE',  ( -0.6823417656249969321, 5.217708333674756283, -1.181850606188749264 ) ) ;
#124630 = CARTESIAN_POINT ( 'NONE',  ( 0.8427765623921362748, -1.607460297381148928, 0.9563107477488577146 ) ) ;
#124631 = CARTESIAN_POINT ( 'NONE',  ( 5.712138547670210009, -1.368237114983595237, -1.064765744168968187 ) ) ;
#124633 = CARTESIAN_POINT ( 'NONE',  ( 3.245827600587628758, 2.191739723504753101, -0.002129563554123526260 ) ) ;
#124632 = CARTESIAN_POINT ( 'NONE',  ( 5.007715329123863766E-16, 0.8281250003414059035, -1.570758158831786266 ) ) ;
#124634 = CARTESIAN_POINT ( 'NONE',  ( 4.682853559034357183, -2.237096095179165633, -0.5655516052204231370 ) ) ;
#124635 = B_SPLINE_CURVE_WITH_KNOTS ( 'NONE', 3,
 ( #131822, #146990, #197831, #48420, #133949, #213008, #100339, #66732, #49464, #180526 ),
 .UNSPECIFIED., .F., .F.,
 ( 4, 3, 3, 4 ),
 ( 1.970267125075963426E-17, 3.125277950706723017E-05, 6.250528927673665086E-05, 0.0001035880062255934710 ),
 .UNSPECIFIED. ) ;
#124636 = CARTESIAN_POINT ( 'NONE',  ( 0.1806374041631699234, -1.998871265498179506, -0.5013196448642556202 ) ) ;
#124637 = CARTESIAN_POINT ( 'NONE',  ( 2.765492612253204641, 1.039303555060458351, 1.640259502831205918 ) ) ;
#124638 = CARTESIAN_POINT ( 'NONE',  ( -5.707619481228834779, 5.761236937629489852, -0.7216878364870197293 ) ) ;
#124639 = CARTESIAN_POINT ( 'NONE',  ( -6.776323704810612192, -7.189630408300039299, -6.777912011469588549 ) ) ;
#124640 = CARTESIAN_POINT ( 'NONE',  ( 5.484674493353773883, -1.343714522216314489, 1.640574901390474460 ) ) ;
#124641 = CARTESIAN_POINT ( 'NONE',  ( 0.6125000000000123679, 2.916666666666671404, -1.060881119635948444 ) ) ;
#124642 = CARTESIAN_POINT ( 'NONE',  ( 3.305314717767214638, 1.277042846462652204, -1.560500556308255238 ) ) ;
#124643 = CARTESIAN_POINT ( 'NONE',  ( -4.243338890952901288, 6.934017225211593249, -1.082531754730548412 ) ) ;
#124644 = CARTESIAN_POINT ( 'NONE',  ( -5.447343857640614573, 9.577261277214532242, -0.7998128361456362523 ) ) ;
#124645 = CARTESIAN_POINT ( 'NONE',  ( 10.26082332744404368, 10.86538205830655279, -0.7998128361456281477 ) ) ;
#124646 = CARTESIAN_POINT ( 'NONE',  ( 1.453431991042982041, 0.5316948868413253759, -1.746555546766684675 ) ) ;
#124647 = CARTESIAN_POINT ( 'NONE',  ( -4.450819567036169211, 8.414649604842665553, -0.7998128361456362523 ) ) ;
#124648 = CARTESIAN_POINT ( 'NONE',  ( -5.818384198920079520, 6.817144982608731141, 1.199719254218452935 ) ) ;
#124649 = CARTESIAN_POINT ( 'NONE',  ( -4.624015273241393942, 8.365221982611680929, 0.3117065211258822077 ) ) ;
#124650 = ORIENTED_EDGE ( 'NONE', *, *, #25859, .T. ) ;
#124651 = CARTESIAN_POINT ( 'NONE',  ( 5.506733764336206427, 1.562011470896901288, -1.344504574768749627 ) ) ;
#124652 = CARTESIAN_POINT ( 'NONE',  ( -5.709392084686210289, 8.714688961225625974, 1.082531754730550855 ) ) ;
#124653 = UNCERTAINTY_MEASURE_WITH_UNIT (LENGTH_MEASURE( 1.000000000000000082E-05 ), #205548, 'distance_accuracy_value', 'NONE');
#124654 = CARTESIAN_POINT ( 'NONE',  ( -4.874319919312905647, 5.645460313075203018, -1.199719254218446718 ) ) ;
#124655 = CARTESIAN_POINT ( 'NONE',  ( -4.167152111353897403, 5.955039778036558040, 1.599625672291270506 ) ) ;
#124656 = CARTESIAN_POINT ( 'NONE',  ( 4.231121231147261241, 1.847467856137770204, 0.8164654241873505747 ) ) ;
#124657 = CARTESIAN_POINT ( 'NONE',  ( 5.813180279319686505, 1.817354232980341378, -1.277000798603223464 ) ) ;
#124659 = CARTESIAN_POINT ( 'NONE',  ( 8.432808358020015049, 11.82173160345663376, 1.082531754730546636 ) ) ;
#124658 = CARTESIAN_POINT ( 'NONE',  ( -4.679499295372141709, 5.488445928469455559, 1.199719254218452935 ) ) ;
#124660 = CARTESIAN_POINT ( 'NONE',  ( 5.575427483717746213, 7.527751369135936343, 1.599625672291267398 ) ) ;
#124661 = CARTESIAN_POINT ( 'NONE',  ( 4.715729953790866347, -2.021515393979388175, 0.4000037541747498704 ) ) ;
#124662 = CARTESIAN_POINT ( 'NONE',  ( 3.445935549842124690, -1.779626424299302956, -0.9480406757386842242 ) ) ;
#124663 = ORIENTED_EDGE ( 'NONE', *, *, #148115, .T. ) ;
#124664 = CARTESIAN_POINT ( 'NONE',  ( 1.913843809498031012, 3.268536626279791690, -0.4294081188993625342 ) ) ;
#124665 = CARTESIAN_POINT ( 'NONE',  ( 5.366329872910639232, 5.155139694684188534, 1.040834085586084257E-14 ) ) ;
#124667 = ORIENTED_EDGE ( 'NONE', *, *, #6610, .T. ) ;
#124666 = CARTESIAN_POINT ( 'NONE',  ( -7.553827861469316396, 8.841829255582865699, -1.199719254218452047 ) ) ;
#124668 = CARTESIAN_POINT ( 'NONE',  ( 4.915098833515745724, 8.004322973991836676, -0.9888141558981374812 ) ) ;
#124669 = CARTESIAN_POINT ( 'NONE',  ( 3.497422563753574298, 1.966343570655813666, 0.4444343670074250574 ) ) ;
#124670 = CARTESIAN_POINT ( 'NONE',  ( 2.185277780439310202, -0.7877041259056734024, 1.664256631099890971 ) ) ;
#124671 = CARTESIAN_POINT ( 'NONE',  ( 0.9444605492630732124, 0.9306326543588975264, -2.111904739147156818 ) ) ;
#124672 = CARTESIAN_POINT ( 'NONE',  ( 7.075376061485196821, 9.347967719856493218, 1.599625672291268286 ) ) ;
#124673 = CARTESIAN_POINT ( 'NONE',  ( 3.954491917119377753, 0.7739500986865335275, 2.018479124525011770 ) ) ;
#124674 = CARTESIAN_POINT ( 'NONE',  ( -6.749261541504576911, 6.768559974710451677, 1.040834085586084257E-14 ) ) ;
#124675 = VECTOR ( 'NONE', #95541, 1000.000000000000000 ) ;
#124676 = VERTEX_POINT ( 'NONE', #130820 ) ;
#124677 = CARTESIAN_POINT ( 'NONE',  ( -10.91970695577495931, -6.134628647623513231, 0.000000000000000000 ) ) ;
#124678 = CARTESIAN_POINT ( 'NONE',  ( 1.850267049257280139, 0.5840378008528935849, 1.777222254475477659 ) ) ;
#124679 = CARTESIAN_POINT ( 'NONE',  ( 6.192255011402767018, -1.961924197356275323, -0.1938383548326528261 ) ) ;
#124681 = CARTESIAN_POINT ( 'NONE',  ( 9.422553571373278203, 11.05569592376608945, -1.082531754730543083 ) ) ;
#124680 = CARTESIAN_POINT ( 'NONE',  ( -0.6823417656249969321, 5.217708333674756283, -1.181850606188749264 ) ) ;
#124683 = CARTESIAN_POINT ( 'NONE',  ( 0.06543086261080394150, -1.973449318085427340, -0.9880335165917543128 ) ) ;
#124682 = CARTESIAN_POINT ( 'NONE',  ( -4.876128802409253282, 8.840567369452784874, 0.7998128361456481317 ) ) ;
#124684 = DIRECTION ( 'NONE',  ( 0.000000000000000000, 1.000000000000000000, 0.000000000000000000 ) ) ;
#124685 = CARTESIAN_POINT ( 'NONE',  ( 6.179819089730593795, 6.104210447640811665, 1.040834085586084257E-14 ) ) ;
#124686 = CARTESIAN_POINT ( 'NONE',  ( -4.076197739202962467, 7.907314462378773001, 1.040834085586084257E-14 ) ) ;
#124687 = FACE_OUTER_BOUND ( 'NONE', #98463, .T. ) ;
#124688 = CARTESIAN_POINT ( 'NONE',  ( 5.823112234018508637, -0.04902082458170010926, 1.971020750367402430 ) ) ;
#124689 = CARTESIAN_POINT ( 'NONE',  ( 5.285860113471884780, 1.546311580504238670, 1.713158476844111933 ) ) ;
#124690 = CARTESIAN_POINT ( 'NONE',  ( 6.355886303346764521, -0.6260325832568144344, 1.752714347800623518 ) ) ;
#124691 = CARTESIAN_POINT ( 'NONE',  ( 2.729405006034294257, 0.1058063225414084541, -2.059999219628326994 ) ) ;
#124692 = CARTESIAN_POINT ( 'NONE',  ( 5.327991180490514012, 9.159814110640187579, 1.040834085586084257E-14 ) ) ;
#124693 = CARTESIAN_POINT ( 'NONE',  ( 7.693325821111733021, 7.940244644243982464, -0.7998128361456341429 ) ) ;
#124694 = CARTESIAN_POINT ( 'NONE',  ( 7.917598520256366790, 8.339545816494993602, 1.040834085586084257E-14 ) ) ;
#124695 = CARTESIAN_POINT ( 'NONE',  ( 1.364683531249986537, 2.717708333674754062, -0.7879004041258239610 ) ) ;
#124696 = CARTESIAN_POINT ( 'NONE',  ( -5.540667111194848893, 14.48160243150212523, 10.65389079987404486 ) ) ;
#124697 = CARTESIAN_POINT ( 'NONE',  ( 5.788968402910812827, 6.816513227226497662, 1.082531754730558626 ) ) ;
#124698 = CARTESIAN_POINT ( 'NONE',  ( 5.318865801915546143, -1.576246948875639209, 1.493384065191505350 ) ) ;
#124700 = CARTESIAN_POINT ( 'NONE',  ( 3.720104550828434942, 1.749555917645674530, 0.5740644926693627692 ) ) ;
#124699 = CARTESIAN_POINT ( 'NONE',  ( 7.320879633048903241E-15, 0.3750000006828252408, 1.224999999999981659 ) ) ;
#124702 = DIRECTION ( 'NONE',  ( 0.000000000000000000, 0.000000000000000000, -1.000000000000000000 ) ) ;
#124701 = CARTESIAN_POINT ( 'NONE',  ( 0.6823417656249899377, 5.676041667008087543, -1.181850606188754593 ) ) ;
#124703 = CARTESIAN_POINT ( 'NONE',  ( 6.409741707328596938, -1.031184584194230647, -1.933826218581576439 ) ) ;
#124704 = CARTESIAN_POINT ( 'NONE',  ( 1.195384358724066508E-16, -4.140708350189171938, 1.000000000000004441 ) ) ;
#124705 = CARTESIAN_POINT ( 'NONE',  ( 6.684454173705361768, -2.217265373380904681, -0.4495064082850850906 ) ) ;
#124706 = CARTESIAN_POINT ( 'NONE',  ( -3.999491622362644883, 7.816382810427971783, -0.3443157113667428271 ) ) ;
#124707 = CARTESIAN_POINT ( 'NONE',  ( -3.719872605471121751, 6.605953636083950364, 2.499999999999999556 ) ) ;
#124708 = CARTESIAN_POINT ( 'NONE',  ( 6.576141308597898139, 6.785670920958930985, -0.3094590540993913952 ) ) ;
#124709 = CARTESIAN_POINT ( 'NONE',  ( -5.953438849732214599, 6.118302544208584770, 0.7216878364870257245 ) ) ;
#124710 = CARTESIAN_POINT ( 'NONE',  ( 11.88235317400313917, 13.75664239773029962, 0.9089793033029933689 ) ) ;
#124711 = CARTESIAN_POINT ( 'NONE',  ( 0.3558548230270657808, 0.6711484630133063289, 1.637870061858819559 ) ) ;
#124712 = CARTESIAN_POINT ( 'NONE',  ( 4.899092244908956673, -0.2488113327579875855, -1.997608342807774218 ) ) ;
#124713 = B_SPLINE_CURVE_WITH_KNOTS ( 'NONE', 3,
 ( #141978, #93218, #27109, #146232, #30332, #212249, #143049 ),
 .UNSPECIFIED., .F., .F.,
 ( 4, 3, 4 ),
 ( 0.0001135037246152898908, 0.0006245292469112882598, 0.002007692286193825740 ),
 .UNSPECIFIED. ) ;
#124714 = CARTESIAN_POINT ( 'NONE',  ( 4.469384193999260901, 8.366031992974468423, -0.7998128361456231517 ) ) ;
#124715 = CARTESIAN_POINT ( 'NONE',  ( 4.436618261691759102, 2.064837277596673903, 0.4132364508900014943 ) ) ;
#124717 = CARTESIAN_POINT ( 'NONE',  ( 3.233901216830310954, 1.915793140838128572, -0.003097617167701141160 ) ) ;
#124716 = CARTESIAN_POINT ( 'NONE',  ( -4.582292731294565158, 4.448355729372827305, 1.214306433183764966E-14 ) ) ;
#124718 = CARTESIAN_POINT ( 'NONE',  ( 0.04570195657714280074, 1.813436143228261743, -11.99992749206847975 ) ) ;
#124719 = CARTESIAN_POINT ( 'NONE',  ( 3.736728436007582310, -1.897426337869069668, -0.5277852043128227200 ) ) ;
#124720 = CARTESIAN_POINT ( 'NONE',  ( 5.906511930418064438, -2.010445946205151380, -0.1936997237232794822 ) ) ;
#124721 = CARTESIAN_POINT ( 'NONE',  ( 2.289737743334671283, -0.8020533187339595749, 1.690132462187944107 ) ) ;
#124723 = CARTESIAN_POINT ( 'NONE',  ( 0.9141475326900462273, -1.912571728325639153, 0.002704284578637640348 ) ) ;
#124722 = CARTESIAN_POINT ( 'NONE',  ( 5.145002536317147879, -1.476695180717332967, 0.8911356905443221788 ) ) ;
#124725 = CARTESIAN_POINT ( 'NONE',  ( 3.063779527008304360, 6.518233848244248563, 0.7216878364870317197 ) ) ;
#124724 = CARTESIAN_POINT ( 'NONE',  ( 2.280145854635793334, 1.358931147977986420, 1.738775483816151768 ) ) ;
#124727 = EDGE_CURVE ( 'NONE', #45587, #55041, #2059, .T. ) ;
#124726 = CONICAL_SURFACE ( 'NONE', #152310, 3.000000000000000000, 0.7853981633974523868 ) ;
#124728 = CARTESIAN_POINT ( 'NONE',  ( 1.364683531249988535, 2.176041667008087543, 0.7879004041258500513 ) ) ;
#124729 = CARTESIAN_POINT ( 'NONE',  ( 6.689906388054261299, -1.280585065398877731, -1.486383542710856043 ) ) ;
#124730 = CARTESIAN_POINT ( 'NONE',  ( 7.914208982075123799, 10.25632978388623684, -1.599625672291262513 ) ) ;
#124731 = CARTESIAN_POINT ( 'NONE',  ( -8.072398248062487625, -5.212532583863426439, 7.453913518772579572 ) ) ;
#124732 = CARTESIAN_POINT ( 'NONE',  ( 10.50000000000000355, 13.50718427492792983, 3.599999999999998312 ) ) ;
#124733 = CARTESIAN_POINT ( 'NONE',  ( -5.739179097286464248, 5.590130456455973729, -0.7998128361456221525 ) ) ;
#124734 = CARTESIAN_POINT ( 'NONE',  ( -2.011244508837060518, -3.223140536948614282E-15, 0.2971265334020881110 ) ) ;
#124735 = ORIENTED_EDGE ( 'NONE', *, *, #185954, .F. ) ;
#124736 = CARTESIAN_POINT ( 'NONE',  ( 2.559107912120599071, 1.664280205102614429, -1.231313097332722872 ) ) ;
#124737 = CARTESIAN_POINT ( 'NONE',  ( -0.7500000000000215383, 3.191666666666689967, 1.299038105676671107 ) ) ;
#124738 = CARTESIAN_POINT ( 'NONE',  ( 5.473741331615251227, 7.409117525016355010, -1.599625672291262513 ) ) ;
#124739 = CARTESIAN_POINT ( 'NONE',  ( 3.203469434578891661, 6.959407783642502565, -0.7998128361456362523 ) ) ;
#124740 = CARTESIAN_POINT ( 'NONE',  ( 6.498696114369957755, -2.079444522786470184, -0.4142970760486197612 ) ) ;
#124741 = CARTESIAN_POINT ( 'NONE',  ( 3.834746474454188013E-15, 10.34375000068279782, 1.500000000000001554 ) ) ;
#124742 = CARTESIAN_POINT ( 'NONE',  ( -1.364683531250012516, 3.988541667008088876, -0.7879004041258300672 ) ) ;
#124744 = CARTESIAN_POINT ( 'NONE',  ( 9.571693261567965294, 10.26932301469188857, 0.7216878364870438212 ) ) ;
#124743 = DIRECTION ( 'NONE',  ( 0.9632918427306595976, 0.000000000000000000, -0.2684563758389253985 ) ) ;
#124745 = CARTESIAN_POINT ( 'NONE',  ( 5.641953822799152363, -0.04667112846407085736, -2.015725140939367499 ) ) ;
#124746 = CARTESIAN_POINT ( 'NONE',  ( 5.102711585370895975, 1.772601733252886280, 0.7270577078305997532 ) ) ;
#124747 = CARTESIAN_POINT ( 'NONE',  ( 6.539320575229236709, 1.252639605590207150, 2.218328189723097754 ) ) ;
#124748 = CARTESIAN_POINT ( 'NONE',  ( 3.087623348389135547, -0.8860277256741244667, 2.004638750299721828 ) ) ;
#124749 = CARTESIAN_POINT ( 'NONE',  ( -0.7500000000000179856, 10.57291666734946212, 1.299038105676658228 ) ) ;
#124750 = CARTESIAN_POINT ( 'NONE',  ( -1.500000000000013101, 1.702083334016151417, 0.8660254037844403729 ) ) ;
#124751 = CARTESIAN_POINT ( 'NONE',  ( 5.906499476128409754, -2.003886227978883383, -0.1931989457738275962 ) ) ;
#124752 = CARTESIAN_POINT ( 'NONE',  ( 2.267699027020404490, 0.5063876334258295975, -1.844086191983687284 ) ) ;
#124753 = CARTESIAN_POINT ( 'NONE',  ( -5.880485940025243607, 7.883652901494672349, 1.599625672291269396 ) ) ;
#124755 = CARTESIAN_POINT ( 'NONE',  ( 6.538674910786447469, -1.636584463124007627, 1.342808005693174156 ) ) ;
#124754 = CARTESIAN_POINT ( 'NONE',  ( -4.121315508874276112, 4.870918184183829602, -1.082531754730549967 ) ) ;
#124756 = CARTESIAN_POINT ( 'NONE',  ( 1.364683531249997417, 9.796875000341396245, 2.602085213965210642E-15 ) ) ;
#124758 = CARTESIAN_POINT ( 'NONE',  ( -6.143779885648060102, 7.196773283791382703, 1.199719254218452047 ) ) ;
#124757 = CARTESIAN_POINT ( 'NONE',  ( 3.913685052542864362, -1.076426932671892711, -1.792217407939109552 ) ) ;
#124760 = ORIENTED_EDGE ( 'NONE', *, *, #46509, .T. ) ;
#124759 = CARTESIAN_POINT ( 'NONE',  ( 2.467434050970338077, 1.692020480068063826, -0.3335236308374764369 ) ) ;
#124761 = CARTESIAN_POINT ( 'NONE',  ( 6.363548717301088509, -1.704009271243651868, -1.262090224194649446 ) ) ;
#124762 = CARTESIAN_POINT ( 'NONE',  ( 6.419949431270806528, 7.448694743692793274, 1.199719254218462483 ) ) ;
#124763 = CARTESIAN_POINT ( 'NONE',  ( -1.204086455771568476, 13.37576698399828246, -0.6670459744446199934 ) ) ;
#124764 = CARTESIAN_POINT ( 'NONE',  ( 10.50000000000000178, 13.40000000000000036, -3.600000000000002309 ) ) ;
#124765 = CARTESIAN_POINT ( 'NONE',  ( -11.84101807917483740, 9.989784997391225829, -1.444039656437080099 ) ) ;
#124766 = CARTESIAN_POINT ( 'NONE',  ( 4.981731378017507872, 7.899438143407371271, -1.199719254218452047 ) ) ;
#124767 = CARTESIAN_POINT ( 'NONE',  ( -11.92050416151432835, 13.65205375279624356, -1.381922468431411088 ) ) ;
#124768 =( GEOMETRIC_REPRESENTATION_CONTEXT ( 3 ) GLOBAL_UNCERTAINTY_ASSIGNED_CONTEXT ( ( #2669 ) ) GLOBAL_UNIT_ASSIGNED_CONTEXT ( ( #201758, #37146, #55541 ) ) REPRESENTATION_CONTEXT ( 'NONE', 'WORKASPACE' ) );
#124769 = ORIENTED_EDGE ( 'NONE', *, *, #177718, .F. ) ;
#124770 = CARTESIAN_POINT ( 'NONE',  ( 2.455456329753392897, -1.343237331403211776, -1.215579648594692808 ) ) ;
#124771 = ORIENTED_EDGE ( 'NONE', *, *, #162539, .T. ) ;
#124772 = CARTESIAN_POINT ( 'NONE',  ( 3.891353782322113375, 4.498666486585943147, -1.199719254218446718 ) ) ;
#124773 = CARTESIAN_POINT ( 'NONE',  ( 3.953084306836263995, 6.769626237021087789, 1.199719254218452047 ) ) ;
#124774 = CARTESIAN_POINT ( 'NONE',  ( 3.545387212860445114, -1.672524232984048620, 0.6962571228125400413 ) ) ;
#124775 = CARTESIAN_POINT ( 'NONE',  ( 0.5151611981367327786, 3.543326390565461281, -0.3998388334338426331 ) ) ;
#124776 = CARTESIAN_POINT ( 'NONE',  ( -10.96287206819832605, -7.723179855899500623, 0.5577339983718334615 ) ) ;
#124777 = CARTESIAN_POINT ( 'NONE',  ( 5.530423754462008290, 6.204488192500752675, 0.9375459734879583173 ) ) ;
#124779 = CARTESIAN_POINT ( 'NONE',  ( -1.364683531250010295, 14.13020833367473372, 0.7879004041258445001 ) ) ;
#124778 = CARTESIAN_POINT ( 'NONE',  ( 3.824516763807362274, -1.251359258362509497, 1.377693585838150936 ) ) ;
#124780 = CARTESIAN_POINT ( 'NONE',  ( 2.003404541029256691, -1.857510701737439929, 0.4675905980212178292 ) ) ;
#124781 = CARTESIAN_POINT ( 'NONE',  ( 0.6041866639863550104, -0.6101368697832668664, -1.720745249832649870 ) ) ;
#124782 = CARTESIAN_POINT ( 'NONE',  ( 4.811213433158714636, 8.116601557201025940, 0.8487219550047861993 ) ) ;
#124783 = CYLINDRICAL_SURFACE ( 'NONE', #95427, 1.224999999999996980 ) ;
#124784 = CARTESIAN_POINT ( 'NONE',  ( 4.954704567260191261, 7.963257648925383236, 1.029694947009308859 ) ) ;
#124785 = CARTESIAN_POINT ( 'NONE',  ( 5.129297441109695654, 7.908270138404875027, 1.225875489271853302 ) ) ;
#124786 = LINE ( 'NONE', #191808, #88081 ) ;
#124787 = CARTESIAN_POINT ( 'NONE',  ( -4.128963376203445890, 3.977025402421431544, 0.4311926875460708186 ) ) ;
#124788 = CARTESIAN_POINT ( 'NONE',  ( 5.978782553946477840, 9.919070713005490703, 1.040834085586084257E-14 ) ) ;
#124789 = CARTESIAN_POINT ( 'NONE',  ( 6.069198383140281372, 1.735254367832469891, 0.9315073086425088578 ) ) ;
#124790 = CARTESIAN_POINT ( 'NONE',  ( -3.684065054611367351, 5.321161868511784299, -1.599625672291256295 ) ) ;
#124791 = CARTESIAN_POINT ( 'NONE',  ( -11.86145017031081217, 10.09418046486151077, -1.100000000000000533 ) ) ;
#124792 = CARTESIAN_POINT ( 'NONE',  ( 0.4102503234837206469, 1.440240287209685111, -1.515647972008065780 ) ) ;
#124793 = CARTESIAN_POINT ( 'NONE',  ( 0.1471128783409255958, -1.407412912164500263, -1.162481699956314785 ) ) ;
#124794 = CARTESIAN_POINT ( 'NONE',  ( -6.124532705071231931, 8.168374127381657246, -1.599625672291263179 ) ) ;
#124795 = CARTESIAN_POINT ( 'NONE',  ( 1.395219695971817941, 1.379742824092672349, 1.195523663710513995 ) ) ;
#124796 = CARTESIAN_POINT ( 'NONE',  ( 1.911028901235469535, 1.633884665098099598, -1.483674895440662667 ) ) ;
#124797 = CARTESIAN_POINT ( 'NONE',  ( 1.499999999999996891, 10.39583333333333037, -0.8660254037844378194 ) ) ;
#124798 = CARTESIAN_POINT ( 'NONE',  ( 1.230557176020010912, 1.282188879665364656, -1.419081615486268433 ) ) ;
#124799 =( BOUNDED_SURFACE ( )  B_SPLINE_SURFACE ( 3, 3, ( 
 ( #77905, #28094, #179690, #113686, #95257, #208954, #126747, #162377, #161307, #80038, #144026, #176484, #128878, #94190, #192706, #212156, #146142, #96322, #44362, #160230, #196991, #114743, #210021, #31307, #60589, #11828, #16083, #213223, #97384, #164498, #63791, #64853, #61664, #78969, #145089, #129949, #15021, #211093, #32368, #195937, #62716, #127832, #81111, #131000, #48627, #112614, #180741, #98432, #45432, #178626, #82166, #111547, #110485, #177556, #194859, #30237, #29166, #46492, #151461, #150394, #119014, #167696, #184993, #100561, #19297, #136281, #166632, #51828, #3033, #49678, #17154, #52878, #117946, #183939, #101630, #85379, #181791, #69103, #199097, #182871, #36618, #202301, #21417, #200175, #20365, #84309, #116870, #53953, #201237, #86451, #35551, #133099, #135225, #37702, #102704, #149313, #168761, #148260, #99503, #33426, #152516, #165560, #1963, #68026, #4100, #134165, #50743, #70170, #34487, #120091, #186066, #893, #65892, #83229, #214260, #66960, #18225, #103779, #169830, #132038, #115803, #198049, #153591, #173051, #206589, #137353, #204436, #8389, #41996, #190335, #59277, #39842, #205518, #55022, #105949, #73384, #7308, #171973, #124377, #174132, #72310, #108103, #88599, #57151, #155724, #87526, #139490, #23564, #154656, #89673, #207658, #6239, #138416, #123317, #189280, #121172, #56089, #58218, #122246, #40919, #107025, #125434, #104851, #188205, #25705, #203369, #170896, #187140, #24632, #38769, #90739, #191398, #74471, #156802, #140578, #22488, #43063, #5162, #109176, #91813, #157872, #9465, #75536, #141647, #175189, #71237, #112371, #163197, #28924, #77663, #78722, #95009, #26775, #161056, #111307, #27851, #193550, #146961, #93948, #143784, #45193, #177309, #60342, #159988, #211916, #61418, #144849, #12651, #64617, #44119, #127582, #179446, #142705, #110240, #126502, #210855, #208715, #62481, #130756, #162131, #128645, #194609, #192467, #212976, #92878, #196750, #176249, #29992, #46253, #178382, #96078, #13719, #209779, #79793, #14780, #145906, #63552, #129708, #195690, #47326, #80872, #113440, #31067, #97144, #11590, #48391, #114505, #158923, #10520, #76594, #199926, #214022, #51571, #16902, #635, #68848, #20105, #53692, #17966, #52623, #116620, #149057, #86192, #19041, #118751, #84053, #165308, #167447, #69909, #183688, #181550, #35294, #180501, #131794, #65645, #184734, #197800, #182613, #34235, #117696, #100308, #82983, #85119, #66699, #2777, #133919, #33179, #98202, #49434, #32118, #115554, #132846, #198850, #50497, #166375, #81926, #101369, #164252, #151206, #134967, #15839, #150141, #200976, #36361, #102437, #152262, #1713, #67767, #148012, #168506, #3836, #136019, #202032, #99260, #209246, #104590, #77136, #120907, #23302, #139221, #153324, #205251, #170634, #154397, #11056, #176777, #210327, #171703, #60890, #55823, #88333, #28393, #172794, #127050, #89412, #22220, #106766, #12131, #123068, #186879, #189022, #119824, #70977, #4899, #193010, #137087, #121979, #187944, #56894, #39573, #5976, #27316, #72047, #159457, #73121, #38512, #37437, #203115, #185804, #54758, #138159, #204167, #105676, #155461, #21156, #40664, #103514, #93420, #143257, #169573, #7045, #44664, #110777, #94488, #160526, #78203, #144328, #87260, #80340, #47874, #196232, #146440, #98731, #148550, #46802, #16381, #63021 ),
 ( #212453, #95559, #129189, #32653, #96621, #113986, #179982, #99791, #79277, #162675, #116, #177856, #145394, #161610, #31603, #29468, #64098, #165858, #197277, #14245, #130239, #13200, #182083, #128121, #33714, #211392, #65132, #97679, #163737, #15318, #81406, #112915, #147489, #198333, #213511, #178926, #131290, #48917, #115038, #49973, #181037, #164789, #82460, #195167, #30541, #66182, #132328, #116092, #17443, #83526, #149609, #61965, #194081, #45734, #111852, #36908, #1191, #88891, #4383, #3323, #186356, #20646, #37992, #51042, #135500, #102990, #199396, #55310, #104064, #35843, #87808, #117165, #170110, #137640, #19593, #84602, #101922, #136570, #22774, #67255, #133390, #183169, #34773, #54243, #86735, #203659, #171184, #169048, #153881, #21697, #39058, #120381, #152804, #5450, #70455, #201523, #202591, #105144, #71529, #85666, #53171, #121459, #68328, #151752, #100845, #119299, #187429, #166931, #18524, #69393, #150690, #118236, #2252, #167988, #134459, #185285, #200463, #52110, #184221, #27056, #207941, #124661, #57440, #156012, #123601, #40130, #28137, #44405, #23853, #188498, #125722, #59562, #41211, #154945, #72607, #108390, #107318, #174414, #89961, #122537, #74759, #106240, #138707, #158153, #92099, #42276, #204723, #172266, #142996, #60630, #7599, #191682, #6529, #73684, #176525, #93163, #43343, #110525, #9746, #159200, #139782, #173342, #24922, #75820, #109463, #91027, #192748, #25991, #8677, #205809, #141928, #175470, #10801, #58506, #76875, #208994, #189566, #126793, #56374, #157088, #140861, #206875, #190618, #49714, #31350, #32405, #29210, #112657, #46536, #163478, #64892, #178666, #132077, #113727, #162418, #193823, #97425, #15060, #98471, #212196, #48665, #195980, #12930, #63834, #115843, #145127, #181829, #210065, #96364, #129992, #94232, #160270, #81152, #13995, #131039, #179731, #197028, #144070, #80080, #47613, #77949, #148299, #114782, #128917, #180779, #61705, #164536, #16122, #30278, #177598, #194898, #147237, #11872, #127873, #45472, #111588, #95300, #213265, #82205, #214296, #161349, #65929, #198087, #79011, #211133, #62757, #146181, #70203, #52912, #167733, #102740, #71272, #103811, #117983, #19334, #169860, #100596, #183975, #66998, #85413, #135258, #99538, #21449, #35586, #136316, #150433, #137386, #200209, #202335, #51861, #201272, #119045, #101665, #120125, #86483, #3066, #1998, #34524, #68063, #133136, #121206, #203401, #116908, #199135, #4135, #152548, #134199, #33462, #165600, #185029, #151497, #36654, #182908, #931, #69136, #50780, #17190, #168795, #20402, #53986, #83265, #166672, #87557, #153625, #18262, #186103, #37735, #84345, #5197, #55055, #149352, #188238, #190368, #187175, #138449, #72345, #191432, #204469, #189316, #40954, #124410, #107062, #172009, #25739, #155759, #9500, #140612, #39878, #104884, #56122, #38803, #6274, #73423, #23601, #139524, #89708, #88633, #58254, #170927, #42028, #91849, #22524, #7344, #108139, #141681, #75572, #158957, #205550, #90774, #154691, #57189, #173087, #24667, #123349, #207694, #59314, #156835, #125471, #105989, #8422, #74507, #122280, #206624, #174166, #157906, #43099, #92911, #109213, #175224, #26809, #10552, #76626, #142741, #208748, #60375, #178414, #46286, #164284, #143816, #161089, #64646, #27883, #209813, #160022, #30023, #93980, #128675 ),
 ( #14811, #15872, #31102, #63583, #163229, #145936, #112403, #195723, #81957, #196780, #210885, #96109, #48422, #193580, #62510, #11621, #162164, #13752, #192500, #114535, #194644, #80902, #28955, #148042, #78755, #146993, #144879, #79826, #211948, #129740, #213010, #179479, #47359, #95040, #130786, #113473, #97175, #180529, #214050, #32151, #98229, #126538, #44151, #45223, #110272, #77695, #176281, #61448, #127615, #111338, #177343, #12679, #182647, #103547, #18000, #168542, #84090, #19076, #151240, #150177, #152297, #118786, #35327, #34268, #66736, #100341, #165339, #153362, #169608, #149089, #99292, #36398, #184772, #166406, #65678, #197834, #85157, #1745, #2809, #669, #33208, #199959, #16933, #49467, #68880, #135000, #167480, #115585, #83015, #53728, #185838, #132879, #102476, #131825, #198881, #87293, #3870, #20139, #21190, #201011, #69943, #50527, #67802, #133951, #52657, #86225, #51605, #181579, #136055, #117730, #116650, #202068, #119860, #37470, #183719, #101407, #106798, #138194, #123101, #26549, #55858, #92657, #120943, #7080, #40695, #4933, #71009, #8169, #73153, #190116, #24398, #41770, #54795, #139259, #172826, #203151, #59053, #107883, #39608, #91591, #186915, #173910, #141428, #23336, #88368, #105711, #140347, #137122, #38546, #104623, #170671, #22258, #57992, #90510, #207434, #174967, #156575, #157643, #25485, #42840, #124155, #74253, #72083, #122014, #89446, #155497, #154434, #204204, #9240, #171739, #56928, #205290, #108947, #6014, #189058, #75312, #187982, #206366, #125211, #191173, #60122, #160833, #196532, #79574, #44969, #94784, #43901, #64396, #10297, #130540, #126281, #161912, #111077, #62262, #12424, #28698, #209550, #29772, #80651, #78504, #61194, #210636, #177082, #95856, #146742, #144622, #128423, #13502, #192239, #27620, #63327, #194390, #46032, #112154, #178157, #110015, #145693, #127353, #193322, #47102, #212761, #31908, #211692, #30847, #129488, #195470, #48174, #113217, #96925, #179222, #143556, #162975, #114287, #14554, #159760, #180284, #158699, #176028, #93721, #76371, #11359, #142478, #208486, #77439, #100090, #82767, #150988, #66485, #134750, #51347, #99036, #15619, #197579, #164044, #131578, #198631, #148841, #50279, #413, #213807, #183463, #81709, #35069, #2553, #147790, #132625, #18814, #52408, #200759, #69696, #116398, #1487, #65428, #182386, #83826, #17737, #34016, #118535, #184518, #166151, #36139, #165092, #67552, #149919, #97985, #133696, #199701, #16683, #117471, #3617, #101140, #102222, #167228, #84901, #68628, #49223, #168292, #19888, #85973, #152048, #135799, #201823, #53468, #119605, #185590, #115342, #181334, #32961, #155247, #24151, #123901, #7904, #71827, #189870, #20940, #206111, #173656, #55605, #120686, #137937, #172569, #58807, #37219, #124961, #87035, #103293, #90254, #56679, #25230, #207183, #205034, #41512, #140086, #75060, #156321, #188806, #73993, #122844, #171488, #106543, #141172, #107625, #121760, #23079, #91333, #104366, #187727, #70756, #89195, #139011, #169354, #157391, #39356, #57743, #154181, #153108, #203958, #8985, #105452, #40442, #4682, #6828, #136869, #202894, #72907, #5749, #38289, #54539, #186662, #170411, #22000, #88111, #10048, #161659, #29517, #77181, #190923, #108692, #144377, #143303, #210376, #126022, #158447, #110822, #76123, #174720, #194134 ),
 ( #129242, #95610, #146488, #128172, #195215, #191984, #209294, #60942, #45784, #13254, #127098, #14297, #62017, #44715, #142226, #111901, #177904, #46851, #94534, #145442, #193062, #79327, #178977, #176829, #160573, #211442, #92408, #59871, #63074, #12181, #78253, #112965, #30591, #208239, #96676, #27368, #11105, #162726, #80392, #64149, #28442, #212508, #42587, #159507, #26293, #43650, #109766, #175774, #93468, #120155, #22558, #136345, #131336, #202367, #130291, #81461, #15368, #137413, #147539, #132381, #198382, #70233, #50023, #115089, #186131, #98785, #169887, #83579, #197330, #47927, #213560, #196280, #163789, #16432, #181085, #82510, #32703, #31655, #4163, #114040, #54016, #37766, #180033, #164840, #103838, #87585, #21476, #104917, #148597, #33765, #97731, #166, #116147, #182135, #66233, #153657, #5226, #99843, #71300, #48972, #165908, #17492, #65182, #152576, #203432, #55086, #121235, #38834, #187205, #170958, #88663, #154723, #6306, #139556, #74540, #10583, #175253, #176311, #110303, #89742, #107096, #76657, #188270, #155791, #106020, #124441, #39911, #140640, #27915, #207723, #173119, #8452, #172041, #192529, #138479, #44183, #23634, #75602, #24700, #190399, #206653, #156866, #123380, #157936, #208778, #58285, #189345, #42057, #9529, #108170, #57220, #125501, #40985, #109245, #25769, #73454, #204501, #7375, #56151, #205583, #90802, #174196, #91881, #141713, #59347, #191464, #122313, #43129, #26839, #92942, #158987, #142772, #60408, #126569, #94011, #160050, #72380, #193609, #30053, #211975, #145965, #96143, #48453, #98256, #210914, #180558, #12709, #129770, #79856, #11654, #63615, #162194, #78785, #178445, #131855, #144907, #62541, #13781, #195753, #45251, #128703, #47390, #164313, #114566, #115615, #49494, #28987, #46316, #15904, #127645, #95073, #111369, #113503, #177373, #179511, #181610, #147021, #112432, #31131, #161122, #197862, #77727, #33239, #194672, #14840, #97206, #163258, #80930, #213044, #64673, #130819, #148074, #196810, #32180, #81986, #214080, #65707, #99322, #143849, #209841, #61480, #66767, #34300, #69976, #135032, #201045, #118817, #184804, #198913, #36433, #1780, #199991, #53764, #4967, #38581, #2843, #37507, #101438, #133983, #71045, #3906, #103583, #68912, #150208, #152328, #54831, #168571, #166443, #20171, #165372, #116680, #50559, #169641, #182679, #167512, #19109, #136087, #51639, #16965, #83046, #102509, #117763, #86258, #100373, #132908, #85187, #18035, #149121, #202104, #119897, #52688, #703, #84122, #153396, #137161, #67837, #185871, #183753, #35363, #186949, #21224, #87329, #120981, #203185, #151270, #122050, #73190, #7117, #140380, #41807, #139296, #125248, #8201, #56962, #72120, #206400, #58025, #9275, #106834, #173945, #24436, #39642, #172865, #108980, #171777, #174999, #154471, #123137, #90547, #104657, #170705, #124189, #189095, #25518, #74286, #91626, #6049, #157677, #156611, #190152, #75346, #141462, #205325, #207469, #138228, #59088, #191208, #40728, #188014, #107920, #42872, #22290, #88403, #204241, #105750, #55893, #23373, #89483, #155538, #39273, #37130, #21916, #186583, #121680, #202813, #20858, #120605, #103210, #3539, #153025, #187645, #154096, #168207, #69611, #5666, #150907, #19806, #117387, #135718, #185507, #149837, #71745, #85890, #38211, #200676, #105367, #36058 ),
 ( #183383, #171404, #83743, #167148, #34989, #54462, #2468, #201743, #1406, #134673, #67467, #199617, #151967, #119519, #133613, #51262, #86958, #53384, #104284, #169272, #170330, #101059, #88025, #4600, #70674, #137860, #203881, #118454, #55525, #18735, #84818, #68544, #102139, #52325, #184441, #136784, #44628, #22995, #110745, #72826, #89112, #76043, #42501, #159422, #192976, #190841, #175689, #125948, #60854, #142145, #174636, #59789, #108609, #157308, #92331, #127017, #93386, #107543, #8898, #11022, #90180, #173577, #56598, #74979, #124876, #155166, #77097, #25146, #191904, #140006, #6750, #189783, #43566, #41434, #26213, #158373, #91248, #109686, #208159, #207097, #206028, #24075, #57664, #122761, #138929, #204947, #106462, #188721, #27279, #143224, #123822, #40359, #172487, #9965, #141087, #209214, #156243, #7820, #58726, #73913, #160491, #179945, #113949, #64058, #12098, #210289, #164750, #82422, #45698, #81369, #28357, #61929, #198293, #114997, #147449, #132288, #31568, #180994, #111813, #195127, #129151, #97643, #213473, #46765, #78, #196195, #30505, #128088, #163700, #15283, #32615, #80304, #131253, #130201, #49935, #47838, #98693, #65096, #66143, #197240, #48879, #16341, #148511, #96586, #176743, #94452, #78166, #112876, #162635, #144296, #29434, #178890, #194046, #14209, #177818, #95525, #161575, #146402, #13162, #79239, #145358, #212416, #211358, #62983, #25919, #187358, #38988, #40060, #72534, #158084, #157018, #190548, #7528, #88817, #90953, #207867, #107250, #105073, #173271, #103994, #55238, #203586, #108321, #121385, #106170, #172196, #41140, #23785, #154874, #8604, #138632, #140788, #57368, #171112, #21624, #22704, #170038, #137569, #204655, #6457, #56304, #122466, #5377, #189496, #87732, #24851, #74687, #153806, #188425, #206802, #58435, #124588, #75749, #89891, #73611, #71456, #155942, #139710, #205734, #123531, #42204, #174341, #92027, #9672, #141859, #59491, #125648, #191610, #111515, #127797, #44330, #209989, #163409, #110452, #94158, #61631, #193752, #76801, #176453, #45399, #195904, #146109, #147166, #81079, #60557, #77875, #47540, #159130, #126716, #142922, #95221, #10731, #177521, #213193, #178592, #143997, #29133, #208922, #14985, #109392, #64820, #161271, #12857, #160197, #128841, #179657, #78932, #11800, #145054, #211057, #194822, #31277, #62682, #46458, #112580, #192676, #28065, #162341, #30201, #96289, #13924, #80004, #212120, #63758, #129918, #113653, #97352, #130966, #43272, #175397, #26982, #93089, #165528, #36585, #35519, #69070, #100528, #181757, #183908, #86418, #200143, #198017, #51797, #196958, #148227, #82135, #201206, #214229, #199066, #50712, #134136, #116838, #33391, #101596, #17120, #19265, #150364, #49645, #114714, #65857, #48596, #16051, #83197, #99469, #149279, #860, #98400, #67994, #180709, #117915, #167664, #32332, #66926, #85347, #151428, #3001, #168730, #133068, #166603, #164465, #182839, #34456, #18192, #84277, #135190, #52845, #1934, #118980, #115768, #184959, #102672, #132007, #20332, #152485, #4067, #70137, #41957, #203336, #187104, #154626, #72275, #169795, #54989, #138384, #74440, #24599, #25670, #174097, #153558, #170866, #140542, #37668, #5129, #21384, #188174, #103744, #204402, #91777, #57119, #22456, #56055, #87493, #108069, #202269, #157834, #71204, #139453 ),
 ( #90708, #9431, #40888, #73350, #173018, #155690, #122212, #205485, #136249, #206556, #6206, #39808, #58184, #121141, #105914, #137320, #171939, #23530, #53920, #124342, #89638, #156770, #38738, #120057, #88568, #8356, #7273, #104820, #123286, #186032, #189249, #106993, #190300, #192429, #76557, #44084, #175154, #163160, #179413, #158887, #109141, #46221, #128608, #176213, #75501, #207621, #28890, #27815, #94974, #10483, #43029, #209744, #26740, #59238, #78688, #12615, #177274, #125397, #92843, #63521, #195658, #142667, #194575, #141612, #208678, #97108, #13686, #112338, #31034, #144813, #79756, #60307, #93912, #159953, #210820, #178350, #11557, #113407, #161020, #143749, #126466, #62445, #29958, #145872, #193516, #96044, #162097, #110203, #45157, #191362, #77627, #61386, #127545, #111271, #211880, #129673, #47292, #17927, #16867, #199886, #34195, #51531, #64581, #117656, #132809, #1674, #101329, #183649, #49399, #167410, #212944, #35253, #151167, #33142, #98169, #115518, #150102, #36321, #14745, #146927, #182573, #181513, #100270, #164217, #196713, #149021, #48354, #130722, #84011, #166335, #116578, #114465, #180465, #2738, #134931, #15804, #133879, #80837, #32081, #102399, #19002, #85083, #184700, #67728, #68809, #81890, #99222, #165272, #200936, #52584, #82947, #118712, #147976, #596, #213986, #65606, #131756, #197761, #198813, #66662, #50459, #87220, #72008, #190049, #4860, #41701, #69870, #170595, #204130, #168467, #20065, #171665, #22181, #139184, #187906, #205214, #3796, #56856, #138121, #155422, #40625, #123030, #203075, #106728, #152225, #188981, #90438, #186842, #37397, #54719, #89373, #86154, #135979, #201994, #53652, #119784, #7006, #39536, #156506, #124086, #121940, #172755, #24330, #206296, #73083, #105637, #8095, #23261, #88297, #74184, #57921, #140277, #38474, #154358, #185765, #21114, #104551, #103472, #5937, #55783, #169534, #153284, #70939, #137049, #120868, #148516, #62986, #213477, #129155, #29438, #125148, #82, #130206, #163705, #80307, #13165, #108880, #79243, #207371, #198298, #66147, #191105, #141357, #81372, #15287, #211361, #107811, #196199, #147455, #157577, #145362, #31571, #65101, #131257, #82426, #195131, #14212, #75245, #46768, #96589, #30508, #112882, #197244, #48883, #95529, #115002, #177821, #146407, #178894, #173836, #162638, #212420, #161578, #64061, #16345, #47841, #113952, #179948, #97646, #58991, #181000, #32620, #98697, #164756, #132292, #25413, #42773, #91518, #9170, #165824, #67221, #83492, #101888, #17408, #52074, #87769, #185250, #150654, #200428, #149574, #170076, #116060, #21663, #1158, #53134, #2217, #167953, #118201, #134425, #100811, #135466, #186322, #184189, #166896, #19557, #68292, #201488, #37957, #35811, #85633, #119265, #133356, #199363, #169015, #151719, #3290, #69358, #36874, #51009, #102956, #18488, #84566, #152770, #117130, #104030, #183132, #34738, #20613, #86701, #153845, #4351, #136537, #70419, #202556, #54208, #5416, #120346, #71495, #137606, #49939, #182050, #33680, #99755, #154911, #205773, #57401, #140826, #123566, #188462, #42241, #172232, #25956, #157053, #204690, #121422, #88856, #55273, #22738, #89925, #40093, #155976, #106206, #105107, #74721, #187392, #173306, #23820, #56340, #7563, #6495, #76839, #93126, #72570, #138670, #174376, #108354, #73649 ),
 ( #206838, #90990, #39024, #122501, #191643, #109427, #139748, #92061, #171147, #189529, #10764, #141893, #158119, #159165, #58471, #207904, #41177, #107284, #24885, #124626, #9710, #8642, #27018, #190584, #75786, #59525, #125685, #43308, #175433, #203622, #97388, #30241, #61667, #46495, #164502, #193787, #16086, #44366, #145092, #178629, #142958, #208960, #146145, #211096, #113691, #162380, #179694, #192711, #31310, #112619, #129953, #15024, #163444, #177559, #81115, #126751, #147201, #64858, #161310, #11833, #29171, #63795, #60593, #110489, #176488, #28099, #94194, #195941, #13958, #131003, #98437, #96325, #213226, #196995, #180745, #47577, #80042, #48630, #212160, #62720, #114747, #32372, #160234, #12893, #128881, #77911, #210026, #78972, #144030, #194862, #127835, #45436, #111550, #95261, #184998, #199101, #120094, #34490, #36623, #100565, #896, #99506, #186071, #101634, #135228, #166637, #66964, #165563, #37706, #167700, #201241, #51831, #50746, #83232, #116875, #181796, #169833, #103782, #17158, #115808, #52882, #119017, #182874, #82170, #214263, #35554, #18229, #19302, #149317, #49681, #1966, #33429, #65896, #85382, #151466, #183944, #132042, #133103, #70173, #202305, #84313, #102707, #148264, #150398, #198052, #20370, #168765, #68030, #3037, #86455, #134170, #200178, #117949, #69106, #152519, #4104, #136285, #53956, #89678, #121175, #24636, #90745, #25709, #139494, #190338, #123321, #154659, #205522, #43067, #72314, #109180, #137357, #23570, #57156, #21420, #87529, #156806, #155728, #206593, #40926, #58222, #71241, #124380, #189284, #8393, #108108, #42000, #56093, #174135, #5167, #91817, #157875, #39847, #104854, #122249, #74475, #153596, #203374, #55026, #187144, #38773, #140582, #107030, #9468, #191401, #173056, #75540, #141650, #59280, #207661, #125440, #170899, #22491, #7312, #88603, #6245, #138419, #105954, #73391, #204439, #188208, #171978, #208719, #161061, #62484, #26778, #31071, #177313, #63555, #77667, #212980, #127586, #129711, #144852, #210858, #128648, #194613, #60345, #46256, #11593, #209782, #195694, #126506, #97147, #44122, #110244, #111310, #143787, #14783, #13723, #47330, #78725, #159992, #162135, #64620, #178385, #176253, #29996, #175192, #192470, #27854, #179450, #93951, #28927, #95012, #112374, #12654, #61421, #79796, #193554, #211920, #96081, #45196, #92882, #145909, #158927, #113444, #163200, #80875, #146965, #130759, #76597, #196755, #10523, #48395, #142710, #164255, #16906, #35297, #68851, #2780, #86195, #66702, #17970, #81929, #132849, #100311, #34239, #198853, #151209, #200979, #99263, #134971, #115557, #84057, #182616, #114508, #166378, #50501, #181554, #116623, #20108, #33182, #165311, #150144, #1716, #148015, #82986, #67771, #52626, #118754, #3839, #152266, #131797, #149061, #184738, #15843, #197803, #214026, #133922, #65650, #199929, #69912, #101374, #638, #51575, #49438, #136022, #180504, #202035, #117700, #183691, #167449, #19044, #85123, #36366, #102441, #168509, #32122, #98205, #104593, #105679, #5980, #139224, #41742, #72051, #171707, #56897, #169576, #137091, #172798, #87263, #154401, #38515, #138162, #170638, #21159, #205255, #119828, #123072, #24369, #103517, #22223, #189026, #8138, #156546, #25453, #204170, #23305, #153328, #55826, #39576, #187948, #121982, #90481, #140318, #88337 ) ),
 .UNSPECIFIED., .T., .F., .F. ) 
 B_SPLINE_SURFACE_WITH_KNOTS ( ( 4, 3, 4 ),
 ( 4, 1, 1, 1, 1, 1, 1, 1, 1, 1, 1, 1, 1, 1, 1, 1, 1, 1, 1, 1, 1, 1, 1, 1, 1, 1, 1, 1, 1, 1, 1, 1, 1, 1, 1, 1, 1, 1, 1, 1, 1, 1, 1, 1, 1, 1, 1, 1, 1, 1, 1, 1, 1, 1, 1, 1, 1, 1, 1, 1, 1, 1, 1, 1, 1, 1, 1, 1, 1, 1, 1, 1, 1, 1, 1, 1, 1, 1, 1, 1, 1, 1, 1, 1, 1, 1, 1, 1, 1, 1, 1, 1, 1, 1, 1, 1, 1, 1, 1, 1, 1, 1, 1, 1, 1, 1, 1, 1, 1, 1, 1, 1, 1, 1, 1, 1, 1, 1, 1, 1, 1, 1, 1, 1, 1, 1, 1, 1, 1, 1, 1, 1, 1, 1, 1, 1, 1, 1, 1, 1, 1, 1, 1, 1, 1, 1, 1, 1, 1, 1, 1, 1, 1, 1, 1, 1, 1, 1, 1, 1, 1, 1, 1, 1, 1, 1, 1, 1, 1, 1, 1, 1, 1, 1, 1, 1, 1, 1, 1, 1, 1, 1, 1, 1, 1, 1, 1, 1, 1, 1, 1, 1, 1, 1, 1, 1, 1, 1, 1, 1, 1, 1, 1, 1, 1, 1, 1, 1, 1, 1, 1, 1, 1, 1, 1, 1, 1, 1, 1, 1, 1, 1, 1, 1, 1, 1, 1, 1, 1, 1, 1, 1, 1, 1, 1, 1, 1, 1, 1, 1, 1, 1, 1, 1, 1, 1, 1, 1, 1, 1, 1, 1, 1, 1, 1, 1, 1, 1, 1, 1, 1, 1, 1, 1, 1, 1, 1, 1, 1, 1, 1, 1, 1, 1, 1, 1, 1, 1, 1, 1, 1, 1, 1, 1, 1, 1, 1, 1, 1, 1, 1, 1, 1, 1, 1, 1, 1, 1, 1, 1, 1, 1, 1, 1, 1, 1, 1, 1, 1, 1, 1, 1, 1, 1, 1, 1, 1, 1, 1, 1, 1, 1, 1, 1, 1, 1, 1, 1, 1, 1, 1, 1, 1, 1, 1, 1, 1, 1, 1, 1, 1, 1, 1, 1, 1, 1, 1, 1, 1, 1, 1, 1, 1, 1, 1, 1, 1, 1, 1, 1, 1, 1, 1, 1, 1, 1, 1, 1, 1, 1, 1, 1, 1, 1, 1, 1, 1, 1, 1, 1, 1, 1, 1, 1, 4 ),
 ( 0.000000000000000000, 0.5000000000000000000, 1.000000000000000000 ),
 ( 0.000000000000000000, 0.002599909708945224215, 0.005208776875251038344, 0.007813105021672143990, 0.01041684075506122895, 0.01302033053878596733, 0.01562516449037322508, 0.01822901888718816976, 0.02083333248856494152, 0.02343767784666880849, 0.02604151204071371642, 0.02864616705684025488, 0.03124974664057501156, 0.03385445107693609706, 0.03645811663825353210, 0.03906264587105176544, 0.04166673705245293319, 0.04427082116499847508, 0.04687535697974040683, 0.04947901875943551409, 0.05208372524935509645, 0.05468730636643894666, 0.05729195276349181160, 0.05989578571700067411, 0.06250012971910297310, 0.06510448174046053194, 0.06770830932160050442, 0.07031296016926287529, 0.07291653972921435800, 0.07552124384959360559, 0.07812490789241745281, 0.08072943556986492131, 0.08333352577934262373, 0.08593760861062926804, 0.08854214333088818167, 0.09114580385899402615, 0.09375050919907033931, 0.09635408915385039463, 0.09895873428887830281, 0.1015625661591952889, 0.1041669088510773916, 0.1067712598504420435, 0.1093750861808121810, 0.1119797359579501050, 0.1145833143474069837, 0.1171880172914337714, 0.1197916802446672702, 0.1223962066585842084, 0.1250002958591681090, 0.1276043774339237491, 0.1302089111537957367, 0.1328125705047451810, 0.1354172747579587832, 0.1380208536162275679, 0.1406254975582941213, 0.1432293284131295197, 0.1458336698625422867, 0.1484380199076493767, 0.1510418450546419100, 0.1536464938294531402, 0.1562500711155297428, 0.1588547729514310503, 0.1614584348822658832, 0.1640629601007041471, 0.1666670483599762276, 0.1692711287458052438, 0.1718756615333107141, 0.1744793197742946778, 0.1770840230088624179, 0.1796876008377196188, 0.1822922436549848091, 0.1848960735616705098, 0.1875004138364584350, 0.1901047629951247708, 0.1927085870260826783, 0.1953132348667029061, 0.1979168111164897881, 0.2005215119124719170, 0.2031251728880697216, 0.2057296969790492203, 0.2083337843645647058, 0.2109378636290424602, 0.2135423955521746908, 0.2161460527503557827, 0.2187507550344668650, 0.2213543319009846355, 0.2239589736615800464, 0.2265628026874214052, 0.2291671418554001027, 0.2317714901954165685, 0.2343753131776551424, 0.2369799601521939414, 0.2395835354327550959, 0.2421882352569974250, 0.2447918953444941648, 0.2473964183760076208, 0.2500005049552969649, 0.2526045831659717300, 0.2552091142926994904, 0.2578127705152143956, 0.2604174719170327390, 0.2630210478882585856, 0.2656256886602897938, 0.2682295168725681855, 0.2708338550015275126, 0.2734382025906618163, 0.2760420245914711468, 0.2786466707680146371, 0.2812502451463897990, 0.2838549440670474211, 0.2864586033335557724, 0.2890631253735708728, 0.2916672112141422968, 0.2942712884385379479, 0.2968758188368077477, 0.2994794741507696423, 0.3020841747384366283, 0.3046877498813952978, 0.3072923897329448151, 0.3098962171989202430, 0.3125005543566263810, 0.3151049012626256918, 0.3177087223492732204, 0.3203133677958864278, 0.3229169413390938770, 0.3255216394243000688, 0.3281252979369121969, 0.3307298190533745630, 0.3333339042227165261, 0.3359379805283350118, 0.3385425102660742369, 0.3411461647385755636, 0.3437508645802123675, 0.3463544389619092612, 0.3489590779610384774, 0.3515629047479519320, 0.3541672410021501904, 0.3567715872927431642, 0.3593754075324762653, 0.3619800523172059803, 0.3645836250922447341, 0.3671883224101137877, 0.3697919802359038166, 0.3723965004967392245, 0.3750005850623230885, 0.3776046605166471504, 0.3802091896617659783, 0.3828128433598806946, 0.3854175425235913388, 0.3880211162110140388, 0.3906257544257662473, 0.3932295806008425099, 0.3958339160192597128, 0.3984382617621595180, 0.4010420812222079689, 0.4036467254130849946, 0.4062502974869375283, 0.4088549941055670267, 0.4114586513115932598, 0.4140631707847102772, 0.4166672548139925825, 0.4192713294844879757, 0.4218758581048823730, 0.4244795110956688933, 0.4270842096495421902, 0.4296877827096635682, 0.4322924202080664635, 0.4348962458385162155, 0.4375005804888632555, 0.4401049257517701263, 0.4427087444993486054, 0.4453133881643903114, 0.4479169596040251111, 0.4505216555914985932, 0.4531253122448062887, 0.4557298309980991058, 0.4583339145585244578, 0.4609379885126426157, 0.4635425166761967808, 0.4661461690266998081, 0.4687508670388120247, 0.4713544395385928509, 0.4739590763886608604, 0.4765629015416836811, 0.4791672354916582388, 0.4817715803422617515, 0.4843753984445725025, 0.4869800416517858221, 0.4895836125241597725, 0.4921883079485492862, 0.4947919641161733773, 0.4973964822175238609, 0.5000005653765271507, 0.5026046386817077938, 0.5052091664562964324, 0.5078128182335502894, 0.5104175157719683664, 0.5130210877783591972, 0.5156257240480961457, 0.5182295487908826770, 0.5208338821081714975, 0.5234382266141532902, 0.5260420441383883983, 0.5286466869557716608, 0.5312502573278325979, 0.5338549522572011430, 0.5364586080061681805, 0.5390631255234488162, 0.5416672083484578293, 0.5442712810721315186, 0.5468758085256230084, 0.5494794597966533578, 0.5520841569294364648, 0.5546877285093810839, 0.5572923642667827471, 0.5598961886665174692, 0.5625005214187991376, 0.5651048656478350196, 0.5677086826611791315, 0.5703133251567252815, 0.5729168950954143247, 0.5755215895978186280, 0.5781252449951498340, 0.5807297619962258350, 0.5833338445546641937, 0.5859379167642547737, 0.5885424439645127181, 0.5911460947963396162, 0.5937507915915425372, 0.5963543628119793993, 0.5989589981250363904, 0.6015628222488997867, 0.6041671545038470592, 0.6067714985236103420, 0.6093753150932430529, 0.6119799573349418154, 0.6145835269071964202, 0.6171882210506893784, 0.6197918761634028106, 0.6223963927161352272, 0.6250004750754242222, 0.6276045468383509851, 0.6302090738532378777, 0.6328127243128783830, 0.6354174208385534595, 0.6380209917664191321, 0.6406256267031188445, 0.6432294506182901772, 0.6458337824435727015, 0.6484381263217364744, 0.6510419425148348260, 0.6536465845706755928, 0.6562501538434313275, 0.6588548476960643940, 0.6614585025911776661, 0.6640630187634258830, 0.6666671009909873602, 0.6692711723746683772, 0.6718756992720475996, 0.6744793494265174383, 0.6770840457507175669, 0.6796876164529486175, 0.6822922510812780006, 0.6848960748549377531, 0.6875004063182246217, 0.6901047501224634173, 0.6927085660062048955, 0.6953132079441787239, 0.6979167769843723779, 0.7005214706141982273, 0.7031251253587310623, 0.7057296412183544643, 0.7083337233816132672, 0.7109377944534676086, 0.7135423213012055399, 0.7161459712175226588, 0.7187506674083037339, 0.7213542379518396164, 0.7239588723397878400, 0.7265626960391206035, 0.7291670272080824633, 0.7317713710060759214, 0.7343751866476402324, 0.7369798285357428425, 0.7395833974103146469, 0.7421880908853900616, 0.7447917455463664016, 0.7473962611612280371, 0.7500003433276148934, 0.7526044141550642941, 0.7552089410210337528, 0.7578125907662203176, 0.7604172868916432293, 0.7630208573434285046, 0.7656254915589897347, 0.7682293152511859846, 0.7708336461934980344, 0.7734379900529331220, 0.7760418055195050790, 0.7786464474257392965, 0.7812500162016354777, 0.7838547095900232353, 0.7864583642344741277, 0.7890628796724428184, 0.7916669619093961163, 0.7942710325598689725, 0.7968755595119511037, 0.7994792091530360523, 0.8020839052811703507, 0.8046874757081575735, 0.8072921098193328593, 0.8098959335715922858, 0.8125002643549369408, 0.8151046083435100620, 0.8177084237022821389, 0.8203130656946604482, 0.8229166344388356702, 0.8255213278086077633, 0.8281249825035741363, 0.8307294978325265866, 0.8333335802074958165, 0.8359376507484286289, 0.8385421778545157911, 0.8411458274585372763, 0.8437505236574627254, 0.8463540941266142204, 0.8489587282014147140, 0.8515625520809478877, 0.8541668827730166669, 0.8567712269584367712, 0.8593750422766117669, 0.8619796844231587540, 0.8645832532025788941, 0.8671879466218186394, 0.8697916014343529678, 0.8723961167221769841, 0.8750001993026245151, 0.8776042698014647758, 0.8802087971294628721, 0.8828124467634709260, 0.8854171431012803906, 0.8880207136795719158, 0.8906253477860208712, 0.8932291718600525732, 0.8958335025285494302, 0.8984378469785403443, 0.9010416623233333810, 0.9036463046920883979, 0.9062498735737328781, 0.9088545671105374701, 0.9114582221077071056, 0.9140627374223044832, 0.9166668202757080053, 0.9192708907999164181, 0.9218754184177497812, 0.9244790681488107564, 0.9270837646936044285, 0.9296873354480212903, 0.9322919696541906998, 0.9348957939899811276, 0.9375001247025137596, 0.9401044694846933947, 0.9427082849236875228, 0.9453129275835465695, 0.9479164966330613229, 0.9505211903504858784, 0.9531248456066239161, 0.9557293610412391782, 0.9583334441921064206, 0.9609375147049603605, 0.9635420428945489224, 0.9661456931510739032, 0.9687503890924937799, 0.9713539588735070618, 0.9739585961357111188, 0.9765624261165479769, 0.9791667493207181217, 0.9817710620974646751, 0.9843748983037424738, 0.9869797303524157073, 0.9895832060093603388, 0.9921869237806116848, 0.9947912468131487884, 0.9974000922265050528, 0.9999999999999998890 ),
 .UNSPECIFIED. ) 
 GEOMETRIC_REPRESENTATION_ITEM ( )  RATIONAL_B_SPLINE_SURFACE ( (
 ( 1.000000000000000000, 1.000000000000000000, 1.000000000000000000, 0.9999999999999997780, 1.000000000000000000, 1.000000000000000444, 0.9999999999999996669, 0.9999999999999996669, 1.000000000000000444, 1.000000000000000000, 1.000000000000000000, 1.000000000000000000, 1.000000000000000222, 1.000000000000000222, 0.9999999999999997780, 1.000000000000000000, 1.000000000000000222, 1.000000000000000000, 1.000000000000000222, 0.9999999999999994449, 1.000000000000000222, 0.9999999999999997780, 1.000000000000000444, 1.000000000000000000, 1.000000000000000000, 1.000000000000000222, 0.9999999999999997780, 1.000000000000000222, 1.000000000000000000, 1.000000000000000222, 0.9999999999999997780, 1.000000000000000000, 1.000000000000000000, 0.9999999999999997780, 1.000000000000000000, 1.000000000000000000, 1.000000000000000222, 1.000000000000000000, 0.9999999999999997780, 1.000000000000000222, 0.9999999999999997780, 1.000000000000000000, 0.9999999999999997780, 1.000000000000000444, 0.9999999999999996669, 1.000000000000000222, 1.000000000000000000, 1.000000000000000000, 1.000000000000000444, 0.9999999999999996669, 1.000000000000000222, 1.000000000000000444, 1.000000000000000000, 0.9999999999999997780, 1.000000000000000444, 1.000000000000000222, 1.000000000000000000, 1.000000000000000000, 1.000000000000000222, 1.000000000000000000, 1.000000000000000222, 0.9999999999999997780, 1.000000000000000222, 1.000000000000000000, 1.000000000000000000, 1.000000000000000444, 0.9999999999999996669, 1.000000000000000000, 0.9999999999999997780, 1.000000000000000222, 0.9999999999999996669, 1.000000000000000000, 1.000000000000000222, 0.9999999999999997780, 1.000000000000000444, 0.9999999999999997780, 1.000000000000000000, 0.9999999999999997780, 1.000000000000000222, 0.9999999999999996669, 1.000000000000000000, 1.000000000000000222, 0.9999999999999996669, 1.000000000000000444, 0.9999999999999997780, 1.000000000000000000, 1.000000000000000222, 0.9999999999999996669, 1.000000000000000222, 1.000000000000000000, 0.9999999999999997780, 1.000000000000000222, 0.9999999999999997780, 1.000000000000000000, 1.000000000000000222, 0.9999999999999997780, 1.000000000000000000, 1.000000000000000000, 0.9999999999999997780, 1.000000000000000000, 1.000000000000000222, 0.9999999999999997780, 1.000000000000000000, 1.000000000000000000, 1.000000000000000000, 0.9999999999999997780, 1.000000000000000222, 0.9999999999999997780, 0.9999999999999997780, 1.000000000000000444, 1.000000000000000000, 1.000000000000000000, 0.9999999999999997780, 1.000000000000000222, 1.000000000000000000, 1.000000000000000000, 1.000000000000000000, 1.000000000000000000, 1.000000000000000222, 1.000000000000000222, 0.9999999999999997780, 1.000000000000000000, 0.9999999999999997780, 1.000000000000000444, 0.9999999999999996669, 1.000000000000000666, 1.000000000000000000, 0.9999999999999997780, 1.000000000000000222, 1.000000000000000000, 1.000000000000000000, 1.000000000000000000, 0.9999999999999994449, 1.000000000000000666, 0.9999999999999996669, 1.000000000000000000, 1.000000000000000222, 0.9999999999999997780, 1.000000000000000222, 0.9999999999999997780, 1.000000000000000222, 0.9999999999999996669, 1.000000000000000444, 1.000000000000000000, 1.000000000000000222, 0.9999999999999996669, 1.000000000000000000, 1.000000000000000222, 0.9999999999999997780, 1.000000000000000000, 0.9999999999999997780, 1.000000000000000000, 1.000000000000000000, 1.000000000000000222, 0.9999999999999997780, 1.000000000000000222, 0.9999999999999997780, 1.000000000000000000, 1.000000000000000000, 1.000000000000000222, 0.9999999999999997780, 1.000000000000000444, 1.000000000000000000, 0.9999999999999997780, 1.000000000000000000, 1.000000000000000000, 1.000000000000000222, 0.9999999999999997780, 1.000000000000000222, 1.000000000000000000, 1.000000000000000000, 1.000000000000000000, 1.000000000000000222, 1.000000000000000000, 0.9999999999999997780, 1.000000000000000000, 1.000000000000000000, 1.000000000000000000, 1.000000000000000444, 0.9999999999999996669, 1.000000000000000222, 1.000000000000000000, 1.000000000000000222, 0.9999999999999997780, 1.000000000000000000, 0.9999999999999997780, 1.000000000000000000, 0.9999999999999997780, 1.000000000000000000, 1.000000000000000444, 0.9999999999999994449, 1.000000000000000444, 1.000000000000000000, 1.000000000000000222, 1.000000000000000222, 0.9999999999999997780, 1.000000000000000222, 0.9999999999999997780, 1.000000000000000222, 1.000000000000000222, 1.000000000000000222, 0.9999999999999997780, 1.000000000000000000, 1.000000000000000444, 0.9999999999999996669, 1.000000000000000000, 0.9999999999999997780, 1.000000000000000222, 1.000000000000000222, 1.000000000000000000, 0.9999999999999997780, 1.000000000000000222, 0.9999999999999997780, 1.000000000000000222, 0.9999999999999997780, 0.9999999999999997780, 1.000000000000000000, 1.000000000000000000, 1.000000000000000000, 1.000000000000000000, 1.000000000000000000, 1.000000000000000222, 1.000000000000000000, 1.000000000000000000, 1.000000000000000222, 1.000000000000000000, 0.9999999999999997780, 1.000000000000000000, 1.000000000000000000, 1.000000000000000000, 0.9999999999999997780, 1.000000000000000000, 0.9999999999999997780, 1.000000000000000000, 1.000000000000000222, 0.9999999999999996669, 1.000000000000000444, 1.000000000000000000, 0.9999999999999997780, 1.000000000000000222, 1.000000000000000000, 0.9999999999999997780, 1.000000000000000222, 1.000000000000000000, 1.000000000000000222, 1.000000000000000000, 0.9999999999999997780, 1.000000000000000222, 1.000000000000000000, 1.000000000000000000, 1.000000000000000222, 1.000000000000000000, 1.000000000000000000, 1.000000000000000222, 0.9999999999999997780, 0.9999999999999996669, 1.000000000000000444, 0.9999999999999994449, 1.000000000000000444, 0.9999999999999997780, 1.000000000000000222, 1.000000000000000000, 1.000000000000000000, 1.000000000000000000, 1.000000000000000000, 1.000000000000000444, 0.9999999999999996669, 1.000000000000000444, 1.000000000000000000, 0.9999999999999997780, 1.000000000000000444, 0.9999999999999994449, 1.000000000000000444, 0.9999999999999997780, 0.9999999999999997780, 1.000000000000000222, 1.000000000000000444, 0.9999999999999997780, 1.000000000000000444, 0.9999999999999997780, 1.000000000000000000, 1.000000000000000444, 0.9999999999999997780, 0.9999999999999997780, 1.000000000000000000, 1.000000000000000000, 1.000000000000000000, 0.9999999999999997780, 1.000000000000000444, 1.000000000000000222, 0.9999999999999997780, 1.000000000000000444, 1.000000000000000000, 1.000000000000000222, 1.000000000000000000, 1.000000000000000000, 1.000000000000000222, 0.9999999999999997780, 1.000000000000000222, 1.000000000000000222, 0.9999999999999997780, 1.000000000000000222, 1.000000000000000000, 1.000000000000000000, 1.000000000000000222, 0.9999999999999997780, 1.000000000000000444, 0.9999999999999997780, 0.9999999999999997780, 1.000000000000000222, 0.9999999999999997780, 1.000000000000000000, 1.000000000000000000, 0.9999999999999997780, 1.000000000000000222, 0.9999999999999996669, 1.000000000000000444, 0.9999999999999997780, 1.000000000000000222, 1.000000000000000222, 0.9999999999999997780, 1.000000000000000222, 0.9999999999999997780, 1.000000000000000000, 0.9999999999999997780, 1.000000000000000444, 0.9999999999999996669, 1.000000000000000222, 0.9999999999999996669, 1.000000000000000444, 1.000000000000000000, 0.9999999999999997780, 1.000000000000000222, 0.9999999999999996669, 1.000000000000000222, 1.000000000000000222, 0.9999999999999996669, 1.000000000000000444, 1.000000000000000222, 0.9999999999999997780, 1.000000000000000222, 0.9999999999999997780, 1.000000000000000222, 1.000000000000000000, 1.000000000000000222, 0.9999999999999996669, 1.000000000000000444, 1.000000000000000000, 1.000000000000000000, 1.000000000000000222, 0.9999999999999997780, 0.9999999999999997780, 1.000000000000000444, 1.000000000000000000, 1.000000000000000000, 0.9999999999999996669, 1.000000000000000000, 1.000000000000000222, 1.000000000000000000, 1.000000000000000000, 1.000000000000000222, 0.9999999999999997780, 1.000000000000000000, 0.9999999999999997780, 0.9999999999999997780, 1.000000000000000222, 0.9999999999999997780, 1.000000000000000000, 1.000000000000000000, 0.9999999999999997780, 1.000000000000000222, 1.000000000000000000, 1.000000000000000222, 1.000000000000000000, 1.000000000000000444, 1.000000000000000000, 1.000000000000000000, 0.9999999999999997780, 0.9999999999999997780, 1.000000000000000222, 1.000000000000000000, 1.000000000000000000, 1.000000000000000000, 0.9999999999999997780, 1.000000000000000222, 1.000000000000000000, 1.000000000000000000),
 ( 0.3333333333333333703, 0.3333333333333333703, 0.3333333333333333703, 0.3333333333333333148, 0.3333333333333334259, 0.3333333333333334814, 0.3333333333333332593, 0.3333333333333332593, 0.3333333333333334814, 0.3333333333333333703, 0.3333333333333333703, 0.3333333333333334259, 0.3333333333333334259, 0.3333333333333334259, 0.3333333333333332593, 0.3333333333333334259, 0.3333333333333334259, 0.3333333333333333703, 0.3333333333333334259, 0.3333333333333332038, 0.3333333333333334259, 0.3333333333333333148, 0.3333333333333334259, 0.3333333333333333703, 0.3333333333333333703, 0.3333333333333334259, 0.3333333333333333148, 0.3333333333333334259, 0.3333333333333333703, 0.3333333333333333703, 0.3333333333333333148, 0.3333333333333334259, 0.3333333333333333703, 0.3333333333333333703, 0.3333333333333333148, 0.3333333333333333148, 0.3333333333333334259, 0.3333333333333333148, 0.3333333333333334259, 0.3333333333333333703, 0.3333333333333333703, 0.3333333333333333703, 0.3333333333333332593, 0.3333333333333334814, 0.3333333333333332593, 0.3333333333333333703, 0.3333333333333333703, 0.3333333333333333703, 0.3333333333333335369, 0.3333333333333332593, 0.3333333333333333703, 0.3333333333333335369, 0.3333333333333333703, 0.3333333333333333703, 0.3333333333333335369, 0.3333333333333333703, 0.3333333333333334259, 0.3333333333333334259, 0.3333333333333333703, 0.3333333333333333703, 0.3333333333333333703, 0.3333333333333333703, 0.3333333333333333703, 0.3333333333333333148, 0.3333333333333334259, 0.3333333333333334814, 0.3333333333333333148, 0.3333333333333333703, 0.3333333333333333148, 0.3333333333333334259, 0.3333333333333332593, 0.3333333333333334259, 0.3333333333333333703, 0.3333333333333334259, 0.3333333333333333703, 0.3333333333333333703, 0.3333333333333333703, 0.3333333333333333148, 0.3333333333333334814, 0.3333333333333332038, 0.3333333333333334259, 0.3333333333333334259, 0.3333333333333333148, 0.3333333333333334259, 0.3333333333333333703, 0.3333333333333333148, 0.3333333333333333703, 0.3333333333333333148, 0.3333333333333334814, 0.3333333333333333148, 0.3333333333333333148, 0.3333333333333334259, 0.3333333333333333148, 0.3333333333333333148, 0.3333333333333334814, 0.3333333333333333148, 0.3333333333333334259, 0.3333333333333333703, 0.3333333333333333148, 0.3333333333333333703, 0.3333333333333334259, 0.3333333333333333148, 0.3333333333333334259, 0.3333333333333333148, 0.3333333333333333703, 0.3333333333333333148, 0.3333333333333333703, 0.3333333333333333703, 0.3333333333333333148, 0.3333333333333334259, 0.3333333333333334259, 0.3333333333333333148, 0.3333333333333333703, 0.3333333333333333703, 0.3333333333333334259, 0.3333333333333333703, 0.3333333333333333703, 0.3333333333333334259, 0.3333333333333333703, 0.3333333333333334259, 0.3333333333333333148, 0.3333333333333333703, 0.3333333333333333148, 0.3333333333333335369, 0.3333333333333333148, 0.3333333333333335369, 0.3333333333333333703, 0.3333333333333332593, 0.3333333333333334259, 0.3333333333333334259, 0.3333333333333333148, 0.3333333333333333703, 0.3333333333333333148, 0.3333333333333335369, 0.3333333333333333148, 0.3333333333333333703, 0.3333333333333333703, 0.3333333333333334259, 0.3333333333333334259, 0.3333333333333333703, 0.3333333333333334259, 0.3333333333333332593, 0.3333333333333334814, 0.3333333333333333148, 0.3333333333333333703, 0.3333333333333333148, 0.3333333333333333148, 0.3333333333333334259, 0.3333333333333332593, 0.3333333333333333148, 0.3333333333333333703, 0.3333333333333333148, 0.3333333333333333703, 0.3333333333333334259, 0.3333333333333333703, 0.3333333333333334259, 0.3333333333333333148, 0.3333333333333333703, 0.3333333333333333703, 0.3333333333333333703, 0.3333333333333333148, 0.3333333333333335369, 0.3333333333333333148, 0.3333333333333333703, 0.3333333333333333148, 0.3333333333333334259, 0.3333333333333334259, 0.3333333333333333703, 0.3333333333333334259, 0.3333333333333333703, 0.3333333333333333703, 0.3333333333333334259, 0.3333333333333333703, 0.3333333333333333703, 0.3333333333333333703, 0.3333333333333334259, 0.3333333333333333148, 0.3333333333333333148, 0.3333333333333335369, 0.3333333333333333148, 0.3333333333333334259, 0.3333333333333333148, 0.3333333333333334259, 0.3333333333333333703, 0.3333333333333333148, 0.3333333333333333148, 0.3333333333333333703, 0.3333333333333333148, 0.3333333333333334259, 0.3333333333333334259, 0.3333333333333332038, 0.3333333333333335369, 0.3333333333333333703, 0.3333333333333334259, 0.3333333333333334259, 0.3333333333333333703, 0.3333333333333334259, 0.3333333333333332593, 0.3333333333333334814, 0.3333333333333333703, 0.3333333333333334259, 0.3333333333333333148, 0.3333333333333333148, 0.3333333333333335369, 0.3333333333333332593, 0.3333333333333333703, 0.3333333333333332593, 0.3333333333333335369, 0.3333333333333333703, 0.3333333333333333703, 0.3333333333333333703, 0.3333333333333334259, 0.3333333333333332593, 0.3333333333333334814, 0.3333333333333332593, 0.3333333333333333703, 0.3333333333333333703, 0.3333333333333333703, 0.3333333333333334259, 0.3333333333333333148, 0.3333333333333334259, 0.3333333333333334259, 0.3333333333333333703, 0.3333333333333333148, 0.3333333333333334259, 0.3333333333333333148, 0.3333333333333333703, 0.3333333333333333148, 0.3333333333333333703, 0.3333333333333333703, 0.3333333333333333148, 0.3333333333333333703, 0.3333333333333333703, 0.3333333333333333703, 0.3333333333333334259, 0.3333333333333333703, 0.3333333333333333703, 0.3333333333333334814, 0.3333333333333332593, 0.3333333333333333703, 0.3333333333333334259, 0.3333333333333333148, 0.3333333333333334259, 0.3333333333333333703, 0.3333333333333334814, 0.3333333333333333703, 0.3333333333333333148, 0.3333333333333334259, 0.3333333333333333703, 0.3333333333333333703, 0.3333333333333333703, 0.3333333333333334259, 0.3333333333333333148, 0.3333333333333334259, 0.3333333333333333148, 0.3333333333333333148, 0.3333333333333335369, 0.3333333333333332038, 0.3333333333333335369, 0.3333333333333333148, 0.3333333333333333703, 0.3333333333333334259, 0.3333333333333333703, 0.3333333333333333148, 0.3333333333333333703, 0.3333333333333334259, 0.3333333333333333703, 0.3333333333333334259, 0.3333333333333333148, 0.3333333333333333703, 0.3333333333333334259, 0.3333333333333333148, 0.3333333333333333703, 0.3333333333333333703, 0.3333333333333333148, 0.3333333333333334259, 0.3333333333333334259, 0.3333333333333333703, 0.3333333333333335369, 0.3333333333333333148, 0.3333333333333333703, 0.3333333333333333703, 0.3333333333333333148, 0.3333333333333333703, 0.3333333333333333703, 0.3333333333333333703, 0.3333333333333333148, 0.3333333333333333703, 0.3333333333333334814, 0.3333333333333333703, 0.3333333333333333703, 0.3333333333333335369, 0.3333333333333333703, 0.3333333333333333703, 0.3333333333333334259, 0.3333333333333334259, 0.3333333333333333703, 0.3333333333333333703, 0.3333333333333333703, 0.3333333333333333703, 0.3333333333333333148, 0.3333333333333334259, 0.3333333333333333703, 0.3333333333333333703, 0.3333333333333333703, 0.3333333333333333148, 0.3333333333333334814, 0.3333333333333333148, 0.3333333333333333148, 0.3333333333333334814, 0.3333333333333333148, 0.3333333333333333148, 0.3333333333333334259, 0.3333333333333333148, 0.3333333333333334259, 0.3333333333333333148, 0.3333333333333334259, 0.3333333333333332593, 0.3333333333333335369, 0.3333333333333333148, 0.3333333333333333148, 0.3333333333333334259, 0.3333333333333333703, 0.3333333333333333703, 0.3333333333333333148, 0.3333333333333334259, 0.3333333333333333148, 0.3333333333333334259, 0.3333333333333333148, 0.3333333333333334259, 0.3333333333333334259, 0.3333333333333333703, 0.3333333333333334259, 0.3333333333333333703, 0.3333333333333333703, 0.3333333333333334259, 0.3333333333333333148, 0.3333333333333335369, 0.3333333333333334259, 0.3333333333333333148, 0.3333333333333333703, 0.3333333333333333148, 0.3333333333333334814, 0.3333333333333333703, 0.3333333333333333703, 0.3333333333333332593, 0.3333333333333334814, 0.3333333333333333703, 0.3333333333333333148, 0.3333333333333334259, 0.3333333333333332593, 0.3333333333333334814, 0.3333333333333333703, 0.3333333333333334259, 0.3333333333333333703, 0.3333333333333333148, 0.3333333333333333703, 0.3333333333333334259, 0.3333333333333333703, 0.3333333333333334259, 0.3333333333333333703, 0.3333333333333333703, 0.3333333333333333148, 0.3333333333333333148, 0.3333333333333333703, 0.3333333333333333703, 0.3333333333333333703, 0.3333333333333333703, 0.3333333333333333703, 0.3333333333333333148, 0.3333333333333334814, 0.3333333333333333148, 0.3333333333333334814, 0.3333333333333333703, 0.3333333333333334259, 0.3333333333333334259, 0.3333333333333333703, 0.3333333333333332593, 0.3333333333333333703, 0.3333333333333333703, 0.3333333333333333703, 0.3333333333333333148, 0.3333333333333333703, 0.3333333333333332593, 0.3333333333333334259, 0.3333333333333333703, 0.3333333333333333703),
 ( 0.3333333333333333703, 0.3333333333333333703, 0.3333333333333333703, 0.3333333333333333148, 0.3333333333333334259, 0.3333333333333334814, 0.3333333333333332593, 0.3333333333333332593, 0.3333333333333334814, 0.3333333333333333703, 0.3333333333333333703, 0.3333333333333334259, 0.3333333333333334259, 0.3333333333333334259, 0.3333333333333332593, 0.3333333333333334259, 0.3333333333333334259, 0.3333333333333333703, 0.3333333333333334259, 0.3333333333333332038, 0.3333333333333334259, 0.3333333333333333148, 0.3333333333333334259, 0.3333333333333333703, 0.3333333333333333703, 0.3333333333333334259, 0.3333333333333333148, 0.3333333333333334259, 0.3333333333333333703, 0.3333333333333333703, 0.3333333333333333148, 0.3333333333333334259, 0.3333333333333333703, 0.3333333333333333703, 0.3333333333333333148, 0.3333333333333333148, 0.3333333333333334259, 0.3333333333333333148, 0.3333333333333334259, 0.3333333333333333703, 0.3333333333333333703, 0.3333333333333333703, 0.3333333333333332593, 0.3333333333333334814, 0.3333333333333332593, 0.3333333333333333703, 0.3333333333333333703, 0.3333333333333333703, 0.3333333333333335369, 0.3333333333333332593, 0.3333333333333333703, 0.3333333333333335369, 0.3333333333333333703, 0.3333333333333333703, 0.3333333333333335369, 0.3333333333333333703, 0.3333333333333334259, 0.3333333333333334259, 0.3333333333333333703, 0.3333333333333333703, 0.3333333333333333703, 0.3333333333333333703, 0.3333333333333333703, 0.3333333333333333148, 0.3333333333333334259, 0.3333333333333334814, 0.3333333333333333148, 0.3333333333333333703, 0.3333333333333333148, 0.3333333333333334259, 0.3333333333333332593, 0.3333333333333334259, 0.3333333333333333703, 0.3333333333333334259, 0.3333333333333333703, 0.3333333333333333703, 0.3333333333333333703, 0.3333333333333333148, 0.3333333333333334814, 0.3333333333333332038, 0.3333333333333334259, 0.3333333333333334259, 0.3333333333333333148, 0.3333333333333334259, 0.3333333333333333703, 0.3333333333333333148, 0.3333333333333333703, 0.3333333333333333148, 0.3333333333333334814, 0.3333333333333333148, 0.3333333333333333148, 0.3333333333333334259, 0.3333333333333333148, 0.3333333333333333148, 0.3333333333333334814, 0.3333333333333333148, 0.3333333333333334259, 0.3333333333333333703, 0.3333333333333333148, 0.3333333333333333703, 0.3333333333333334259, 0.3333333333333333148, 0.3333333333333334259, 0.3333333333333333148, 0.3333333333333333703, 0.3333333333333333148, 0.3333333333333333703, 0.3333333333333333703, 0.3333333333333333148, 0.3333333333333334259, 0.3333333333333334259, 0.3333333333333333148, 0.3333333333333333703, 0.3333333333333333703, 0.3333333333333334259, 0.3333333333333333703, 0.3333333333333333703, 0.3333333333333334259, 0.3333333333333333703, 0.3333333333333334259, 0.3333333333333333148, 0.3333333333333333703, 0.3333333333333333148, 0.3333333333333335369, 0.3333333333333333148, 0.3333333333333335369, 0.3333333333333333703, 0.3333333333333332593, 0.3333333333333334259, 0.3333333333333334259, 0.3333333333333333148, 0.3333333333333333703, 0.3333333333333333148, 0.3333333333333335369, 0.3333333333333333148, 0.3333333333333333703, 0.3333333333333333703, 0.3333333333333334259, 0.3333333333333334259, 0.3333333333333333703, 0.3333333333333334259, 0.3333333333333332593, 0.3333333333333334814, 0.3333333333333333148, 0.3333333333333333703, 0.3333333333333333148, 0.3333333333333333148, 0.3333333333333334259, 0.3333333333333332593, 0.3333333333333333148, 0.3333333333333333703, 0.3333333333333333148, 0.3333333333333333703, 0.3333333333333334259, 0.3333333333333333703, 0.3333333333333334259, 0.3333333333333333148, 0.3333333333333333703, 0.3333333333333333703, 0.3333333333333333703, 0.3333333333333333148, 0.3333333333333335369, 0.3333333333333333148, 0.3333333333333333703, 0.3333333333333333148, 0.3333333333333334259, 0.3333333333333334259, 0.3333333333333333703, 0.3333333333333334259, 0.3333333333333333703, 0.3333333333333333703, 0.3333333333333334259, 0.3333333333333333703, 0.3333333333333333703, 0.3333333333333333703, 0.3333333333333334259, 0.3333333333333333148, 0.3333333333333333148, 0.3333333333333335369, 0.3333333333333333148, 0.3333333333333334259, 0.3333333333333333148, 0.3333333333333334259, 0.3333333333333333703, 0.3333333333333333148, 0.3333333333333333148, 0.3333333333333333703, 0.3333333333333333148, 0.3333333333333334259, 0.3333333333333334259, 0.3333333333333332038, 0.3333333333333335369, 0.3333333333333333703, 0.3333333333333334259, 0.3333333333333334259, 0.3333333333333333703, 0.3333333333333334259, 0.3333333333333332593, 0.3333333333333334814, 0.3333333333333333703, 0.3333333333333334259, 0.3333333333333333148, 0.3333333333333333148, 0.3333333333333335369, 0.3333333333333332593, 0.3333333333333333703, 0.3333333333333332593, 0.3333333333333335369, 0.3333333333333333703, 0.3333333333333333703, 0.3333333333333333703, 0.3333333333333334259, 0.3333333333333332593, 0.3333333333333334814, 0.3333333333333332593, 0.3333333333333333703, 0.3333333333333333703, 0.3333333333333333703, 0.3333333333333334259, 0.3333333333333333148, 0.3333333333333334259, 0.3333333333333334259, 0.3333333333333333703, 0.3333333333333333148, 0.3333333333333334259, 0.3333333333333333148, 0.3333333333333333703, 0.3333333333333333148, 0.3333333333333333703, 0.3333333333333333703, 0.3333333333333333148, 0.3333333333333333703, 0.3333333333333333703, 0.3333333333333333703, 0.3333333333333334259, 0.3333333333333333703, 0.3333333333333333703, 0.3333333333333334814, 0.3333333333333332593, 0.3333333333333333703, 0.3333333333333334259, 0.3333333333333333148, 0.3333333333333334259, 0.3333333333333333703, 0.3333333333333334814, 0.3333333333333333703, 0.3333333333333333148, 0.3333333333333334259, 0.3333333333333333703, 0.3333333333333333703, 0.3333333333333333703, 0.3333333333333334259, 0.3333333333333333148, 0.3333333333333334259, 0.3333333333333333148, 0.3333333333333333148, 0.3333333333333335369, 0.3333333333333332038, 0.3333333333333335369, 0.3333333333333333148, 0.3333333333333333703, 0.3333333333333334259, 0.3333333333333333703, 0.3333333333333333148, 0.3333333333333333703, 0.3333333333333334259, 0.3333333333333333703, 0.3333333333333334259, 0.3333333333333333148, 0.3333333333333333703, 0.3333333333333334259, 0.3333333333333333148, 0.3333333333333333703, 0.3333333333333333703, 0.3333333333333333148, 0.3333333333333334259, 0.3333333333333334259, 0.3333333333333333703, 0.3333333333333335369, 0.3333333333333333148, 0.3333333333333333703, 0.3333333333333333703, 0.3333333333333333148, 0.3333333333333333703, 0.3333333333333333703, 0.3333333333333333703, 0.3333333333333333148, 0.3333333333333333703, 0.3333333333333334814, 0.3333333333333333703, 0.3333333333333333703, 0.3333333333333335369, 0.3333333333333333703, 0.3333333333333333703, 0.3333333333333334259, 0.3333333333333334259, 0.3333333333333333703, 0.3333333333333333703, 0.3333333333333333703, 0.3333333333333333703, 0.3333333333333333148, 0.3333333333333334259, 0.3333333333333333703, 0.3333333333333333703, 0.3333333333333333703, 0.3333333333333333148, 0.3333333333333334814, 0.3333333333333333148, 0.3333333333333333148, 0.3333333333333334814, 0.3333333333333333148, 0.3333333333333333148, 0.3333333333333334259, 0.3333333333333333148, 0.3333333333333334259, 0.3333333333333333148, 0.3333333333333334259, 0.3333333333333332593, 0.3333333333333335369, 0.3333333333333333148, 0.3333333333333333148, 0.3333333333333334259, 0.3333333333333333703, 0.3333333333333333703, 0.3333333333333333148, 0.3333333333333334259, 0.3333333333333333148, 0.3333333333333334259, 0.3333333333333333148, 0.3333333333333334259, 0.3333333333333334259, 0.3333333333333333703, 0.3333333333333334259, 0.3333333333333333703, 0.3333333333333333703, 0.3333333333333334259, 0.3333333333333333148, 0.3333333333333335369, 0.3333333333333334259, 0.3333333333333333148, 0.3333333333333333703, 0.3333333333333333148, 0.3333333333333334814, 0.3333333333333333703, 0.3333333333333333703, 0.3333333333333332593, 0.3333333333333334814, 0.3333333333333333703, 0.3333333333333333148, 0.3333333333333334259, 0.3333333333333332593, 0.3333333333333334814, 0.3333333333333333703, 0.3333333333333334259, 0.3333333333333333703, 0.3333333333333333148, 0.3333333333333333703, 0.3333333333333334259, 0.3333333333333333703, 0.3333333333333334259, 0.3333333333333333703, 0.3333333333333333703, 0.3333333333333333148, 0.3333333333333333148, 0.3333333333333333703, 0.3333333333333333703, 0.3333333333333333703, 0.3333333333333333703, 0.3333333333333333703, 0.3333333333333333148, 0.3333333333333334814, 0.3333333333333333148, 0.3333333333333334814, 0.3333333333333333703, 0.3333333333333334259, 0.3333333333333334259, 0.3333333333333333703, 0.3333333333333332593, 0.3333333333333333703, 0.3333333333333333703, 0.3333333333333333703, 0.3333333333333333148, 0.3333333333333333703, 0.3333333333333332593, 0.3333333333333334259, 0.3333333333333333703, 0.3333333333333333703),
 ( 1.000000000000000000, 1.000000000000000000, 1.000000000000000000, 0.9999999999999997780, 1.000000000000000000, 1.000000000000000444, 0.9999999999999996669, 0.9999999999999996669, 1.000000000000000444, 1.000000000000000000, 1.000000000000000000, 1.000000000000000000, 1.000000000000000222, 1.000000000000000222, 0.9999999999999997780, 1.000000000000000000, 1.000000000000000222, 1.000000000000000000, 1.000000000000000222, 0.9999999999999994449, 1.000000000000000222, 0.9999999999999997780, 1.000000000000000444, 1.000000000000000000, 1.000000000000000000, 1.000000000000000222, 0.9999999999999997780, 1.000000000000000222, 1.000000000000000000, 1.000000000000000222, 0.9999999999999997780, 1.000000000000000000, 1.000000000000000000, 0.9999999999999997780, 1.000000000000000000, 1.000000000000000000, 1.000000000000000222, 1.000000000000000000, 0.9999999999999997780, 1.000000000000000222, 0.9999999999999997780, 1.000000000000000000, 0.9999999999999997780, 1.000000000000000444, 0.9999999999999996669, 1.000000000000000222, 1.000000000000000000, 1.000000000000000000, 1.000000000000000444, 0.9999999999999996669, 1.000000000000000222, 1.000000000000000444, 1.000000000000000000, 0.9999999999999997780, 1.000000000000000444, 1.000000000000000222, 1.000000000000000000, 1.000000000000000000, 1.000000000000000222, 1.000000000000000000, 1.000000000000000222, 0.9999999999999997780, 1.000000000000000222, 1.000000000000000000, 1.000000000000000000, 1.000000000000000444, 0.9999999999999996669, 1.000000000000000000, 0.9999999999999997780, 1.000000000000000222, 0.9999999999999996669, 1.000000000000000000, 1.000000000000000222, 0.9999999999999997780, 1.000000000000000444, 0.9999999999999997780, 1.000000000000000000, 0.9999999999999997780, 1.000000000000000222, 0.9999999999999996669, 1.000000000000000000, 1.000000000000000222, 0.9999999999999996669, 1.000000000000000444, 0.9999999999999997780, 1.000000000000000000, 1.000000000000000222, 0.9999999999999996669, 1.000000000000000222, 1.000000000000000000, 0.9999999999999997780, 1.000000000000000222, 0.9999999999999997780, 1.000000000000000000, 1.000000000000000222, 0.9999999999999997780, 1.000000000000000000, 1.000000000000000000, 0.9999999999999997780, 1.000000000000000000, 1.000000000000000222, 0.9999999999999997780, 1.000000000000000000, 1.000000000000000000, 1.000000000000000000, 0.9999999999999997780, 1.000000000000000222, 0.9999999999999997780, 0.9999999999999997780, 1.000000000000000444, 1.000000000000000000, 1.000000000000000000, 0.9999999999999997780, 1.000000000000000222, 1.000000000000000000, 1.000000000000000000, 1.000000000000000000, 1.000000000000000000, 1.000000000000000222, 1.000000000000000222, 0.9999999999999997780, 1.000000000000000000, 0.9999999999999997780, 1.000000000000000444, 0.9999999999999996669, 1.000000000000000666, 1.000000000000000000, 0.9999999999999997780, 1.000000000000000222, 1.000000000000000000, 1.000000000000000000, 1.000000000000000000, 0.9999999999999994449, 1.000000000000000666, 0.9999999999999996669, 1.000000000000000000, 1.000000000000000222, 0.9999999999999997780, 1.000000000000000222, 0.9999999999999997780, 1.000000000000000222, 0.9999999999999996669, 1.000000000000000444, 1.000000000000000000, 1.000000000000000222, 0.9999999999999996669, 1.000000000000000000, 1.000000000000000222, 0.9999999999999997780, 1.000000000000000000, 0.9999999999999997780, 1.000000000000000000, 1.000000000000000000, 1.000000000000000222, 0.9999999999999997780, 1.000000000000000222, 0.9999999999999997780, 1.000000000000000000, 1.000000000000000000, 1.000000000000000222, 0.9999999999999997780, 1.000000000000000444, 1.000000000000000000, 0.9999999999999997780, 1.000000000000000000, 1.000000000000000000, 1.000000000000000222, 0.9999999999999997780, 1.000000000000000222, 1.000000000000000000, 1.000000000000000000, 1.000000000000000000, 1.000000000000000222, 1.000000000000000000, 0.9999999999999997780, 1.000000000000000000, 1.000000000000000000, 1.000000000000000000, 1.000000000000000444, 0.9999999999999996669, 1.000000000000000222, 1.000000000000000000, 1.000000000000000222, 0.9999999999999997780, 1.000000000000000000, 0.9999999999999997780, 1.000000000000000000, 0.9999999999999997780, 1.000000000000000000, 1.000000000000000444, 0.9999999999999994449, 1.000000000000000444, 1.000000000000000000, 1.000000000000000222, 1.000000000000000222, 0.9999999999999997780, 1.000000000000000222, 0.9999999999999997780, 1.000000000000000222, 1.000000000000000222, 1.000000000000000222, 0.9999999999999997780, 1.000000000000000000, 1.000000000000000444, 0.9999999999999996669, 1.000000000000000000, 0.9999999999999997780, 1.000000000000000222, 1.000000000000000222, 1.000000000000000000, 0.9999999999999997780, 1.000000000000000222, 0.9999999999999997780, 1.000000000000000222, 0.9999999999999997780, 0.9999999999999997780, 1.000000000000000000, 1.000000000000000000, 1.000000000000000000, 1.000000000000000000, 1.000000000000000000, 1.000000000000000222, 1.000000000000000000, 1.000000000000000000, 1.000000000000000222, 1.000000000000000000, 0.9999999999999997780, 1.000000000000000000, 1.000000000000000000, 1.000000000000000000, 0.9999999999999997780, 1.000000000000000000, 0.9999999999999997780, 1.000000000000000000, 1.000000000000000222, 0.9999999999999996669, 1.000000000000000444, 1.000000000000000000, 0.9999999999999997780, 1.000000000000000222, 1.000000000000000000, 0.9999999999999997780, 1.000000000000000222, 1.000000000000000000, 1.000000000000000222, 1.000000000000000000, 0.9999999999999997780, 1.000000000000000222, 1.000000000000000000, 1.000000000000000000, 1.000000000000000222, 1.000000000000000000, 1.000000000000000000, 1.000000000000000222, 0.9999999999999997780, 0.9999999999999996669, 1.000000000000000444, 0.9999999999999994449, 1.000000000000000444, 0.9999999999999997780, 1.000000000000000222, 1.000000000000000000, 1.000000000000000000, 1.000000000000000000, 1.000000000000000000, 1.000000000000000444, 0.9999999999999996669, 1.000000000000000444, 1.000000000000000000, 0.9999999999999997780, 1.000000000000000444, 0.9999999999999994449, 1.000000000000000444, 0.9999999999999997780, 0.9999999999999997780, 1.000000000000000222, 1.000000000000000444, 0.9999999999999997780, 1.000000000000000444, 0.9999999999999997780, 1.000000000000000000, 1.000000000000000444, 0.9999999999999997780, 0.9999999999999997780, 1.000000000000000000, 1.000000000000000000, 1.000000000000000000, 0.9999999999999997780, 1.000000000000000444, 1.000000000000000222, 0.9999999999999997780, 1.000000000000000444, 1.000000000000000000, 1.000000000000000222, 1.000000000000000000, 1.000000000000000000, 1.000000000000000222, 0.9999999999999997780, 1.000000000000000222, 1.000000000000000222, 0.9999999999999997780, 1.000000000000000222, 1.000000000000000000, 1.000000000000000000, 1.000000000000000222, 0.9999999999999997780, 1.000000000000000444, 0.9999999999999997780, 0.9999999999999997780, 1.000000000000000222, 0.9999999999999997780, 1.000000000000000000, 1.000000000000000000, 0.9999999999999997780, 1.000000000000000222, 0.9999999999999996669, 1.000000000000000444, 0.9999999999999997780, 1.000000000000000222, 1.000000000000000222, 0.9999999999999997780, 1.000000000000000222, 0.9999999999999997780, 1.000000000000000000, 0.9999999999999997780, 1.000000000000000444, 0.9999999999999996669, 1.000000000000000222, 0.9999999999999996669, 1.000000000000000444, 1.000000000000000000, 0.9999999999999997780, 1.000000000000000222, 0.9999999999999996669, 1.000000000000000222, 1.000000000000000222, 0.9999999999999996669, 1.000000000000000444, 1.000000000000000222, 0.9999999999999997780, 1.000000000000000222, 0.9999999999999997780, 1.000000000000000222, 1.000000000000000000, 1.000000000000000222, 0.9999999999999996669, 1.000000000000000444, 1.000000000000000000, 1.000000000000000000, 1.000000000000000222, 0.9999999999999997780, 0.9999999999999997780, 1.000000000000000444, 1.000000000000000000, 1.000000000000000000, 0.9999999999999996669, 1.000000000000000000, 1.000000000000000222, 1.000000000000000000, 1.000000000000000000, 1.000000000000000222, 0.9999999999999997780, 1.000000000000000000, 0.9999999999999997780, 0.9999999999999997780, 1.000000000000000222, 0.9999999999999997780, 1.000000000000000000, 1.000000000000000000, 0.9999999999999997780, 1.000000000000000222, 1.000000000000000000, 1.000000000000000222, 1.000000000000000000, 1.000000000000000444, 1.000000000000000000, 1.000000000000000000, 0.9999999999999997780, 0.9999999999999997780, 1.000000000000000222, 1.000000000000000000, 1.000000000000000000, 1.000000000000000000, 0.9999999999999997780, 1.000000000000000222, 1.000000000000000000, 1.000000000000000000),
 ( 0.3333333333333333703, 0.3333333333333333703, 0.3333333333333333703, 0.3333333333333333148, 0.3333333333333334259, 0.3333333333333334814, 0.3333333333333332593, 0.3333333333333332593, 0.3333333333333334814, 0.3333333333333333703, 0.3333333333333333703, 0.3333333333333334259, 0.3333333333333334259, 0.3333333333333334259, 0.3333333333333332593, 0.3333333333333334259, 0.3333333333333334259, 0.3333333333333333703, 0.3333333333333334259, 0.3333333333333332038, 0.3333333333333334259, 0.3333333333333333148, 0.3333333333333334259, 0.3333333333333333703, 0.3333333333333333703, 0.3333333333333334259, 0.3333333333333333148, 0.3333333333333334259, 0.3333333333333333703, 0.3333333333333333703, 0.3333333333333333148, 0.3333333333333334259, 0.3333333333333333703, 0.3333333333333333703, 0.3333333333333333148, 0.3333333333333333148, 0.3333333333333334259, 0.3333333333333333148, 0.3333333333333334259, 0.3333333333333333703, 0.3333333333333333703, 0.3333333333333333703, 0.3333333333333332593, 0.3333333333333334814, 0.3333333333333332593, 0.3333333333333333703, 0.3333333333333333703, 0.3333333333333333703, 0.3333333333333335369, 0.3333333333333332593, 0.3333333333333333703, 0.3333333333333335369, 0.3333333333333333703, 0.3333333333333333703, 0.3333333333333335369, 0.3333333333333333703, 0.3333333333333334259, 0.3333333333333334259, 0.3333333333333333703, 0.3333333333333333703, 0.3333333333333333703, 0.3333333333333333703, 0.3333333333333333703, 0.3333333333333333148, 0.3333333333333334259, 0.3333333333333334814, 0.3333333333333333148, 0.3333333333333333703, 0.3333333333333333148, 0.3333333333333334259, 0.3333333333333332593, 0.3333333333333334259, 0.3333333333333333703, 0.3333333333333334259, 0.3333333333333333703, 0.3333333333333333703, 0.3333333333333333703, 0.3333333333333333148, 0.3333333333333334814, 0.3333333333333332038, 0.3333333333333334259, 0.3333333333333334259, 0.3333333333333333148, 0.3333333333333334259, 0.3333333333333333703, 0.3333333333333333148, 0.3333333333333333703, 0.3333333333333333148, 0.3333333333333334814, 0.3333333333333333148, 0.3333333333333333148, 0.3333333333333334259, 0.3333333333333333148, 0.3333333333333333148, 0.3333333333333334814, 0.3333333333333333148, 0.3333333333333334259, 0.3333333333333333703, 0.3333333333333333148, 0.3333333333333333703, 0.3333333333333334259, 0.3333333333333333148, 0.3333333333333334259, 0.3333333333333333148, 0.3333333333333333703, 0.3333333333333333148, 0.3333333333333333703, 0.3333333333333333703, 0.3333333333333333148, 0.3333333333333334259, 0.3333333333333334259, 0.3333333333333333148, 0.3333333333333333703, 0.3333333333333333703, 0.3333333333333334259, 0.3333333333333333703, 0.3333333333333333703, 0.3333333333333334259, 0.3333333333333333703, 0.3333333333333334259, 0.3333333333333333148, 0.3333333333333333703, 0.3333333333333333148, 0.3333333333333335369, 0.3333333333333333148, 0.3333333333333335369, 0.3333333333333333703, 0.3333333333333332593, 0.3333333333333334259, 0.3333333333333334259, 0.3333333333333333148, 0.3333333333333333703, 0.3333333333333333148, 0.3333333333333335369, 0.3333333333333333148, 0.3333333333333333703, 0.3333333333333333703, 0.3333333333333334259, 0.3333333333333334259, 0.3333333333333333703, 0.3333333333333334259, 0.3333333333333332593, 0.3333333333333334814, 0.3333333333333333148, 0.3333333333333333703, 0.3333333333333333148, 0.3333333333333333148, 0.3333333333333334259, 0.3333333333333332593, 0.3333333333333333148, 0.3333333333333333703, 0.3333333333333333148, 0.3333333333333333703, 0.3333333333333334259, 0.3333333333333333703, 0.3333333333333334259, 0.3333333333333333148, 0.3333333333333333703, 0.3333333333333333703, 0.3333333333333333703, 0.3333333333333333148, 0.3333333333333335369, 0.3333333333333333148, 0.3333333333333333703, 0.3333333333333333148, 0.3333333333333334259, 0.3333333333333334259, 0.3333333333333333703, 0.3333333333333334259, 0.3333333333333333703, 0.3333333333333333703, 0.3333333333333334259, 0.3333333333333333703, 0.3333333333333333703, 0.3333333333333333703, 0.3333333333333334259, 0.3333333333333333148, 0.3333333333333333148, 0.3333333333333335369, 0.3333333333333333148, 0.3333333333333334259, 0.3333333333333333148, 0.3333333333333334259, 0.3333333333333333703, 0.3333333333333333148, 0.3333333333333333148, 0.3333333333333333703, 0.3333333333333333148, 0.3333333333333334259, 0.3333333333333334259, 0.3333333333333332038, 0.3333333333333335369, 0.3333333333333333703, 0.3333333333333334259, 0.3333333333333334259, 0.3333333333333333703, 0.3333333333333334259, 0.3333333333333332593, 0.3333333333333334814, 0.3333333333333333703, 0.3333333333333334259, 0.3333333333333333148, 0.3333333333333333148, 0.3333333333333335369, 0.3333333333333332593, 0.3333333333333333703, 0.3333333333333332593, 0.3333333333333335369, 0.3333333333333333703, 0.3333333333333333703, 0.3333333333333333703, 0.3333333333333334259, 0.3333333333333332593, 0.3333333333333334814, 0.3333333333333332593, 0.3333333333333333703, 0.3333333333333333703, 0.3333333333333333703, 0.3333333333333334259, 0.3333333333333333148, 0.3333333333333334259, 0.3333333333333334259, 0.3333333333333333703, 0.3333333333333333148, 0.3333333333333334259, 0.3333333333333333148, 0.3333333333333333703, 0.3333333333333333148, 0.3333333333333333703, 0.3333333333333333703, 0.3333333333333333148, 0.3333333333333333703, 0.3333333333333333703, 0.3333333333333333703, 0.3333333333333334259, 0.3333333333333333703, 0.3333333333333333703, 0.3333333333333334814, 0.3333333333333332593, 0.3333333333333333703, 0.3333333333333334259, 0.3333333333333333148, 0.3333333333333334259, 0.3333333333333333703, 0.3333333333333334814, 0.3333333333333333703, 0.3333333333333333148, 0.3333333333333334259, 0.3333333333333333703, 0.3333333333333333703, 0.3333333333333333703, 0.3333333333333334259, 0.3333333333333333148, 0.3333333333333334259, 0.3333333333333333148, 0.3333333333333333148, 0.3333333333333335369, 0.3333333333333332038, 0.3333333333333335369, 0.3333333333333333148, 0.3333333333333333703, 0.3333333333333334259, 0.3333333333333333703, 0.3333333333333333148, 0.3333333333333333703, 0.3333333333333334259, 0.3333333333333333703, 0.3333333333333334259, 0.3333333333333333148, 0.3333333333333333703, 0.3333333333333334259, 0.3333333333333333148, 0.3333333333333333703, 0.3333333333333333703, 0.3333333333333333148, 0.3333333333333334259, 0.3333333333333334259, 0.3333333333333333703, 0.3333333333333335369, 0.3333333333333333148, 0.3333333333333333703, 0.3333333333333333703, 0.3333333333333333148, 0.3333333333333333703, 0.3333333333333333703, 0.3333333333333333703, 0.3333333333333333148, 0.3333333333333333703, 0.3333333333333334814, 0.3333333333333333703, 0.3333333333333333703, 0.3333333333333335369, 0.3333333333333333703, 0.3333333333333333703, 0.3333333333333334259, 0.3333333333333334259, 0.3333333333333333703, 0.3333333333333333703, 0.3333333333333333703, 0.3333333333333333703, 0.3333333333333333148, 0.3333333333333334259, 0.3333333333333333703, 0.3333333333333333703, 0.3333333333333333703, 0.3333333333333333148, 0.3333333333333334814, 0.3333333333333333148, 0.3333333333333333148, 0.3333333333333334814, 0.3333333333333333148, 0.3333333333333333148, 0.3333333333333334259, 0.3333333333333333148, 0.3333333333333334259, 0.3333333333333333148, 0.3333333333333334259, 0.3333333333333332593, 0.3333333333333335369, 0.3333333333333333148, 0.3333333333333333148, 0.3333333333333334259, 0.3333333333333333703, 0.3333333333333333703, 0.3333333333333333148, 0.3333333333333334259, 0.3333333333333333148, 0.3333333333333334259, 0.3333333333333333148, 0.3333333333333334259, 0.3333333333333334259, 0.3333333333333333703, 0.3333333333333334259, 0.3333333333333333703, 0.3333333333333333703, 0.3333333333333334259, 0.3333333333333333148, 0.3333333333333335369, 0.3333333333333334259, 0.3333333333333333148, 0.3333333333333333703, 0.3333333333333333148, 0.3333333333333334814, 0.3333333333333333703, 0.3333333333333333703, 0.3333333333333332593, 0.3333333333333334814, 0.3333333333333333703, 0.3333333333333333148, 0.3333333333333334259, 0.3333333333333332593, 0.3333333333333334814, 0.3333333333333333703, 0.3333333333333334259, 0.3333333333333333703, 0.3333333333333333148, 0.3333333333333333703, 0.3333333333333334259, 0.3333333333333333703, 0.3333333333333334259, 0.3333333333333333703, 0.3333333333333333703, 0.3333333333333333148, 0.3333333333333333148, 0.3333333333333333703, 0.3333333333333333703, 0.3333333333333333703, 0.3333333333333333703, 0.3333333333333333703, 0.3333333333333333148, 0.3333333333333334814, 0.3333333333333333148, 0.3333333333333334814, 0.3333333333333333703, 0.3333333333333334259, 0.3333333333333334259, 0.3333333333333333703, 0.3333333333333332593, 0.3333333333333333703, 0.3333333333333333703, 0.3333333333333333703, 0.3333333333333333148, 0.3333333333333333703, 0.3333333333333332593, 0.3333333333333334259, 0.3333333333333333703, 0.3333333333333333703),
 ( 0.3333333333333333703, 0.3333333333333333703, 0.3333333333333333703, 0.3333333333333333148, 0.3333333333333334259, 0.3333333333333334814, 0.3333333333333332593, 0.3333333333333332593, 0.3333333333333334814, 0.3333333333333333703, 0.3333333333333333703, 0.3333333333333334259, 0.3333333333333334259, 0.3333333333333334259, 0.3333333333333332593, 0.3333333333333334259, 0.3333333333333334259, 0.3333333333333333703, 0.3333333333333334259, 0.3333333333333332038, 0.3333333333333334259, 0.3333333333333333148, 0.3333333333333334259, 0.3333333333333333703, 0.3333333333333333703, 0.3333333333333334259, 0.3333333333333333148, 0.3333333333333334259, 0.3333333333333333703, 0.3333333333333333703, 0.3333333333333333148, 0.3333333333333334259, 0.3333333333333333703, 0.3333333333333333703, 0.3333333333333333148, 0.3333333333333333148, 0.3333333333333334259, 0.3333333333333333148, 0.3333333333333334259, 0.3333333333333333703, 0.3333333333333333703, 0.3333333333333333703, 0.3333333333333332593, 0.3333333333333334814, 0.3333333333333332593, 0.3333333333333333703, 0.3333333333333333703, 0.3333333333333333703, 0.3333333333333335369, 0.3333333333333332593, 0.3333333333333333703, 0.3333333333333335369, 0.3333333333333333703, 0.3333333333333333703, 0.3333333333333335369, 0.3333333333333333703, 0.3333333333333334259, 0.3333333333333334259, 0.3333333333333333703, 0.3333333333333333703, 0.3333333333333333703, 0.3333333333333333703, 0.3333333333333333703, 0.3333333333333333148, 0.3333333333333334259, 0.3333333333333334814, 0.3333333333333333148, 0.3333333333333333703, 0.3333333333333333148, 0.3333333333333334259, 0.3333333333333332593, 0.3333333333333334259, 0.3333333333333333703, 0.3333333333333334259, 0.3333333333333333703, 0.3333333333333333703, 0.3333333333333333703, 0.3333333333333333148, 0.3333333333333334814, 0.3333333333333332038, 0.3333333333333334259, 0.3333333333333334259, 0.3333333333333333148, 0.3333333333333334259, 0.3333333333333333703, 0.3333333333333333148, 0.3333333333333333703, 0.3333333333333333148, 0.3333333333333334814, 0.3333333333333333148, 0.3333333333333333148, 0.3333333333333334259, 0.3333333333333333148, 0.3333333333333333148, 0.3333333333333334814, 0.3333333333333333148, 0.3333333333333334259, 0.3333333333333333703, 0.3333333333333333148, 0.3333333333333333703, 0.3333333333333334259, 0.3333333333333333148, 0.3333333333333334259, 0.3333333333333333148, 0.3333333333333333703, 0.3333333333333333148, 0.3333333333333333703, 0.3333333333333333703, 0.3333333333333333148, 0.3333333333333334259, 0.3333333333333334259, 0.3333333333333333148, 0.3333333333333333703, 0.3333333333333333703, 0.3333333333333334259, 0.3333333333333333703, 0.3333333333333333703, 0.3333333333333334259, 0.3333333333333333703, 0.3333333333333334259, 0.3333333333333333148, 0.3333333333333333703, 0.3333333333333333148, 0.3333333333333335369, 0.3333333333333333148, 0.3333333333333335369, 0.3333333333333333703, 0.3333333333333332593, 0.3333333333333334259, 0.3333333333333334259, 0.3333333333333333148, 0.3333333333333333703, 0.3333333333333333148, 0.3333333333333335369, 0.3333333333333333148, 0.3333333333333333703, 0.3333333333333333703, 0.3333333333333334259, 0.3333333333333334259, 0.3333333333333333703, 0.3333333333333334259, 0.3333333333333332593, 0.3333333333333334814, 0.3333333333333333148, 0.3333333333333333703, 0.3333333333333333148, 0.3333333333333333148, 0.3333333333333334259, 0.3333333333333332593, 0.3333333333333333148, 0.3333333333333333703, 0.3333333333333333148, 0.3333333333333333703, 0.3333333333333334259, 0.3333333333333333703, 0.3333333333333334259, 0.3333333333333333148, 0.3333333333333333703, 0.3333333333333333703, 0.3333333333333333703, 0.3333333333333333148, 0.3333333333333335369, 0.3333333333333333148, 0.3333333333333333703, 0.3333333333333333148, 0.3333333333333334259, 0.3333333333333334259, 0.3333333333333333703, 0.3333333333333334259, 0.3333333333333333703, 0.3333333333333333703, 0.3333333333333334259, 0.3333333333333333703, 0.3333333333333333703, 0.3333333333333333703, 0.3333333333333334259, 0.3333333333333333148, 0.3333333333333333148, 0.3333333333333335369, 0.3333333333333333148, 0.3333333333333334259, 0.3333333333333333148, 0.3333333333333334259, 0.3333333333333333703, 0.3333333333333333148, 0.3333333333333333148, 0.3333333333333333703, 0.3333333333333333148, 0.3333333333333334259, 0.3333333333333334259, 0.3333333333333332038, 0.3333333333333335369, 0.3333333333333333703, 0.3333333333333334259, 0.3333333333333334259, 0.3333333333333333703, 0.3333333333333334259, 0.3333333333333332593, 0.3333333333333334814, 0.3333333333333333703, 0.3333333333333334259, 0.3333333333333333148, 0.3333333333333333148, 0.3333333333333335369, 0.3333333333333332593, 0.3333333333333333703, 0.3333333333333332593, 0.3333333333333335369, 0.3333333333333333703, 0.3333333333333333703, 0.3333333333333333703, 0.3333333333333334259, 0.3333333333333332593, 0.3333333333333334814, 0.3333333333333332593, 0.3333333333333333703, 0.3333333333333333703, 0.3333333333333333703, 0.3333333333333334259, 0.3333333333333333148, 0.3333333333333334259, 0.3333333333333334259, 0.3333333333333333703, 0.3333333333333333148, 0.3333333333333334259, 0.3333333333333333148, 0.3333333333333333703, 0.3333333333333333148, 0.3333333333333333703, 0.3333333333333333703, 0.3333333333333333148, 0.3333333333333333703, 0.3333333333333333703, 0.3333333333333333703, 0.3333333333333334259, 0.3333333333333333703, 0.3333333333333333703, 0.3333333333333334814, 0.3333333333333332593, 0.3333333333333333703, 0.3333333333333334259, 0.3333333333333333148, 0.3333333333333334259, 0.3333333333333333703, 0.3333333333333334814, 0.3333333333333333703, 0.3333333333333333148, 0.3333333333333334259, 0.3333333333333333703, 0.3333333333333333703, 0.3333333333333333703, 0.3333333333333334259, 0.3333333333333333148, 0.3333333333333334259, 0.3333333333333333148, 0.3333333333333333148, 0.3333333333333335369, 0.3333333333333332038, 0.3333333333333335369, 0.3333333333333333148, 0.3333333333333333703, 0.3333333333333334259, 0.3333333333333333703, 0.3333333333333333148, 0.3333333333333333703, 0.3333333333333334259, 0.3333333333333333703, 0.3333333333333334259, 0.3333333333333333148, 0.3333333333333333703, 0.3333333333333334259, 0.3333333333333333148, 0.3333333333333333703, 0.3333333333333333703, 0.3333333333333333148, 0.3333333333333334259, 0.3333333333333334259, 0.3333333333333333703, 0.3333333333333335369, 0.3333333333333333148, 0.3333333333333333703, 0.3333333333333333703, 0.3333333333333333148, 0.3333333333333333703, 0.3333333333333333703, 0.3333333333333333703, 0.3333333333333333148, 0.3333333333333333703, 0.3333333333333334814, 0.3333333333333333703, 0.3333333333333333703, 0.3333333333333335369, 0.3333333333333333703, 0.3333333333333333703, 0.3333333333333334259, 0.3333333333333334259, 0.3333333333333333703, 0.3333333333333333703, 0.3333333333333333703, 0.3333333333333333703, 0.3333333333333333148, 0.3333333333333334259, 0.3333333333333333703, 0.3333333333333333703, 0.3333333333333333703, 0.3333333333333333148, 0.3333333333333334814, 0.3333333333333333148, 0.3333333333333333148, 0.3333333333333334814, 0.3333333333333333148, 0.3333333333333333148, 0.3333333333333334259, 0.3333333333333333148, 0.3333333333333334259, 0.3333333333333333148, 0.3333333333333334259, 0.3333333333333332593, 0.3333333333333335369, 0.3333333333333333148, 0.3333333333333333148, 0.3333333333333334259, 0.3333333333333333703, 0.3333333333333333703, 0.3333333333333333148, 0.3333333333333334259, 0.3333333333333333148, 0.3333333333333334259, 0.3333333333333333148, 0.3333333333333334259, 0.3333333333333334259, 0.3333333333333333703, 0.3333333333333334259, 0.3333333333333333703, 0.3333333333333333703, 0.3333333333333334259, 0.3333333333333333148, 0.3333333333333335369, 0.3333333333333334259, 0.3333333333333333148, 0.3333333333333333703, 0.3333333333333333148, 0.3333333333333334814, 0.3333333333333333703, 0.3333333333333333703, 0.3333333333333332593, 0.3333333333333334814, 0.3333333333333333703, 0.3333333333333333148, 0.3333333333333334259, 0.3333333333333332593, 0.3333333333333334814, 0.3333333333333333703, 0.3333333333333334259, 0.3333333333333333703, 0.3333333333333333148, 0.3333333333333333703, 0.3333333333333334259, 0.3333333333333333703, 0.3333333333333334259, 0.3333333333333333703, 0.3333333333333333703, 0.3333333333333333148, 0.3333333333333333148, 0.3333333333333333703, 0.3333333333333333703, 0.3333333333333333703, 0.3333333333333333703, 0.3333333333333333703, 0.3333333333333333148, 0.3333333333333334814, 0.3333333333333333148, 0.3333333333333334814, 0.3333333333333333703, 0.3333333333333334259, 0.3333333333333334259, 0.3333333333333333703, 0.3333333333333332593, 0.3333333333333333703, 0.3333333333333333703, 0.3333333333333333703, 0.3333333333333333148, 0.3333333333333333703, 0.3333333333333332593, 0.3333333333333334259, 0.3333333333333333703, 0.3333333333333333703),
 ( 1.000000000000000000, 1.000000000000000000, 1.000000000000000000, 0.9999999999999997780, 1.000000000000000000, 1.000000000000000444, 0.9999999999999996669, 0.9999999999999996669, 1.000000000000000444, 1.000000000000000000, 1.000000000000000000, 1.000000000000000000, 1.000000000000000222, 1.000000000000000222, 0.9999999999999997780, 1.000000000000000000, 1.000000000000000222, 1.000000000000000000, 1.000000000000000222, 0.9999999999999994449, 1.000000000000000222, 0.9999999999999997780, 1.000000000000000444, 1.000000000000000000, 1.000000000000000000, 1.000000000000000222, 0.9999999999999997780, 1.000000000000000222, 1.000000000000000000, 1.000000000000000222, 0.9999999999999997780, 1.000000000000000000, 1.000000000000000000, 0.9999999999999997780, 1.000000000000000000, 1.000000000000000000, 1.000000000000000222, 1.000000000000000000, 0.9999999999999997780, 1.000000000000000222, 0.9999999999999997780, 1.000000000000000000, 0.9999999999999997780, 1.000000000000000444, 0.9999999999999996669, 1.000000000000000222, 1.000000000000000000, 1.000000000000000000, 1.000000000000000444, 0.9999999999999996669, 1.000000000000000222, 1.000000000000000444, 1.000000000000000000, 0.9999999999999997780, 1.000000000000000444, 1.000000000000000222, 1.000000000000000000, 1.000000000000000000, 1.000000000000000222, 1.000000000000000000, 1.000000000000000222, 0.9999999999999997780, 1.000000000000000222, 1.000000000000000000, 1.000000000000000000, 1.000000000000000444, 0.9999999999999996669, 1.000000000000000000, 0.9999999999999997780, 1.000000000000000222, 0.9999999999999996669, 1.000000000000000000, 1.000000000000000222, 0.9999999999999997780, 1.000000000000000444, 0.9999999999999997780, 1.000000000000000000, 0.9999999999999997780, 1.000000000000000222, 0.9999999999999996669, 1.000000000000000000, 1.000000000000000222, 0.9999999999999996669, 1.000000000000000444, 0.9999999999999997780, 1.000000000000000000, 1.000000000000000222, 0.9999999999999996669, 1.000000000000000222, 1.000000000000000000, 0.9999999999999997780, 1.000000000000000222, 0.9999999999999997780, 1.000000000000000000, 1.000000000000000222, 0.9999999999999997780, 1.000000000000000000, 1.000000000000000000, 0.9999999999999997780, 1.000000000000000000, 1.000000000000000222, 0.9999999999999997780, 1.000000000000000000, 1.000000000000000000, 1.000000000000000000, 0.9999999999999997780, 1.000000000000000222, 0.9999999999999997780, 0.9999999999999997780, 1.000000000000000444, 1.000000000000000000, 1.000000000000000000, 0.9999999999999997780, 1.000000000000000222, 1.000000000000000000, 1.000000000000000000, 1.000000000000000000, 1.000000000000000000, 1.000000000000000222, 1.000000000000000222, 0.9999999999999997780, 1.000000000000000000, 0.9999999999999997780, 1.000000000000000444, 0.9999999999999996669, 1.000000000000000666, 1.000000000000000000, 0.9999999999999997780, 1.000000000000000222, 1.000000000000000000, 1.000000000000000000, 1.000000000000000000, 0.9999999999999994449, 1.000000000000000666, 0.9999999999999996669, 1.000000000000000000, 1.000000000000000222, 0.9999999999999997780, 1.000000000000000222, 0.9999999999999997780, 1.000000000000000222, 0.9999999999999996669, 1.000000000000000444, 1.000000000000000000, 1.000000000000000222, 0.9999999999999996669, 1.000000000000000000, 1.000000000000000222, 0.9999999999999997780, 1.000000000000000000, 0.9999999999999997780, 1.000000000000000000, 1.000000000000000000, 1.000000000000000222, 0.9999999999999997780, 1.000000000000000222, 0.9999999999999997780, 1.000000000000000000, 1.000000000000000000, 1.000000000000000222, 0.9999999999999997780, 1.000000000000000444, 1.000000000000000000, 0.9999999999999997780, 1.000000000000000000, 1.000000000000000000, 1.000000000000000222, 0.9999999999999997780, 1.000000000000000222, 1.000000000000000000, 1.000000000000000000, 1.000000000000000000, 1.000000000000000222, 1.000000000000000000, 0.9999999999999997780, 1.000000000000000000, 1.000000000000000000, 1.000000000000000000, 1.000000000000000444, 0.9999999999999996669, 1.000000000000000222, 1.000000000000000000, 1.000000000000000222, 0.9999999999999997780, 1.000000000000000000, 0.9999999999999997780, 1.000000000000000000, 0.9999999999999997780, 1.000000000000000000, 1.000000000000000444, 0.9999999999999994449, 1.000000000000000444, 1.000000000000000000, 1.000000000000000222, 1.000000000000000222, 0.9999999999999997780, 1.000000000000000222, 0.9999999999999997780, 1.000000000000000222, 1.000000000000000222, 1.000000000000000222, 0.9999999999999997780, 1.000000000000000000, 1.000000000000000444, 0.9999999999999996669, 1.000000000000000000, 0.9999999999999997780, 1.000000000000000222, 1.000000000000000222, 1.000000000000000000, 0.9999999999999997780, 1.000000000000000222, 0.9999999999999997780, 1.000000000000000222, 0.9999999999999997780, 0.9999999999999997780, 1.000000000000000000, 1.000000000000000000, 1.000000000000000000, 1.000000000000000000, 1.000000000000000000, 1.000000000000000222, 1.000000000000000000, 1.000000000000000000, 1.000000000000000222, 1.000000000000000000, 0.9999999999999997780, 1.000000000000000000, 1.000000000000000000, 1.000000000000000000, 0.9999999999999997780, 1.000000000000000000, 0.9999999999999997780, 1.000000000000000000, 1.000000000000000222, 0.9999999999999996669, 1.000000000000000444, 1.000000000000000000, 0.9999999999999997780, 1.000000000000000222, 1.000000000000000000, 0.9999999999999997780, 1.000000000000000222, 1.000000000000000000, 1.000000000000000222, 1.000000000000000000, 0.9999999999999997780, 1.000000000000000222, 1.000000000000000000, 1.000000000000000000, 1.000000000000000222, 1.000000000000000000, 1.000000000000000000, 1.000000000000000222, 0.9999999999999997780, 0.9999999999999996669, 1.000000000000000444, 0.9999999999999994449, 1.000000000000000444, 0.9999999999999997780, 1.000000000000000222, 1.000000000000000000, 1.000000000000000000, 1.000000000000000000, 1.000000000000000000, 1.000000000000000444, 0.9999999999999996669, 1.000000000000000444, 1.000000000000000000, 0.9999999999999997780, 1.000000000000000444, 0.9999999999999994449, 1.000000000000000444, 0.9999999999999997780, 0.9999999999999997780, 1.000000000000000222, 1.000000000000000444, 0.9999999999999997780, 1.000000000000000444, 0.9999999999999997780, 1.000000000000000000, 1.000000000000000444, 0.9999999999999997780, 0.9999999999999997780, 1.000000000000000000, 1.000000000000000000, 1.000000000000000000, 0.9999999999999997780, 1.000000000000000444, 1.000000000000000222, 0.9999999999999997780, 1.000000000000000444, 1.000000000000000000, 1.000000000000000222, 1.000000000000000000, 1.000000000000000000, 1.000000000000000222, 0.9999999999999997780, 1.000000000000000222, 1.000000000000000222, 0.9999999999999997780, 1.000000000000000222, 1.000000000000000000, 1.000000000000000000, 1.000000000000000222, 0.9999999999999997780, 1.000000000000000444, 0.9999999999999997780, 0.9999999999999997780, 1.000000000000000222, 0.9999999999999997780, 1.000000000000000000, 1.000000000000000000, 0.9999999999999997780, 1.000000000000000222, 0.9999999999999996669, 1.000000000000000444, 0.9999999999999997780, 1.000000000000000222, 1.000000000000000222, 0.9999999999999997780, 1.000000000000000222, 0.9999999999999997780, 1.000000000000000000, 0.9999999999999997780, 1.000000000000000444, 0.9999999999999996669, 1.000000000000000222, 0.9999999999999996669, 1.000000000000000444, 1.000000000000000000, 0.9999999999999997780, 1.000000000000000222, 0.9999999999999996669, 1.000000000000000222, 1.000000000000000222, 0.9999999999999996669, 1.000000000000000444, 1.000000000000000222, 0.9999999999999997780, 1.000000000000000222, 0.9999999999999997780, 1.000000000000000222, 1.000000000000000000, 1.000000000000000222, 0.9999999999999996669, 1.000000000000000444, 1.000000000000000000, 1.000000000000000000, 1.000000000000000222, 0.9999999999999997780, 0.9999999999999997780, 1.000000000000000444, 1.000000000000000000, 1.000000000000000000, 0.9999999999999996669, 1.000000000000000000, 1.000000000000000222, 1.000000000000000000, 1.000000000000000000, 1.000000000000000222, 0.9999999999999997780, 1.000000000000000000, 0.9999999999999997780, 0.9999999999999997780, 1.000000000000000222, 0.9999999999999997780, 1.000000000000000000, 1.000000000000000000, 0.9999999999999997780, 1.000000000000000222, 1.000000000000000000, 1.000000000000000222, 1.000000000000000000, 1.000000000000000444, 1.000000000000000000, 1.000000000000000000, 0.9999999999999997780, 0.9999999999999997780, 1.000000000000000222, 1.000000000000000000, 1.000000000000000000, 1.000000000000000000, 0.9999999999999997780, 1.000000000000000222, 1.000000000000000000, 1.000000000000000000) ) ) 
 REPRESENTATION_ITEM ( '' )  SURFACE ( )  );
#124800 = ORIENTED_EDGE ( 'NONE', *, *, #120795, .T. ) ;
#124801 = CARTESIAN_POINT ( 'NONE',  ( 0.7308274648059713829, -1.853293357156562404, -0.6670056901108140091 ) ) ;
#124802 = CARTESIAN_POINT ( 'NONE',  ( 2.296341162515431744, 1.558512652156778699, -1.158513924970270059 ) ) ;
#124803 = EDGE_LOOP ( 'NONE', ( #39362, #67931, #177736, #170658 ) ) ;
#124804 = DIRECTION ( 'NONE',  ( 0.2684563758389304500, -5.821219718043054220E-15, -0.9632918427306581544 ) ) ;
#124806 = CARTESIAN_POINT ( 'NONE',  ( 6.702007135557183304, 0.7127468228822000373, -1.719244972783180225 ) ) ;
#124805 = CARTESIAN_POINT ( 'NONE',  ( -5.991777542596674166, 5.955104985976372944, 0.000000000000000000 ) ) ;
#124807 = CARTESIAN_POINT ( 'NONE',  ( 4.980641328173811999, 6.904110530993182948, 1.599625672291269396 ) ) ;
#124808 = CARTESIAN_POINT ( 'NONE',  ( 8.723781775389312543, 12.26516360700784958, -1.199719254218446718 ) ) ;
#124809 = CARTESIAN_POINT ( 'NONE',  ( -6.180537922983287302, 8.303989891604203422, -1.599625672291271394 ) ) ;
#124810 = CARTESIAN_POINT ( 'NONE',  ( 3.034921719543516971, -1.931671641359738567, 1.035203715903771915 ) ) ;
#124811 = CARTESIAN_POINT ( 'NONE',  ( 10.99968117833243042, -6.698521824825881765, -0.09510031644102620585 ) ) ;
#124812 = DIRECTION ( 'NONE',  ( 5.176899690512889097E-31, -0.6000000000000018652, -0.7999999999999984901 ) ) ;
#124813 = CARTESIAN_POINT ( 'NONE',  ( 2.859763506297557711, 1.816872213737670938, -0.1792109616642542924 ) ) ;
#124814 = CARTESIAN_POINT ( 'NONE',  ( -4.274898507010545856, 3.881803101134051470, -0.7998128361456221525 ) ) ;
#124815 = CARTESIAN_POINT ( 'NONE',  ( -4.882431421883429046, 8.154724402237897962, -1.012048471081774093 ) ) ;
#124816 = CARTESIAN_POINT ( 'NONE',  ( 7.079328764629950754, 11.41096732537697633, 0.7998128361456462443 ) ) ;
#124817 = CARTESIAN_POINT ( 'NONE',  ( 1.119610834840406577, -1.879747399699664978, 0.4211694731556160365 ) ) ;
#124818 = CARTESIAN_POINT ( 'NONE',  ( 5.401206054008879320, -1.684469800357458302, 1.005230755432365175 ) ) ;
#124819 = CARTESIAN_POINT ( 'NONE',  ( 0.7500000000000006661, 15.08333333333333748, 1.299038105676657340 ) ) ;
#124820 = CARTESIAN_POINT ( 'NONE',  ( -6.527360889975461156, 9.702672574024962415, 1.199719254218452047 ) ) ;
#124821 = CARTESIAN_POINT ( 'NONE',  ( 5.229694566569264680, 7.124396299129368337, 1.599625672291267398 ) ) ;
#124822 = CARTESIAN_POINT ( 'NONE',  ( 4.476244563333130699, -2.125884358948509689, -0.5320566845071761364 ) ) ;
#124823 = DIRECTION ( 'NONE',  ( -0.2636425362803287986, 0.9646204502620061572, 0.000000000000000000 ) ) ;
#124824 = CARTESIAN_POINT ( 'NONE',  ( -2.819732761962335577, 5.273143408055916304, -1.082531754730543971 ) ) ;
#124825 = CARTESIAN_POINT ( 'NONE',  ( 5.559458666840932928, 1.689222788819956245, 1.196583256836199149 ) ) ;
#124827 = CARTESIAN_POINT ( 'NONE',  ( -0.6823417656250212460, 2.613541667008084879, 1.181850606188767472 ) ) ;
#124826 = SURFACE_STYLE_USAGE ( .BOTH. , #29383 ) ;
#124828 = CARTESIAN_POINT ( 'NONE',  ( 4.852278370791485607, 0.2271405875100707961, -2.287421213010778942 ) ) ;
#124829 = CARTESIAN_POINT ( 'NONE',  ( 6.236387472606139681, 8.298871356172400127, -1.443375672974057666 ) ) ;
#124831 = CARTESIAN_POINT ( 'NONE',  ( 1.286956418854593442, 3.612814789603055132, 0.5511290012047642684 ) ) ;
#124830 = CARTESIAN_POINT ( 'NONE',  ( 6.075462232699553766, 6.260663157670496304, -0.7216878364870458196 ) ) ;
#124832 = CARTESIAN_POINT ( 'NONE',  ( 0.09422489544355044933, -2.291893678819735491, -0.04953789299679511871 ) ) ;
#124833 = CARTESIAN_POINT ( 'NONE',  ( -7.661067326845563130, -5.325441678136415113, -7.893838479094846150 ) ) ;
#124834 = CARTESIAN_POINT ( 'NONE',  ( -5.088052786878465739, 9.158088361325352977, 0.000000000000000000 ) ) ;
#124835 = CARTESIAN_POINT ( 'NONE',  ( 4.927648248775200912, 0.9969592527751047761, -1.666372862991059245 ) ) ;
#124836 = ORIENTED_EDGE ( 'NONE', *, *, #122827, .T. ) ;
#124837 = CARTESIAN_POINT ( 'NONE',  ( 8.663296969007976855, 12.09063498294259809, -1.082531754730543083 ) ) ;
#124838 = ORIENTED_EDGE ( 'NONE', *, *, #52342, .T. ) ;
#124839 = CARTESIAN_POINT ( 'NONE',  ( 5.660397963661894849, 1.910509065610028090, 0.08734628876111423523 ) ) ;
#124840 = CARTESIAN_POINT ( 'NONE',  ( 6.247054435025749086, -1.454095476552646593, 0.9272665607438534963 ) ) ;
#124841 = CARTESIAN_POINT ( 'NONE',  ( 5.524625123954316486, 0.3981063221985549072, 1.976670730632006601 ) ) ;
#124843 = CARTESIAN_POINT ( 'NONE',  ( -11.94654170777226021, 12.44825673841064173, 1.134972293687618539 ) ) ;
#124842 = CARTESIAN_POINT ( 'NONE',  ( -9.179033691651859783, 10.66762638080401260, 1.199719254218462483 ) ) ;
#124844 = CARTESIAN_POINT ( 'NONE',  ( -3.285556943750000070, -1.246874999522043392, 0.000000000000000000 ) ) ;
#124846 = CARTESIAN_POINT ( 'NONE',  ( 0.6019893773144822102, -0.5904995772347610972, -1.668576399176853853 ) ) ;
#124845 = CARTESIAN_POINT ( 'NONE',  ( 1.992240001063511290, -0.5588421479580056861, -2.014483121414586186 ) ) ;
#124847 = CARTESIAN_POINT ( 'NONE',  ( 5.748672702226536479, 1.986101125435947301, -0.3474646712962395911 ) ) ;
#124848 = ADVANCED_FACE ( 'NONE', ( #50560 ), #192374, .F. ) ;
#124850 = CARTESIAN_POINT ( 'NONE',  ( 2.748291532463055020, 0.7732563850255981253, 2.158024254592408209 ) ) ;
#124849 = CARTESIAN_POINT ( 'NONE',  ( 5.896870467300973750, 5.844380064798101237, 0.7998128361456352531 ) ) ;
#124851 = CARTESIAN_POINT ( 'NONE',  ( 1.974151807821213245, -0.08369685440555743594, -1.738446472377056740 ) ) ;
#124852 = B_SPLINE_CURVE_WITH_KNOTS ( 'NONE', 3,
 ( #88695, #54050, #21507, #5256, #71332, #163026, #160887, #14609, #159812, #111131 ),
 .UNSPECIFIED., .F., .F.,
 ( 4, 2, 2, 2, 4 ),
 ( 0.000000000000000000, 0.0003432858056828389979, 0.0006865716113656779957, 0.001029857417048516939, 0.001373143222731355991 ),
 .UNSPECIFIED. ) ;
#124853 = AXIS2_PLACEMENT_3D ( 'NONE', #109596, #62891, #175602 ) ;
#124854 = CARTESIAN_POINT ( 'NONE',  ( 1.333315192109769454, 8.250054423670803772, 10.85938449304425113 ) ) ;
#124855 = CARTESIAN_POINT ( 'NONE',  ( 2.741176079829604539, -1.657949034129829302, -0.5072451560675111937 ) ) ;
#124856 = CARTESIAN_POINT ( 'NONE',  ( -1.360316468750026653, 2.192708333674788346, 0.7853790794158680422 ) ) ;
#124857 = CARTESIAN_POINT ( 'NONE',  ( 1.715070751487054013, -1.593955780799067412, -0.9604075334226671590 ) ) ;
#124858 = CARTESIAN_POINT ( 'NONE',  ( 2.506498380571024143, 2.170641363890627229, 0.05523593993728668355 ) ) ;
#124859 = CARTESIAN_POINT ( 'NONE',  ( 4.012907874177486178, 0.1037781579101039742, 2.014008197856680393 ) ) ;
#124860 = CARTESIAN_POINT ( 'NONE',  ( 4.156250000000002665, -1.895863743163992199, 0.7852924748302037017 ) ) ;
#124861 = CARTESIAN_POINT ( 'NONE',  ( 1.499999999999987121, 1.285416667349485120, 0.8660254037844524744 ) ) ;
#124862 = CARTESIAN_POINT ( 'NONE',  ( 0.5867820057828515568, -0.2326963965399355405, -1.912219011898611765 ) ) ;
#124863 = CARTESIAN_POINT ( 'NONE',  ( 0.6823417656249969321, 14.27604166700806232, -1.181850606188757036 ) ) ;
#124864 = CARTESIAN_POINT ( 'NONE',  ( 3.779691724966814270, 0.2693221142107836696, -2.204936161957889329 ) ) ;
#124865 = VERTEX_POINT ( 'NONE', #93489 ) ;
#124866 = DIRECTION ( 'NONE',  ( 0.000000000000000000, -1.000000000000000000, 0.000000000000000000 ) ) ;
#124867 = CARTESIAN_POINT ( 'NONE',  ( -1.402160292154681736E-14, 0.4625000000000214495, 1.732050807568877637 ) ) ;
#124868 = CARTESIAN_POINT ( 'NONE',  ( 6.591235234537977661, 10.84152487360300299, 0.7998128361456462443 ) ) ;
#124869 = CARTESIAN_POINT ( 'NONE',  ( -1.364683531250014514, -0.7614583329919104582, -0.7879004041258359514 ) ) ;
#124870 = CARTESIAN_POINT ( 'NONE',  ( 5.906509255234578148, -2.210603606603298132, -0.2184946463264207661 ) ) ;
#124872 = CARTESIAN_POINT ( 'NONE',  ( 4.562918044398325712, 1.517878595006398212, -1.242988302126393663 ) ) ;
#124871 = MECHANICAL_DESIGN_GEOMETRIC_PRESENTATION_REPRESENTATION (  '', ( #190472 ), #93734 ) ;
#124874 = CARTESIAN_POINT ( 'NONE',  ( -6.317736394288148816, 8.393778431468064127, 1.443375672974078761 ) ) ;
#124873 = CARTESIAN_POINT ( 'NONE',  ( 8.270110514656016321, 12.59228666716665401, 0.7216878364870438212 ) ) ;
#124875 = CARTESIAN_POINT ( 'NONE',  ( -1.265302052550098200, 3.778627107522626094, -0.4993130731308045300 ) ) ;
#124876 = CARTESIAN_POINT ( 'NONE',  ( 5.817715961848279882, -2.209163325107537101, 0.4873710261694869095 ) ) ;
#124877 = B_SPLINE_CURVE_WITH_KNOTS ( 'NONE', 3,
 ( #73084, #90439, #106729, #141358 ),
 .UNSPECIFIED., .F., .F.,
 ( 4, 4 ),
 ( 1.113895128243735996E-15, 8.505390839970735750E-05 ),
 .UNSPECIFIED. ) ;
#124878 = CARTESIAN_POINT ( 'NONE',  ( -6.048345925472225382, 8.149765894507963182, 1.443375672974058777 ) ) ;
#124879 = CARTESIAN_POINT ( 'NONE',  ( 1.838405449727827268, -1.105357634037696046, 1.741336484761913272 ) ) ;
#124880 = CARTESIAN_POINT ( 'NONE',  ( -6.124532705071231931, 8.168374127381657246, -1.599625672291263179 ) ) ;
#124881 = EDGE_CURVE ( 'NONE', #1738, #132613, #81571, .T. ) ;
#124882 = ORIENTED_EDGE ( 'NONE', *, *, #187512, .F. ) ;
#124883 = CARTESIAN_POINT ( 'NONE',  ( 0.7499999999999885647, 2.097916667349486453, -1.299038105676652899 ) ) ;
#124884 = CARTESIAN_POINT ( 'NONE',  ( -1.201851678989727383E-14, 3.759375000341422801, -1.575800808251660134 ) ) ;
#124885 = CARTESIAN_POINT ( 'NONE',  ( 4.077312411328878561, 1.762187477035919603, -0.6278270876356045749 ) ) ;
#124886 = CARTESIAN_POINT ( 'NONE',  ( 3.058897358425614055, -1.030606816589432873, 1.394497854932384762 ) ) ;
#124887 = CARTESIAN_POINT ( 'NONE',  ( 0.02941885139840036759, -2.092310700284722103, 0.9370380844745775928 ) ) ;
#124888 = CARTESIAN_POINT ( 'NONE',  ( 1.220068447022312652, -2.152735442661047216, 0.4846846590640523367 ) ) ;
#124889 = CARTESIAN_POINT ( 'NONE',  ( 4.388279639374990104, -0.4598052185818923832, -2.039381826187444791 ) ) ;
#124890 = CARTESIAN_POINT ( 'NONE',  ( 5.648367429523982963, -1.529681991043756017, 1.196244224141077561 ) ) ;
#124892 = ORIENTED_EDGE ( 'NONE', *, *, #13749, .F. ) ;
#124891 = DIRECTION ( 'NONE',  ( 0.000000000000000000, 1.485208455459594811E-16, -1.000000000000000000 ) ) ;
#124893 = CARTESIAN_POINT ( 'NONE',  ( 0.2812500008225146120, 0.7852924545924094835, 1.895863743164083681 ) ) ;
#124894 = CARTESIAN_POINT ( 'NONE',  ( 0.01820432788856435335, -1.842448466851685840, 0.8197770699841927522 ) ) ;
#124895 = CARTESIAN_POINT ( 'NONE',  ( -1.665334536937729880E-16, 0.000000000000000000, 3.000000000000000444 ) ) ;
#124896 = DIRECTION ( 'NONE',  ( 0.000000000000000000, 0.000000000000000000, 1.000000000000000000 ) ) ;
#124897 = SURFACE_STYLE_FILL_AREA ( #27296 ) ;
#124898 = CARTESIAN_POINT ( 'NONE',  ( -7.720478407978036195, 11.09464301169468037, -1.199719254218446718 ) ) ;
#124899 = CARTESIAN_POINT ( 'NONE',  ( 8.132193210098487057, 8.381980254736715708, 1.040834085586084257E-14 ) ) ;
#124900 = CYLINDRICAL_SURFACE ( 'NONE', #187822, 10.25000000000000000 ) ;
#124901 = CARTESIAN_POINT ( 'NONE',  ( 4.512205841073367196, -0.7830535718562798841, -1.649371741558727678 ) ) ;
#124902 = CARTESIAN_POINT ( 'NONE',  ( 1.887996149947854807, 1.521953097117642706, 1.598203399828190152 ) ) ;
#124903 = ORIENTED_EDGE ( 'NONE', *, *, #39920, .T. ) ;
#124904 = CARTESIAN_POINT ( 'NONE',  ( -6.583366107887490770, 9.838288338247510367, 1.199719254218452935 ) ) ;
#124905 = CARTESIAN_POINT ( 'NONE',  ( -1.642778471874998480, -2.238541666188708312, 2.845375778867863303 ) ) ;
#124906 = CARTESIAN_POINT ( 'NONE',  ( -7.157815033010924921, 10.43820240756634199, 1.199719254218453823 ) ) ;
#124907 = CARTESIAN_POINT ( 'NONE',  ( 1.371359653073561891, -1.734546099648653472, -1.034550878434212784 ) ) ;
#124908 = CARTESIAN_POINT ( 'NONE',  ( -9.898321827453750998, 15.00000000001253753, -7.924999999985899990 ) ) ;
#124909 = CARTESIAN_POINT ( 'NONE',  ( -3.800028193580205382, 7.655393002477360653, -0.7998128361456481317 ) ) ;
#124910 = CARTESIAN_POINT ( 'NONE',  ( 2.975287861635074194, -0.1872683251897942214, 1.851525965346143554 ) ) ;
#124911 = CARTESIAN_POINT ( 'NONE',  ( 4.566398809704347528, 4.221886787610169556, -0.7998128361456211532 ) ) ;
#124912 = CARTESIAN_POINT ( 'NONE',  ( -4.911894908834722351, 4.738238661368090909, 0.4458799699701230246 ) ) ;
#124913 = ORIENTED_EDGE ( 'NONE', *, *, #207112, .T. ) ;
#124914 = CARTESIAN_POINT ( 'NONE',  ( -4.741601036477307574, 6.554953847355395880, 1.599625672291267398 ) ) ;
#124915 =( GEOMETRIC_REPRESENTATION_CONTEXT ( 3 ) GLOBAL_UNCERTAINTY_ASSIGNED_CONTEXT ( ( #80768 ) ) GLOBAL_UNIT_ASSIGNED_CONTEXT ( ( #78182, #46779, #162650 ) ) REPRESENTATION_CONTEXT ( 'NONE', 'WORKASPACE' ) );
#124916 = CARTESIAN_POINT ( 'NONE',  ( -9.169391961543940539, 9.592045464756413509, 1.040834085586084257E-14 ) ) ;
#124917 = CARTESIAN_POINT ( 'NONE',  ( 4.055160972438559774, -1.518969423100406946, -1.012540670841777013 ) ) ;
#124918 = CIRCLE ( 'NONE', #183727, 11.99999999999999112 ) ;
#124920 = CARTESIAN_POINT ( 'NONE',  ( -5.747250929305832479, 6.247137566976777912, -1.064685594968674209 ) ) ;
#124919 = CARTESIAN_POINT ( 'NONE',  ( -4.085803189671902480, 5.860132702740892263, -1.599625672291271394 ) ) ;
#124921 = CARTESIAN_POINT ( 'NONE',  ( 5.862225131719664972, 7.287605523280396902, -1.268052015211480033 ) ) ;
#124922 = CARTESIAN_POINT ( 'NONE',  ( 0.7899210882133401723, -1.648783996043493350, 0.5366646198887611297 ) ) ;
#124923 = CARTESIAN_POINT ( 'NONE',  ( 5.912015133600425187, 1.233162958052456348, -1.367321061651972869 ) ) ;
#124924 = AXIS2_PLACEMENT_3D ( 'NONE', #180564, #3912, #49500 ) ;
#124925 = CARTESIAN_POINT ( 'NONE',  ( 4.494930827260392725, -0.5027447494639860626, -2.252120713733107404 ) ) ;
#124926 = CARTESIAN_POINT ( 'NONE',  ( 6.052789233858158369, 6.026285292448116948, 0.000000000000000000 ) ) ;
#124927 = CARTESIAN_POINT ( 'NONE',  ( 6.643834073375672666, 0.8340821395082242962, -1.994398315854857495 ) ) ;
#124928 = CARTESIAN_POINT ( 'NONE',  ( 7.308008492965924141, 8.484763649003774333, -1.199719254218451159 ) ) ;
#124929 = CARTESIAN_POINT ( 'NONE',  ( 5.501416862357105586, 2.263058191380825424, 0.4008149593560642598 ) ) ;
#124930 = CARTESIAN_POINT ( 'NONE',  ( 5.335766472694954743, 4.384919054141799499, 2.499999999999998668 ) ) ;
#124931 = CARTESIAN_POINT ( 'NONE',  ( -7.587723245503481095, 8.881373870289390737, 1.199719254218452047 ) ) ;
#124932 = CARTESIAN_POINT ( 'NONE',  ( 5.348468966913380029, 0.5439794105128460400, 1.789823788735760646 ) ) ;
#124933 = EDGE_LOOP ( 'NONE', ( #170736, #119328, #103640, #27761 ) ) ;
#124935 = CARTESIAN_POINT ( 'NONE',  ( -4.878955176071358757, 6.785476686873604280, -1.599625672291271394 ) ) ;
#124934 = CARTESIAN_POINT ( 'NONE',  ( 2.707167837304753633, 1.638089068140319071, -0.9866689735503200165 ) ) ;
#124936 = CARTESIAN_POINT ( 'NONE',  ( 3.492985898914053866, -0.4302566696539159574, -2.164365734511737305 ) ) ;
#124937 = CARTESIAN_POINT ( 'NONE',  ( 4.821547164884887771, -1.499609098395672246, -1.495007082409164356 ) ) ;
#124938 = CARTESIAN_POINT ( 'NONE',  ( -0.6125000000000019318, 0.5208333340161186431, -1.060881119635944891 ) ) ;
#124939 = B_SPLINE_CURVE_WITH_KNOTS ( 'NONE', 3,
 ( #201811, #101127, #17725, #2539, #185576, #184507, #103280, #36125 ),
 .UNSPECIFIED., .F., .F.,
 ( 4, 2, 2, 4 ),
 ( 0.000000000000000000, 0.0004365159022975833875, 0.0006547738534463757318, 0.0008730318045951679677 ),
 .UNSPECIFIED. ) ;
#124940 = CARTESIAN_POINT ( 'NONE',  ( 6.983263157960371892, 7.629137130509070275, 2.546189081643289942 ) ) ;
#124941 = CARTESIAN_POINT ( 'NONE',  ( -0.2110808730066962846, 5.724502961415374180, -2.391230805320884834 ) ) ;
#124942 = CARTESIAN_POINT ( 'NONE',  ( 4.543390873910894356, 8.314723429622471684, 0.7216878364870317197 ) ) ;
#124943 = CARTESIAN_POINT ( 'NONE',  ( -3.797692425159308716, 7.444741906078900406, 0.000000000000000000 ) ) ;
#124944 = CARTESIAN_POINT ( 'NONE',  ( 1.975998049093165232, 2.207973392102855925, -0.6707195784038646469 ) ) ;
#124945 = CARTESIAN_POINT ( 'NONE',  ( 2.435929278166943490, 1.204617592564939166, 1.548422000036096202 ) ) ;
#124946 = DIRECTION ( 'NONE',  ( 0.000000000000000000, -1.000000000000000000, 0.000000000000000000 ) ) ;
#124947 = CARTESIAN_POINT ( 'NONE',  ( 6.649293052619501765, 1.797374026962361482, -1.011582863395175114 ) ) ;
#124948 = CARTESIAN_POINT ( 'NONE',  ( 4.853455804012228647, 4.764712647543454693, 0.7216878364870317197 ) ) ;
#124949 = CARTESIAN_POINT ( 'NONE',  ( 3.379725431556547477, 7.165039780116438273, -1.734723475976807094E-15 ) ) ;
#124950 = ORIENTED_EDGE ( 'NONE', *, *, #12835, .T. ) ;
#124951 = CARTESIAN_POINT ( 'NONE',  ( 4.522672878804367969, 0.3494810548456111499, 1.985869246038343583 ) ) ;
#124952 = CARTESIAN_POINT ( 'NONE',  ( -10.13202086811422475, 10.71511252242175161, -0.7998128361456291469 ) ) ;
#124953 = CARTESIAN_POINT ( 'NONE',  ( -0.7500000000000215383, 4.191666666666690411, 1.299038105676671107 ) ) ;
#124954 = CARTESIAN_POINT ( 'NONE',  ( -10.44369633504468631, 5.112959841837461994, -5.232137017608345708 ) ) ;
#124955 = CARTESIAN_POINT ( 'NONE',  ( 10.26082332744404368, 10.86538205830655279, -0.7998128361456281477 ) ) ;
#124956 = CARTESIAN_POINT ( 'NONE',  ( 2.518641040286667465, 0.9249485440519630286, 1.964284900515224530 ) ) ;
#124957 = CARTESIAN_POINT ( 'NONE',  ( 5.285699784481295183, 7.260012063351913625, 1.599625672291268286 ) ) ;
#124958 =( LENGTH_UNIT ( ) NAMED_UNIT ( * ) SI_UNIT ( .MILLI., .METRE. ) );
#124959 = CARTESIAN_POINT ( 'NONE',  ( -3.159872497350062481, 2.806782174840205091, 2.466584723216629360 ) ) ;
#124960 = CARTESIAN_POINT ( 'NONE',  ( 2.354581831802166736, -1.448805955455864769, 1.183207591018392568 ) ) ;
#124961 = CARTESIAN_POINT ( 'NONE',  ( 1.264995835974036975, -1.861883480270887903, -0.8836341380922418942 ) ) ;
#124963 = CARTESIAN_POINT ( 'NONE',  ( 6.727182134110257117, 2.064761932694148872, 2.218145506119094890 ) ) ;
#124962 = DIRECTION ( 'NONE',  ( 1.039099362110107450E-15, 1.000000000000000000, -4.583713267641621330E-32 ) ) ;
#124964 = CARTESIAN_POINT ( 'NONE',  ( -1.402160292154681736E-14, 0.07187500034142156602, 1.575800808251672791 ) ) ;
#124965 = SURFACE_STYLE_FILL_AREA ( #8989 ) ;
#124966 = VERTEX_POINT ( 'NONE', #143324 ) ;
#124967 = CARTESIAN_POINT ( 'NONE',  ( 2.947808941170467545, -1.285945688040548207, -1.415481726668985196 ) ) ;
#124968 = CARTESIAN_POINT ( 'NONE',  ( 5.313276456144085280, -0.2569279779609782155, 1.750970204404985964 ) ) ;
#124969 = CARTESIAN_POINT ( 'NONE',  ( 1.734869227892420707, 1.784761669998648381, 0.6870963898520031643 ) ) ;
#124970 = CARTESIAN_POINT ( 'NONE',  ( -4.416205349749324327, 6.175325546172740765, 1.599625672291267398 ) ) ;
#124972 = CARTESIAN_POINT ( 'NONE',  ( 0.1806861152609346710, 1.591142543434557632, -1.066548322639774504 ) ) ;
#124971 = LINE ( 'NONE', #207192, #35433 ) ;
#124973 = CARTESIAN_POINT ( 'NONE',  ( -1.402160292154681736E-14, -0.03749999999998095135, 1.732050807568877637 ) ) ;
#124974 = CARTESIAN_POINT ( 'NONE',  ( 0.6782873735513493818, -1.106163567672680204, -1.749894625276714688 ) ) ;
#124975 = CARTESIAN_POINT ( 'NONE',  ( -0.7499999999999972244, 5.608333333333353821, -1.299038105676652011 ) ) ;
#124976 = CARTESIAN_POINT ( 'NONE',  ( 5.928550619183988957, 1.803260976426118489, 0.4972845834502263584 ) ) ;
#124977 = CARTESIAN_POINT ( 'NONE',  ( 2.209345402013741300, -0.4006574107652469130, 1.781019818369505847 ) ) ;
#124979 = CARTESIAN_POINT ( 'NONE',  ( 4.594747986498664005, 8.374059380672374431, -0.03693212167796278145 ) ) ;
#124978 = CARTESIAN_POINT ( 'NONE',  ( 5.356176587289051660, 2.204499490778097481, -0.1052899746726426722 ) ) ;
#124980 = EDGE_CURVE ( 'NONE', #149597, #211791, #162041, .T. ) ;
#124981 = CARTESIAN_POINT ( 'NONE',  ( 0.6823417656249882723, 0.3427083336747516196, 1.181850606188755259 ) ) ;
#124982 = CARTESIAN_POINT ( 'NONE',  ( 2.682143534289625375, -1.185536078076434796, -1.687771684069488076 ) ) ;
#124983 = CARTESIAN_POINT ( 'NONE',  ( -7.725448601688521322, 7.907444878258402809, 1.040834085586084257E-14 ) ) ;
#124984 = CARTESIAN_POINT ( 'NONE',  ( 8.751951852821344247, 10.16936423550178503, -1.199719254218446718 ) ) ;
#124985 = CARTESIAN_POINT ( 'NONE',  ( 6.003563092752935759, 5.898578451166879510, 0.7998128361456341429 ) ) ;
#124986 = CIRCLE ( 'NONE', #117996, 0.07999999999999998779 ) ;
#124987 = CARTESIAN_POINT ( 'NONE',  ( 0.4566077865506939504, 0.8268718848777978359, 1.997384878126715391 ) ) ;
#124988 = CARTESIAN_POINT ( 'NONE',  ( 5.559725510055676168, 8.644040974110419384, 1.199719254218451159 ) ) ;
#124989 = CARTESIAN_POINT ( 'NONE',  ( 4.967269779104159788, 1.799668380515653920, 1.023422521214325309 ) ) ;
#124990 = CARTESIAN_POINT ( 'NONE',  ( 1.364683531249986537, -0.07395833299191513499, 0.7879004041258500513 ) ) ;
#124991 = CARTESIAN_POINT ( 'NONE',  ( 2.442841770826277514, 0.4709965094221583159, 2.109507199432036018 ) ) ;
#124992 = CARTESIAN_POINT ( 'NONE',  ( -4.604539980425653489, 8.383423159197839425, -0.07723066608773809794 ) ) ;
#124994 = CARTESIAN_POINT ( 'NONE',  ( 2.207404936347991065, -1.573848641742966459, -1.171066219227391070 ) ) ;
#124993 = CARTESIAN_POINT ( 'NONE',  ( 3.035811672558884400, -1.945802561663440455, 0.5409189654149139104 ) ) ;
#124995 = CARTESIAN_POINT ( 'NONE',  ( 6.620655732516642189, 2.417337544263608251, 2.554705107920357321 ) ) ;
#124996 = PRODUCT_DEFINITION_SHAPE ( 'NONE', 'NONE',  #135165 ) ;
#124997 = EDGE_CURVE ( 'NONE', #71069, #143793, #150856, .T. ) ;
#124999 = CARTESIAN_POINT ( 'NONE',  ( 5.938108093105483931, 8.911247961056314892, -1.082531754730537088 ) ) ;
#124998 = CARTESIAN_POINT ( 'NONE',  ( -3.475000000000000533, -1.049999999999998934, 0.000000000000000000 ) ) ;
#125000 = CARTESIAN_POINT ( 'NONE',  ( -5.420227550413282636, 9.545625585449309725, 0.7998128361456291469 ) ) ;
#125001 = CARTESIAN_POINT ( 'NONE',  ( 0.9543149826918421175, -1.275552737861269437, 1.561884623745241951 ) ) ;
#125003 = CARTESIAN_POINT ( 'NONE',  ( 6.603104432341277530, -0.4828188497946246382, 2.145653685147373313 ) ) ;
#125002 = CARTESIAN_POINT ( 'NONE',  ( -4.042302355168801320, 7.867769847672247074, 0.7998128361456341429 ) ) ;
#125004 = CARTESIAN_POINT ( 'NONE',  ( -1.499999999999997780, 5.900000000000023448, 1.214306433183764966E-14 ) ) ;
#125005 = CARTESIAN_POINT ( 'NONE',  ( 5.888906298306327614, -1.818048641159516254, -0.5935555146628914702 ) ) ;
#125006 = CARTESIAN_POINT ( 'NONE',  ( -2.819205876637805641, 5.376491725131008259, -1.199719254218446718 ) ) ;
#125007 = CARTESIAN_POINT ( 'NONE',  ( 4.921246571636183731, 7.724909519342112674, -1.082531754730549078 ) ) ;
#125009 = CARTESIAN_POINT ( 'NONE',  ( 3.550407796516129366, -1.352142120786763213, 1.496064415113136592 ) ) ;
#125008 = CARTESIAN_POINT ( 'NONE',  ( -8.134528978075012517, 12.43410820782212767, 1.040834085586084257E-14 ) ) ;
#125010 = CARTESIAN_POINT ( 'NONE',  ( 1.499999999999989120, 4.254166666666687746, 0.8660254037844524744 ) ) ;
#125011 = CARTESIAN_POINT ( 'NONE',  ( 1.364683531250000303, 14.06770833367473550, -0.7879004041258355073 ) ) ;
#125012 = CARTESIAN_POINT ( 'NONE',  ( 6.106443901014584341, -0.6257089282217034309, -1.607472872393211683 ) ) ;
#125013 = CARTESIAN_POINT ( 'NONE',  ( 6.550524494058025837, 7.671308660269694712, -1.199719254218452047 ) ) ;
#125014 = CARTESIAN_POINT ( 'NONE',  ( 3.708318708537623021, 4.285125567170706695, -1.199719254218446718 ) ) ;
#125015 = CIRCLE ( 'NONE', #31545, 0.08000000000000030698 ) ;
#125016 = CARTESIAN_POINT ( 'NONE',  ( 10.99861993420630135, -9.955063214563365293, -0.1919715503784026334 ) ) ;
#125017 = CARTESIAN_POINT ( 'NONE',  ( 4.200366636497298245, -0.5845007089231197828, -1.776970133648393624 ) ) ;
#125018 = CARTESIAN_POINT ( 'NONE',  ( 1.220000000000003304, 6.400000000000022560, 1.229247124133362667E-14 ) ) ;
#125019 = CARTESIAN_POINT ( 'NONE',  ( 1.375928118113247445, -2.020660359122231409, 0.4497719141252009556 ) ) ;
#125020 = FACE_OUTER_BOUND ( 'NONE', #202874, .T. ) ;
#125021 = ORIENTED_EDGE ( 'NONE', *, *, #110409, .T. ) ;
#125022 = CARTESIAN_POINT ( 'NONE',  ( 5.228604516725597229, 6.129068686715179126, -1.199719254218450271 ) ) ;
#125024 = ADVANCED_FACE ( 'NONE', ( #6050 ), #109789, .T. ) ;
#125023 = CARTESIAN_POINT ( 'NONE',  ( 0.08751785467620704084, -0.5350655163729299835, 1.944078888069140865 ) ) ;
#125025 = CARTESIAN_POINT ( 'NONE',  ( 0.4393641590584134171, -1.719983824569010444, 0.5688467837753272693 ) ) ;
#125026 = CARTESIAN_POINT ( 'NONE',  ( 6.021229617800532452, 6.197391773621639288, 0.000000000000000000 ) ) ;
#125027 = CARTESIAN_POINT ( 'NONE',  ( 0.1019944501368414136, 2.531386338185347640, -1.997494965961774005 ) ) ;
#125028 = ORIENTED_EDGE ( 'NONE', *, *, #86537, .F. ) ;
#125029 = CARTESIAN_POINT ( 'NONE',  ( 9.693716643646601128, 10.41168362711695750, 0.7216878364870438212 ) ) ;
#125031 = CARTESIAN_POINT ( 'NONE',  ( 6.805303039055573322, 10.02693841461847057, 1.199719254218460707 ) ) ;
#125030 = CARTESIAN_POINT ( 'NONE',  ( 0.8011316787140990714, -1.684513426579350659, 1.005393624328714264 ) ) ;
#125032 = CARTESIAN_POINT ( 'NONE',  ( 4.780823714695519477, 1.590225366507077354, -1.067722475238532365 ) ) ;
#125033 = CARTESIAN_POINT ( 'NONE',  ( -11.44779963594995564, 13.39999999999999147, 3.600000000000075140 ) ) ;
#125034 = CARTESIAN_POINT ( 'NONE',  ( -0.3037066968988046400, -3.101636548795144943, 3.416163890146756810 ) ) ;
#125035 = EDGE_CURVE ( 'NONE', #179985, #170847, #178513, .T. ) ;
#125036 = CARTESIAN_POINT ( 'NONE',  ( -10.25877837909746937, 3.235871879154613051, 5.476282928277060869 ) ) ;
#125038 = ORIENTED_EDGE ( 'NONE', *, *, #121204, .F. ) ;
#125037 = CARTESIAN_POINT ( 'NONE',  ( 4.202664430556247055, 6.886563688082179446, 1.082531754730558626 ) ) ;
#125039 = CARTESIAN_POINT ( 'NONE',  ( -6.724481002698115439, 10.78905223654906109, -0.7216878364870267237 ) ) ;
#125040 = CARTESIAN_POINT ( 'NONE',  ( 3.010779355932476253, 1.566693023359872372, -1.489686202715050145 ) ) ;
#125041 = EDGE_CURVE ( 'NONE', #167380, #213109, #26360, .T. ) ;
#125042 = CARTESIAN_POINT ( 'NONE',  ( -4.878955176071358757, 6.785476686873604280, -1.599625672291271394 ) ) ;
#125043 = CARTESIAN_POINT ( 'NONE',  ( 6.943184063974162434, 9.193743722760251202, -1.443375672974064550 ) ) ;
#125044 = CARTESIAN_POINT ( 'NONE',  ( 7.632173801829039911E-16, -0.4330127018922214077, 6.200000000000000178 ) ) ;
#125045 = CARTESIAN_POINT ( 'NONE',  ( 4.418855976699648025, 1.669273799801282765, 0.7395231729718022562 ) ) ;
#125046 = CARTESIAN_POINT ( 'NONE',  ( 8.994968294694656308, 12.46332533355852590, 7.469580661692561740 ) ) ;
#125047 = CARTESIAN_POINT ( 'NONE',  ( 1.493369529629706705, 1.490176471889271603, 1.290657618255620864 ) ) ;
#125048 = CARTESIAN_POINT ( 'NONE',  ( 3.955252344019274169, -1.661368509396843995, 0.9470704235666274062 ) ) ;
#125049 = ORIENTED_EDGE ( 'NONE', *, *, #41997, .F. ) ;
#125050 = CARTESIAN_POINT ( 'NONE',  ( 0.3999999999999825917, 3.963633530850413145, 0.9046180958550574802 ) ) ;
#125051 = CARTESIAN_POINT ( 'NONE',  ( 4.914487397858644080, 0.7518983826605809551, 1.820584232156793769 ) ) ;
#125052 = ORIENTED_EDGE ( 'NONE', *, *, #60132, .T. ) ;
#125053 = CARTESIAN_POINT ( 'NONE',  ( 6.233930015136599501, 1.921560620327814606, 0.2806146417165931717 ) ) ;
#125054 = ORIENTED_EDGE ( 'NONE', *, *, #206395, .T. ) ;
#125055 = CARTESIAN_POINT ( 'NONE',  ( -6.784929528996132220, 6.880448970109080520, 0.000000000000000000 ) ) ;
#125057 = CARTESIAN_POINT ( 'NONE',  ( 6.381110825713084189, -1.939362502171553482, -0.8581636585355473246 ) ) ;
#125056 = CARTESIAN_POINT ( 'NONE',  ( -3.772911886352873445, 7.623757310712140800, 0.7998128361456352531 ) ) ;
#125058 = CARTESIAN_POINT ( 'NONE',  ( 8.136301581532414673, 8.664975731308866003, 0.000000000000000000 ) ) ;
#125060 = ORIENTED_EDGE ( 'NONE', *, *, #79549, .F. ) ;
#125059 = CARTESIAN_POINT ( 'NONE',  ( 3.580628178849315280, -1.282259035790348722, 1.418852674340838060 ) ) ;
#125061 = CARTESIAN_POINT ( 'NONE',  ( -2.974698719455045381, 6.690899969729074748, -0.05384663926280564006 ) ) ;
#125062 = CARTESIAN_POINT ( 'NONE',  ( 9.367496997597591246, 3.530917816115240360, -7.500000000000005329 ) ) ;
#125063 = CARTESIAN_POINT ( 'NONE',  ( 5.022139790744326149, -2.003173700978663874, 0.1997323756105211789 ) ) ;
#125064 = DIRECTION ( 'NONE',  ( 0.6507913734559641616, -0.7592566023653004592, 0.000000000000000000 ) ) ;
#125066 = CARTESIAN_POINT ( 'NONE',  ( 6.410779360540267646, 1.349177972556347971, -1.230185023894624141 ) ) ;
#125065 = PRODUCT_DEFINITION_FORMATION_WITH_SPECIFIED_SOURCE ( 'ANY', '', #26328, .NOT_KNOWN. ) ;
#125067 = CARTESIAN_POINT ( 'NONE',  ( 2.066927875543830950, 1.535623996113824496, -1.388825173883188713 ) ) ;
#125068 = CARTESIAN_POINT ( 'NONE',  ( -6.413170354464012846, 7.440785820751486312, 1.199719254218450271 ) ) ;
#125069 = CIRCLE ( 'NONE', #69594, 11.00000000000000000 ) ;
#125070 = CARTESIAN_POINT ( 'NONE',  ( -6.127277117991962285, 7.006264510460848527, -0.9572512136472415278 ) ) ;
#125071 = CARTESIAN_POINT ( 'NONE',  ( -1.734723475976807094E-15, 2.999999999999988898, -6.938893903907228378E-15 ) ) ;
#125072 = CARTESIAN_POINT ( 'NONE',  ( 6.420764531294745225, 1.746252128813120086, 0.6712297951826234899 ) ) ;
#125073 = CARTESIAN_POINT ( 'NONE',  ( 6.474182045725470402, 7.511966127223233869, -1.199719254218446718 ) ) ;
#125074 = AXIS2_PLACEMENT_3D ( 'NONE', #196601, #79647, #96996 ) ;
#125075 = CARTESIAN_POINT ( 'NONE',  ( -3.100010679019018500, 6.768429558830820980, 1.040834085586084257E-14 ) ) ;
#125076 = CARTESIAN_POINT ( 'NONE',  ( 5.587368702607580673, 5.691220705896524734, -0.7216878364870458196 ) ) ;
#125077 = CARTESIAN_POINT ( 'NONE',  ( -5.721177634842498527, 5.777054783512106440, 0.000000000000000000 ) ) ;
#125078 = CARTESIAN_POINT ( 'NONE',  ( 1.364683531249997417, 11.79687500034139802, 2.602085213965210642E-15 ) ) ;
#125080 = CARTESIAN_POINT ( 'NONE',  ( -5.433785704026946384, 9.561443431331920095, 0.000000000000000000 ) ) ;
#125079 = CARTESIAN_POINT ( 'NONE',  ( 6.825078400183526739, -0.0002198122173602961866, 1.955566246027613531 ) ) ;
#125081 = CARTESIAN_POINT ( 'NONE',  ( 4.834428552630634535, 0.5376618173574229109, -1.648781088846348108 ) ) ;
#125082 = CARTESIAN_POINT ( 'NONE',  ( -5.091250377131585125, 5.898545847196970726, 1.199719254218450271 ) ) ;
#125083 = CARTESIAN_POINT ( 'NONE',  ( 2.764580022184208730, -0.7881864689132519475, -1.914544693583389634 ) ) ;
#125084 = CARTESIAN_POINT ( 'NONE',  ( 3.163770493730236666, 1.345063228294058000, 1.635049775249038051 ) ) ;
#125085 = CARTESIAN_POINT ( 'NONE',  ( 8.762647353133951711, 9.117510088278095282, 1.040834085586084257E-14 ) ) ;
#125086 = CARTESIAN_POINT ( 'NONE',  ( 0.08359363160202464005, -9.910747646673584654, 10.99968245379461607 ) ) ;
#125087 = CARTESIAN_POINT ( 'NONE',  ( 2.254690153889327586, -0.5205305878250593432, -1.899364841092534339 ) ) ;
#125088 = CARTESIAN_POINT ( 'NONE',  ( 6.080382892099663650, 6.037283676876850969, 0.3399492115118609714 ) ) ;
#125090 = CARTESIAN_POINT ( 'NONE',  ( 11.92619526913699879, 12.69999999999999929, -1.328859060402686199 ) ) ;
#125089 = CARTESIAN_POINT ( 'NONE',  ( 3.475000000000000533, -0.9041666666666666741, 2.006292185433948827 ) ) ;
#125091 = CARTESIAN_POINT ( 'NONE',  ( 4.154423454741348110, -1.699848520643287175, 1.538017723768041023 ) ) ;
#125092 = CARTESIAN_POINT ( 'NONE',  ( 1.734698295210383767, 0.1775668987445792879, 1.817036636966688823 ) ) ;
#125093 = CARTESIAN_POINT ( 'NONE',  ( 5.006703865196457492, 9.063181286029688977, 0.000000000000000000 ) ) ;
#125094 = CARTESIAN_POINT ( 'NONE',  ( 4.961921032477176752, 8.732732271291288484, 1.040834085586084257E-14 ) ) ;
#125095 = CARTESIAN_POINT ( 'NONE',  ( -7.263417608619167076, 9.497073181520933716, -1.599625672291263179 ) ) ;
#125096 = CARTESIAN_POINT ( 'NONE',  ( 2.724860606552154785, 1.455292111517191511, -1.391298800531393765 ) ) ;
#125097 = CARTESIAN_POINT ( 'NONE',  ( 2.254674508890702089, -0.5182927192734412269, -1.892014123021222627 ) ) ;
#125098 = CARTESIAN_POINT ( 'NONE',  ( -8.402302512167102222, 10.82577223566020841, -1.599625672291263179 ) ) ;
#125099 = CARTESIAN_POINT ( 'NONE',  ( -6.575868197828002693, 7.630599971342813426, 1.199719254218450271 ) ) ;
#125100 = CARTESIAN_POINT ( 'NONE',  ( 0.1751657365761885576, 5.722053558346082092, -2.638081460773045617 ) ) ;
#125102 = CARTESIAN_POINT ( 'NONE',  ( 3.766244448481158802, -1.188900867318806176, 1.311211162958977328 ) ) ;
#125101 = CARTESIAN_POINT ( 'NONE',  ( 5.121074860632232273, -1.985326386471301552, 0.6553513102709652705 ) ) ;
#125103 = CARTESIAN_POINT ( 'NONE',  ( -3.501245407925490216, 15.00000000000010658, 11.28115623562641900 ) ) ;
#125104 = EDGE_CURVE ( 'NONE', #116176, #158436, #178483, .T. ) ;
#125105 = CARTESIAN_POINT ( 'NONE',  ( 6.386719491623852996, 1.997645938776301477, -1.124140632904375936 ) ) ;
#125106 = CARTESIAN_POINT ( 'NONE',  ( 5.331890987662370129, 1.715487909331077310, 0.2919898797263379975 ) ) ;
#125107 = CARTESIAN_POINT ( 'NONE',  ( 7.618792255875527886, 10.97600916757510170, 1.199719254218460707 ) ) ;
#125108 = CARTESIAN_POINT ( 'NONE',  ( 6.153027625867640182, 1.178261263523974645, 1.973664585577431518 ) ) ;
#125109 = CARTESIAN_POINT ( 'NONE',  ( 0.1333692844072802142, 2.017199222642913625, -2.468757726274827036 ) ) ;
#125110 = CARTESIAN_POINT ( 'NONE',  ( 5.712138547670210009, -1.368237114983595237, -1.064765744168968187 ) ) ;
#125111 = CARTESIAN_POINT ( 'NONE',  ( 5.687976231080541289, -1.372897218612447290, -1.682037316681925132 ) ) ;
#125112 = DIRECTION ( 'NONE',  ( 0.000000000000000000, 0.000000000000000000, -1.000000000000000000 ) ) ;
#125113 = CARTESIAN_POINT ( 'NONE',  ( 0.07561343334091479018, 1.573685453729951833, 1.416787448489342127 ) ) ;
#125114 = CARTESIAN_POINT ( 'NONE',  ( 5.281250000000004441, 0.7852924748302615443, 1.895863743163964665 ) ) ;
#125115 = CARTESIAN_POINT ( 'NONE',  ( 6.827182134110224787, 2.426453598513299337, 2.470348285387702347 ) ) ;
#125116 = CARTESIAN_POINT ( 'NONE',  ( 3.909137014540211119, 1.651653515444248876, 0.9912706138347370244 ) ) ;
#125117 = CARTESIAN_POINT ( 'NONE',  ( 1.499999999999993117, 11.88541666734946034, 0.8660254037844409281 ) ) ;
#125118 = CARTESIAN_POINT ( 'NONE',  ( 0.5225339808294949817, -2.210013125053798433, 0.2238140636349055246 ) ) ;
#125119 = ORIENTED_EDGE ( 'NONE', *, *, #71283, .F. ) ;
#125120 = CARTESIAN_POINT ( 'NONE',  ( -1.001543065824772872E-14, 4.712500000000017231, 1.732050807568877637 ) ) ;
#125121 = CARTESIAN_POINT ( 'NONE',  ( 4.473300617505036492, 7.306268922809479704, -1.199719254218452047 ) ) ;
#125122 = CARTESIAN_POINT ( 'NONE',  ( 7.793239369756836510, 7.986534107671458216, 0.7998128361456341429 ) ) ;
#125123 = CARTESIAN_POINT ( 'NONE',  ( 2.579030809547431247, -1.529751724882743247, 1.610829425214066246 ) ) ;
#125124 = CARTESIAN_POINT ( 'NONE',  ( 6.534666852106798096, 7.686494751288491578, -1.082531754730543083 ) ) ;
#125125 = EDGE_CURVE ( 'NONE', #65489, #160319, #36715, .T. ) ;
#125126 = CARTESIAN_POINT ( 'NONE',  ( -8.961576348508641487, 11.47825837805867799, -1.443375672974058777 ) ) ;
#125127 = CARTESIAN_POINT ( 'NONE',  ( 5.668717624289557833, 8.667235424096215723, -1.082531754730548412 ) ) ;
#125128 = CARTESIAN_POINT ( 'NONE',  ( 0.6158615555539399544, 0.1511424999406512648, 2.010826230049263863 ) ) ;
#125130 = CARTESIAN_POINT ( 'NONE',  ( 5.266109189975630045, -2.053049664954803788, 0.1989083462991206031 ) ) ;
#125129 = CARTESIAN_POINT ( 'NONE',  ( 7.377608144130607393, 11.75895993479440982, -0.7998128361456291469 ) ) ;
#125131 = CARTESIAN_POINT ( 'NONE',  ( 1.499999999999989120, 6.280000000000042881, -2.873333333333329520 ) ) ;
#125132 = CARTESIAN_POINT ( 'NONE',  ( 7.471952054462756010, 7.889901283060952508, 0.7216878364870267237 ) ) ;
#125133 = B_SPLINE_CURVE_WITH_KNOTS ( 'NONE', 3,
 ( #146044, #147102, #61566, #45334, #163341, #177458, #95156, #12793, #78867, #96224 ),
 .UNSPECIFIED., .F., .F.,
 ( 4, 3, 3, 4 ),
 ( 0.000000000000000000, 0.0001748932287411561373, 0.0003221082053133044300, 0.0004700044474451332398 ),
 .UNSPECIFIED. ) ;
#125134 = CARTESIAN_POINT ( 'NONE',  ( 2.449293598294706414E-16, -4.500000000000003553, -2.000000000000000000 ) ) ;
#125135 = CARTESIAN_POINT ( 'NONE',  ( -0.6823417656250212460, 1.051041667008083325, 1.181850606188755259 ) ) ;
#125136 = CARTESIAN_POINT ( 'NONE',  ( 1.774285776001020221, -1.678457933910833644, -0.5611888468203419800 ) ) ;
#125137 = CARTESIAN_POINT ( 'NONE',  ( 0.03578008775950020093, -1.617816776142148250, 1.203357013023528932 ) ) ;
#125138 = CARTESIAN_POINT ( 'NONE',  ( 5.776847720190436242, 1.604795045139913556, -0.6741588622883755155 ) ) ;
#125139 = CARTESIAN_POINT ( 'NONE',  ( 3.913864042289341150, -1.178888685321772156, -1.965896434285055117 ) ) ;
#125140 = CARTESIAN_POINT ( 'NONE',  ( 0.6823417656249882723, 0.09270833367475139752, 1.181850606188755259 ) ) ;
#125141 = CARTESIAN_POINT ( 'NONE',  ( 2.202840038917678545, -0.4038221959529255112, 1.796142596185656526 ) ) ;
#125142 = ADVANCED_FACE ( 'NONE', ( #4968 ), #144399, .F. ) ;
#125143 = CARTESIAN_POINT ( 'NONE',  ( 8.563946585326370098, 13.14302144952281814, 0.7998128361456462443 ) ) ;
#125144 = CARTESIAN_POINT ( 'NONE',  ( 11.88429252019798632, 7.170827761689094970, -1.886747465692856451 ) ) ;
#125145 = CARTESIAN_POINT ( 'NONE',  ( 3.188313505853744179, -1.798300186086329688, -0.3134973320952222364 ) ) ;
#125146 = CARTESIAN_POINT ( 'NONE',  ( 4.131482539099665452, 0.5404898895830790861, 1.942541833525657680 ) ) ;
#125147 = CARTESIAN_POINT ( 'NONE',  ( -10.47775378526269918, 11.11846759242831872, -0.7998128361456221525 ) ) ;
#125148 = CARTESIAN_POINT ( 'NONE',  ( 2.800010096142038218, -0.7105090101824761417, 2.148112714708799942 ) ) ;
#125149 = CARTESIAN_POINT ( 'NONE',  ( 5.420966337283807945, 1.944620675078809757, 0.8088979906116978702 ) ) ;
#125150 = CARTESIAN_POINT ( 'NONE',  ( 9.504385499323440456, 15.23678955516845868, 8.235007229972609366 ) ) ;
#125151 = CARTESIAN_POINT ( 'NONE',  ( 2.260293373024503616, -2.069953001785612479, 0.04851313490940312168 ) ) ;
#125152 = CARTESIAN_POINT ( 'NONE',  ( 3.506755287428983792, 7.242964935309132990, 1.040834085586084257E-14 ) ) ;
#125153 = CARTESIAN_POINT ( 'NONE',  ( -5.558564015327489343E-14, 0.4843750003414603600, 1.570758158831762286 ) ) ;
#125154 = CARTESIAN_POINT ( 'NONE',  ( 4.371814246616528621, 0.4635510597098578267, -2.069045912693792566 ) ) ;
#125155 = ITEM_DEFINED_TRANSFORMATION ( 'NONE', 'NONE', #34824,  #200407 ) ;
#125156 = CARTESIAN_POINT ( 'NONE',  ( 0.5043604530000692643, -0.6477430859608296343, -1.814464506502324159 ) ) ;
#125157 = CARTESIAN_POINT ( 'NONE',  ( -5.276058054373441664, 6.184431147304315424, -1.199719254218453823 ) ) ;
#125158 = CARTESIAN_POINT ( 'NONE',  ( 7.723341061279088038, 12.16231500480096983, -0.7998128361456291469 ) ) ;
#125159 = CARTESIAN_POINT ( 'NONE',  ( 6.346625304528514810, 6.577020074804287297, 0.000000000000000000 ) ) ;
#125160 = CARTESIAN_POINT ( 'NONE',  ( 3.475000000000000533, -0.8604166657107521488, 2.006292185433948827 ) ) ;
#125161 = CARTESIAN_POINT ( 'NONE',  ( -4.009460741339347045, 5.700790169694431420, -1.599625672291256295 ) ) ;
#125162 = CARTESIAN_POINT ( 'NONE',  ( 5.836213162209912930, -1.179542664122106510, -1.762073437084572314 ) ) ;
#125163 = CARTESIAN_POINT ( 'NONE',  ( 1.729655969393493642, -1.983145177596838948, 0.7090631796887718608 ) ) ;
#125164 = CARTESIAN_POINT ( 'NONE',  ( -6.303615075710993665, 6.318915441276411471, -0.7998128361456362523 ) ) ;
#125165 = CARTESIAN_POINT ( 'NONE',  ( 8.426556166093362776, 9.789735934319136135, -1.199719254218446718 ) ) ;
#125166 = CARTESIAN_POINT ( 'NONE',  ( 6.332830178222744522, -1.766687566082520533, -0.5848361604409312298 ) ) ;
#125167 = CARTESIAN_POINT ( 'NONE',  ( 6.913768267964901071, 10.15348118167935709, -1.199719254218441611 ) ) ;
#125168 = CARTESIAN_POINT ( 'NONE',  ( 11.94980361490430099, 10.09667875264134551, 1.099999952233555955 ) ) ;
#125169 = CARTESIAN_POINT ( 'NONE',  ( -4.995253251992230581, 4.792493313604505367, 0.000000000000000000 ) ) ;
#125170 = CARTESIAN_POINT ( 'NONE',  ( -9.354762803749327560, 10.01623748057011376, 0.7216878364870438212 ) ) ;
#125171 = CARTESIAN_POINT ( 'NONE',  ( 0.3520121086563637314, -1.504009422257305495, -1.495223887398588358 ) ) ;
#125173 = CARTESIAN_POINT ( 'NONE',  ( 3.103904542773823660, 0.7086415210641981988, -1.829580771271981154 ) ) ;
#125172 = CARTESIAN_POINT ( 'NONE',  ( -0.6801582343750108839, 2.880208333674722176, -1.178068619123848526 ) ) ;
#125174 = CARTESIAN_POINT ( 'NONE',  ( 1.042116488573753497, 0.8753402851892390091, -1.976733581976031218 ) ) ;
#125176 = CARTESIAN_POINT ( 'NONE',  ( -5.408724846006345288, 6.482216231307839749, 1.333832282565196925 ) ) ;
#125175 = CARTESIAN_POINT ( 'NONE',  ( -3.949167883330528372, 7.829389307186077396, 1.214306433183764966E-14 ) ) ;
#125177 = CARTESIAN_POINT ( 'NONE',  ( -1.402160292154681736E-14, 1.696875000341421469, -1.575800808251659024 ) ) ;
#125178 = CARTESIAN_POINT ( 'NONE',  ( 2.132362993881876889, -1.555188906917738700, 0.7812613976432846163 ) ) ;
#125179 = CARTESIAN_POINT ( 'NONE',  ( 5.178851490740187913, 8.985817805931475277, 0.7216878364870438212 ) ) ;
#125180 = CARTESIAN_POINT ( 'NONE',  ( -12.15057777967900243, 9.234859088329544718, 2.778757836088345812 ) ) ;
#125181 = CIRCLE ( 'NONE', #100801, 0.07999999999999972411 ) ;
#125182 = EDGE_CURVE ( 'NONE', #127411, #135468, #32727, .T. ) ;
#125183 = CARTESIAN_POINT ( 'NONE',  ( 2.161482305958133399, -0.5350050527693461788, -1.943774068525660148 ) ) ;
#125184 = CARTESIAN_POINT ( 'NONE',  ( 6.825078400183518745, 4.686743419949856104, 2.806861564458093650 ) ) ;
#125185 = CARTESIAN_POINT ( 'NONE',  ( -5.971440312176176768, 5.931378217152456500, 0.000000000000000000 ) ) ;
#125186 = CARTESIAN_POINT ( 'NONE',  ( 2.448066223300342514, 1.970991375097268961, 0.05018580263361701460 ) ) ;
#125188 = CARTESIAN_POINT ( 'NONE',  ( -4.340018570150306232, 8.077455741901736985, -0.7216878364870338292 ) ) ;
#125187 = CARTESIAN_POINT ( 'NONE',  ( 6.135011676971934058, 1.786887936952135991, 0.6819008164158719687 ) ) ;
#125189 = CARTESIAN_POINT ( 'NONE',  ( -4.760321331729590710, 8.567808963744235839, 0.7216878364870267237 ) ) ;
#125190 = CARTESIAN_POINT ( 'NONE',  ( 4.525389411911321602, 8.501647757197021704, -0.7998128361456381397 ) ) ;
#125191 = CARTESIAN_POINT ( 'NONE',  ( -6.317173229324657413, 6.334733287159020954, 0.000000000000000000 ) ) ;
#125192 = CARTESIAN_POINT ( 'NONE',  ( 1.576825605243727502, -1.426663165427190405, 1.429853764617691647 ) ) ;
#125193 = DIRECTION ( 'NONE',  ( 0.000000000000000000, 0.000000000000000000, 1.000000000000000000 ) ) ;
#125194 = CARTESIAN_POINT ( 'NONE',  ( 5.930798096255836427, 2.221851032742766741, 0.6229754028606748761 ) ) ;
#125195 = CARTESIAN_POINT ( 'NONE',  ( 6.531700620877029628, 1.877769495358465157, -0.5682946464737671510 ) ) ;
#125196 = CARTESIAN_POINT ( 'NONE',  ( 3.028120845615460688, 1.045410262836780069, 1.659804706804830277 ) ) ;
#125197 = CARTESIAN_POINT ( 'NONE',  ( 7.584896871841365851, 10.93646455286856956, -1.199719254218446718 ) ) ;
#125198 = CARTESIAN_POINT ( 'NONE',  ( 0.4400775573648734174, -1.704940109561555950, -1.076314675215600314 ) ) ;
#125199 = ORIENTED_EDGE ( 'NONE', *, *, #138892, .F. ) ;
#125200 = CARTESIAN_POINT ( 'NONE',  ( 0.8314520141109645879, -1.673154641659507558, -1.297526329946703472 ) ) ;
#125202 = CARTESIAN_POINT ( 'NONE',  ( -7.477485413136760073, 8.682486722536401302, -1.199719254218446718 ) ) ;
#125201 = CARTESIAN_POINT ( 'NONE',  ( -2.774614992291035698, 6.388801257648172971, 1.040834085586084257E-14 ) ) ;
#125203 = CARTESIAN_POINT ( 'NONE',  ( 2.132514540308296791, -1.644867172388216003, 0.8273176719292076875 ) ) ;
#125204 = ORIENTED_EDGE ( 'NONE', *, *, #15332, .T. ) ;
#125205 = B_SPLINE_CURVE_WITH_KNOTS ( 'NONE', 3,
 ( #45781, #114036, #129239, #127095 ),
 .UNSPECIFIED., .F., .F.,
 ( 4, 4 ),
 ( -3.662496629072134259E-08, 0.0006801242851315165375 ),
 .UNSPECIFIED. ) ;
#125206 = CARTESIAN_POINT ( 'NONE',  ( -1.500000000000079936, 7.176846818246208848, 4.202462424328226476 ) ) ;
#125207 = CARTESIAN_POINT ( 'NONE',  ( 2.531617689938488791, -0.2033970545941807817, 2.110794199748195599 ) ) ;
#125208 = CARTESIAN_POINT ( 'NONE',  ( -1.500000000000011324, 4.410416667349484676, -0.8660254037844313801 ) ) ;
#125209 = CARTESIAN_POINT ( 'NONE',  ( 8.776205506747620788, 9.133327934160710981, -0.7998128361456221525 ) ) ;
#125210 = CARTESIAN_POINT ( 'NONE',  ( 6.003228155800906407, 10.22579295840155744, 0.000000000000000000 ) ) ;
#125211 = CARTESIAN_POINT ( 'NONE',  ( 3.813790581289760784, -2.030913156241159978, 0.3485601269093330234 ) ) ;
#125213 = CARTESIAN_POINT ( 'NONE',  ( 1.399689850468607277, -0.6632477835330424787, -1.717811453623831808 ) ) ;
#125212 = CARTESIAN_POINT ( 'NONE',  ( -7.283754839039664475, 9.520799950344851936, -1.599625672291263179 ) ) ;
#125214 = CARTESIAN_POINT ( 'NONE',  ( -1.364683531250012516, 4.238541667008090208, -0.7879004041258300672 ) ) ;
#125215 = CARTESIAN_POINT ( 'NONE',  ( -0.02224634325202321655, 2.854569189074110280, -2.777010687634806629 ) ) ;
#125216 =( BOUNDED_SURFACE ( )  B_SPLINE_SURFACE ( 3, 3, ( 
 ( #129347, #161767, #158555, #41622, #208347, #107736, #173761, #25338, #11215, #42696, #128283, #91439, #10152, #94642, #191029, #210486, #62123, #44826, #159618, #27475, #157500, #28553, #58915, #110931, #125072, #45889, #112010, #26404, #76226, #59978, #43759, #192092, #77296, #178010, #9095, #115198, #46956, #147645, #113073, #99950, #167090, #68488, #150847, #2411, #114146, #34927, #149773, #197438, #83684, #65288, #101001, #166014, #179079, #195325, #196389, #17600, #50135, #133551, #117325, #18681, #1348, #84760, #212616, #30701, #98892, #67410, #199559, #148704, #164945, #96782, #49078, #131435, #48032, #130399, #51203, #162833, #183323, #64256, #66345, #181191, #32818, #14411, #132489, #80501, #81561, #146598, #82619, #180138, #31766, #97836, #198491, #163901, #15477, #213663, #16537, #273, #116258, #182247, #33872, #89050, #37068, #201681, #85828, #171340, #102080, #35999, #200618, #40290, #55462, #202751, #10689, #103149, #53327, #185448, #169210, #20801, #118392, #86897, #151907, #87963, #106400, #120543, #134616, #152964, #69548, #168148, #71685, #4538, #155107, #52265, #19748, #70612, #119460, #3481, #184380, #72767, #136727, #135658, #54404, #121617, #22934, #159091, #186522, #38152, #188661, #104224, #187586, #39212, #170271, #21856, #154037, #5603, #105303, #137798, #6692, #203817, #138866, #93050, #204884, #56536, #122698, #172424, #26943, #97305, #79961, #163364, #208883, #110412, #145011, #213148, #192637, #146064, #76759, #180664, #142881, #44290, #114670, #13882, #212077, #176415, #162295, #63716, #126674, #164420, #28022, #78888, #112534, #94119, #160160, #196912, #77832, #11758, #143953, #129874, #195857, #47497, #209948, #179610, #32289, #128798, #130919, #127756, #113606, #64778, #96244, #98355, #48552, #31231, #60513, #61587, #193713, #14940, #81035, #147122, #45356, #111475, #177480, #29095, #95179, #161228, #194780, #12815, #211017, #30156, #46417, #62640, #178546, #100479, #17075, #165479, #52797, #131958, #152441, #99425, #70089, #168683, #83153, #67945, #181714, #16004, #35474, #184916, #185985, #120009, #807, #53876, #20287, #202222, #151384, #66875, #36540, #51747, #86372, #136204, #84231, #19220, #85298, #4020, #33343, #150319, #65811, #37619, #200098, #18143, #1885, #2954, #133020, #199019, #149233, #50666, #214183, #116792, #182789, #34407, #134090, #166555, #117870, #183861, #103699, #101552, #82089, #167621, #148182, #118936, #197968, #49599, #69025, #115723, #135142, #201158, #102627, #141570, #139405, #170820, #41915, #207578, #6159, #8312, #104771, #74397, #124298, #57075, #7227, #23487, #153513, #90659, #187060, #24552, #121093, #58139, #174052, #22411, #138335, #88520, #171890, #39759, #38693, #106950, #156721, #89594, #21338, #122161, #87444, #140498, #59198, #42985, #125354, #191317, #154582, #9386, #190257, #155643, #108026, #105864, #5082, #188128, #71157, #206508, #169750, #137274, #203294, #54941, #72228, #75457, #25625, #73303, #91737, #205439, #204351, #157790, #56009, #123239, #189204, #40841, #172973, #47249, #30990, #14700, #211835, #146884, #126423, #109095, #12571, #63472, #113363, #62402, #78643, #175111, #177230, #193474, #110160, #44041, #145830, #10441, #97065, #192387, #163118, #179368, #176172, #160980, #60266, #26698, #128565, #129627, #64537, #212904, #93868 ),
 ( #210779, #27772, #130681, #159906, #112291, #13642, #143707, #142624, #80794, #195612, #196670, #158844, #94931, #92799, #11513, #77584, #209699, #76513, #208633, #61343, #127502, #45117, #29916, #28843, #111227, #144769, #194530, #46177, #178307, #95998, #162052, #79714, #213946, #1626, #20020, #34153, #48310, #16818, #197717, #164177, #199842, #99174, #2692, #114421, #15762, #82903, #115478, #65567, #180421, #200891, #148976, #32039, #116534, #35206, #85037, #69824, #550, #49359, #102352, #17880, #101282, #167365, #66615, #98126, #132762, #81847, #18953, #86109, #135932, #3750, #147930, #181470, #168424, #68764, #50415, #151126, #198765, #152180, #134884, #131714, #33099, #165226, #52537, #117607, #118671, #184654, #182523, #36275, #100223, #166291, #83965, #150054, #67685, #133831, #51484, #183599, #201950, #55737, #71961, #203030, #137002, #24283, #103426, #124037, #70892, #41653, #140228, #54671, #39488, #153239, #53606, #6959, #156458, #157531, #91469, #186796, #25369, #206249, #173793, #122978, #38425, #8044, #23214, #57875, #107767, #121892, #205167, #56808, #190003, #4810, #187861, #37352, #9125, #171620, #204084, #105586, #188937, #104504, #170548, #120819, #22132, #185719, #88245, #154315, #5888, #89327, #138071, #155374, #73040, #75201, #139138, #119740, #40576, #169488, #90389, #21071, #87169, #106682, #172705, #74134, #179109, #207324, #113103, #110963, #142370, #13388, #30731, #192128, #194278, #76261, #45923, #95746, #28588, #193212, #209438, #125102, #62157, #158587, #210521, #92548, #29660, #145581, #208379, #109906, #60011, #143441, #11250, #10187, #78393, #128315, #61082, #58945, #161797, #77328, #195355, #112043, #191060, #162863, #126164, #178044, #79464, #211578, #63212, #46987, #129376, #96814, #43793, #141312, #44859, #14442, #42725, #94676, #176971, #108833, #127242, #160718, #175917, #27508, #174859, #26438, #93608, #159653, #12312, #144513, #147678, #132523, #31796, #80532, #99981, #34960, #36032, #184413, #65317, #118427, #84792, #52298, #1381, #131466, #101031, #116288, #150880, #200649, #148736, #83717, #149807, #2443, #97871, #304, #130433, #102110, #50167, #82652, #66375, #67442, #197467, #49111, #163931, #115231, #64287, #213695, #181221, #15506, #198521, #81593, #32848, #98924, #168181, #164977, #146628, #16569, #212645, #117358, #196419, #48063, #182278, #114176, #33903, #180170, #166047, #17631, #133587, #199591, #167122, #51234, #183356, #18709, #68517, #134644, #188694, #121651, #71718, #88000, #3511, #155140, #37104, #89083, #185479, #122731, #24044, #20832, #202786, #86930, #21890, #104256, #103184, #171375, #6721, #154072, #85862, #186555, #151937, #138900, #206000, #107515, #189753, #41405, #152997, #73885, #40330, #5637, #169244, #137831, #4573, #70647, #136757, #19780, #54436, #57636, #120578, #69581, #56572, #123795, #139978, #38184, #135692, #170302, #201717, #53358, #119492, #203852, #55497, #106435, #187618, #39246, #72800, #105338, #204919, #172457, #22968, #90148, #156216, #7792, #94424, #190812, #28328, #124846, #61901, #177791, #174610, #142117, #26186, #175663, #43538, #42472, #110715, #160463, #93357, #25118, #125919, #91221, #78139, #145328, #46736, #129123, #195100, #92301, #13133, #128062, #27250, #194018, #109661, #79210, #144270, #157282, #173544, #158345, #210263 ),
 ( #126989, #77068, #8871, #159394, #10993, #9939, #108582, #45668, #74950, #95499, #76014, #211329, #111785, #208130, #143197, #59759, #141061, #192948, #29407, #207068, #62954, #191878, #58698, #209188, #60828, #44600, #176715, #12071, #161546, #49910, #83461, #213448, #146374, #54, #64031, #2183, #179919, #116031, #17377, #147423, #212389, #50975, #149541, #34709, #162607, #98667, #67189, #15257, #31541, #96560, #97617, #163674, #130177, #32590, #113923, #81344, #65070, #68260, #131226, #150623, #197214, #134392, #1127, #200395, #18456, #48854, #112848, #114968, #178864, #30475, #84533, #82396, #180968, #199329, #14183, #164722, #165794, #47810, #133326, #117097, #66117, #16311, #148485, #80276, #33648, #196169, #182017, #132260, #183098, #100778, #198267, #99722, #166861, #54172, #136502, #69323, #203590, #38992, #186286, #118170, #4316, #184156, #171115, #23788, #139714, #7531, #73614, #185215, #106173, #6461, #120312, #154878, #202523, #172199, #22708, #35778, #52044, #53098, #88821, #121389, #204658, #188429, #89895, #72538, #155946, #135433, #101854, #170041, #138636, #56308, #5381, #21627, #167922, #37924, #103998, #119232, #201455, #122469, #19520, #40064, #36839, #85597, #151685, #102921, #87735, #3255, #168982, #71459, #20582, #86667, #152734, #70386, #153810, #137572, #55242, #187362, #105077, #160200, #26985, #209992, #111518, #59494, #208925, #60560, #61634, #157021, #125651, #41143, #29136, #175400, #207871, #191613, #192679, #42207, #108324, #8607, #174344, #124592, #74690, #43275, #206805, #190551, #25922, #161274, #92030, #95224, #158087, #12860, #28068, #78935, #177524, #9676, #205738, #75752, #57371, #123534, #189499, #93092, #58438, #77878, #107254, #141862, #44333, #140791, #110455, #11803, #159133, #109396, #10734, #173274, #126719, #76804, #176456, #142925, #94161, #127800, #144000, #193755, #45402, #24854, #90956, #162344, #82138, #132010, #64823, #211060, #97355, #62685, #49648, #119775, #21105, #103463, #169525, #63761, #201985, #99472, #147169, #33394, #14988, #53642, #115771, #128844, #145057, #146112, #181760, #214232, #86145, #69860, #185755, #165531, #37388, #13927, #194825, #48599, #17123, #152216, #98403, #114717, #46461, #213196, #81082, #212123, #80007, #3785, #112583, #135969, #129921, #178595, #30204, #195907, #196961, #96292, #47543, #164468, #113656, #179660, #31280, #163412, #130969, #180712, #32335, #16054, #148230, #65860, #198020, #91505, #207360, #155412, #90426, #156495, #157566, #38464, #6995, #137038, #125136, #56847, #89364, #73073, #74173, #138110, #204121, #104540, #55773, #70929, #154349, #203065, #174892, #54708, #139174, #123019, #120859, #186832, #58980, #88285, #170585, #22170, #172745, #24320, #206285, #5927, #190038, #42762, #205205, #141345, #121930, #124074, #187897, #153273, #71999, #23251, #171654, #188970, #191093, #8084, #57909, #39527, #105625, #40614, #106718, #108868, #140265, #41690, #107801, #173826, #25403, #9159, #75235, #87209, #4850, #12346, #195391, #143476, #93639, #192162, #63247, #208411, #142403, #92582, #146664, #161833, #94709, #114208, #209472, #159682, #77362, #61114, #127274, #10221, #193246, #43822, #194314, #212678, #78426, #26472, #44893, #175948, #60045, #178077, #110999, #47021, #158624, #126200, #177004, #11283, #109939, #76295, #179143 ),
 ( #13421, #28621, #27544, #160751, #144548, #79496, #210555, #145615, #62191, #128347, #196453, #45955, #112076, #29695, #95776, #80565, #113136, #211611, #30766, #129408, #96846, #162893, #14476, #64319, #130463, #48096, #69618, #180206, #147710, #3548, #117394, #34996, #213728, #51270, #183391, #101068, #167155, #84827, #65351, #68553, #135728, #17667, #19813, #16604, #2476, #336, #31828, #165009, #116320, #50202, #33940, #151974, #18742, #150915, #66409, #131498, #67476, #197502, #201750, #32881, #134680, #200683, #132554, #49145, #118462, #52334, #102148, #15540, #166079, #184448, #82685, #98958, #115261, #36066, #181254, #81625, #97903, #85900, #168214, #100015, #53391, #148767, #198553, #182311, #83753, #149844, #163964, #1414, #133622, #199624, #91255, #105374, #119528, #88032, #54468, #20865, #56604, #170338, #73919, #185514, #86964, #154104, #186589, #70681, #37138, #57671, #5673, #103219, #187653, #106468, #156249, #141094, #71751, #120612, #173584, #89119, #172495, #24081, #137867, #169279, #104290, #121686, #90186, #203887, #7827, #55531, #155173, #74986, #153033, #39279, #4607, #136793, #25154, #140012, #122768, #206037, #202819, #38217, #171413, #41442, #21923, #188728, #23001, #8906, #6757, #72832, #157315, #40366, #123829, #138935, #204956, #189791, #107550, #207106, #174643, #60861, #94458, #26220, #158378, #178897, #59796, #92336, #108616, #124885, #30511, #28363, #125953, #145365, #96592, #109691, #111822, #208165, #177824, #13168, #160498, #110750, #127022, #42510, #194051, #76049, #128093, #9971, #161581, #62989, #191909, #27285, #43572, #192981, #143229, #142150, #210294, #45703, #44635, #190849, #11027, #175695, #29441, #162641, #146410, #14215, #80310, #93391, #112885, #79246, #176748, #211364, #209219, #58733, #95532, #159428, #77105, #12103, #129158, #195135, #46771, #78173, #144301, #61935, #35814, #15290, #212423, #116063, #166899, #2220, #165827, #182053, #64065, #66150, #82429, #213480, #147459, #34741, #113955, #134428, #81375, #52078, #150657, #65104, #49942, #163708, #130209, #17411, #18491, #167956, #101891, #197247, #132295, #47844, #48886, #100814, #115005, #84570, #33683, #68295, #118205, #198301, #1161, #67224, #200431, #131260, #99759, #179951, #19560, #83495, #85, #149577, #199366, #181003, #32623, #98700, #164759, #196202, #16349, #148519, #133359, #51012, #117133, #183136, #184192, #85636, #31574, #97649, #70424, #173310, #188466, #189533, #57405, #202560, #41181, #37961, #107288, #119269, #53138, #3294, #123571, #72574, #5420, #24889, #120350, #4356, #54212, #186326, #104034, #135471, #170080, #102960, #105111, #151722, #137610, #69362, #21667, #86705, #185254, #88860, #87774, #106210, #201492, #36878, #153849, #136541, #169019, #20617, #89929, #71499, #152774, #203626, #138674, #40098, #55277, #121426, #187396, #205777, #39028, #204694, #56344, #171152, #22742, #154915, #6499, #122505, #172236, #23824, #155980, #7567, #73653, #139752, #43312, #124630, #8646, #145096, #111554, #94198, #177563, #74725, #190588, #159169, #12897, #206843, #160238, #90994, #194866, #157057, #58475, #128885, #28103, #11837, #42245, #176492, #77915, #140830, #178633, #108358, #93130, #126755, #174380, #25960, #211100, #92065, #158123, #9714, #144034, #210030, #61671, #75790, #193791, #46499, #142962 ),
 ( #10769, #127839, #45440, #95265, #141898, #76843, #207908, #112623, #60597, #208964, #192716, #29175, #59529, #125689, #191647, #109431, #175437, #27022, #44370, #110493, #161313, #78976, #62724, #196999, #96329, #149321, #1968, #117951, #200180, #51833, #163448, #84315, #199104, #32376, #133106, #114751, #150400, #899, #13962, #30245, #31314, #66967, #99510, #182877, #166640, #68032, #50749, #134172, #47581, #162384, #148268, #116878, #34493, #198055, #214267, #80046, #98441, #180749, #97392, #179699, #100567, #146149, #18231, #113695, #212164, #63799, #15028, #82174, #195945, #129957, #49685, #81119, #147205, #213230, #64862, #164506, #131007, #48634, #16090, #65900, #132046, #115812, #181800, #33433, #165567, #17162, #83236, #188209, #135230, #37707, #19304, #7313, #153597, #186072, #103783, #170900, #20372, #86457, #201243, #152521, #167702, #36625, #102709, #52884, #169834, #185000, #168767, #4106, #139495, #70175, #73392, #136287, #205523, #6246, #57157, #89680, #202307, #183946, #53957, #35556, #101636, #155729, #5168, #120095, #56094, #85384, #21421, #22492, #119019, #88604, #138420, #71242, #87530, #137358, #151468, #104856, #203375, #38774, #55027, #72315, #39848, #121176, #187145, #154660, #204440, #122250, #105955, #171979, #23571, #3039, #69108, #192471, #123322, #12655, #189285, #90746, #161062, #60346, #44125, #156807, #208720, #126507, #173057, #210860, #24637, #125441, #158928, #8394, #74477, #28929, #124381, #140584, #206594, #110245, #176254, #27855, #58223, #11594, #78726, #175194, #177315, #174136, #159993, #157876, #40927, #108109, #59282, #207663, #191402, #95013, #93952, #77668, #9469, #190339, #10524, #42001, #144853, #25710, #143788, #209783, #75541, #91818, #61422, #127589, #45197, #141651, #109181, #193555, #43068, #26779, #92883, #111311, #76598, #142711, #107031, #165313, #98206, #14785, #66704, #47331, #145910, #129712, #113445, #195695, #194615, #179451, #96082, #48396, #16908, #146966, #62485, #31072, #211922, #178386, #164256, #97148, #197805, #128649, #162136, #163202, #80876, #79798, #46257, #99265, #212982, #112375, #196756, #131798, #181555, #29997, #64621, #130760, #13725, #65651, #82988, #149063, #114509, #63556, #33183, #180505, #32125, #640, #15844, #81930, #148016, #214027, #49440, #115559, #195198, #143286, #94519, #64132, #46835, #208221, #31638, #11088, #47911, #161642, #79310, #43632, #95594, #13237, #59853, #97715, #126005, #12165, #45766, #191966, #109747, #130276, #77165, #175757, #27349, #145426, #211427, #129224, #93451, #112949, #180017, #62000, #196264, #60924, #178960, #44698, #76103, #209277, #160557, #78237, #144359, #114021, #63057, #30575, #110805, #159489, #111884, #127081, #10028, #193044, #96656, #162709, #176810, #28426, #14281, #80376, #146471, #210360, #128156, #212490, #194116, #177888, #29501, #142206, #131321, #65166, #15351, #69426, #84632, #17476, #36943, #132364, #16414, #150, #198366, #66216, #147522, #116130, #115073, #117199, #135532, #149642, #163773, #50006, #98767, #197314, #100878, #182118, #118267, #81444, #48955, #33747, #82494, #181069, #213543, #101953, #99825, #32687, #83560, #150723, #200495, #185320, #165891, #164823, #3356, #133425, #2283, #68359, #1224, #148581, #67286, #199432, #134492, #51074, #52139, #183197, #34803, #119333, #166965 ),
 ( #18555, #184251, #35878, #53202, #168020, #19624, #85695, #151783, #201556, #38024, #139811, #4414, #24954, #186387, #157117, #41241, #170144, #154974, #54275, #103024, #122566, #57472, #58533, #206902, #87840, #22806, #152839, #153911, #205839, #5481, #123632, #138736, #107348, #8706, #171212, #106273, #172294, #173370, #120412, #88921, #70485, #140891, #72639, #105175, #6559, #89988, #71562, #137669, #104095, #203690, #86768, #21730, #55337, #121489, #204754, #187461, #39089, #56405, #124688, #188528, #190646, #40159, #169079, #189595, #20678, #74790, #23882, #136601, #156039, #202625, #7628, #73713, #91056, #43370, #128947, #14017, #93195, #95329, #191712, #161378, #211160, #144098, #94259, #110551, #26019, #177629, #59593, #111617, #207967, #145154, #46562, #109492, #10827, #175499, #44434, #126819, #125750, #193851, #29237, #176553, #108421, #209020, #174443, #12962, #80104, #130015, #212225, #63859, #27087, #28163, #210093, #79039, #159226, #192776, #96391, #62784, #92129, #42306, #76901, #194925, #112682, #178692, #30306, #162442, #146208, #158183, #143025, #9775, #160298, #75848, #141955, #61732, #11901, #60656, #77975, #45501, #127900, #153376, #196006, #97449, #167494, #51620, #150191, #47641, #137139, #19090, #113752, #52670, #185853, #21205, #6029, #85170, #133965, #38563, #168555, #37485, #103562, #151254, #179756, #183736, #201028, #169622, #2824, #87307, #68894, #20154, #154450, #31373, #84104, #136069, #118800, #102491, #4947, #202083, #71024, #166424, #18015, #184786, #120959, #1760, #53742, #67818, #88381, #199972, #117745, #22272, #119875, #203166, #35343, #69957, #54811, #101422, #72098, #135014, #36412, #86240, #152311, #3887, #104638, #186931, #170685, #187996, #9256, #75326, #42854, #171756, #26564, #93735, #190131, #192252, #189075, #174981, #172842, #204221, #123115, #74267, #8183, #206379, #110029, #141443, #108961, #24414, #23351, #25499, #89461, #27634, #205305, #207449, #92670, #90527, #155514, #76386, #158714, #60136, #39621, #124169, #10311, #40708, #56943, #7096, #142494, #105726, #73168, #55873, #43915, #59068, #58005, #11373, #106812, #156589, #140360, #41787, #107900, #122030, #173926, #139274, #91607, #176042, #157658, #138208, #125229, #191187, #126293, #208501, #159774, #31921, #194404, #144635, #28712, #114300, #44982, #193337, #143571, #197595, #212774, #145708, #165106, #46046, #210650, #128438, #112167, #178170, #61209, #29786, #94798, #30861, #49238, #63342, #77453, #95871, #12439, #111091, #14570, #161926, #98000, #209563, #177097, #13516, #62277, #160847, #127366, #15636, #79588, #78518, #211706, #64410, #180299, #99051, #129501, #195482, #131593, #47115, #130555, #196546, #113233, #179237, #96938, #162989, #48189, #80665, #164057, #146756, #81723, #32975, #147806, #213824, #65442, #115357, #181349, #37237, #19904, #103308, #148856, #50295, #84915, #153124, #132640, #85989, #16698, #120702, #82783, #198646, #54556, #168306, #152063, #116413, #102235, #3633, #66501, #104382, #182404, #18831, #52426, #34033, #100106, #136884, #17755, #166166, #83844, #69712, #135815, #201838, #149933, #119621, #186677, #68643, #70770, #67568, #53483, #51364, #430, #1502, #167243, #101157, #151003, #202911, #185605, #169370, #117487, #133712, #118551, #199718, #38305, #183478, #20954, #87052, #35086 ),
 ( #2573, #134766, #4695, #200774, #184533, #36156, #173672, #42601, #88126, #203973, #24166, #92422, #71845, #25247, #170429, #59887, #22016, #137953, #208253, #107640, #91347, #55620, #41528, #157409, #5764, #43664, #121777, #172587, #206128, #187744, #39372, #76138, #171502, #105469, #23094, #9000, #75075, #141188, #89210, #58823, #126036, #7923, #10062, #6844, #207198, #205052, #154196, #155263, #106559, #40456, #90269, #142241, #124976, #190937, #56694, #72922, #57758, #139028, #191999, #122861, #108707, #174736, #188822, #156338, #26309, #158462, #74009, #140101, #123919, #189886, #12196, #176844, #60957, #146505, #77197, #11120, #175790, #15381, #30605, #177918, #197344, #78266, #28457, #160589, #144391, #210392, #93482, #62034, #127114, #63089, #81475, #95624, #109781, #128188, #44731, #143316, #46866, #194149, #64163, #27381, #209310, #45797, #94551, #193081, #159521, #47940, #111918, #110838, #29532, #96693, #212522, #131348, #161674, #13268, #163805, #79341, #162741, #14314, #145459, #211454, #129258, #80407, #147552, #195228, #65196, #112979, #178990, #130306, #196293, #114054, #180047, #31669, #213574, #97746, #32717, #70515, #50040, #19655, #118297, #201587, #185352, #169111, #151815, #86801, #66248, #48986, #166996, #3388, #53234, #2316, #18587, #115104, #117229, #133458, #116163, #198398, #85730, #164853, #36974, #132396, #103057, #119364, #182149, #100907, #180, #181102, #68392, #69458, #4445, #152867, #33779, #183227, #98799, #99858, #135563, #165920, #20707, #84665, #136630, #16445, #34833, #52171, #184283, #82525, #17505, #150754, #148611, #83593, #134521, #51104, #200525, #35909, #149675, #1256, #67314, #199462, #101984, #168053, #121521, #5509, #122597, #203719, #187491, #39121, #158216, #105204, #26051, #171241, #9805, #24988, #92164, #108455, #22837, #75880, #88951, #202657, #54306, #174475, #172325, #55367, #74824, #120444, #155005, #41275, #137699, #107384, #157151, #90019, #40191, #56438, #186418, #123664, #71590, #57505, #153941, #91091, #206938, #6590, #72669, #138767, #204785, #188560, #106303, #139842, #189627, #23914, #38056, #156076, #7662, #104127, #73747, #170173, #205871, #173407, #21761, #8743, #140924, #58567, #87869, #124721, #190681, #42340, #93226, #141987, #80138, #110585, #208001, #210126, #128981, #178726, #163537, #176587, #76932, #196039, #111650, #194960, #46596, #28199, #59627, #126853, #144133, #112714, #94293, #30341, #160333, #177662, #97480, #125784, #27120, #79071, #61768, #45536, #162477, #145189, #14049, #191746, #175531, #127936, #63891, #43401, #211195, #109524, #31406, #159258, #10859, #179786, #62821, #96426, #143058, #12996, #146241, #209053, #15122, #60689, #193888, #29270, #192811, #44469, #47673, #11937, #78009, #95362, #212257, #130046, #113784, #161412, #184027, #36709, #133192, #135313, #132134, #118041, #115900, #147290, #65984, #17246, #165659, #149410, #52965, #18322, #51918, #181885, #114837, #182966, #32462, #185085, #148355, #84405, #200266, #33521, #180835, #19388, #35643, #3123, #131096, #67056, #101722, #198141, #214354, #98531, #167793, #48723, #197085, #213322, #201327, #2052, #992, #168853, #49773, #99593, #83323, #199194, #50842, #64944, #116969, #164592, #34581, #102795, #100653, #119103, #16178, #81210, #166731, #82262, #85467, #150493, #68125 ) ),
 .UNSPECIFIED., .T., .F., .T. ) 
 B_SPLINE_SURFACE_WITH_KNOTS ( ( 4, 3, 4 ),
 ( 4, 1, 1, 1, 1, 1, 1, 1, 1, 1, 1, 1, 1, 1, 1, 1, 1, 1, 1, 1, 1, 1, 1, 1, 1, 1, 1, 1, 1, 1, 1, 1, 1, 1, 1, 1, 1, 1, 1, 1, 1, 1, 1, 1, 1, 1, 1, 1, 1, 1, 1, 1, 1, 1, 1, 1, 1, 1, 1, 1, 1, 1, 1, 1, 1, 1, 1, 1, 1, 1, 1, 1, 1, 1, 1, 1, 1, 1, 1, 1, 1, 1, 1, 1, 1, 1, 1, 1, 1, 1, 1, 1, 1, 1, 1, 1, 1, 1, 1, 1, 1, 1, 1, 1, 1, 1, 1, 1, 1, 1, 1, 1, 1, 1, 1, 1, 1, 1, 1, 1, 1, 1, 1, 1, 1, 1, 1, 1, 1, 1, 1, 1, 1, 1, 1, 1, 1, 1, 1, 1, 1, 1, 1, 1, 1, 1, 1, 1, 1, 1, 1, 1, 1, 1, 1, 1, 1, 1, 1, 1, 1, 1, 1, 1, 1, 1, 1, 1, 1, 1, 1, 1, 1, 1, 1, 1, 1, 1, 1, 1, 1, 1, 1, 1, 1, 1, 1, 1, 1, 1, 1, 1, 1, 1, 1, 1, 1, 1, 1, 1, 1, 1, 1, 1, 1, 1, 1, 1, 1, 1, 1, 1, 1, 1, 1, 1, 1, 1, 1, 1, 1, 1, 1, 1, 1, 1, 1, 1, 1, 1, 1, 1, 1, 1, 1, 1, 1, 1, 1, 1, 1, 1, 1, 1, 1, 1, 1, 1, 1, 1, 1, 1, 1, 1, 1, 1, 1, 1, 1, 1, 1, 1, 1, 1, 1, 1, 1, 1, 1, 1, 1, 1, 1, 1, 1, 1, 1, 1, 1, 1, 1, 1, 1, 1, 1, 1, 1, 1, 1, 1, 1, 1, 1, 1, 1, 1, 1, 1, 1, 1, 1, 1, 1, 1, 1, 1, 1, 1, 1, 1, 1, 1, 1, 1, 1, 1, 1, 1, 1, 1, 1, 1, 1, 1, 1, 1, 1, 1, 1, 1, 1, 1, 1, 1, 1, 1, 1, 1, 1, 1, 1, 1, 1, 1, 1, 1, 1, 1, 1, 1, 1, 1, 1, 1, 1, 1, 1, 1, 1, 1, 1, 1, 1, 1, 1, 1, 1, 1, 1, 1, 1, 1, 1, 1, 1, 1, 1, 1, 1, 1, 1, 1, 1, 1, 4 ),
 ( 0.000000000000000000, 0.5000000000000000000, 1.000000000000000000 ),
 ( 0.000000000000000000, 0.002600154539856827565, 0.005208839490340733125, 0.007813275572638063438, 0.01041576435696154809, 0.01302135854728175661, 0.01562456786780599440, 0.01822932761385693060, 0.02083324874646079461, 0.02343713590986815087, 0.02604192363554110393, 0.02864519953128016536, 0.03125045858075606309, 0.03385359029894085409, 0.03645870005206112291, 0.03906221013386886737, 0.04166657361863843057, 0.04427092160485841116, 0.04687444683368256759, 0.04947954930481244379, 0.05208268618576387260, 0.05468794662449812799, 0.05729120536831356497, 0.05989601299138836571, 0.06249988999545372931, 0.06510378435733490954, 0.06770858081828938502, 0.07031184975024351580, 0.07291710771924506118, 0.07552024060328325905, 0.07812534933470290099, 0.08072885870519988516, 0.08333322157114708695, 0.08593756915452624434, 0.08854109358761537429, 0.09114619558392741960, 0.09374933183658358538, 0.09635459170495851156, 0.09895784999447977681, 0.1015626569530685003, 0.1041665336043751944, 0.1067704272253022224, 0.1093752232910748662, 0.1119784915631429623, 0.1145837490571069844, 0.1171868814509031548, 0.1197919896162490533, 0.1223954986480551566, 0.1249998608471283579, 0.1276042081199000311, 0.1302077318846941445, 0.1328128334964322199, 0.1354159692195129883, 0.1380212286176593917, 0.1406244865514671982, 0.1432292929439143159, 0.1458331693420142072, 0.1484370623210626572, 0.1510418580899855479, 0.1536451258019158050, 0.1562503829188521542, 0.1588535149221727560, 0.1614586226195926788, 0.1640621314121666618, 0.1666664930431534797, 0.1692708401040713406, 0.1718743633000545112, 0.1744794646253388370, 0.1770825999186152189, 0.1796878589445308205, 0.1822911166222762891, 0.1848959225469683498, 0.1874997987909985397, 0.1901036912273387502, 0.1927084867977703619, 0.1953117540492253223, 0.1979170108871138589, 0.2005201425997050479, 0.2031252499273119572, 0.2057287585800815777, 0.2083331197417381819, 0.2109374666895270922, 0.2135409894161511279, 0.2161460905530729892, 0.2187492255162853672, 0.2213544842679382729, 0.2239577417892439637, 0.2265625473445374016, 0.2291664235336075273, 0.2317703155263790282, 0.2343751109966507595, 0.2369783778872631419, 0.2395836345440564008, 0.2421867660656364940, 0.2447918731215153465, 0.2473953817338825356, 0.2499997425249363969, 0.2526040894582959329, 0.2552076118149841921, 0.2578127128616094499, 0.2604158475944712281, 0.2630211061698037311, 0.2656243636342671688, 0.2682291689184919115, 0.2708330451516883230, 0.2734369368000036937, 0.2760417322684234342, 0.2786449988978000336, 0.2812502554714267355, 0.2838533869016899303, 0.2864584937839013135, 0.2890620024552456591, 0.2916663629743991848, 0.2942707099920074398, 0.2968742320781582733, 0.2994793331325310004, 0.3020824677347322962, 0.3046877262316646240, 0.3072909837388622112, 0.3098957888503254821, 0.3124996652267145181, 0.3151035566296633839, 0.3177083521945192612, 0.3203116186622446127, 0.3229168752506134110, 0.3255200066892336430, 0.3281251134958176330, 0.3307286223255002655, 0.3333329826714347410, 0.3359373298719517953, 0.3385408517869427647, 0.3411459529470890484, 0.3437490875183005223, 0.3463543460347343617, 0.3489576036842249041, 0.3515624087212146920, 0.3541662853398466204, 0.3567701765964986227, 0.3593749723560626386, 0.3619782387617029862, 0.3645834954627060198, 0.3671866270093405715, 0.3697917338383204244, 0.3723952429256875973, 0.3749996031970665444, 0.3776039506791386557, 0.3802074725223298923, 0.3828125738862612759, 0.3854157085261381011, 0.3880209671599602617, 0.3906242250512887426, 0.3932290301120778819, 0.3958329070719905363, 0.3984367982813996067, 0.4010415943339316058, 0.4036448607770379837, 0.4062501176885546794, 0.4088532494428480657, 0.4114583563922335485, 0.4140618658366201910, 0.4166662261320933647, 0.4192705739943561327, 0.4218740958650940009, 0.4244791975308115917, 0.4270823323389966175, 0.4296875911880828069, 0.4322908494207843844, 0.4348956546036337745, 0.4374995320038561619, 0.4401034232650644085, 0.4427082197088152427, 0.4453114862889279713, 0.4479167435088288185, 0.4505198755704162283, 0.4531249827382076711, 0.4557284926389418844, 0.4583328530571487147, 0.4609372013982309668, 0.4635407233958523388, 0.4661458254613498609, 0.4687489605374778323, 0.4713542196996960976, 0.4739574783732994345, 0.4765622837764619812, 0.4791661617160185016, 0.4817700531280592058, 0.4843748500612748420, 0.4869781168779269698, 0.4895833745040767959, 0.4921865069725880892, 0.4947916144567798824, 0.4973951249131855490, 0.4999994855527590265, 0.5026038344712867589, 0.5052073566951218453, 0.5078124592583899144, 0.5104155947020908579, 0.5130208542753056378, 0.5156241134893367883, 0.5182289192110610676, 0.5208327977889742888, 0.5234366894508762913, 0.5260414869718011976, 0.5286447541245218318, 0.5312500122547839654, 0.5338531452298473923, 0.5364582531284315392, 0.5390617642398328746, 0.5416661251994032700, 0.5442704747940029231, 0.5468739973433798252, 0.5494791005024090014, 0.5520822364133124438, 0.5546874964953879550, 0.5572907563493740835, 0.5598955624879079496, 0.5624994418032033261, 0.5651033338139942463, 0.5677081320208752224, 0.5703113996091939697, 0.5729166583414331271, 0.5755197919226788805, 0.5781249003336490500, 0.5807284121993739889, 0.5833327735775721834, 0.5859371239468746939, 0.5885406469211225122, 0.5911457507739076300, 0.5937488872516457628, 0.5963541479404496082, 0.5989574085339228748, 0.6015622151875171797, 0.6041660953392257172, 0.6067699877979360057, 0.6093747867890261238, 0.6119780549124759217, 0.6145833143445629254, 0.6171864486316270826, 0.6197915576529816617, 0.6223950703723655220, 0.6249994322678273928, 0.6276037835104713025, 0.6302073070089242446, 0.6328124116534677990, 0.6354155487976793637, 0.6380208101910863627, 0.6406240716235875876, 0.6432288788904997334, 0.6458327599776627626, 0.6484366529833293091, 0.6510414528568908565, 0.6536447216150126360, 0.6562499818448275235, 0.6588531169373553764, 0.6614582266671018562, 0.6640617403394915019, 0.6666661028508605868, 0.6692704550654967610, 0.6718739791874978051, 0.6744790847218130603, 0.6770822226321474568, 0.6796874848280434200, 0.6822907471991253026, 0.6848955551776233497, 0.6874994372992955238, 0.6901033309509650993, 0.6927081318052739078, 0.6953114012976200353, 0.6979166624230551674, 0.7005197984207056638, 0.7031249089568636368, 0.7057284236816204759, 0.7083327869075525252, 0.7109371401928469281, 0.7135406650377511539, 0.7161457715598668061, 0.7187489103359874232, 0.7213541734322722609, 0.7239574368415039318, 0.7265622456298695964, 0.7291661288851226663, 0.7317700232818561412, 0.7343748252152053624, 0.7369780955413426371, 0.7395833576603073611, 0.7421864946627563242, 0.7447916061033615920, 0.7473951219798656842, 0.7499994860190324353, 0.7526038404736700160, 0.7552073661408488237, 0.7578124737488122209, 0.7604156134903999886, 0.7630208775849919300, 0.7656241421319622820, 0.7682289518284949326, 0.7708328363164217434, 0.7734367315572975299, 0.7760415346680002990, 0.7786448059275148381, 0.7812500691379388185, 0.7838532072448821664, 0.7864583196879902927, 0.7890618368156444573, 0.7916662017667361884, 0.7942705574894247667, 0.7968740840782696511, 0.7994791928701499018, 0.8020823336769073997, 0.8046875988677468783, 0.8072908646520678966, 0.8098956753550886623, 0.8124995611748068169, 0.8151034573589240884, 0.8177082617453185209, 0.8203115340378186460, 0.8229167984376549727, 0.8255199377488137147, 0.8281250512925039109, 0.8307285697707365024, 0.8333329357324672504, 0.8359372928219411802, 0.8385408204318668401, 0.8411459305057594760, 0.8437490724774151518, 0.8463543388624672481, 0.8489576059837783406, 0.8515624177916331083, 0.8541663050422881875, 0.8567702022687715413, 0.8593750080292236193, 0.8619782814543437421, 0.8645835471415733720, 0.8671866877566964948, 0.8697918024990743957, 0.8723953224273439666, 0.8749996894984543028, 0.8776040480534781363, 0.8802075767839265819, 0.8828126882379567775, 0.8854158314742670566, 0.8880210991515266050, 0.8906243677094983768, 0.8932291807205616774, 0.8958330695013316802, 0.8984369678693342465, 0.9010417751022415933, 0.9036450497596462128, 0.9062503168322812996, 0.9088534588511494317, 0.9114585748903522022, 0.9140620963681507227, 0.9166664646474114164, 0.9192708247667824573, 0.9218743547172278952, 0.9244794676495572405, 0.9270826122503010858, 0.9296878813177945622, 0.9322911514121841048, 0.9348959657248061550, 0.9374998561347748227, 0.9401037557438677306, 0.9427085645475906661, 0.9453118405358371668, 0.9479171090940153865, 0.9505202526155902554, 0.9531253700418979014, 0.9557288931959170286, 0.9583332627756006028, 0.9609376244112938226, 0.9635411559431285022, 0.9661462708106475228, 0.9687494151757961580, 0.9713546862302190332, 0.9739579640138142924, 0.9765627705390533819, 0.9791666547386930208, 0.9817705986233274951, 0.9843753609709087193, 0.9869785915570626900, 0.9895841932699848131, 0.9921866851465583892, 0.9947911401134668097, 0.9973998225951543617, 1.000000000000000000 ),
 .UNSPECIFIED. ) 
 GEOMETRIC_REPRESENTATION_ITEM ( )  RATIONAL_B_SPLINE_SURFACE ( (
 ( 1.000000000000000000, 1.000000000000000000, 1.000000000000000222, 1.000000000000000000, 0.9999999999999996669, 1.000000000000000444, 0.9999999999999997780, 1.000000000000000000, 1.000000000000000222, 0.9999999999999996669, 1.000000000000000222, 0.9999999999999996669, 1.000000000000000000, 0.9999999999999997780, 1.000000000000000222, 0.9999999999999997780, 1.000000000000000222, 1.000000000000000222, 0.9999999999999997780, 1.000000000000000222, 1.000000000000000222, 0.9999999999999996669, 1.000000000000000444, 0.9999999999999997780, 1.000000000000000000, 1.000000000000000222, 1.000000000000000000, 1.000000000000000000, 1.000000000000000000, 1.000000000000000000, 1.000000000000000222, 1.000000000000000000, 1.000000000000000000, 0.9999999999999997780, 1.000000000000000000, 1.000000000000000000, 1.000000000000000000, 1.000000000000000000, 0.9999999999999997780, 1.000000000000000222, 1.000000000000000000, 1.000000000000000000, 1.000000000000000444, 0.9999999999999997780, 1.000000000000000222, 0.9999999999999996669, 1.000000000000000444, 0.9999999999999997780, 1.000000000000000000, 0.9999999999999997780, 1.000000000000000000, 1.000000000000000222, 0.9999999999999997780, 1.000000000000000444, 0.9999999999999997780, 1.000000000000000000, 0.9999999999999996669, 1.000000000000000444, 0.9999999999999997780, 1.000000000000000444, 1.000000000000000000, 1.000000000000000444, 0.9999999999999996669, 1.000000000000000000, 0.9999999999999996669, 1.000000000000000444, 0.9999999999999997780, 1.000000000000000000, 1.000000000000000000, 1.000000000000000000, 1.000000000000000000, 0.9999999999999996669, 1.000000000000000000, 1.000000000000000222, 0.9999999999999997780, 1.000000000000000000, 0.9999999999999997780, 0.9999999999999997780, 1.000000000000000000, 1.000000000000000222, 0.9999999999999997780, 1.000000000000000000, 1.000000000000000222, 1.000000000000000222, 1.000000000000000222, 0.9999999999999997780, 1.000000000000000000, 1.000000000000000222, 0.9999999999999997780, 1.000000000000000222, 1.000000000000000222, 0.9999999999999997780, 0.9999999999999997780, 0.9999999999999997780, 1.000000000000000444, 1.000000000000000000, 1.000000000000000000, 1.000000000000000000, 1.000000000000000222, 0.9999999999999997780, 1.000000000000000000, 1.000000000000000444, 0.9999999999999996669, 1.000000000000000444, 1.000000000000000000, 1.000000000000000000, 1.000000000000000222, 0.9999999999999997780, 1.000000000000000444, 0.9999999999999996669, 1.000000000000000444, 1.000000000000000000, 0.9999999999999997780, 1.000000000000000222, 0.9999999999999996669, 1.000000000000000222, 1.000000000000000000, 1.000000000000000222, 0.9999999999999997780, 1.000000000000000222, 0.9999999999999996669, 1.000000000000000222, 1.000000000000000222, 1.000000000000000222, 1.000000000000000000, 0.9999999999999997780, 1.000000000000000000, 0.9999999999999997780, 1.000000000000000000, 0.9999999999999997780, 0.9999999999999997780, 1.000000000000000222, 1.000000000000000222, 1.000000000000000222, 0.9999999999999997780, 0.9999999999999997780, 1.000000000000000444, 0.9999999999999997780, 1.000000000000000000, 0.9999999999999997780, 1.000000000000000000, 0.9999999999999997780, 1.000000000000000222, 1.000000000000000000, 1.000000000000000000, 1.000000000000000222, 1.000000000000000000, 0.9999999999999997780, 1.000000000000000444, 1.000000000000000000, 1.000000000000000000, 1.000000000000000444, 0.9999999999999997780, 1.000000000000000222, 0.9999999999999997780, 1.000000000000000444, 1.000000000000000000, 1.000000000000000222, 0.9999999999999997780, 0.9999999999999997780, 1.000000000000000000, 1.000000000000000444, 0.9999999999999996669, 1.000000000000000000, 1.000000000000000222, 1.000000000000000222, 0.9999999999999997780, 1.000000000000000222, 0.9999999999999997780, 1.000000000000000222, 1.000000000000000000, 1.000000000000000000, 0.9999999999999997780, 1.000000000000000444, 0.9999999999999997780, 1.000000000000000222, 0.9999999999999996669, 1.000000000000000444, 0.9999999999999996669, 1.000000000000000222, 1.000000000000000000, 1.000000000000000000, 1.000000000000000000, 1.000000000000000444, 1.000000000000000222, 0.9999999999999997780, 1.000000000000000444, 0.9999999999999997780, 1.000000000000000000, 0.9999999999999996669, 1.000000000000000000, 0.9999999999999996669, 1.000000000000000000, 1.000000000000000222, 1.000000000000000000, 0.9999999999999997780, 1.000000000000000222, 1.000000000000000000, 1.000000000000000222, 0.9999999999999996669, 1.000000000000000000, 1.000000000000000000, 1.000000000000000000, 0.9999999999999997780, 1.000000000000000000, 1.000000000000000000, 1.000000000000000222, 1.000000000000000000, 1.000000000000000000, 0.9999999999999997780, 1.000000000000000000, 1.000000000000000222, 0.9999999999999997780, 1.000000000000000000, 1.000000000000000222, 1.000000000000000000, 1.000000000000000000, 0.9999999999999997780, 0.9999999999999997780, 1.000000000000000000, 1.000000000000000000, 0.9999999999999997780, 1.000000000000000000, 1.000000000000000000, 1.000000000000000000, 1.000000000000000222, 1.000000000000000000, 1.000000000000000000, 0.9999999999999997780, 1.000000000000000000, 0.9999999999999997780, 1.000000000000000444, 0.9999999999999997780, 1.000000000000000222, 0.9999999999999997780, 1.000000000000000444, 0.9999999999999994449, 1.000000000000000444, 0.9999999999999997780, 1.000000000000000222, 1.000000000000000000, 1.000000000000000000, 0.9999999999999997780, 1.000000000000000000, 1.000000000000000000, 0.9999999999999997780, 1.000000000000000000, 1.000000000000000000, 0.9999999999999997780, 1.000000000000000222, 1.000000000000000000, 1.000000000000000222, 0.9999999999999997780, 1.000000000000000222, 0.9999999999999997780, 1.000000000000000222, 0.9999999999999997780, 1.000000000000000444, 0.9999999999999996669, 1.000000000000000222, 0.9999999999999997780, 1.000000000000000000, 1.000000000000000000, 1.000000000000000000, 1.000000000000000222, 1.000000000000000222, 1.000000000000000000, 1.000000000000000444, 1.000000000000000222, 0.9999999999999997780, 1.000000000000000222, 0.9999999999999996669, 1.000000000000000444, 0.9999999999999997780, 0.9999999999999997780, 1.000000000000000222, 1.000000000000000000, 1.000000000000000222, 1.000000000000000000, 1.000000000000000000, 1.000000000000000222, 1.000000000000000000, 0.9999999999999997780, 1.000000000000000222, 0.9999999999999997780, 1.000000000000000000, 1.000000000000000222, 1.000000000000000000, 0.9999999999999997780, 0.9999999999999997780, 1.000000000000000000, 0.9999999999999997780, 1.000000000000000000, 1.000000000000000000, 1.000000000000000000, 1.000000000000000222, 0.9999999999999997780, 1.000000000000000000, 1.000000000000000222, 1.000000000000000000, 0.9999999999999997780, 1.000000000000000000, 1.000000000000000000, 1.000000000000000222, 0.9999999999999997780, 1.000000000000000222, 1.000000000000000000, 1.000000000000000000, 1.000000000000000222, 1.000000000000000000, 1.000000000000000000, 1.000000000000000222, 1.000000000000000000, 1.000000000000000444, 0.9999999999999996669, 1.000000000000000444, 0.9999999999999997780, 1.000000000000000000, 1.000000000000000222, 0.9999999999999996669, 1.000000000000000444, 1.000000000000000000, 1.000000000000000000, 1.000000000000000222, 1.000000000000000444, 1.000000000000000000, 0.9999999999999996669, 1.000000000000000444, 0.9999999999999997780, 0.9999999999999997780, 0.9999999999999997780, 1.000000000000000222, 1.000000000000000000, 0.9999999999999996669, 1.000000000000000222, 1.000000000000000000, 1.000000000000000444, 0.9999999999999997780, 1.000000000000000000, 1.000000000000000222, 1.000000000000000222, 1.000000000000000222, 1.000000000000000222, 1.000000000000000000, 1.000000000000000000, 1.000000000000000000, 1.000000000000000000, 1.000000000000000000, 1.000000000000000444, 1.000000000000000000, 0.9999999999999997780, 1.000000000000000000, 1.000000000000000222, 1.000000000000000000, 1.000000000000000222, 1.000000000000000222, 1.000000000000000000, 0.9999999999999997780, 0.9999999999999997780, 1.000000000000000222, 0.9999999999999997780, 1.000000000000000000, 1.000000000000000222, 1.000000000000000000, 1.000000000000000222, 1.000000000000000000, 0.9999999999999997780, 1.000000000000000000, 0.9999999999999997780, 1.000000000000000222, 1.000000000000000000, 0.9999999999999997780, 0.9999999999999997780, 1.000000000000000222, 1.000000000000000000, 1.000000000000000222, 0.9999999999999996669, 1.000000000000000000, 1.000000000000000222, 0.9999999999999997780, 1.000000000000000000, 1.000000000000000000, 1.000000000000000222, 1.000000000000000222, 1.000000000000000000, 1.000000000000000222, 1.000000000000000222),
 ( 0.3333333333333333703, 0.3333333333333333703, 0.3333333333333333703, 0.3333333333333333703, 0.3333333333333333148, 0.3333333333333334259, 0.3333333333333333703, 0.3333333333333333148, 0.3333333333333334259, 0.3333333333333333148, 0.3333333333333334259, 0.3333333333333332038, 0.3333333333333333703, 0.3333333333333332593, 0.3333333333333333703, 0.3333333333333332593, 0.3333333333333334814, 0.3333333333333334259, 0.3333333333333333703, 0.3333333333333334259, 0.3333333333333334259, 0.3333333333333332038, 0.3333333333333335369, 0.3333333333333333148, 0.3333333333333333148, 0.3333333333333334259, 0.3333333333333333703, 0.3333333333333333148, 0.3333333333333334259, 0.3333333333333333148, 0.3333333333333335369, 0.3333333333333333148, 0.3333333333333334259, 0.3333333333333333148, 0.3333333333333334259, 0.3333333333333333703, 0.3333333333333333148, 0.3333333333333333703, 0.3333333333333334259, 0.3333333333333333703, 0.3333333333333334259, 0.3333333333333333703, 0.3333333333333334814, 0.3333333333333333148, 0.3333333333333334259, 0.3333333333333332593, 0.3333333333333335369, 0.3333333333333332593, 0.3333333333333334259, 0.3333333333333333148, 0.3333333333333333703, 0.3333333333333334259, 0.3333333333333333148, 0.3333333333333334814, 0.3333333333333332593, 0.3333333333333333703, 0.3333333333333332593, 0.3333333333333335369, 0.3333333333333333148, 0.3333333333333334259, 0.3333333333333334259, 0.3333333333333334259, 0.3333333333333333148, 0.3333333333333333148, 0.3333333333333333703, 0.3333333333333333703, 0.3333333333333333703, 0.3333333333333334259, 0.3333333333333333148, 0.3333333333333333703, 0.3333333333333333703, 0.3333333333333332593, 0.3333333333333334259, 0.3333333333333333703, 0.3333333333333333703, 0.3333333333333333148, 0.3333333333333333148, 0.3333333333333334259, 0.3333333333333333148, 0.3333333333333334259, 0.3333333333333333148, 0.3333333333333334259, 0.3333333333333333703, 0.3333333333333334259, 0.3333333333333333703, 0.3333333333333333703, 0.3333333333333333148, 0.3333333333333335369, 0.3333333333333332593, 0.3333333333333334814, 0.3333333333333333703, 0.3333333333333333703, 0.3333333333333333148, 0.3333333333333333703, 0.3333333333333334259, 0.3333333333333334259, 0.3333333333333333148, 0.3333333333333333703, 0.3333333333333334259, 0.3333333333333333148, 0.3333333333333333703, 0.3333333333333334814, 0.3333333333333332038, 0.3333333333333334814, 0.3333333333333333703, 0.3333333333333333148, 0.3333333333333334259, 0.3333333333333333148, 0.3333333333333334259, 0.3333333333333332593, 0.3333333333333333703, 0.3333333333333334259, 0.3333333333333333148, 0.3333333333333333703, 0.3333333333333333148, 0.3333333333333334259, 0.3333333333333333703, 0.3333333333333333703, 0.3333333333333333703, 0.3333333333333334259, 0.3333333333333332038, 0.3333333333333334259, 0.3333333333333334259, 0.3333333333333333703, 0.3333333333333333703, 0.3333333333333332593, 0.3333333333333333703, 0.3333333333333333148, 0.3333333333333334259, 0.3333333333333332593, 0.3333333333333334259, 0.3333333333333333703, 0.3333333333333334259, 0.3333333333333334259, 0.3333333333333333148, 0.3333333333333334259, 0.3333333333333334259, 0.3333333333333332593, 0.3333333333333334259, 0.3333333333333333703, 0.3333333333333333703, 0.3333333333333333148, 0.3333333333333334259, 0.3333333333333333703, 0.3333333333333334259, 0.3333333333333334259, 0.3333333333333333703, 0.3333333333333333703, 0.3333333333333334814, 0.3333333333333333703, 0.3333333333333333703, 0.3333333333333335369, 0.3333333333333332593, 0.3333333333333334259, 0.3333333333333333148, 0.3333333333333334259, 0.3333333333333334259, 0.3333333333333334259, 0.3333333333333332593, 0.3333333333333333148, 0.3333333333333333703, 0.3333333333333334259, 0.3333333333333333148, 0.3333333333333333703, 0.3333333333333333148, 0.3333333333333334259, 0.3333333333333333148, 0.3333333333333334259, 0.3333333333333333148, 0.3333333333333334259, 0.3333333333333333703, 0.3333333333333334259, 0.3333333333333333703, 0.3333333333333334259, 0.3333333333333333148, 0.3333333333333333703, 0.3333333333333333703, 0.3333333333333334259, 0.3333333333333333703, 0.3333333333333334259, 0.3333333333333333703, 0.3333333333333333703, 0.3333333333333334259, 0.3333333333333334814, 0.3333333333333333703, 0.3333333333333333703, 0.3333333333333334814, 0.3333333333333333148, 0.3333333333333333703, 0.3333333333333333148, 0.3333333333333333703, 0.3333333333333333148, 0.3333333333333334259, 0.3333333333333334259, 0.3333333333333333703, 0.3333333333333333703, 0.3333333333333333703, 0.3333333333333333703, 0.3333333333333334259, 0.3333333333333332593, 0.3333333333333333703, 0.3333333333333333703, 0.3333333333333333703, 0.3333333333333333148, 0.3333333333333333703, 0.3333333333333333148, 0.3333333333333334259, 0.3333333333333333148, 0.3333333333333333703, 0.3333333333333333703, 0.3333333333333334259, 0.3333333333333333703, 0.3333333333333333148, 0.3333333333333333703, 0.3333333333333333703, 0.3333333333333333148, 0.3333333333333333703, 0.3333333333333333148, 0.3333333333333333703, 0.3333333333333333703, 0.3333333333333334814, 0.3333333333333333148, 0.3333333333333334259, 0.3333333333333334259, 0.3333333333333333703, 0.3333333333333334259, 0.3333333333333333703, 0.3333333333333334259, 0.3333333333333332593, 0.3333333333333334259, 0.3333333333333333148, 0.3333333333333334259, 0.3333333333333333148, 0.3333333333333334259, 0.3333333333333332593, 0.3333333333333335369, 0.3333333333333332038, 0.3333333333333334259, 0.3333333333333333703, 0.3333333333333333148, 0.3333333333333334259, 0.3333333333333333148, 0.3333333333333333148, 0.3333333333333333148, 0.3333333333333334814, 0.3333333333333332593, 0.3333333333333334259, 0.3333333333333333148, 0.3333333333333333148, 0.3333333333333334814, 0.3333333333333333703, 0.3333333333333334259, 0.3333333333333333148, 0.3333333333333333703, 0.3333333333333332593, 0.3333333333333334814, 0.3333333333333333148, 0.3333333333333334259, 0.3333333333333333148, 0.3333333333333334259, 0.3333333333333333703, 0.3333333333333333703, 0.3333333333333334259, 0.3333333333333333148, 0.3333333333333334814, 0.3333333333333333703, 0.3333333333333333703, 0.3333333333333334814, 0.3333333333333333703, 0.3333333333333332593, 0.3333333333333334259, 0.3333333333333332593, 0.3333333333333334814, 0.3333333333333333148, 0.3333333333333333703, 0.3333333333333333703, 0.3333333333333334259, 0.3333333333333333703, 0.3333333333333333703, 0.3333333333333333148, 0.3333333333333334259, 0.3333333333333334259, 0.3333333333333333703, 0.3333333333333334259, 0.3333333333333333148, 0.3333333333333333703, 0.3333333333333334259, 0.3333333333333333703, 0.3333333333333333148, 0.3333333333333334259, 0.3333333333333333703, 0.3333333333333333148, 0.3333333333333333148, 0.3333333333333334259, 0.3333333333333333148, 0.3333333333333333703, 0.3333333333333333703, 0.3333333333333333703, 0.3333333333333334259, 0.3333333333333334259, 0.3333333333333333148, 0.3333333333333334259, 0.3333333333333333148, 0.3333333333333334814, 0.3333333333333332593, 0.3333333333333334814, 0.3333333333333333703, 0.3333333333333333703, 0.3333333333333334259, 0.3333333333333333703, 0.3333333333333333703, 0.3333333333333333703, 0.3333333333333333703, 0.3333333333333334814, 0.3333333333333333148, 0.3333333333333334259, 0.3333333333333333148, 0.3333333333333333703, 0.3333333333333333703, 0.3333333333333333703, 0.3333333333333335369, 0.3333333333333333703, 0.3333333333333333148, 0.3333333333333334814, 0.3333333333333334259, 0.3333333333333333148, 0.3333333333333333148, 0.3333333333333335369, 0.3333333333333332593, 0.3333333333333333703, 0.3333333333333333148, 0.3333333333333333703, 0.3333333333333333703, 0.3333333333333332593, 0.3333333333333334259, 0.3333333333333332593, 0.3333333333333335369, 0.3333333333333333148, 0.3333333333333333703, 0.3333333333333334259, 0.3333333333333333703, 0.3333333333333333703, 0.3333333333333334814, 0.3333333333333333148, 0.3333333333333333148, 0.3333333333333334259, 0.3333333333333333148, 0.3333333333333333703, 0.3333333333333334814, 0.3333333333333333703, 0.3333333333333333703, 0.3333333333333333703, 0.3333333333333333703, 0.3333333333333334814, 0.3333333333333333703, 0.3333333333333334814, 0.3333333333333333703, 0.3333333333333333703, 0.3333333333333333148, 0.3333333333333334259, 0.3333333333333333148, 0.3333333333333334259, 0.3333333333333333148, 0.3333333333333333703, 0.3333333333333334814, 0.3333333333333333148, 0.3333333333333333148, 0.3333333333333333703, 0.3333333333333333703, 0.3333333333333333703, 0.3333333333333334259, 0.3333333333333333148, 0.3333333333333333703, 0.3333333333333334259, 0.3333333333333333148, 0.3333333333333333703, 0.3333333333333332593, 0.3333333333333333703, 0.3333333333333334259, 0.3333333333333333703, 0.3333333333333333703, 0.3333333333333333703, 0.3333333333333333703, 0.3333333333333334814, 0.3333333333333333703, 0.3333333333333334259, 0.3333333333333334259),
 ( 0.3333333333333333703, 0.3333333333333333703, 0.3333333333333333703, 0.3333333333333333703, 0.3333333333333333148, 0.3333333333333334259, 0.3333333333333333703, 0.3333333333333333148, 0.3333333333333334259, 0.3333333333333333148, 0.3333333333333334259, 0.3333333333333332038, 0.3333333333333333703, 0.3333333333333332593, 0.3333333333333333703, 0.3333333333333332593, 0.3333333333333334814, 0.3333333333333334259, 0.3333333333333333703, 0.3333333333333334259, 0.3333333333333334259, 0.3333333333333332038, 0.3333333333333335369, 0.3333333333333333148, 0.3333333333333333148, 0.3333333333333334259, 0.3333333333333333703, 0.3333333333333333148, 0.3333333333333334259, 0.3333333333333333148, 0.3333333333333335369, 0.3333333333333333148, 0.3333333333333334259, 0.3333333333333333148, 0.3333333333333334259, 0.3333333333333333703, 0.3333333333333333148, 0.3333333333333333703, 0.3333333333333334259, 0.3333333333333333703, 0.3333333333333334259, 0.3333333333333333703, 0.3333333333333334814, 0.3333333333333333148, 0.3333333333333334259, 0.3333333333333332593, 0.3333333333333335369, 0.3333333333333332593, 0.3333333333333334259, 0.3333333333333333148, 0.3333333333333333703, 0.3333333333333334259, 0.3333333333333333148, 0.3333333333333334814, 0.3333333333333332593, 0.3333333333333333703, 0.3333333333333332593, 0.3333333333333335369, 0.3333333333333333148, 0.3333333333333334259, 0.3333333333333334259, 0.3333333333333334259, 0.3333333333333333148, 0.3333333333333333148, 0.3333333333333333703, 0.3333333333333333703, 0.3333333333333333703, 0.3333333333333334259, 0.3333333333333333148, 0.3333333333333333703, 0.3333333333333333703, 0.3333333333333332593, 0.3333333333333334259, 0.3333333333333333703, 0.3333333333333333703, 0.3333333333333333148, 0.3333333333333333148, 0.3333333333333334259, 0.3333333333333333148, 0.3333333333333334259, 0.3333333333333333148, 0.3333333333333334259, 0.3333333333333333703, 0.3333333333333334259, 0.3333333333333333703, 0.3333333333333333703, 0.3333333333333333148, 0.3333333333333335369, 0.3333333333333332593, 0.3333333333333334814, 0.3333333333333333703, 0.3333333333333333703, 0.3333333333333333148, 0.3333333333333333703, 0.3333333333333334259, 0.3333333333333334259, 0.3333333333333333148, 0.3333333333333333703, 0.3333333333333334259, 0.3333333333333333148, 0.3333333333333333703, 0.3333333333333334814, 0.3333333333333332038, 0.3333333333333334814, 0.3333333333333333703, 0.3333333333333333148, 0.3333333333333334259, 0.3333333333333333148, 0.3333333333333334259, 0.3333333333333332593, 0.3333333333333333703, 0.3333333333333334259, 0.3333333333333333148, 0.3333333333333333703, 0.3333333333333333148, 0.3333333333333334259, 0.3333333333333333703, 0.3333333333333333703, 0.3333333333333333703, 0.3333333333333334259, 0.3333333333333332038, 0.3333333333333334259, 0.3333333333333334259, 0.3333333333333333703, 0.3333333333333333703, 0.3333333333333332593, 0.3333333333333333703, 0.3333333333333333148, 0.3333333333333334259, 0.3333333333333332593, 0.3333333333333334259, 0.3333333333333333703, 0.3333333333333334259, 0.3333333333333334259, 0.3333333333333333148, 0.3333333333333334259, 0.3333333333333334259, 0.3333333333333332593, 0.3333333333333334259, 0.3333333333333333703, 0.3333333333333333703, 0.3333333333333333148, 0.3333333333333334259, 0.3333333333333333703, 0.3333333333333334259, 0.3333333333333334259, 0.3333333333333333703, 0.3333333333333333703, 0.3333333333333334814, 0.3333333333333333703, 0.3333333333333333703, 0.3333333333333335369, 0.3333333333333332593, 0.3333333333333334259, 0.3333333333333333148, 0.3333333333333334259, 0.3333333333333334259, 0.3333333333333334259, 0.3333333333333332593, 0.3333333333333333148, 0.3333333333333333703, 0.3333333333333334259, 0.3333333333333333148, 0.3333333333333333703, 0.3333333333333333148, 0.3333333333333334259, 0.3333333333333333148, 0.3333333333333334259, 0.3333333333333333148, 0.3333333333333334259, 0.3333333333333333703, 0.3333333333333334259, 0.3333333333333333703, 0.3333333333333334259, 0.3333333333333333148, 0.3333333333333333703, 0.3333333333333333703, 0.3333333333333334259, 0.3333333333333333703, 0.3333333333333334259, 0.3333333333333333703, 0.3333333333333333703, 0.3333333333333334259, 0.3333333333333334814, 0.3333333333333333703, 0.3333333333333333703, 0.3333333333333334814, 0.3333333333333333148, 0.3333333333333333703, 0.3333333333333333148, 0.3333333333333333703, 0.3333333333333333148, 0.3333333333333334259, 0.3333333333333334259, 0.3333333333333333703, 0.3333333333333333703, 0.3333333333333333703, 0.3333333333333333703, 0.3333333333333334259, 0.3333333333333332593, 0.3333333333333333703, 0.3333333333333333703, 0.3333333333333333703, 0.3333333333333333148, 0.3333333333333333703, 0.3333333333333333148, 0.3333333333333334259, 0.3333333333333333148, 0.3333333333333333703, 0.3333333333333333703, 0.3333333333333334259, 0.3333333333333333703, 0.3333333333333333148, 0.3333333333333333703, 0.3333333333333333703, 0.3333333333333333148, 0.3333333333333333703, 0.3333333333333333148, 0.3333333333333333703, 0.3333333333333333703, 0.3333333333333334814, 0.3333333333333333148, 0.3333333333333334259, 0.3333333333333334259, 0.3333333333333333703, 0.3333333333333334259, 0.3333333333333333703, 0.3333333333333334259, 0.3333333333333332593, 0.3333333333333334259, 0.3333333333333333148, 0.3333333333333334259, 0.3333333333333333148, 0.3333333333333334259, 0.3333333333333332593, 0.3333333333333335369, 0.3333333333333332038, 0.3333333333333334259, 0.3333333333333333703, 0.3333333333333333148, 0.3333333333333334259, 0.3333333333333333148, 0.3333333333333333148, 0.3333333333333333148, 0.3333333333333334814, 0.3333333333333332593, 0.3333333333333334259, 0.3333333333333333148, 0.3333333333333333148, 0.3333333333333334814, 0.3333333333333333703, 0.3333333333333334259, 0.3333333333333333148, 0.3333333333333333703, 0.3333333333333332593, 0.3333333333333334814, 0.3333333333333333148, 0.3333333333333334259, 0.3333333333333333148, 0.3333333333333334259, 0.3333333333333333703, 0.3333333333333333703, 0.3333333333333334259, 0.3333333333333333148, 0.3333333333333334814, 0.3333333333333333703, 0.3333333333333333703, 0.3333333333333334814, 0.3333333333333333703, 0.3333333333333332593, 0.3333333333333334259, 0.3333333333333332593, 0.3333333333333334814, 0.3333333333333333148, 0.3333333333333333703, 0.3333333333333333703, 0.3333333333333334259, 0.3333333333333333703, 0.3333333333333333703, 0.3333333333333333148, 0.3333333333333334259, 0.3333333333333334259, 0.3333333333333333703, 0.3333333333333334259, 0.3333333333333333148, 0.3333333333333333703, 0.3333333333333334259, 0.3333333333333333703, 0.3333333333333333148, 0.3333333333333334259, 0.3333333333333333703, 0.3333333333333333148, 0.3333333333333333148, 0.3333333333333334259, 0.3333333333333333148, 0.3333333333333333703, 0.3333333333333333703, 0.3333333333333333703, 0.3333333333333334259, 0.3333333333333334259, 0.3333333333333333148, 0.3333333333333334259, 0.3333333333333333148, 0.3333333333333334814, 0.3333333333333332593, 0.3333333333333334814, 0.3333333333333333703, 0.3333333333333333703, 0.3333333333333334259, 0.3333333333333333703, 0.3333333333333333703, 0.3333333333333333703, 0.3333333333333333703, 0.3333333333333334814, 0.3333333333333333148, 0.3333333333333334259, 0.3333333333333333148, 0.3333333333333333703, 0.3333333333333333703, 0.3333333333333333703, 0.3333333333333335369, 0.3333333333333333703, 0.3333333333333333148, 0.3333333333333334814, 0.3333333333333334259, 0.3333333333333333148, 0.3333333333333333148, 0.3333333333333335369, 0.3333333333333332593, 0.3333333333333333703, 0.3333333333333333148, 0.3333333333333333703, 0.3333333333333333703, 0.3333333333333332593, 0.3333333333333334259, 0.3333333333333332593, 0.3333333333333335369, 0.3333333333333333148, 0.3333333333333333703, 0.3333333333333334259, 0.3333333333333333703, 0.3333333333333333703, 0.3333333333333334814, 0.3333333333333333148, 0.3333333333333333148, 0.3333333333333334259, 0.3333333333333333148, 0.3333333333333333703, 0.3333333333333334814, 0.3333333333333333703, 0.3333333333333333703, 0.3333333333333333703, 0.3333333333333333703, 0.3333333333333334814, 0.3333333333333333703, 0.3333333333333334814, 0.3333333333333333703, 0.3333333333333333703, 0.3333333333333333148, 0.3333333333333334259, 0.3333333333333333148, 0.3333333333333334259, 0.3333333333333333148, 0.3333333333333333703, 0.3333333333333334814, 0.3333333333333333148, 0.3333333333333333148, 0.3333333333333333703, 0.3333333333333333703, 0.3333333333333333703, 0.3333333333333334259, 0.3333333333333333148, 0.3333333333333333703, 0.3333333333333334259, 0.3333333333333333148, 0.3333333333333333703, 0.3333333333333332593, 0.3333333333333333703, 0.3333333333333334259, 0.3333333333333333703, 0.3333333333333333703, 0.3333333333333333703, 0.3333333333333333703, 0.3333333333333334814, 0.3333333333333333703, 0.3333333333333334259, 0.3333333333333334259),
 ( 1.000000000000000000, 1.000000000000000000, 1.000000000000000222, 1.000000000000000000, 0.9999999999999996669, 1.000000000000000444, 0.9999999999999997780, 1.000000000000000000, 1.000000000000000222, 0.9999999999999996669, 1.000000000000000222, 0.9999999999999996669, 1.000000000000000000, 0.9999999999999997780, 1.000000000000000222, 0.9999999999999997780, 1.000000000000000222, 1.000000000000000222, 0.9999999999999997780, 1.000000000000000222, 1.000000000000000222, 0.9999999999999996669, 1.000000000000000444, 0.9999999999999997780, 1.000000000000000000, 1.000000000000000222, 1.000000000000000000, 1.000000000000000000, 1.000000000000000000, 1.000000000000000000, 1.000000000000000222, 1.000000000000000000, 1.000000000000000000, 0.9999999999999997780, 1.000000000000000000, 1.000000000000000000, 1.000000000000000000, 1.000000000000000000, 0.9999999999999997780, 1.000000000000000222, 1.000000000000000000, 1.000000000000000000, 1.000000000000000444, 0.9999999999999997780, 1.000000000000000222, 0.9999999999999996669, 1.000000000000000444, 0.9999999999999997780, 1.000000000000000000, 0.9999999999999997780, 1.000000000000000000, 1.000000000000000222, 0.9999999999999997780, 1.000000000000000444, 0.9999999999999997780, 1.000000000000000000, 0.9999999999999996669, 1.000000000000000444, 0.9999999999999997780, 1.000000000000000444, 1.000000000000000000, 1.000000000000000444, 0.9999999999999996669, 1.000000000000000000, 0.9999999999999996669, 1.000000000000000444, 0.9999999999999997780, 1.000000000000000000, 1.000000000000000000, 1.000000000000000000, 1.000000000000000000, 0.9999999999999996669, 1.000000000000000000, 1.000000000000000222, 0.9999999999999997780, 1.000000000000000000, 0.9999999999999997780, 0.9999999999999997780, 1.000000000000000000, 1.000000000000000222, 0.9999999999999997780, 1.000000000000000000, 1.000000000000000222, 1.000000000000000222, 1.000000000000000222, 0.9999999999999997780, 1.000000000000000000, 1.000000000000000222, 0.9999999999999997780, 1.000000000000000222, 1.000000000000000222, 0.9999999999999997780, 0.9999999999999997780, 0.9999999999999997780, 1.000000000000000444, 1.000000000000000000, 1.000000000000000000, 1.000000000000000000, 1.000000000000000222, 0.9999999999999997780, 1.000000000000000000, 1.000000000000000444, 0.9999999999999996669, 1.000000000000000444, 1.000000000000000000, 1.000000000000000000, 1.000000000000000222, 0.9999999999999997780, 1.000000000000000444, 0.9999999999999996669, 1.000000000000000444, 1.000000000000000000, 0.9999999999999997780, 1.000000000000000222, 0.9999999999999996669, 1.000000000000000222, 1.000000000000000000, 1.000000000000000222, 0.9999999999999997780, 1.000000000000000222, 0.9999999999999996669, 1.000000000000000222, 1.000000000000000222, 1.000000000000000222, 1.000000000000000000, 0.9999999999999997780, 1.000000000000000000, 0.9999999999999997780, 1.000000000000000000, 0.9999999999999997780, 0.9999999999999997780, 1.000000000000000222, 1.000000000000000222, 1.000000000000000222, 0.9999999999999997780, 0.9999999999999997780, 1.000000000000000444, 0.9999999999999997780, 1.000000000000000000, 0.9999999999999997780, 1.000000000000000000, 0.9999999999999997780, 1.000000000000000222, 1.000000000000000000, 1.000000000000000000, 1.000000000000000222, 1.000000000000000000, 0.9999999999999997780, 1.000000000000000444, 1.000000000000000000, 1.000000000000000000, 1.000000000000000444, 0.9999999999999997780, 1.000000000000000222, 0.9999999999999997780, 1.000000000000000444, 1.000000000000000000, 1.000000000000000222, 0.9999999999999997780, 0.9999999999999997780, 1.000000000000000000, 1.000000000000000444, 0.9999999999999996669, 1.000000000000000000, 1.000000000000000222, 1.000000000000000222, 0.9999999999999997780, 1.000000000000000222, 0.9999999999999997780, 1.000000000000000222, 1.000000000000000000, 1.000000000000000000, 0.9999999999999997780, 1.000000000000000444, 0.9999999999999997780, 1.000000000000000222, 0.9999999999999996669, 1.000000000000000444, 0.9999999999999996669, 1.000000000000000222, 1.000000000000000000, 1.000000000000000000, 1.000000000000000000, 1.000000000000000444, 1.000000000000000222, 0.9999999999999997780, 1.000000000000000444, 0.9999999999999997780, 1.000000000000000000, 0.9999999999999996669, 1.000000000000000000, 0.9999999999999996669, 1.000000000000000000, 1.000000000000000222, 1.000000000000000000, 0.9999999999999997780, 1.000000000000000222, 1.000000000000000000, 1.000000000000000222, 0.9999999999999996669, 1.000000000000000000, 1.000000000000000000, 1.000000000000000000, 0.9999999999999997780, 1.000000000000000000, 1.000000000000000000, 1.000000000000000222, 1.000000000000000000, 1.000000000000000000, 0.9999999999999997780, 1.000000000000000000, 1.000000000000000222, 0.9999999999999997780, 1.000000000000000000, 1.000000000000000222, 1.000000000000000000, 1.000000000000000000, 0.9999999999999997780, 0.9999999999999997780, 1.000000000000000000, 1.000000000000000000, 0.9999999999999997780, 1.000000000000000000, 1.000000000000000000, 1.000000000000000000, 1.000000000000000222, 1.000000000000000000, 1.000000000000000000, 0.9999999999999997780, 1.000000000000000000, 0.9999999999999997780, 1.000000000000000444, 0.9999999999999997780, 1.000000000000000222, 0.9999999999999997780, 1.000000000000000444, 0.9999999999999994449, 1.000000000000000444, 0.9999999999999997780, 1.000000000000000222, 1.000000000000000000, 1.000000000000000000, 0.9999999999999997780, 1.000000000000000000, 1.000000000000000000, 0.9999999999999997780, 1.000000000000000000, 1.000000000000000000, 0.9999999999999997780, 1.000000000000000222, 1.000000000000000000, 1.000000000000000222, 0.9999999999999997780, 1.000000000000000222, 0.9999999999999997780, 1.000000000000000222, 0.9999999999999997780, 1.000000000000000444, 0.9999999999999996669, 1.000000000000000222, 0.9999999999999997780, 1.000000000000000000, 1.000000000000000000, 1.000000000000000000, 1.000000000000000222, 1.000000000000000222, 1.000000000000000000, 1.000000000000000444, 1.000000000000000222, 0.9999999999999997780, 1.000000000000000222, 0.9999999999999996669, 1.000000000000000444, 0.9999999999999997780, 0.9999999999999997780, 1.000000000000000222, 1.000000000000000000, 1.000000000000000222, 1.000000000000000000, 1.000000000000000000, 1.000000000000000222, 1.000000000000000000, 0.9999999999999997780, 1.000000000000000222, 0.9999999999999997780, 1.000000000000000000, 1.000000000000000222, 1.000000000000000000, 0.9999999999999997780, 0.9999999999999997780, 1.000000000000000000, 0.9999999999999997780, 1.000000000000000000, 1.000000000000000000, 1.000000000000000000, 1.000000000000000222, 0.9999999999999997780, 1.000000000000000000, 1.000000000000000222, 1.000000000000000000, 0.9999999999999997780, 1.000000000000000000, 1.000000000000000000, 1.000000000000000222, 0.9999999999999997780, 1.000000000000000222, 1.000000000000000000, 1.000000000000000000, 1.000000000000000222, 1.000000000000000000, 1.000000000000000000, 1.000000000000000222, 1.000000000000000000, 1.000000000000000444, 0.9999999999999996669, 1.000000000000000444, 0.9999999999999997780, 1.000000000000000000, 1.000000000000000222, 0.9999999999999996669, 1.000000000000000444, 1.000000000000000000, 1.000000000000000000, 1.000000000000000222, 1.000000000000000444, 1.000000000000000000, 0.9999999999999996669, 1.000000000000000444, 0.9999999999999997780, 0.9999999999999997780, 0.9999999999999997780, 1.000000000000000222, 1.000000000000000000, 0.9999999999999996669, 1.000000000000000222, 1.000000000000000000, 1.000000000000000444, 0.9999999999999997780, 1.000000000000000000, 1.000000000000000222, 1.000000000000000222, 1.000000000000000222, 1.000000000000000222, 1.000000000000000000, 1.000000000000000000, 1.000000000000000000, 1.000000000000000000, 1.000000000000000000, 1.000000000000000444, 1.000000000000000000, 0.9999999999999997780, 1.000000000000000000, 1.000000000000000222, 1.000000000000000000, 1.000000000000000222, 1.000000000000000222, 1.000000000000000000, 0.9999999999999997780, 0.9999999999999997780, 1.000000000000000222, 0.9999999999999997780, 1.000000000000000000, 1.000000000000000222, 1.000000000000000000, 1.000000000000000222, 1.000000000000000000, 0.9999999999999997780, 1.000000000000000000, 0.9999999999999997780, 1.000000000000000222, 1.000000000000000000, 0.9999999999999997780, 0.9999999999999997780, 1.000000000000000222, 1.000000000000000000, 1.000000000000000222, 0.9999999999999996669, 1.000000000000000000, 1.000000000000000222, 0.9999999999999997780, 1.000000000000000000, 1.000000000000000000, 1.000000000000000222, 1.000000000000000222, 1.000000000000000000, 1.000000000000000222, 1.000000000000000222),
 ( 0.3333333333333333703, 0.3333333333333333703, 0.3333333333333333703, 0.3333333333333333703, 0.3333333333333333148, 0.3333333333333334259, 0.3333333333333333703, 0.3333333333333333148, 0.3333333333333334259, 0.3333333333333333148, 0.3333333333333334259, 0.3333333333333332038, 0.3333333333333333703, 0.3333333333333332593, 0.3333333333333333703, 0.3333333333333332593, 0.3333333333333334814, 0.3333333333333334259, 0.3333333333333333703, 0.3333333333333334259, 0.3333333333333334259, 0.3333333333333332038, 0.3333333333333335369, 0.3333333333333333148, 0.3333333333333333148, 0.3333333333333334259, 0.3333333333333333703, 0.3333333333333333148, 0.3333333333333334259, 0.3333333333333333148, 0.3333333333333335369, 0.3333333333333333148, 0.3333333333333334259, 0.3333333333333333148, 0.3333333333333334259, 0.3333333333333333703, 0.3333333333333333148, 0.3333333333333333703, 0.3333333333333334259, 0.3333333333333333703, 0.3333333333333334259, 0.3333333333333333703, 0.3333333333333334814, 0.3333333333333333148, 0.3333333333333334259, 0.3333333333333332593, 0.3333333333333335369, 0.3333333333333332593, 0.3333333333333334259, 0.3333333333333333148, 0.3333333333333333703, 0.3333333333333334259, 0.3333333333333333148, 0.3333333333333334814, 0.3333333333333332593, 0.3333333333333333703, 0.3333333333333332593, 0.3333333333333335369, 0.3333333333333333148, 0.3333333333333334259, 0.3333333333333334259, 0.3333333333333334259, 0.3333333333333333148, 0.3333333333333333148, 0.3333333333333333703, 0.3333333333333333703, 0.3333333333333333703, 0.3333333333333334259, 0.3333333333333333148, 0.3333333333333333703, 0.3333333333333333703, 0.3333333333333332593, 0.3333333333333334259, 0.3333333333333333703, 0.3333333333333333703, 0.3333333333333333148, 0.3333333333333333148, 0.3333333333333334259, 0.3333333333333333148, 0.3333333333333334259, 0.3333333333333333148, 0.3333333333333334259, 0.3333333333333333703, 0.3333333333333334259, 0.3333333333333333703, 0.3333333333333333703, 0.3333333333333333148, 0.3333333333333335369, 0.3333333333333332593, 0.3333333333333334814, 0.3333333333333333703, 0.3333333333333333703, 0.3333333333333333148, 0.3333333333333333703, 0.3333333333333334259, 0.3333333333333334259, 0.3333333333333333148, 0.3333333333333333703, 0.3333333333333334259, 0.3333333333333333148, 0.3333333333333333703, 0.3333333333333334814, 0.3333333333333332038, 0.3333333333333334814, 0.3333333333333333703, 0.3333333333333333148, 0.3333333333333334259, 0.3333333333333333148, 0.3333333333333334259, 0.3333333333333332593, 0.3333333333333333703, 0.3333333333333334259, 0.3333333333333333148, 0.3333333333333333703, 0.3333333333333333148, 0.3333333333333334259, 0.3333333333333333703, 0.3333333333333333703, 0.3333333333333333703, 0.3333333333333334259, 0.3333333333333332038, 0.3333333333333334259, 0.3333333333333334259, 0.3333333333333333703, 0.3333333333333333703, 0.3333333333333332593, 0.3333333333333333703, 0.3333333333333333148, 0.3333333333333334259, 0.3333333333333332593, 0.3333333333333334259, 0.3333333333333333703, 0.3333333333333334259, 0.3333333333333334259, 0.3333333333333333148, 0.3333333333333334259, 0.3333333333333334259, 0.3333333333333332593, 0.3333333333333334259, 0.3333333333333333703, 0.3333333333333333703, 0.3333333333333333148, 0.3333333333333334259, 0.3333333333333333703, 0.3333333333333334259, 0.3333333333333334259, 0.3333333333333333703, 0.3333333333333333703, 0.3333333333333334814, 0.3333333333333333703, 0.3333333333333333703, 0.3333333333333335369, 0.3333333333333332593, 0.3333333333333334259, 0.3333333333333333148, 0.3333333333333334259, 0.3333333333333334259, 0.3333333333333334259, 0.3333333333333332593, 0.3333333333333333148, 0.3333333333333333703, 0.3333333333333334259, 0.3333333333333333148, 0.3333333333333333703, 0.3333333333333333148, 0.3333333333333334259, 0.3333333333333333148, 0.3333333333333334259, 0.3333333333333333148, 0.3333333333333334259, 0.3333333333333333703, 0.3333333333333334259, 0.3333333333333333703, 0.3333333333333334259, 0.3333333333333333148, 0.3333333333333333703, 0.3333333333333333703, 0.3333333333333334259, 0.3333333333333333703, 0.3333333333333334259, 0.3333333333333333703, 0.3333333333333333703, 0.3333333333333334259, 0.3333333333333334814, 0.3333333333333333703, 0.3333333333333333703, 0.3333333333333334814, 0.3333333333333333148, 0.3333333333333333703, 0.3333333333333333148, 0.3333333333333333703, 0.3333333333333333148, 0.3333333333333334259, 0.3333333333333334259, 0.3333333333333333703, 0.3333333333333333703, 0.3333333333333333703, 0.3333333333333333703, 0.3333333333333334259, 0.3333333333333332593, 0.3333333333333333703, 0.3333333333333333703, 0.3333333333333333703, 0.3333333333333333148, 0.3333333333333333703, 0.3333333333333333148, 0.3333333333333334259, 0.3333333333333333148, 0.3333333333333333703, 0.3333333333333333703, 0.3333333333333334259, 0.3333333333333333703, 0.3333333333333333148, 0.3333333333333333703, 0.3333333333333333703, 0.3333333333333333148, 0.3333333333333333703, 0.3333333333333333148, 0.3333333333333333703, 0.3333333333333333703, 0.3333333333333334814, 0.3333333333333333148, 0.3333333333333334259, 0.3333333333333334259, 0.3333333333333333703, 0.3333333333333334259, 0.3333333333333333703, 0.3333333333333334259, 0.3333333333333332593, 0.3333333333333334259, 0.3333333333333333148, 0.3333333333333334259, 0.3333333333333333148, 0.3333333333333334259, 0.3333333333333332593, 0.3333333333333335369, 0.3333333333333332038, 0.3333333333333334259, 0.3333333333333333703, 0.3333333333333333148, 0.3333333333333334259, 0.3333333333333333148, 0.3333333333333333148, 0.3333333333333333148, 0.3333333333333334814, 0.3333333333333332593, 0.3333333333333334259, 0.3333333333333333148, 0.3333333333333333148, 0.3333333333333334814, 0.3333333333333333703, 0.3333333333333334259, 0.3333333333333333148, 0.3333333333333333703, 0.3333333333333332593, 0.3333333333333334814, 0.3333333333333333148, 0.3333333333333334259, 0.3333333333333333148, 0.3333333333333334259, 0.3333333333333333703, 0.3333333333333333703, 0.3333333333333334259, 0.3333333333333333148, 0.3333333333333334814, 0.3333333333333333703, 0.3333333333333333703, 0.3333333333333334814, 0.3333333333333333703, 0.3333333333333332593, 0.3333333333333334259, 0.3333333333333332593, 0.3333333333333334814, 0.3333333333333333148, 0.3333333333333333703, 0.3333333333333333703, 0.3333333333333334259, 0.3333333333333333703, 0.3333333333333333703, 0.3333333333333333148, 0.3333333333333334259, 0.3333333333333334259, 0.3333333333333333703, 0.3333333333333334259, 0.3333333333333333148, 0.3333333333333333703, 0.3333333333333334259, 0.3333333333333333703, 0.3333333333333333148, 0.3333333333333334259, 0.3333333333333333703, 0.3333333333333333148, 0.3333333333333333148, 0.3333333333333334259, 0.3333333333333333148, 0.3333333333333333703, 0.3333333333333333703, 0.3333333333333333703, 0.3333333333333334259, 0.3333333333333334259, 0.3333333333333333148, 0.3333333333333334259, 0.3333333333333333148, 0.3333333333333334814, 0.3333333333333332593, 0.3333333333333334814, 0.3333333333333333703, 0.3333333333333333703, 0.3333333333333334259, 0.3333333333333333703, 0.3333333333333333703, 0.3333333333333333703, 0.3333333333333333703, 0.3333333333333334814, 0.3333333333333333148, 0.3333333333333334259, 0.3333333333333333148, 0.3333333333333333703, 0.3333333333333333703, 0.3333333333333333703, 0.3333333333333335369, 0.3333333333333333703, 0.3333333333333333148, 0.3333333333333334814, 0.3333333333333334259, 0.3333333333333333148, 0.3333333333333333148, 0.3333333333333335369, 0.3333333333333332593, 0.3333333333333333703, 0.3333333333333333148, 0.3333333333333333703, 0.3333333333333333703, 0.3333333333333332593, 0.3333333333333334259, 0.3333333333333332593, 0.3333333333333335369, 0.3333333333333333148, 0.3333333333333333703, 0.3333333333333334259, 0.3333333333333333703, 0.3333333333333333703, 0.3333333333333334814, 0.3333333333333333148, 0.3333333333333333148, 0.3333333333333334259, 0.3333333333333333148, 0.3333333333333333703, 0.3333333333333334814, 0.3333333333333333703, 0.3333333333333333703, 0.3333333333333333703, 0.3333333333333333703, 0.3333333333333334814, 0.3333333333333333703, 0.3333333333333334814, 0.3333333333333333703, 0.3333333333333333703, 0.3333333333333333148, 0.3333333333333334259, 0.3333333333333333148, 0.3333333333333334259, 0.3333333333333333148, 0.3333333333333333703, 0.3333333333333334814, 0.3333333333333333148, 0.3333333333333333148, 0.3333333333333333703, 0.3333333333333333703, 0.3333333333333333703, 0.3333333333333334259, 0.3333333333333333148, 0.3333333333333333703, 0.3333333333333334259, 0.3333333333333333148, 0.3333333333333333703, 0.3333333333333332593, 0.3333333333333333703, 0.3333333333333334259, 0.3333333333333333703, 0.3333333333333333703, 0.3333333333333333703, 0.3333333333333333703, 0.3333333333333334814, 0.3333333333333333703, 0.3333333333333334259, 0.3333333333333334259),
 ( 0.3333333333333333703, 0.3333333333333333703, 0.3333333333333333703, 0.3333333333333333703, 0.3333333333333333148, 0.3333333333333334259, 0.3333333333333333703, 0.3333333333333333148, 0.3333333333333334259, 0.3333333333333333148, 0.3333333333333334259, 0.3333333333333332038, 0.3333333333333333703, 0.3333333333333332593, 0.3333333333333333703, 0.3333333333333332593, 0.3333333333333334814, 0.3333333333333334259, 0.3333333333333333703, 0.3333333333333334259, 0.3333333333333334259, 0.3333333333333332038, 0.3333333333333335369, 0.3333333333333333148, 0.3333333333333333148, 0.3333333333333334259, 0.3333333333333333703, 0.3333333333333333148, 0.3333333333333334259, 0.3333333333333333148, 0.3333333333333335369, 0.3333333333333333148, 0.3333333333333334259, 0.3333333333333333148, 0.3333333333333334259, 0.3333333333333333703, 0.3333333333333333148, 0.3333333333333333703, 0.3333333333333334259, 0.3333333333333333703, 0.3333333333333334259, 0.3333333333333333703, 0.3333333333333334814, 0.3333333333333333148, 0.3333333333333334259, 0.3333333333333332593, 0.3333333333333335369, 0.3333333333333332593, 0.3333333333333334259, 0.3333333333333333148, 0.3333333333333333703, 0.3333333333333334259, 0.3333333333333333148, 0.3333333333333334814, 0.3333333333333332593, 0.3333333333333333703, 0.3333333333333332593, 0.3333333333333335369, 0.3333333333333333148, 0.3333333333333334259, 0.3333333333333334259, 0.3333333333333334259, 0.3333333333333333148, 0.3333333333333333148, 0.3333333333333333703, 0.3333333333333333703, 0.3333333333333333703, 0.3333333333333334259, 0.3333333333333333148, 0.3333333333333333703, 0.3333333333333333703, 0.3333333333333332593, 0.3333333333333334259, 0.3333333333333333703, 0.3333333333333333703, 0.3333333333333333148, 0.3333333333333333148, 0.3333333333333334259, 0.3333333333333333148, 0.3333333333333334259, 0.3333333333333333148, 0.3333333333333334259, 0.3333333333333333703, 0.3333333333333334259, 0.3333333333333333703, 0.3333333333333333703, 0.3333333333333333148, 0.3333333333333335369, 0.3333333333333332593, 0.3333333333333334814, 0.3333333333333333703, 0.3333333333333333703, 0.3333333333333333148, 0.3333333333333333703, 0.3333333333333334259, 0.3333333333333334259, 0.3333333333333333148, 0.3333333333333333703, 0.3333333333333334259, 0.3333333333333333148, 0.3333333333333333703, 0.3333333333333334814, 0.3333333333333332038, 0.3333333333333334814, 0.3333333333333333703, 0.3333333333333333148, 0.3333333333333334259, 0.3333333333333333148, 0.3333333333333334259, 0.3333333333333332593, 0.3333333333333333703, 0.3333333333333334259, 0.3333333333333333148, 0.3333333333333333703, 0.3333333333333333148, 0.3333333333333334259, 0.3333333333333333703, 0.3333333333333333703, 0.3333333333333333703, 0.3333333333333334259, 0.3333333333333332038, 0.3333333333333334259, 0.3333333333333334259, 0.3333333333333333703, 0.3333333333333333703, 0.3333333333333332593, 0.3333333333333333703, 0.3333333333333333148, 0.3333333333333334259, 0.3333333333333332593, 0.3333333333333334259, 0.3333333333333333703, 0.3333333333333334259, 0.3333333333333334259, 0.3333333333333333148, 0.3333333333333334259, 0.3333333333333334259, 0.3333333333333332593, 0.3333333333333334259, 0.3333333333333333703, 0.3333333333333333703, 0.3333333333333333148, 0.3333333333333334259, 0.3333333333333333703, 0.3333333333333334259, 0.3333333333333334259, 0.3333333333333333703, 0.3333333333333333703, 0.3333333333333334814, 0.3333333333333333703, 0.3333333333333333703, 0.3333333333333335369, 0.3333333333333332593, 0.3333333333333334259, 0.3333333333333333148, 0.3333333333333334259, 0.3333333333333334259, 0.3333333333333334259, 0.3333333333333332593, 0.3333333333333333148, 0.3333333333333333703, 0.3333333333333334259, 0.3333333333333333148, 0.3333333333333333703, 0.3333333333333333148, 0.3333333333333334259, 0.3333333333333333148, 0.3333333333333334259, 0.3333333333333333148, 0.3333333333333334259, 0.3333333333333333703, 0.3333333333333334259, 0.3333333333333333703, 0.3333333333333334259, 0.3333333333333333148, 0.3333333333333333703, 0.3333333333333333703, 0.3333333333333334259, 0.3333333333333333703, 0.3333333333333334259, 0.3333333333333333703, 0.3333333333333333703, 0.3333333333333334259, 0.3333333333333334814, 0.3333333333333333703, 0.3333333333333333703, 0.3333333333333334814, 0.3333333333333333148, 0.3333333333333333703, 0.3333333333333333148, 0.3333333333333333703, 0.3333333333333333148, 0.3333333333333334259, 0.3333333333333334259, 0.3333333333333333703, 0.3333333333333333703, 0.3333333333333333703, 0.3333333333333333703, 0.3333333333333334259, 0.3333333333333332593, 0.3333333333333333703, 0.3333333333333333703, 0.3333333333333333703, 0.3333333333333333148, 0.3333333333333333703, 0.3333333333333333148, 0.3333333333333334259, 0.3333333333333333148, 0.3333333333333333703, 0.3333333333333333703, 0.3333333333333334259, 0.3333333333333333703, 0.3333333333333333148, 0.3333333333333333703, 0.3333333333333333703, 0.3333333333333333148, 0.3333333333333333703, 0.3333333333333333148, 0.3333333333333333703, 0.3333333333333333703, 0.3333333333333334814, 0.3333333333333333148, 0.3333333333333334259, 0.3333333333333334259, 0.3333333333333333703, 0.3333333333333334259, 0.3333333333333333703, 0.3333333333333334259, 0.3333333333333332593, 0.3333333333333334259, 0.3333333333333333148, 0.3333333333333334259, 0.3333333333333333148, 0.3333333333333334259, 0.3333333333333332593, 0.3333333333333335369, 0.3333333333333332038, 0.3333333333333334259, 0.3333333333333333703, 0.3333333333333333148, 0.3333333333333334259, 0.3333333333333333148, 0.3333333333333333148, 0.3333333333333333148, 0.3333333333333334814, 0.3333333333333332593, 0.3333333333333334259, 0.3333333333333333148, 0.3333333333333333148, 0.3333333333333334814, 0.3333333333333333703, 0.3333333333333334259, 0.3333333333333333148, 0.3333333333333333703, 0.3333333333333332593, 0.3333333333333334814, 0.3333333333333333148, 0.3333333333333334259, 0.3333333333333333148, 0.3333333333333334259, 0.3333333333333333703, 0.3333333333333333703, 0.3333333333333334259, 0.3333333333333333148, 0.3333333333333334814, 0.3333333333333333703, 0.3333333333333333703, 0.3333333333333334814, 0.3333333333333333703, 0.3333333333333332593, 0.3333333333333334259, 0.3333333333333332593, 0.3333333333333334814, 0.3333333333333333148, 0.3333333333333333703, 0.3333333333333333703, 0.3333333333333334259, 0.3333333333333333703, 0.3333333333333333703, 0.3333333333333333148, 0.3333333333333334259, 0.3333333333333334259, 0.3333333333333333703, 0.3333333333333334259, 0.3333333333333333148, 0.3333333333333333703, 0.3333333333333334259, 0.3333333333333333703, 0.3333333333333333148, 0.3333333333333334259, 0.3333333333333333703, 0.3333333333333333148, 0.3333333333333333148, 0.3333333333333334259, 0.3333333333333333148, 0.3333333333333333703, 0.3333333333333333703, 0.3333333333333333703, 0.3333333333333334259, 0.3333333333333334259, 0.3333333333333333148, 0.3333333333333334259, 0.3333333333333333148, 0.3333333333333334814, 0.3333333333333332593, 0.3333333333333334814, 0.3333333333333333703, 0.3333333333333333703, 0.3333333333333334259, 0.3333333333333333703, 0.3333333333333333703, 0.3333333333333333703, 0.3333333333333333703, 0.3333333333333334814, 0.3333333333333333148, 0.3333333333333334259, 0.3333333333333333148, 0.3333333333333333703, 0.3333333333333333703, 0.3333333333333333703, 0.3333333333333335369, 0.3333333333333333703, 0.3333333333333333148, 0.3333333333333334814, 0.3333333333333334259, 0.3333333333333333148, 0.3333333333333333148, 0.3333333333333335369, 0.3333333333333332593, 0.3333333333333333703, 0.3333333333333333148, 0.3333333333333333703, 0.3333333333333333703, 0.3333333333333332593, 0.3333333333333334259, 0.3333333333333332593, 0.3333333333333335369, 0.3333333333333333148, 0.3333333333333333703, 0.3333333333333334259, 0.3333333333333333703, 0.3333333333333333703, 0.3333333333333334814, 0.3333333333333333148, 0.3333333333333333148, 0.3333333333333334259, 0.3333333333333333148, 0.3333333333333333703, 0.3333333333333334814, 0.3333333333333333703, 0.3333333333333333703, 0.3333333333333333703, 0.3333333333333333703, 0.3333333333333334814, 0.3333333333333333703, 0.3333333333333334814, 0.3333333333333333703, 0.3333333333333333703, 0.3333333333333333148, 0.3333333333333334259, 0.3333333333333333148, 0.3333333333333334259, 0.3333333333333333148, 0.3333333333333333703, 0.3333333333333334814, 0.3333333333333333148, 0.3333333333333333148, 0.3333333333333333703, 0.3333333333333333703, 0.3333333333333333703, 0.3333333333333334259, 0.3333333333333333148, 0.3333333333333333703, 0.3333333333333334259, 0.3333333333333333148, 0.3333333333333333703, 0.3333333333333332593, 0.3333333333333333703, 0.3333333333333334259, 0.3333333333333333703, 0.3333333333333333703, 0.3333333333333333703, 0.3333333333333333703, 0.3333333333333334814, 0.3333333333333333703, 0.3333333333333334259, 0.3333333333333334259),
 ( 1.000000000000000000, 1.000000000000000000, 1.000000000000000222, 1.000000000000000000, 0.9999999999999996669, 1.000000000000000444, 0.9999999999999997780, 1.000000000000000000, 1.000000000000000222, 0.9999999999999996669, 1.000000000000000222, 0.9999999999999996669, 1.000000000000000000, 0.9999999999999997780, 1.000000000000000222, 0.9999999999999997780, 1.000000000000000222, 1.000000000000000222, 0.9999999999999997780, 1.000000000000000222, 1.000000000000000222, 0.9999999999999996669, 1.000000000000000444, 0.9999999999999997780, 1.000000000000000000, 1.000000000000000222, 1.000000000000000000, 1.000000000000000000, 1.000000000000000000, 1.000000000000000000, 1.000000000000000222, 1.000000000000000000, 1.000000000000000000, 0.9999999999999997780, 1.000000000000000000, 1.000000000000000000, 1.000000000000000000, 1.000000000000000000, 0.9999999999999997780, 1.000000000000000222, 1.000000000000000000, 1.000000000000000000, 1.000000000000000444, 0.9999999999999997780, 1.000000000000000222, 0.9999999999999996669, 1.000000000000000444, 0.9999999999999997780, 1.000000000000000000, 0.9999999999999997780, 1.000000000000000000, 1.000000000000000222, 0.9999999999999997780, 1.000000000000000444, 0.9999999999999997780, 1.000000000000000000, 0.9999999999999996669, 1.000000000000000444, 0.9999999999999997780, 1.000000000000000444, 1.000000000000000000, 1.000000000000000444, 0.9999999999999996669, 1.000000000000000000, 0.9999999999999996669, 1.000000000000000444, 0.9999999999999997780, 1.000000000000000000, 1.000000000000000000, 1.000000000000000000, 1.000000000000000000, 0.9999999999999996669, 1.000000000000000000, 1.000000000000000222, 0.9999999999999997780, 1.000000000000000000, 0.9999999999999997780, 0.9999999999999997780, 1.000000000000000000, 1.000000000000000222, 0.9999999999999997780, 1.000000000000000000, 1.000000000000000222, 1.000000000000000222, 1.000000000000000222, 0.9999999999999997780, 1.000000000000000000, 1.000000000000000222, 0.9999999999999997780, 1.000000000000000222, 1.000000000000000222, 0.9999999999999997780, 0.9999999999999997780, 0.9999999999999997780, 1.000000000000000444, 1.000000000000000000, 1.000000000000000000, 1.000000000000000000, 1.000000000000000222, 0.9999999999999997780, 1.000000000000000000, 1.000000000000000444, 0.9999999999999996669, 1.000000000000000444, 1.000000000000000000, 1.000000000000000000, 1.000000000000000222, 0.9999999999999997780, 1.000000000000000444, 0.9999999999999996669, 1.000000000000000444, 1.000000000000000000, 0.9999999999999997780, 1.000000000000000222, 0.9999999999999996669, 1.000000000000000222, 1.000000000000000000, 1.000000000000000222, 0.9999999999999997780, 1.000000000000000222, 0.9999999999999996669, 1.000000000000000222, 1.000000000000000222, 1.000000000000000222, 1.000000000000000000, 0.9999999999999997780, 1.000000000000000000, 0.9999999999999997780, 1.000000000000000000, 0.9999999999999997780, 0.9999999999999997780, 1.000000000000000222, 1.000000000000000222, 1.000000000000000222, 0.9999999999999997780, 0.9999999999999997780, 1.000000000000000444, 0.9999999999999997780, 1.000000000000000000, 0.9999999999999997780, 1.000000000000000000, 0.9999999999999997780, 1.000000000000000222, 1.000000000000000000, 1.000000000000000000, 1.000000000000000222, 1.000000000000000000, 0.9999999999999997780, 1.000000000000000444, 1.000000000000000000, 1.000000000000000000, 1.000000000000000444, 0.9999999999999997780, 1.000000000000000222, 0.9999999999999997780, 1.000000000000000444, 1.000000000000000000, 1.000000000000000222, 0.9999999999999997780, 0.9999999999999997780, 1.000000000000000000, 1.000000000000000444, 0.9999999999999996669, 1.000000000000000000, 1.000000000000000222, 1.000000000000000222, 0.9999999999999997780, 1.000000000000000222, 0.9999999999999997780, 1.000000000000000222, 1.000000000000000000, 1.000000000000000000, 0.9999999999999997780, 1.000000000000000444, 0.9999999999999997780, 1.000000000000000222, 0.9999999999999996669, 1.000000000000000444, 0.9999999999999996669, 1.000000000000000222, 1.000000000000000000, 1.000000000000000000, 1.000000000000000000, 1.000000000000000444, 1.000000000000000222, 0.9999999999999997780, 1.000000000000000444, 0.9999999999999997780, 1.000000000000000000, 0.9999999999999996669, 1.000000000000000000, 0.9999999999999996669, 1.000000000000000000, 1.000000000000000222, 1.000000000000000000, 0.9999999999999997780, 1.000000000000000222, 1.000000000000000000, 1.000000000000000222, 0.9999999999999996669, 1.000000000000000000, 1.000000000000000000, 1.000000000000000000, 0.9999999999999997780, 1.000000000000000000, 1.000000000000000000, 1.000000000000000222, 1.000000000000000000, 1.000000000000000000, 0.9999999999999997780, 1.000000000000000000, 1.000000000000000222, 0.9999999999999997780, 1.000000000000000000, 1.000000000000000222, 1.000000000000000000, 1.000000000000000000, 0.9999999999999997780, 0.9999999999999997780, 1.000000000000000000, 1.000000000000000000, 0.9999999999999997780, 1.000000000000000000, 1.000000000000000000, 1.000000000000000000, 1.000000000000000222, 1.000000000000000000, 1.000000000000000000, 0.9999999999999997780, 1.000000000000000000, 0.9999999999999997780, 1.000000000000000444, 0.9999999999999997780, 1.000000000000000222, 0.9999999999999997780, 1.000000000000000444, 0.9999999999999994449, 1.000000000000000444, 0.9999999999999997780, 1.000000000000000222, 1.000000000000000000, 1.000000000000000000, 0.9999999999999997780, 1.000000000000000000, 1.000000000000000000, 0.9999999999999997780, 1.000000000000000000, 1.000000000000000000, 0.9999999999999997780, 1.000000000000000222, 1.000000000000000000, 1.000000000000000222, 0.9999999999999997780, 1.000000000000000222, 0.9999999999999997780, 1.000000000000000222, 0.9999999999999997780, 1.000000000000000444, 0.9999999999999996669, 1.000000000000000222, 0.9999999999999997780, 1.000000000000000000, 1.000000000000000000, 1.000000000000000000, 1.000000000000000222, 1.000000000000000222, 1.000000000000000000, 1.000000000000000444, 1.000000000000000222, 0.9999999999999997780, 1.000000000000000222, 0.9999999999999996669, 1.000000000000000444, 0.9999999999999997780, 0.9999999999999997780, 1.000000000000000222, 1.000000000000000000, 1.000000000000000222, 1.000000000000000000, 1.000000000000000000, 1.000000000000000222, 1.000000000000000000, 0.9999999999999997780, 1.000000000000000222, 0.9999999999999997780, 1.000000000000000000, 1.000000000000000222, 1.000000000000000000, 0.9999999999999997780, 0.9999999999999997780, 1.000000000000000000, 0.9999999999999997780, 1.000000000000000000, 1.000000000000000000, 1.000000000000000000, 1.000000000000000222, 0.9999999999999997780, 1.000000000000000000, 1.000000000000000222, 1.000000000000000000, 0.9999999999999997780, 1.000000000000000000, 1.000000000000000000, 1.000000000000000222, 0.9999999999999997780, 1.000000000000000222, 1.000000000000000000, 1.000000000000000000, 1.000000000000000222, 1.000000000000000000, 1.000000000000000000, 1.000000000000000222, 1.000000000000000000, 1.000000000000000444, 0.9999999999999996669, 1.000000000000000444, 0.9999999999999997780, 1.000000000000000000, 1.000000000000000222, 0.9999999999999996669, 1.000000000000000444, 1.000000000000000000, 1.000000000000000000, 1.000000000000000222, 1.000000000000000444, 1.000000000000000000, 0.9999999999999996669, 1.000000000000000444, 0.9999999999999997780, 0.9999999999999997780, 0.9999999999999997780, 1.000000000000000222, 1.000000000000000000, 0.9999999999999996669, 1.000000000000000222, 1.000000000000000000, 1.000000000000000444, 0.9999999999999997780, 1.000000000000000000, 1.000000000000000222, 1.000000000000000222, 1.000000000000000222, 1.000000000000000222, 1.000000000000000000, 1.000000000000000000, 1.000000000000000000, 1.000000000000000000, 1.000000000000000000, 1.000000000000000444, 1.000000000000000000, 0.9999999999999997780, 1.000000000000000000, 1.000000000000000222, 1.000000000000000000, 1.000000000000000222, 1.000000000000000222, 1.000000000000000000, 0.9999999999999997780, 0.9999999999999997780, 1.000000000000000222, 0.9999999999999997780, 1.000000000000000000, 1.000000000000000222, 1.000000000000000000, 1.000000000000000222, 1.000000000000000000, 0.9999999999999997780, 1.000000000000000000, 0.9999999999999997780, 1.000000000000000222, 1.000000000000000000, 0.9999999999999997780, 0.9999999999999997780, 1.000000000000000222, 1.000000000000000000, 1.000000000000000222, 0.9999999999999996669, 1.000000000000000000, 1.000000000000000222, 0.9999999999999997780, 1.000000000000000000, 1.000000000000000000, 1.000000000000000222, 1.000000000000000222, 1.000000000000000000, 1.000000000000000222, 1.000000000000000222) ) ) 
 REPRESENTATION_ITEM ( '' )  SURFACE ( )  );
#125217 = CARTESIAN_POINT ( 'NONE',  ( -2.974698719455045381, 6.690899969729074748, -0.05384663926280564006 ) ) ;
#125218 = DIRECTION ( 'NONE',  ( 5.551115123125783935E-17, 0.7071067811865536790, -0.7071067811865413555 ) ) ;
#125219 = AXIS2_PLACEMENT_3D ( 'NONE', #75678, #8534, #154800 ) ;
#125220 = CARTESIAN_POINT ( 'NONE',  ( 1.366164030173490973, 2.173753390890633685, -0.3800739277931909355 ) ) ;
#125221 = CARTESIAN_POINT ( 'NONE',  ( 2.530887537405112298, 2.193952394701288000, 0.5517939747049571686 ) ) ;
#125222 =( GEOMETRIC_REPRESENTATION_CONTEXT ( 3 ) GLOBAL_UNCERTAINTY_ASSIGNED_CONTEXT ( ( #194583 ) ) GLOBAL_UNIT_ASSIGNED_CONTEXT ( ( #156177, #57598, #41371 ) ) REPRESENTATION_CONTEXT ( 'NONE', 'WORKASPACE' ) );
#125223 = CARTESIAN_POINT ( 'NONE',  ( -7.809133291791416909, 11.09411069285655493, 1.082531754730549967 ) ) ;
#125224 = CARTESIAN_POINT ( 'NONE',  ( 1.986290607305480460, -1.112306265806988437, 1.429831149274364721 ) ) ;
#125225 = ADVANCED_FACE ( 'NONE', ( #131358 ), #164861, .T. ) ;
#125226 = CARTESIAN_POINT ( 'NONE',  ( 3.274530738273524033, -0.3788105498489474088, -1.877706502262687760 ) ) ;
#125227 = CARTESIAN_POINT ( 'NONE',  ( 4.316890830952234914, -1.536253448065309613, 1.388129241271539138 ) ) ;
#125228 = CARTESIAN_POINT ( 'NONE',  ( -1.402160292154681736E-14, 2.509375000341417028, -1.575800808251660134 ) ) ;
#125229 = CARTESIAN_POINT ( 'NONE',  ( 2.272288244244465627, -1.214158342444570327, 1.553133305774859974 ) ) ;
#125230 = CARTESIAN_POINT ( 'NONE',  ( 0.4813100693330485957, 1.798698175156054457, -0.6901501906162701427 ) ) ;
#125231 = CARTESIAN_POINT ( 'NONE',  ( 3.731198135974967300, -1.728734619261709904, 0.7151963084984153118 ) ) ;
#125233 = CARTESIAN_POINT ( 'NONE',  ( 4.915098833515745724, 8.004322973991836676, -0.9888141558981374812 ) ) ;
#125232 = CARTESIAN_POINT ( 'NONE',  ( 1.893647147081824356, 2.006347305559322169, -1.140069799644787940 ) ) ;
#125234 = CARTESIAN_POINT ( 'NONE',  ( 3.437814515362676016, 1.178941034414218603, 1.440021488233768521 ) ) ;
#125235 = CARTESIAN_POINT ( 'NONE',  ( -1.364683531250012516, 3.738541667008087099, -0.7879004041258300672 ) ) ;
#125236 = CARTESIAN_POINT ( 'NONE',  ( -3.438964519360665051, 7.163875705896082913, -0.7998128361456281477 ) ) ;
#125237 = CARTESIAN_POINT ( 'NONE',  ( 5.961834861707224320, 7.978559976790334574, -1.599625672291262513 ) ) ;
#125238 = CARTESIAN_POINT ( 'NONE',  ( 11.35993080936262345, 3.555461883994698979, -3.691065267805079042 ) ) ;
#125239 = CARTESIAN_POINT ( 'NONE',  ( 0.7332070197069834316, 0.1568218392365756941, 2.100289424198895194 ) ) ;
#125241 = CARTESIAN_POINT ( 'NONE',  ( 5.061565854856461932, 4.907682761174942065, 0.2605415071502180657 ) ) ;
#125240 = CARTESIAN_POINT ( 'NONE',  ( 1.364683531249988535, 4.217708333674752730, -0.7879004041258239610 ) ) ;
#125242 = CARTESIAN_POINT ( 'NONE',  ( 6.661405305706385782, 0.3767857563467743032, -2.128362917677539379 ) ) ;
#125243 = CARTESIAN_POINT ( 'NONE',  ( 2.021885665735908333, -0.4598567139443253682, 2.069992740399699382 ) ) ;
#125244 = CARTESIAN_POINT ( 'NONE',  ( -0.1403647893034008221, -1.563942476893056543, -1.277904792927646582 ) ) ;
#125245 = CARTESIAN_POINT ( 'NONE',  ( -1.402160292154681736E-14, 0.07187500034142156602, 1.575800808251672791 ) ) ;
#125246 = CARTESIAN_POINT ( 'NONE',  ( -3.145128448690310830, 6.613140923539910787, -0.7216878364870267237 ) ) ;
#125247 = EDGE_CURVE ( 'NONE', #63949, #184190, #213115, .T. ) ;
#125248 = CARTESIAN_POINT ( 'NONE',  ( 1.476082264964494906, 1.286352913914396545, 1.737049067733025032 ) ) ;
#125251 = CARTESIAN_POINT ( 'NONE',  ( 2.901081683644312736, 6.328419697652925002, 0.7216878364870338292 ) ) ;
#125250 = CARTESIAN_POINT ( 'NONE',  ( 6.825078400183526739, 3.708013787890347857, 2.270222819304415385 ) ) ;
#125249 = CARTESIAN_POINT ( 'NONE',  ( 5.742760583840166966, 8.857581893525663830, 1.199719254218452047 ) ) ;
#125252 = CARTESIAN_POINT ( 'NONE',  ( -5.164730172163054966, 4.990216387137135889, -0.7998128361456362523 ) ) ;
#125253 = CARTESIAN_POINT ( 'NONE',  ( 4.803922858132807505, -1.082837210388952309, -1.700963621564715700 ) ) ;
#125255 = CARTESIAN_POINT ( 'NONE',  ( -6.089020385868850305, 10.11795786024005572, -0.7216878364870338292 ) ) ;
#125254 = CARTESIAN_POINT ( 'NONE',  ( -9.002250809794000830, 11.52571191622492464, -1.443375672974059665 ) ) ;
#125256 = CARTESIAN_POINT ( 'NONE',  ( -9.361942704757909794, 14.57097479506862037, -7.422992708136343154 ) ) ;
#125258 = CARTESIAN_POINT ( 'NONE',  ( -0.6823417656250003738, 10.40104166700806587, 1.181850606188754593 ) ) ;
#125257 = CARTESIAN_POINT ( 'NONE',  ( 0.1985910703563107393, -2.262096406685298877, -0.05156929113746439725 ) ) ;
#125259 = CARTESIAN_POINT ( 'NONE',  ( -10.29471871147821282, 10.90492667301307605, -0.7998128361456291469 ) ) ;
#125261 = CARTESIAN_POINT ( 'NONE',  ( 6.239861269555550649, 2.010826412442122013, -0.1511553674920090573 ) ) ;
#125260 = CARTESIAN_POINT ( 'NONE',  ( -5.056828107772852299, 7.883087978168217269, -1.082531754730548412 ) ) ;
#125262 = CARTESIAN_POINT ( 'NONE',  ( -1.201851678989727383E-14, 0.8843750003414173610, 1.575800808251672791 ) ) ;
#125263 = CARTESIAN_POINT ( 'NONE',  ( 0.05083690440159209512, 14.51152975025495806, 11.99422659986761808 ) ) ;
#125264 = CARTESIAN_POINT ( 'NONE',  ( 11.97181073603049484, 11.38000000000000078, 0.8318477717169575625 ) ) ;
#125265 = CARTESIAN_POINT ( 'NONE',  ( 3.387030231456603424, 1.558874866368621159, -0.7386201850746020314 ) ) ;
#125266 = CARTESIAN_POINT ( 'NONE',  ( 5.273195401072370281, 5.116759154198018855, -0.7998128361456481317 ) ) ;
#125267 = CARTESIAN_POINT ( 'NONE',  ( 6.540882763950133238, 6.595727744222092959, 0.000000000000000000 ) ) ;
#125268 = CARTESIAN_POINT ( 'NONE',  ( 0.8953273879380260203, -0.6444125412686675380, 1.648433012593934155 ) ) ;
#125269 = CARTESIAN_POINT ( 'NONE',  ( 2.086589530005359183, -1.236640506920426263, 1.588416314350507674 ) ) ;
#125270 = PRESENTATION_STYLE_ASSIGNMENT (( #206423 ) ) ;
#125271 = CARTESIAN_POINT ( 'NONE',  ( 4.630015379333586978, -1.354682855507854278, -1.741961856448564383 ) ) ;
#125272 = ORIENTED_EDGE ( 'NONE', *, *, #115265, .F. ) ;
#125273 = CARTESIAN_POINT ( 'NONE',  ( 1.499999999999987121, -0.4958333333333110882, 0.8660254037844524744 ) ) ;
#125274 = CARTESIAN_POINT ( 'NONE',  ( 8.283668667825342169, 9.726996869626816533, -1.082531754730543083 ) ) ;
#125276 = CARTESIAN_POINT ( 'NONE',  ( 3.462517696756307384, -1.944077823024586538, -0.5350690621670484148 ) ) ;
#125275 = CARTESIAN_POINT ( 'NONE',  ( 2.719513590175401063, 1.792643918890064247, 1.132349250948051500 ) ) ;
#125278 = ORIENTED_EDGE ( 'NONE', *, *, #96134, .F. ) ;
#125277 = CARTESIAN_POINT ( 'NONE',  ( 3.462975342835975301, -1.477922853017235916, 1.047338699574466014 ) ) ;
#125279 = CARTESIAN_POINT ( 'NONE',  ( 3.739016502318667445, 7.584212696005614873, 0.7998128361456271485 ) ) ;
#125280 = ORIENTED_EDGE ( 'NONE', *, *, #119318, .F. ) ;
#125281 = CARTESIAN_POINT ( 'NONE',  ( 0.1450994221751950586, -1.442925249786636943, -1.190247126510869613 ) ) ;
#125282 = CARTESIAN_POINT ( 'NONE',  ( 4.704842999142070603, 5.447737239542574272, -1.199719254218452047 ) ) ;
#125283 = VECTOR ( 'NONE', #162957, 1000.000000000000000 ) ;
#125284 = CARTESIAN_POINT ( 'NONE',  ( 6.094357461763901362, -1.817385979143220309, -0.1739998769475574192 ) ) ;
#125286 = CARTESIAN_POINT ( 'NONE',  ( 2.905391412282500863, -1.844872930762898600, 0.5157873856561823178 ) ) ;
#125285 = CARTESIAN_POINT ( 'NONE',  ( -3.735435015764967837, 4.316761258935923884, -1.199719254218452047 ) ) ;
#125287 = FILL_AREA_STYLE ('',( #59129 ) ) ;
#125288 = ADVANCED_FACE ( 'NONE', ( #163814, #115113 ), #16454, .F. ) ;
#125289 = CARTESIAN_POINT ( 'NONE',  ( -0.6823417656250212460, 1.113541667008083325, 1.181850606188755259 ) ) ;
#125290 = CARTESIAN_POINT ( 'NONE',  ( -0.4000000000000218936, 3.949999999999960654, 0.8627243683429972609 ) ) ;
#125291 = CARTESIAN_POINT ( 'NONE',  ( 6.021229618244865023, 10.03886863134542828, -0.7216878364870458196 ) ) ;
#125292 = EDGE_CURVE ( 'NONE', #75675, #175679, #128197, .T. ) ;
#125293 = CARTESIAN_POINT ( 'NONE',  ( -6.305950844131887223, 6.529566537674873494, 0.000000000000000000 ) ) ;
#125294 = CARTESIAN_POINT ( 'NONE',  ( -5.399890319992785237, 9.521898816625391504, 0.7998128361456291469 ) ) ;
#125295 = CARTESIAN_POINT ( 'NONE',  ( 2.724977724663907530, 1.532976055022855499, -1.465462182430438798 ) ) ;
#125297 = CARTESIAN_POINT ( 'NONE',  ( -11.03396297008821847, 6.349565552376400746, 6.086320354413141231 ) ) ;
#125296 = CARTESIAN_POINT ( 'NONE',  ( -0.02988540731099428513, 1.418068428043406382, -1.986943242881351601 ) ) ;
#125298 = CARTESIAN_POINT ( 'NONE',  ( 4.604731966549804767, 1.525920046185350376, -1.248162976031294003 ) ) ;
#125299 = CARTESIAN_POINT ( 'NONE',  ( -0.05247892273943338681, -1.838936383286099652, 0.8197664084235550819 ) ) ;
#125300 = CARTESIAN_POINT ( 'NONE',  ( 6.368375629516933145, -2.076896536817146810, -0.4110353314962181259 ) ) ;
#125301 =( NAMED_UNIT ( * ) SI_UNIT ( $, .STERADIAN. ) SOLID_ANGLE_UNIT ( ) );
#125302 = CARTESIAN_POINT ( 'NONE',  ( 1.645070734656968625, -0.3017366986639741788, -2.048123538821471801 ) ) ;
#125303 = CARTESIAN_POINT ( 'NONE',  ( 2.589705103518041618, -1.936761303218867969, -0.1426656448052856518 ) ) ;
#125304 = VERTEX_POINT ( 'NONE', #78273 ) ;
#125305 = CARTESIAN_POINT ( 'NONE',  ( 4.681308178468477799, 8.683552984847038303, 0.000000000000000000 ) ) ;
#125306 = CARTESIAN_POINT ( 'NONE',  ( 5.338878628731272613, 9.450718510153643948, -0.7998128361456481317 ) ) ;
#125308 = CARTESIAN_POINT ( 'NONE',  ( 7.318703993278529829, 7.432909501780090800, 1.040834085586084257E-14 ) ) ;
#125307 = CARTESIAN_POINT ( 'NONE',  ( 3.662131271747073757, -1.403999256393541284, 1.549221476816674548 ) ) ;
#125309 = CARTESIAN_POINT ( 'NONE',  ( 4.001064729364292916, 6.721640380016713934, -1.082531754730548412 ) ) ;
#125311 = ORIENTED_EDGE ( 'NONE', *, *, #168278, .T. ) ;
#125310 = CARTESIAN_POINT ( 'NONE',  ( 0.9788403037365877024, -1.637337388150851725, -0.7752084675131820646 ) ) ;
#125312 = CARTESIAN_POINT ( 'NONE',  ( 5.742855475442601332, 0.4270144693867898300, 2.165010647329483895 ) ) ;
#125313 = FACE_OUTER_BOUND ( 'NONE', #23020, .T. ) ;
#125314 = CARTESIAN_POINT ( 'NONE',  ( 4.647634198631804381, -1.703412986257560879, -1.402924735643434673 ) ) ;
#125315 = CARTESIAN_POINT ( 'NONE',  ( 8.446893396513862839, 9.813462703143045474, -1.199719254218445830 ) ) ;
#125316 = FACE_OUTER_BOUND ( 'NONE', #183175, .T. ) ;
#125317 = CARTESIAN_POINT ( 'NONE',  ( 2.648957786072099641, 0.2360777847093403214, 1.897596177352772306 ) ) ;
#125318 = CARTESIAN_POINT ( 'NONE',  ( 8.452618703115982512, 11.94880668935564216, 1.199719254218450271 ) ) ;
#125319 = CARTESIAN_POINT ( 'NONE',  ( 5.160626937512653001, -0.6942339714755951796, -1.950645400549338104 ) ) ;
#125321 = CARTESIAN_POINT ( 'NONE',  ( 2.325270847726228940, -0.0006328605136555342939, 2.161883445422786654 ) ) ;
#125320 = FACE_OUTER_BOUND ( 'NONE', #177808, .T. ) ;
#125322 = CARTESIAN_POINT ( 'NONE',  ( 4.581673536070863584, -1.032772929490553215, 1.932928240684625099 ) ) ;
#125323 = VERTEX_POINT ( 'NONE', #162751 ) ;
#125324 = ORIENTED_EDGE ( 'NONE', *, *, #58676, .F. ) ;
#125325 = CARTESIAN_POINT ( 'NONE',  ( 10.07387183015377197, 11.71160420905630062, -1.199719254218440723 ) ) ;
#125326 = SURFACE_STYLE_USAGE ( .BOTH. , #126392 ) ;
#125327 = CARTESIAN_POINT ( 'NONE',  ( 5.411639590510088027, 6.342609606130419131, -1.199719254218452047 ) ) ;
#125328 = CARTESIAN_POINT ( 'NONE',  ( -3.285556943750000514, -2.326041666188708668, -1.896917185911906722 ) ) ;
#125329 = CARTESIAN_POINT ( 'NONE',  ( -9.680158490477310806, 10.39586578175276266, 0.7216878364870438212 ) ) ;
#125330 = CARTESIAN_POINT ( 'NONE',  ( 4.929271367020211514, 7.908511140569038922, 1.199719254218452047 ) ) ;
#125331 = CARTESIAN_POINT ( 'NONE',  ( 5.787960296632533641, -1.308950758395693414, -1.603975846202657429 ) ) ;
#125332 = CARTESIAN_POINT ( 'NONE',  ( 4.811117629317255506, 1.676929503210132122, 0.9481960042460689797 ) ) ;
#125333 = CARTESIAN_POINT ( 'NONE',  ( 6.468375645409351726, -2.076397406075684682, -0.4129765506453788038 ) ) ;
#125334 = CARTESIAN_POINT ( 'NONE',  ( 7.856023664475727308, 8.130058794835305136, -0.7998128361456341429 ) ) ;
#125335 = CARTESIAN_POINT ( 'NONE',  ( -2.788906526875773208E-15, 13.18750000000000000, -1.499999999999998446 ) ) ;
#125336 = CARTESIAN_POINT ( 'NONE',  ( 5.383641442822343137, -1.871314765454759055, 0.6142198095173864170 ) ) ;
#125337 = CARTESIAN_POINT ( 'NONE',  ( 6.562434020506859866, -2.092894318229638895, -0.9354203566987564500 ) ) ;
#125338 = CARTESIAN_POINT ( 'NONE',  ( 4.934128534657983067, 0.9357288403324083292, -1.567518238613223813 ) ) ;
#125339 = CARTESIAN_POINT ( 'NONE',  ( 5.180624094197585627, 8.097792972322238825, -1.082531754730548412 ) ) ;
#125340 = CARTESIAN_POINT ( 'NONE',  ( 2.833290915131624566, 6.249330467721451399, -0.7216878364870267237 ) ) ;
#125341 = CARTESIAN_POINT ( 'NONE',  ( -5.981082042284069367, 7.006959133200059142, 1.199719254218452935 ) ) ;
#125342 = CARTESIAN_POINT ( 'NONE',  ( 4.203910148689107729, 7.062256385849379647, -1.199719254218448494 ) ) ;
#125343 = ORIENTED_EDGE ( 'NONE', *, *, #81050, .F. ) ;
#125345 = CARTESIAN_POINT ( 'NONE',  ( -0.07552757677437360595, -0.8618087116909570744, -1.817275918844815541 ) ) ;
#125344 = CARTESIAN_POINT ( 'NONE',  ( 2.718100415690410721, 1.734538518968967935, 0.6181264464550640936 ) ) ;
#125346 = CARTESIAN_POINT ( 'NONE',  ( 1.283028839759347894, -2.242172747002548316, 0.5046827817699239827 ) ) ;
#125347 = CARTESIAN_POINT ( 'NONE',  ( 5.401206054008879320, -1.684469800357458302, 1.005230755432365175 ) ) ;
#125348 = CARTESIAN_POINT ( 'NONE',  ( -4.693093728624763372, 8.627026450037540428, 0.7998128361456481317 ) ) ;
#125349 = CARTESIAN_POINT ( 'NONE',  ( -7.055786748303249922, -6.583711766989059910, 6.534012848836718845 ) ) ;
#125350 = CARTESIAN_POINT ( 'NONE',  ( -4.796887421136680985, 4.490790167614548523, 1.214306433183764966E-14 ) ) ;
#125351 = CARTESIAN_POINT ( 'NONE',  ( 0.5728211633247158874, 1.428863753495920763, -1.498466819491943269 ) ) ;
#125352 = CARTESIAN_POINT ( 'NONE',  ( -5.984998465789844069, 5.947196063035064206, 0.7998128361456281477 ) ) ;
#125354 = CARTESIAN_POINT ( 'NONE',  ( 1.111929834214450796, -0.8377583890188080584, -1.672643128629976772 ) ) ;
#125353 = CARTESIAN_POINT ( 'NONE',  ( 1.118821681092090126, -0.04763362108583040627, 2.090370170816723494 ) ) ;
#125355 = CARTESIAN_POINT ( 'NONE',  ( 1.792342068719571468, -1.899328565777322231, 0.6766080823841430503 ) ) ;
#125356 = EDGE_LOOP ( 'NONE', ( #187241, #177219, #128263, #52184 ) ) ;
#125357 = CARTESIAN_POINT ( 'NONE',  ( -1.364683531250012516, 4.301041667008089320, -0.7879004041258300672 ) ) ;
#125358 = CARTESIAN_POINT ( 'NONE',  ( 2.225747907193951214, 1.688420964825324555, 0.4218146122960535482 ) ) ;
#125359 = CARTESIAN_POINT ( 'NONE',  ( 5.996784015946103885, 5.890669528225568996, 1.040834085586084257E-14 ) ) ;
#125360 = CARTESIAN_POINT ( 'NONE',  ( 1.510809298642989296, 8.679800937805028482, 2.538927604451451270 ) ) ;
#125361 = CARTESIAN_POINT ( 'NONE',  ( 2.367434161175852925, 1.691737554211050210, -0.3355112704105273624 ) ) ;
#125362 = CARTESIAN_POINT ( 'NONE',  ( 3.105210138592546798, -0.4252477525170209605, 2.149737936336936883 ) ) ;
#125363 = CARTESIAN_POINT ( 'NONE',  ( 0.1583034150156861219, 0.9959709328331721734, 1.419360398433693549 ) ) ;
#125364 = CARTESIAN_POINT ( 'NONE',  ( 4.951907052881864502, 0.6945806438464275923, -2.094803410698709900 ) ) ;
#125365 = CARTESIAN_POINT ( 'NONE',  ( -9.949604414185204249, 5.483733089116166859, -6.039292150722699759 ) ) ;
#125366 = CARTESIAN_POINT ( 'NONE',  ( 2.448294946665624749, -0.9317531996627312907, 1.961122280359078873 ) ) ;
#125367 = CARTESIAN_POINT ( 'NONE',  ( 1.277666653898035021, 1.085793613588705853, 1.467558327050644484 ) ) ;
#125368 = CARTESIAN_POINT ( 'NONE',  ( 3.766910327102332978, -0.2117226681838789426, -2.106763584193247940 ) ) ;
#125369 = AXIS2_PLACEMENT_3D ( 'NONE', #1287, #67345, #199493 ) ;
#125370 = DIRECTION ( 'NONE',  ( 0.000000000000000000, 0.8000000000000117018, -0.5999999999999843237 ) ) ;
#125371 = ORIENTED_EDGE ( 'NONE', *, *, #211811, .T. ) ;
#125373 = CARTESIAN_POINT ( 'NONE',  ( 0.6823417656249899377, 1.905208333674752952, 1.181850606188755259 ) ) ;
#125372 = CARTESIAN_POINT ( 'NONE',  ( 3.984120879971131401, -2.267471576223866414, -0.3361144993852988594 ) ) ;
#125374 = CARTESIAN_POINT ( 'NONE',  ( 6.727182134110200273, -0.004969159814478123736, 2.189081792362323586 ) ) ;
#125375 = CARTESIAN_POINT ( 'NONE',  ( 2.544126380858701797, 6.119897877643793116, 0.7998128361456462443 ) ) ;
#125376 = CARTESIAN_POINT ( 'NONE',  ( 6.164703477482621707, 0.6939275443377226349, 2.110173311658748663 ) ) ;
#125377 = CARTESIAN_POINT ( 'NONE',  ( -6.073689629242160493, 8.109057205581079231, -1.443375672974059665 ) ) ;
#125378 = CARTESIAN_POINT ( 'NONE',  ( 4.094199201646931741, 4.839282492418613302, -1.082531754730543083 ) ) ;
#125379 = CARTESIAN_POINT ( 'NONE',  ( -7.497295758232736418, 7.849192594134070333, -0.7216878364870267237 ) ) ;
#125380 = CARTESIAN_POINT ( 'NONE',  ( 0.02890330888917177696, -9.971207602185762298, 10.91966316483287613 ) ) ;
#125381 = ORIENTED_EDGE ( 'NONE', *, *, #27912, .F. ) ;
#125382 = CARTESIAN_POINT ( 'NONE',  ( 4.096327398540238640, -0.3419367296172080017, 1.987046374476949095 ) ) ;
#125384 = CARTESIAN_POINT ( 'NONE',  ( 3.678632908625163012, 1.312080992568062321, -1.591389186695492342 ) ) ;
#125383 = CARTESIAN_POINT ( 'NONE',  ( 6.823831386379729302, 6.855558127064808716, -0.7998128361456281477 ) ) ;
#125385 = CARTESIAN_POINT ( 'NONE',  ( 7.506374323821472849, 8.786466794993730289, -1.199719254218452047 ) ) ;
#125386 = CARTESIAN_POINT ( 'NONE',  ( 6.933015448541703485, 9.181880338089085214, 1.599625672291268286 ) ) ;
#125387 = CARTESIAN_POINT ( 'NONE',  ( -1.642778471874998480, -3.201041666188710000, 2.845375778867863303 ) ) ;
#125388 = CARTESIAN_POINT ( 'NONE',  ( -1.364683531250012516, 4.988541667008084879, -0.7879004041258300672 ) ) ;
#125389 = CARTESIAN_POINT ( 'NONE',  ( 6.316381784907312280, 2.043361914081378128, 0.7923855730916644635 ) ) ;
#125390 = CARTESIAN_POINT ( 'NONE',  ( 3.709611425391425854, 1.915599900965975433, 0.6298755557959597740 ) ) ;
#125391 = CARTESIAN_POINT ( 'NONE',  ( 1.927068723821170559, -1.203646435588998420, -1.393412863611859454 ) ) ;
#125392 = CARTESIAN_POINT ( 'NONE',  ( 5.296431564432884542, 9.330920591813708143, 1.040834085586084257E-14 ) ) ;
#125393 = CARTESIAN_POINT ( 'NONE',  ( 0.09417432218480553674, -0.3651332853754212238, -1.691417143215419028 ) ) ;
#125394 =( BOUNDED_SURFACE ( )  B_SPLINE_SURFACE ( 1, 2, ( 
 ( #77120, #31591, #143243, #161597, #79264, #129176, #97666, #145381, #14230, #80325, #76063, #142162, #208179, #48903, #117150, #181020, #115023, #100830, #199381, #32640, #98717, #134444, #184206, #67242, #164776, #16366, #182068, #84588, #68313, #131275, #1178, #200447, #52093, #148534, #163724, #118220, #116078, #35829, #33700, #99777, #197263, #183153, #81392, #167972, #19578, #101907, #15304, #82444, #149594, #51028, #147477, #101, #213497, #66167, #65119, #132314, #198319, #165842, #2236, #49959, #17428, #83511, #166915, #133376, #34756, #18509, #150675, #112510, #193687, #178522, #63695, #126647, #161204, #143929, #110387, #14917, #164398, #29069, #12790, #114647, #177455, #62617, #192612, #97283, #128779, #13859, #208858, #78864, #47470, #130895, #129849, #144985, #45331, #64753, #180640, #96221, #194756, #127729, #179587, #113585, #46393, #111450, #30132, #94094, #196889, #27997, #60489, #176392, #162272, #163338, #95152, #61563, #44265, #31209, #79936, #210990, #146041, #212055, #195832, #81011, #147099, #160133, #209924, #213123, #15981, #48527, #142854, #32265, #98332, #11732, #77808, #70066, #148158, #117847, #783, #202197, #214159, #20263, #152418, #66850, #53853, #150295, #1862, #67923, #166528, #86347, #37595, #35448, #134067, #101528, #200076, #136179, #17049, #33320, #135119, #51725, #183839, #131935, #182765, #119986, #18119, #165454, #184893, #169726, #132994, #3997, #198995, #185963, #83128, #167597, #19196, #149208, #85274, #151361, #84207, #103678, #2930, #168658, #69002, #201135, #82066, #50641, #52773, #65785, #116767, #34382, #118910, #99401, #36517, #100455, #102604, #197946, #49573, #115698, #181690, #157766, #59175, #106928, #22387, #187037, #155622, #41895, #91717, #121069, #40820, #25605, #9366, #204328, #21315, #174033, #171867, #75437, #23461, #89573, #54918, #8292, #153489, #125334, #191297, #141549, #207556, #88496, #139384, #172953, #190236, #42965, #109073, #39735, #87422, #74375, #5059, #140477, #71134, #137252, #7207, #104748, #55986, #105840, #72205, #205417, #203272 ),
 ( #122138, #73280, #38669, #108006, #57055, #24532, #170796, #123219, #206489, #154557, #156700, #189183, #138313, #6136, #188105, #90640, #58119, #124278, #76483, #27742, #142594, #141540, #126394, #10411, #140467, #92770, #24521, #208603, #158815, #60234, #57044, #39725, #159876, #123210, #204319, #189171, #93837, #188093, #55977, #23451, #11481, #192354, #77552, #174024, #207548, #59167, #157758, #40811, #7198, #73271, #105831, #172943, #25594, #171856, #176142, #106919, #75429, #8281, #44011, #122130, #90631, #110131, #156691, #89563, #205405, #58110, #190227, #139374, #91707, #9355, #206480, #155613, #124269, #74365, #125327, #41886, #107997, #191288, #42954, #109064, #175080, #26666, #145800, #163090, #79688, #47218, #94898, #14671, #2401, #146854, #210749, #113334, #194503, #179341, #64507, #127472, #162024, #144739, #111195, #18674, #168139, #29886, #13615, #118384, #178276, #63444, #193443, #100993, #129596, #80765, #209668, #211806, #51196, #134607, #130651, #195583, #46149, #68480, #184372, #97038, #30963, #128534, #12540, #117318, #112262, #62372, #212874, #160950, #200611, #28814, #61311, #177199, #199552, #167083, #95970, #183315, #45086, #34920, #84753, #150840, #52258, #35992, #102073, #19740, #143675, #78614, #86890, #87956, #173504, #136719, #107478, #105296, #38143, #187578, #172417, #73841, #151899, #121608, #4531, #205963, #3474, #24006, #156174, #70605, #57595, #154030, #5596, #71677, #170263, #90108, #41367, #39205, #137790, #171332, #203810, #139936, #20794, #37060, #138859, #55455, #22927, #135650, #186512, #123753, #21849, #169201, #89042, #155099, #6683, #72760, #7754, #85820, #204874, #56529, #122690, #188652, #189715, #152955, #103142, #40284, #106393, #69543, #201673, #104216, #53320, #119453, #202744, #185440, #54396, #120536, #29365, #158307, #145286, #26147, #93319, #10953, #174571, #126948, #44562, #175626, #46694, #27213, #111744, #192905, #190773, #95460, #8834, #79170, #144228, #28290, #141020, #159355, #110677, #77026, #143156, #42435, #176677, #161509, #94384, #92261, #209150 ) ),
 .UNSPECIFIED., .F., .F., .T. ) 
 B_SPLINE_SURFACE_WITH_KNOTS ( ( 2, 2 ),
 ( 3, 2, 2, 2, 2, 2, 2, 2, 2, 2, 2, 2, 2, 2, 2, 2, 2, 2, 2, 2, 2, 2, 2, 2, 2, 2, 2, 2, 2, 2, 2, 2, 2, 2, 2, 2, 2, 2, 2, 2, 2, 2, 2, 2, 2, 2, 2, 2, 2, 2, 2, 2, 2, 2, 2, 2, 2, 2, 2, 2, 2, 2, 2, 2, 2, 2, 2, 2, 2, 2, 2, 2, 2, 2, 2, 2, 2, 2, 2, 2, 2, 2, 2, 2, 2, 2, 2, 2, 2, 2, 2, 2, 2, 2, 2, 2, 2, 2, 2, 2, 2, 2, 2, 2, 2, 2, 2, 2, 2, 2, 2, 2, 2, 2, 2, 2, 2, 2, 2, 2, 3 ),
 ( 0.000000000000000000, 1.000000000000000000 ),
 ( 0.000000000000000000, 0.008333333333333333218, 0.01666666666666666644, 0.02500000000000000139, 0.03333333333333333287, 0.04166666666666666435, 0.05000000000000000278, 0.05833333333333333426, 0.06666666666666666574, 0.07499999999999999722, 0.08333333333333332871, 0.09166666666666666019, 0.1000000000000000056, 0.1083333333333333370, 0.1166666666666666685, 0.1250000000000000000, 0.1333333333333333315, 0.1416666666666666630, 0.1499999999999999944, 0.1583333333333333259, 0.1666666666666666574, 0.1749999999999999889, 0.1833333333333333204, 0.1916666666666666796, 0.2000000000000000111, 0.2083333333333333426, 0.2166666666666666741, 0.2250000000000000056, 0.2333333333333333370, 0.2416666666666666685, 0.2500000000000000000, 0.2583333333333333592, 0.2666666666666666630, 0.2750000000000000222, 0.2833333333333333259, 0.2916666666666666852, 0.2999999999999999889, 0.3083333333333333481, 0.3166666666666666519, 0.3250000000000000111, 0.3333333333333333148, 0.3416666666666666741, 0.3499999999999999778, 0.3583333333333333370, 0.3666666666666666408, 0.3750000000000000000, 0.3833333333333333592, 0.3916666666666666630, 0.4000000000000000222, 0.4083333333333333259, 0.4166666666666666852, 0.4249999999999999889, 0.4333333333333333481, 0.4416666666666666519, 0.4500000000000000111, 0.4583333333333333148, 0.4666666666666666741, 0.4749999999999999778, 0.4833333333333333370, 0.4916666666666666408, 0.5000000000000000000, 0.5083333333333333037, 0.5166666666666667185, 0.5250000000000000222, 0.5333333333333333259, 0.5416666666666666297, 0.5500000000000000444, 0.5583333333333333481, 0.5666666666666666519, 0.5749999999999999556, 0.5833333333333333703, 0.5916666666666666741, 0.5999999999999999778, 0.6083333333333332815, 0.6166666666666666963, 0.6250000000000000000, 0.6333333333333333037, 0.6416666666666667185, 0.6500000000000000222, 0.6583333333333333259, 0.6666666666666666297, 0.6750000000000000444, 0.6833333333333333481, 0.6916666666666666519, 0.6999999999999999556, 0.7083333333333333703, 0.7166666666666666741, 0.7249999999999999778, 0.7333333333333332815, 0.7416666666666666963, 0.7500000000000000000, 0.7583333333333333037, 0.7666666666666667185, 0.7750000000000000222, 0.7833333333333333259, 0.7916666666666666297, 0.8000000000000000444, 0.8083333333333333481, 0.8166666666666666519, 0.8249999999999999556, 0.8333333333333333703, 0.8416666666666666741, 0.8499999999999999778, 0.8583333333333332815, 0.8666666666666666963, 0.8750000000000000000, 0.8833333333333333037, 0.8916666666666667185, 0.9000000000000000222, 0.9083333333333333259, 0.9166666666666666297, 0.9250000000000000444, 0.9333333333333333481, 0.9416666666666666519, 0.9499999999999999556, 0.9583333333333333703, 0.9666666666666666741, 0.9749999999999999778, 0.9833333333333332815, 0.9916666666666666963, 1.000000000000000000 ),
 .UNSPECIFIED. ) 
 GEOMETRIC_REPRESENTATION_ITEM ( )  RATIONAL_B_SPLINE_SURFACE ( (
 ( 1.000000000000000000, 0.8660254037844387076, 1.000000000000000000, 0.8660254037844387076, 1.000000000000000000, 0.8660254037844387076, 1.000000000000000000, 0.8660254037844387076, 1.000000000000000000, 0.8660254037844387076, 1.000000000000000000, 0.8660254037844387076, 1.000000000000000000, 0.8660254037844387076, 1.000000000000000000, 0.8660254037844387076, 1.000000000000000000, 0.8660254037844387076, 1.000000000000000000, 0.8660254037844387076, 1.000000000000000000, 0.8660254037844387076, 1.000000000000000000, 0.8660254037844387076, 1.000000000000000000, 0.8660254037844387076, 1.000000000000000000, 0.8660254037844387076, 1.000000000000000000, 0.8660254037844387076, 1.000000000000000000, 0.8660254037844387076, 1.000000000000000000, 0.8660254037844387076, 1.000000000000000000, 0.8660254037844387076, 1.000000000000000000, 0.8660254037844387076, 1.000000000000000000, 0.8660254037844387076, 1.000000000000000000, 0.8660254037844387076, 1.000000000000000000, 0.8660254037844387076, 1.000000000000000000, 0.8660254037844387076, 1.000000000000000000, 0.8660254037844387076, 1.000000000000000000, 0.8660254037844387076, 1.000000000000000000, 0.8660254037844387076, 1.000000000000000000, 0.8660254037844387076, 1.000000000000000000, 0.8660254037844387076, 1.000000000000000000, 0.8660254037844387076, 1.000000000000000000, 0.8660254037844387076, 1.000000000000000000, 0.8660254037844387076, 1.000000000000000000, 0.8660254037844387076, 1.000000000000000000, 0.8660254037844387076, 1.000000000000000000, 0.8660254037844387076, 1.000000000000000000, 0.8660254037844387076, 1.000000000000000000, 0.8660254037844387076, 1.000000000000000000, 0.8660254037844387076, 1.000000000000000000, 0.8660254037844387076, 1.000000000000000000, 0.8660254037844387076, 1.000000000000000000, 0.8660254037844387076, 1.000000000000000000, 0.8660254037844387076, 1.000000000000000000, 0.8660254037844387076, 1.000000000000000000, 0.8660254037844387076, 1.000000000000000000, 0.8660254037844387076, 1.000000000000000000, 0.8660254037844387076, 1.000000000000000000, 0.8660254037844387076, 1.000000000000000000, 0.8660254037844387076, 1.000000000000000000, 0.8660254037844387076, 1.000000000000000000, 0.8660254037844387076, 1.000000000000000000, 0.8660254037844387076, 1.000000000000000000, 0.8660254037844387076, 1.000000000000000000, 0.8660254037844387076, 1.000000000000000000, 0.8660254037844387076, 1.000000000000000000, 0.8660254037844387076, 1.000000000000000000, 0.8660254037844387076, 1.000000000000000000, 0.8660254037844387076, 1.000000000000000000, 0.8660254037844387076, 1.000000000000000000, 0.8660254037844387076, 1.000000000000000000, 0.8660254037844387076, 1.000000000000000000, 0.8660254037844387076, 1.000000000000000000, 0.8660254037844387076, 1.000000000000000000, 0.8660254037844387076, 1.000000000000000000, 0.8660254037844387076, 1.000000000000000000, 0.8660254037844387076, 1.000000000000000000, 0.8660254037844387076, 1.000000000000000000, 0.8660254037844387076, 1.000000000000000000, 0.8660254037844387076, 1.000000000000000000, 0.8660254037844387076, 1.000000000000000000, 0.8660254037844387076, 1.000000000000000000, 0.8660254037844387076, 1.000000000000000000, 0.8660254037844387076, 1.000000000000000000, 0.8660254037844387076, 1.000000000000000000, 0.8660254037844387076, 1.000000000000000000, 0.8660254037844387076, 1.000000000000000000, 0.8660254037844387076, 1.000000000000000000, 0.8660254037844387076, 1.000000000000000000, 0.8660254037844387076, 1.000000000000000000, 0.8660254037844387076, 1.000000000000000000, 0.8660254037844387076, 1.000000000000000000, 0.8660254037844387076, 1.000000000000000000, 0.8660254037844387076, 1.000000000000000000, 0.8660254037844387076, 1.000000000000000000, 0.8660254037844387076, 1.000000000000000000, 0.8660254037844387076, 1.000000000000000000, 0.8660254037844387076, 1.000000000000000000, 0.8660254037844387076, 1.000000000000000000, 0.8660254037844387076, 1.000000000000000000, 0.8660254037844387076, 1.000000000000000000, 0.8660254037844387076, 1.000000000000000000, 0.8660254037844387076, 1.000000000000000000, 0.8660254037844387076, 1.000000000000000000, 0.8660254037844387076, 1.000000000000000000, 0.8660254037844387076, 1.000000000000000000, 0.8660254037844387076, 1.000000000000000000, 0.8660254037844387076, 1.000000000000000000, 0.8660254037844387076, 1.000000000000000000, 0.8660254037844387076, 1.000000000000000000, 0.8660254037844387076, 1.000000000000000000, 0.8660254037844387076, 1.000000000000000000, 0.8660254037844387076, 1.000000000000000000, 0.8660254037844387076, 1.000000000000000000, 0.8660254037844387076, 1.000000000000000000, 0.8660254037844387076, 1.000000000000000000, 0.8660254037844387076, 1.000000000000000000, 0.8660254037844387076, 1.000000000000000000, 0.8660254037844387076, 1.000000000000000000, 0.8660254037844387076, 1.000000000000000000, 0.8660254037844387076, 1.000000000000000000, 0.8660254037844387076, 1.000000000000000000, 0.8660254037844387076, 1.000000000000000000, 0.8660254037844387076, 1.000000000000000000, 0.8660254037844387076, 1.000000000000000000, 0.8660254037844387076, 1.000000000000000000, 0.8660254037844387076, 1.000000000000000000, 0.8660254037844387076, 1.000000000000000000, 0.8660254037844387076, 1.000000000000000000, 0.8660254037844387076, 1.000000000000000000, 0.8660254037844387076, 1.000000000000000000, 0.8660254037844387076, 1.000000000000000000, 0.8660254037844387076, 1.000000000000000000),
 ( 1.000000000000000000, 0.8660254037844387076, 1.000000000000000000, 0.8660254037844387076, 1.000000000000000000, 0.8660254037844387076, 1.000000000000000000, 0.8660254037844387076, 1.000000000000000000, 0.8660254037844387076, 1.000000000000000000, 0.8660254037844387076, 1.000000000000000000, 0.8660254037844387076, 1.000000000000000000, 0.8660254037844387076, 1.000000000000000000, 0.8660254037844387076, 1.000000000000000000, 0.8660254037844387076, 1.000000000000000000, 0.8660254037844387076, 1.000000000000000000, 0.8660254037844387076, 1.000000000000000000, 0.8660254037844387076, 1.000000000000000000, 0.8660254037844387076, 1.000000000000000000, 0.8660254037844387076, 1.000000000000000000, 0.8660254037844387076, 1.000000000000000000, 0.8660254037844387076, 1.000000000000000000, 0.8660254037844387076, 1.000000000000000000, 0.8660254037844387076, 1.000000000000000000, 0.8660254037844387076, 1.000000000000000000, 0.8660254037844387076, 1.000000000000000000, 0.8660254037844387076, 1.000000000000000000, 0.8660254037844387076, 1.000000000000000000, 0.8660254037844387076, 1.000000000000000000, 0.8660254037844387076, 1.000000000000000000, 0.8660254037844387076, 1.000000000000000000, 0.8660254037844387076, 1.000000000000000000, 0.8660254037844387076, 1.000000000000000000, 0.8660254037844387076, 1.000000000000000000, 0.8660254037844387076, 1.000000000000000000, 0.8660254037844387076, 1.000000000000000000, 0.8660254037844387076, 1.000000000000000000, 0.8660254037844387076, 1.000000000000000000, 0.8660254037844387076, 1.000000000000000000, 0.8660254037844387076, 1.000000000000000000, 0.8660254037844387076, 1.000000000000000000, 0.8660254037844387076, 1.000000000000000000, 0.8660254037844387076, 1.000000000000000000, 0.8660254037844387076, 1.000000000000000000, 0.8660254037844387076, 1.000000000000000000, 0.8660254037844387076, 1.000000000000000000, 0.8660254037844387076, 1.000000000000000000, 0.8660254037844387076, 1.000000000000000000, 0.8660254037844387076, 1.000000000000000000, 0.8660254037844387076, 1.000000000000000000, 0.8660254037844387076, 1.000000000000000000, 0.8660254037844387076, 1.000000000000000000, 0.8660254037844387076, 1.000000000000000000, 0.8660254037844387076, 1.000000000000000000, 0.8660254037844387076, 1.000000000000000000, 0.8660254037844387076, 1.000000000000000000, 0.8660254037844387076, 1.000000000000000000, 0.8660254037844387076, 1.000000000000000000, 0.8660254037844387076, 1.000000000000000000, 0.8660254037844387076, 1.000000000000000000, 0.8660254037844387076, 1.000000000000000000, 0.8660254037844387076, 1.000000000000000000, 0.8660254037844387076, 1.000000000000000000, 0.8660254037844387076, 1.000000000000000000, 0.8660254037844387076, 1.000000000000000000, 0.8660254037844387076, 1.000000000000000000, 0.8660254037844387076, 1.000000000000000000, 0.8660254037844387076, 1.000000000000000000, 0.8660254037844387076, 1.000000000000000000, 0.8660254037844387076, 1.000000000000000000, 0.8660254037844387076, 1.000000000000000000, 0.8660254037844387076, 1.000000000000000000, 0.8660254037844387076, 1.000000000000000000, 0.8660254037844387076, 1.000000000000000000, 0.8660254037844387076, 1.000000000000000000, 0.8660254037844387076, 1.000000000000000000, 0.8660254037844387076, 1.000000000000000000, 0.8660254037844387076, 1.000000000000000000, 0.8660254037844387076, 1.000000000000000000, 0.8660254037844387076, 1.000000000000000000, 0.8660254037844387076, 1.000000000000000000, 0.8660254037844387076, 1.000000000000000000, 0.8660254037844387076, 1.000000000000000000, 0.8660254037844387076, 1.000000000000000000, 0.8660254037844387076, 1.000000000000000000, 0.8660254037844387076, 1.000000000000000000, 0.8660254037844387076, 1.000000000000000000, 0.8660254037844387076, 1.000000000000000000, 0.8660254037844387076, 1.000000000000000000, 0.8660254037844387076, 1.000000000000000000, 0.8660254037844387076, 1.000000000000000000, 0.8660254037844387076, 1.000000000000000000, 0.8660254037844387076, 1.000000000000000000, 0.8660254037844387076, 1.000000000000000000, 0.8660254037844387076, 1.000000000000000000, 0.8660254037844387076, 1.000000000000000000, 0.8660254037844387076, 1.000000000000000000, 0.8660254037844387076, 1.000000000000000000, 0.8660254037844387076, 1.000000000000000000, 0.8660254037844387076, 1.000000000000000000, 0.8660254037844387076, 1.000000000000000000, 0.8660254037844387076, 1.000000000000000000, 0.8660254037844387076, 1.000000000000000000, 0.8660254037844387076, 1.000000000000000000, 0.8660254037844387076, 1.000000000000000000, 0.8660254037844387076, 1.000000000000000000, 0.8660254037844387076, 1.000000000000000000, 0.8660254037844387076, 1.000000000000000000, 0.8660254037844387076, 1.000000000000000000, 0.8660254037844387076, 1.000000000000000000, 0.8660254037844387076, 1.000000000000000000, 0.8660254037844387076, 1.000000000000000000, 0.8660254037844387076, 1.000000000000000000, 0.8660254037844387076, 1.000000000000000000, 0.8660254037844387076, 1.000000000000000000, 0.8660254037844387076, 1.000000000000000000, 0.8660254037844387076, 1.000000000000000000, 0.8660254037844387076, 1.000000000000000000, 0.8660254037844387076, 1.000000000000000000, 0.8660254037844387076, 1.000000000000000000, 0.8660254037844387076, 1.000000000000000000, 0.8660254037844387076, 1.000000000000000000, 0.8660254037844387076, 1.000000000000000000, 0.8660254037844387076, 1.000000000000000000, 0.8660254037844387076, 1.000000000000000000) ) ) 
 REPRESENTATION_ITEM ( '' )  SURFACE ( )  );
#125395 = CARTESIAN_POINT ( 'NONE',  ( 0.05395445667428447334, -1.494411465983748855, 1.746745294031383455 ) ) ;
#125396 = CARTESIAN_POINT ( 'NONE',  ( -7.226659571283968297, 8.389856573708110332, 1.199719254218450271 ) ) ;
#125398 = CARTESIAN_POINT ( 'NONE',  ( -3.644109427023046521, 7.473487774827342278, 0.000000000000000000 ) ) ;
#125397 = CARTESIAN_POINT ( 'NONE',  ( 5.840765815766128632, 0.4347934677991367458, 2.220198762108383850 ) ) ;
#125399 = CARTESIAN_POINT ( 'NONE',  ( 1.893330831959182836, 1.831869315246800189, -1.038985425167998633 ) ) ;
#125400 = CARTESIAN_POINT ( 'NONE',  ( -5.478376588373717659, 8.549133898814758936, -1.199719254218452047 ) ) ;
#125401 = CARTESIAN_POINT ( 'NONE',  ( 8.914649696185335870, 10.35917838609310593, -1.199719254218446718 ) ) ;
#125402 = CARTESIAN_POINT ( 'NONE',  ( 7.471952054462754234, 8.850270497362297206, 1.082531754730549078 ) ) ;
#125403 = CARTESIAN_POINT ( 'NONE',  ( -8.040148788103921973, 9.338927326664741457, 1.199719254218462483 ) ) ;
#125404 = CARTESIAN_POINT ( 'NONE',  ( -3.801259017012812436, 7.351524727272684245, -0.7148551115157241176 ) ) ;
#125405 = CARTESIAN_POINT ( 'NONE',  ( 6.738039155867407537, 10.80487008191325771, -0.7216878364870267237 ) ) ;
#125406 = CARTESIAN_POINT ( 'NONE',  ( 3.999300167945916584, 7.828775037665852921, -0.06519116529766534607 ) ) ;
#125407 = CARTESIAN_POINT ( 'NONE',  ( -5.005985031943793295, 6.863401842066301661, -1.599625672291256295 ) ) ;
#125408 = CARTESIAN_POINT ( 'NONE',  ( 2.795431959603801086, -0.1677860356435970368, -2.215157990583861203 ) ) ;
#125409 = CIRCLE ( 'NONE', #163367, 11.89429233241351902 ) ;
#125410 = CARTESIAN_POINT ( 'NONE',  ( 0.06543086261080394150, -1.973449318085427340, -0.9880335165917543128 ) ) ;
#125411 = CARTESIAN_POINT ( 'NONE',  ( -5.795184315198522285, 5.725746220678519904, -0.7998128361456362523 ) ) ;
#125412 = CARTESIAN_POINT ( 'NONE',  ( 6.335737856287750880, 6.286115675290828264, -0.7998128361456281477 ) ) ;
#125413 = CARTESIAN_POINT ( 'NONE',  ( 4.633228507203630997, 0.002057781214020309134, -1.962046631861932067 ) ) ;
#125414 = CARTESIAN_POINT ( 'NONE',  ( 7.703003830858588863, 12.13858823597705872, -0.7998128361456291469 ) ) ;
#125415 = CARTESIAN_POINT ( 'NONE',  ( -4.789689200157987159, 6.785576372466274542, 1.244997348908165602 ) ) ;
#125416 = CARTESIAN_POINT ( 'NONE',  ( 4.220665892555866883, 3.818531717603609987, -0.7998128361456211532 ) ) ;
#125417 = CARTESIAN_POINT ( 'NONE',  ( -1.201851678989727383E-14, 0.8218750003414171390, 1.575800808251672791 ) ) ;
#125418 = CARTESIAN_POINT ( 'NONE',  ( -4.665414256878293031, 7.496714828783040296, -1.082531754730549967 ) ) ;
#125420 = ORIENTED_EDGE ( 'NONE', *, *, #46917, .F. ) ;
#125419 = CARTESIAN_POINT ( 'NONE',  ( -6.399085315970155285, 6.567947078161039620, -0.7216878364870278340 ) ) ;
#125421 = CARTESIAN_POINT ( 'NONE',  ( 3.357788437482766675, -1.608272433257527556, -1.382313803475518244 ) ) ;
#125422 = CARTESIAN_POINT ( 'NONE',  ( -3.610214042988883598, 7.433943160120816351, 0.7998128361456352531 ) ) ;
#125423 = CARTESIAN_POINT ( 'NONE',  ( 5.120075222393803749, -1.153228217640640985, -1.828211184805514922 ) ) ;
#125424 = CARTESIAN_POINT ( 'NONE',  ( 3.561895345837225779, -1.234009368583251165, 1.366721199326895952 ) ) ;
#125425 = CARTESIAN_POINT ( 'NONE',  ( 4.856657812281613751, -1.900414607462055816, -0.6748505307947461063 ) ) ;
#125426 = CARTESIAN_POINT ( 'NONE',  ( -5.505981461394960697, 6.253680794909101337, 0.9796770575781436063 ) ) ;
#125427 = CARTESIAN_POINT ( 'NONE',  ( -1.402160292154681736E-14, 1.259375000341419248, -1.575800808251659024 ) ) ;
#125428 = B_SPLINE_CURVE_WITH_KNOTS ( 'NONE', 3,
 ( #161479, #25051, #160395, #129052, #9868, #110648 ),
 .UNSPECIFIED., .F., .F.,
 ( 4, 2, 4 ),
 ( 0.002243932016730776184, 0.002555488403984033582, 0.002867044791237291414 ),
 .UNSPECIFIED. ) ;
#125429 = CARTESIAN_POINT ( 'NONE',  ( 6.527322169609689695, -1.143008000885838760, -1.312471774050189444 ) ) ;
#125431 = ADVANCED_FACE ( 'NONE', ( #110845 ), #139921, .F. ) ;
#125430 = CARTESIAN_POINT ( 'NONE',  ( 6.727182134110170075, 7.629137130509032971, 2.310944104600751281 ) ) ;
#125432 = CARTESIAN_POINT ( 'NONE',  ( 4.717874267875568961, 4.606534188717351874, -0.7216878364870188411 ) ) ;
#125433 = CARTESIAN_POINT ( 'NONE',  ( 1.500000000000001332, 11.87499999999999645, 0.000000000000000000 ) ) ;
#125434 = CARTESIAN_POINT ( 'NONE',  ( 4.012696165952275962, 1.530467462299599513, -1.526897427004340280 ) ) ;
#125435 = EDGE_CURVE ( 'NONE', #13120, #51039, #200597, .T. ) ;
#125436 = TOROIDAL_SURFACE ( 'NONE', #87313, 1.052419468952678239, 0.9475805310473219834 ) ;
#125437 = CARTESIAN_POINT ( 'NONE',  ( 5.097029748277864591, 1.038832625704217527, -1.727738606215820205 ) ) ;
#125438 = CARTESIAN_POINT ( 'NONE',  ( -7.822691444960700125, 11.10992853822074444, -1.082531754730543083 ) ) ;
#125440 = CARTESIAN_POINT ( 'NONE',  ( 3.151412294154242844, -1.766339975446712174, -1.245920677233211871 ) ) ;
#125439 = TOROIDAL_SURFACE ( 'NONE', #4246, 12.17999999982603399, 0.5000000000000008882 ) ;
#125441 = CARTESIAN_POINT ( 'NONE',  ( 4.042224286460029958, 1.961553563453529492, 0.1965975345302218569 ) ) ;
#125442 = FILL_AREA_STYLE_COLOUR ( '', #33971 ) ;
#125443 = CARTESIAN_POINT ( 'NONE',  ( 0.7984239956072606281, -0.8271026589724904676, 2.154427444091823851 ) ) ;
#125444 = CARTESIAN_POINT ( 'NONE',  ( 2.073578556082512403, 1.972924284924733929, -0.5953725496260859895 ) ) ;
#125445 = CARTESIAN_POINT ( 'NONE',  ( 5.091328012616338938, -0.6953414466571452568, 1.813493487445563046 ) ) ;
#125448 = ORIENTED_EDGE ( 'NONE', *, *, #113684, .T. ) ;
#125447 = CARTESIAN_POINT ( 'NONE',  ( -6.828399852920244761, -6.891066458783222437, 6.756361134959175452 ) ) ;
#125446 = CARTESIAN_POINT ( 'NONE',  ( -8.148087131688683371, 11.48955683940339867, -1.082531754730543083 ) ) ;
#125449 = CARTESIAN_POINT ( 'NONE',  ( -5.094831863685302942, 9.165997284266655498, 0.7998128361456291469 ) ) ;
#125450 = DIRECTION ( 'NONE',  ( -0.6507913734559640506, -0.7592566023653004592, 0.000000000000000000 ) ) ;
#125452 = ORIENTED_EDGE ( 'NONE', *, *, #141149, .F. ) ;
#125451 = CARTESIAN_POINT ( 'NONE',  ( -3.955946960137363799, 7.837298230127379917, 0.7998128361456352531 ) ) ;
#125453 = CARTESIAN_POINT ( 'NONE',  ( -7.171900071504738072, 10.35067193585544665, -1.082531754730543083 ) ) ;
#125454 = CARTESIAN_POINT ( 'NONE',  ( 2.380145745526092593, 1.357289424207007489, 1.739932290444376584 ) ) ;
#125455 = CARTESIAN_POINT ( 'NONE',  ( 1.642778471875001811, -3.930208332855376074, 2.845375778867859751 ) ) ;
#125456 = CARTESIAN_POINT ( 'NONE',  ( 6.666857073735664052, 1.455856877570886887, -1.315125143065517532 ) ) ;
#125457 = CARTESIAN_POINT ( 'NONE',  ( 3.834746474454188013E-15, 9.062500000000001776, 1.500000000000001554 ) ) ;
#125458 = CARTESIAN_POINT ( 'NONE',  ( -1.001543065824772872E-14, 4.243750000682819490, 1.732050807568877637 ) ) ;
#125459 = CARTESIAN_POINT ( 'NONE',  ( -9.488641820551103834, -8.200000000000001066, 0.4644097342743105372 ) ) ;
#125461 = DIRECTION ( 'NONE',  ( 1.000000000000000000, -7.771561172376097755E-16, -4.440892098500627148E-16 ) ) ;
#125460 = CARTESIAN_POINT ( 'NONE',  ( 4.000000000000012434, 6.499999999999999112, -1.214306433183764966E-14 ) ) ;
#125462 = CARTESIAN_POINT ( 'NONE',  ( 5.367088761235753402, 1.773375748883701419, -0.4946613714205680967 ) ) ;
#125463 = ORIENTED_EDGE ( 'NONE', *, *, #21454, .F. ) ;
#125464 = CARTESIAN_POINT ( 'NONE',  ( 1.360316468749975582, -0.4635416663252802660, -0.7853790794159301036 ) ) ;
#125465 = CARTESIAN_POINT ( 'NONE',  ( -8.030507057996002729, 8.263346410617135263, 1.040834085586084257E-14 ) ) ;
#125466 = CARTESIAN_POINT ( 'NONE',  ( -3.070003471035267495, 6.451017196056028524, -0.6895117023006979151 ) ) ;
#125467 = CARTESIAN_POINT ( 'NONE',  ( 6.310795917644286490, -0.5669512758468171487, -2.043305014803979525 ) ) ;
#125468 = CARTESIAN_POINT ( 'NONE',  ( 9.281668279142875733, 11.48512158433666386, 7.535354720287775088 ) ) ;
#125469 = CARTESIAN_POINT ( 'NONE',  ( 5.671388329218120639, 5.511041227042920099, 1.040834085586084257E-14 ) ) ;
#125470 = CIRCLE ( 'NONE', #97732, 0.7499999999999997780 ) ;
#125471 = CARTESIAN_POINT ( 'NONE',  ( 0.5673477787482993362, 0.2024836561579176908, -2.050924697174760780 ) ) ;
#125472 = ADVANCED_FACE ( 'NONE', ( #120453 ), #201596, .T. ) ;
#125475 = CARTESIAN_POINT ( 'NONE',  ( 4.352959896991869471, 0.3989296284454147412, -1.797357466088687961 ) ) ;
#125474 = CARTESIAN_POINT ( 'NONE',  ( 2.189708182147569460, -1.212837473668834098, -1.411683579110091458 ) ) ;
#125473 = CYLINDRICAL_SURFACE ( 'NONE', #7294, 1.850000000000000089 ) ;
#125476 = CARTESIAN_POINT ( 'NONE',  ( 8.118635056484817980, 8.366162408854107113, 0.7998128361456481317 ) ) ;
#125477 = CARTESIAN_POINT ( 'NONE',  ( -5.633484485803696096, 15.51846582102598227, 10.60471134310094321 ) ) ;
#125478 = CARTESIAN_POINT ( 'NONE',  ( -6.479871072688648148, 6.524547437750345402, 0.000000000000000000 ) ) ;
#125480 = VERTEX_POINT ( 'NONE', #52181 ) ;
#125479 = CARTESIAN_POINT ( 'NONE',  ( 6.610000000000029630, 4.695285100415147461, 2.562642482393460153 ) ) ;
#125481 = CARTESIAN_POINT ( 'NONE',  ( 4.266400587755204477, 1.039063272370500668, 1.946970035688735390 ) ) ;
#125482 = CARTESIAN_POINT ( 'NONE',  ( 5.817715961848279882, -2.209163325107537101, 0.4873710261694869095 ) ) ;
#125483 = CARTESIAN_POINT ( 'NONE',  ( -5.043269954603569083, 7.867270132804026872, 1.082531754730560403 ) ) ;
#125484 = CARTESIAN_POINT ( 'NONE',  ( 0.07037084582631887575, 0.7337836260858082715, 1.766209603411242668 ) ) ;
#125485 = CARTESIAN_POINT ( 'NONE',  ( 6.262892222096183126, -0.1014175117164286682, -1.913191589401983528 ) ) ;
#125486 = CARTESIAN_POINT ( 'NONE',  ( -4.609606157881824373, 5.330435195252891667, 1.197383514668200144 ) ) ;
#125487 = DIRECTION ( 'NONE',  ( -0.000000000000000000, -0.000000000000000000, -1.000000000000000000 ) ) ;
#125488 = CARTESIAN_POINT ( 'NONE',  ( 5.619756671179352736, -0.4603523440993939619, 1.855926886426211952 ) ) ;
#125489 = CARTESIAN_POINT ( 'NONE',  ( 6.539320575229279342, 7.629137130509070275, 2.496737603865983868 ) ) ;
#125490 = CARTESIAN_POINT ( 'NONE',  ( 1.287742131874554552, -0.8442722623961744777, 1.669378388412197767 ) ) ;
#125491 = CARTESIAN_POINT ( 'NONE',  ( 2.114470590943520634, 1.957170936680457052, 0.4852650170619755565 ) ) ;
#125493 = CARTESIAN_POINT ( 'NONE',  ( 3.879594643445562152, 1.983085605235184845, -0.7095211871808704274 ) ) ;
#125492 = CARTESIAN_POINT ( 'NONE',  ( -7.479294296233107708, 11.87759377891399204, 0.7998128361456481317 ) ) ;
#125494 = CARTESIAN_POINT ( 'NONE',  ( 8.229962938695207342, 9.560377169021284871, 1.199719254218462483 ) ) ;
#125496 = CARTESIAN_POINT ( 'NONE',  ( -8.877891658850122880, 9.251961778280284321, 0.7998128361456462443 ) ) ;
#125495 = CARTESIAN_POINT ( 'NONE',  ( -1.500000000000001332, -0.09999999999997510880, 0.000000000000000000 ) ) ;
#125497 = CARTESIAN_POINT ( 'NONE',  ( 3.094014924146833323, 1.284692261361711774, 1.558518293110554565 ) ) ;
#125498 = CARTESIAN_POINT ( 'NONE',  ( -1.364683531250010295, 5.030208333674757171, 0.7879004041258379498 ) ) ;
#125499 = CARTESIAN_POINT ( 'NONE',  ( 8.595506201384004896, 12.01154575404795466, 1.082531754730546636 ) ) ;
#125500 = EDGE_CURVE ( 'NONE', #28251, #18174, #185457, .T. ) ;
#125501 = CARTESIAN_POINT ( 'NONE',  ( 4.288457955665158750, -2.137403104576699242, -0.3218062170811594735 ) ) ;
#125502 = CARTESIAN_POINT ( 'NONE',  ( 7.849244587668864348, 8.122149871893999062, 0.7998128361456291469 ) ) ;
#125503 = CARTESIAN_POINT ( 'NONE',  ( 1.499999999999989120, 5.254166666666684193, 0.8660254037844524744 ) ) ;
#125505 = SURFACE_STYLE_USAGE ( .BOTH. , #157940 ) ;
#125504 = CARTESIAN_POINT ( 'NONE',  ( 7.503511670520385479, 7.718794801887437274, 0.7998128361456281477 ) ) ;
#125506 = CARTESIAN_POINT ( 'NONE',  ( 7.551528372687370094, 11.75394083486988528, -0.7216878364870267237 ) ) ;
#125508 = CARTESIAN_POINT ( 'NONE',  ( -0.2972806740312780582, -7.751137252134800093, 10.97067717498812200 ) ) ;
#125507 = CARTESIAN_POINT ( 'NONE',  ( 1.891327416536987105, 0.2117802020594385659, 2.160802721360413070 ) ) ;
#125510 = CARTESIAN_POINT ( 'NONE',  ( 0.8371598888798935656, 0.7463826720714299423, -1.683355135116317847 ) ) ;
#125509 = CARTESIAN_POINT ( 'NONE',  ( -7.565086526745425033, 7.928281824065535055, 0.7216878364870317197 ) ) ;
#125511 = CARTESIAN_POINT ( 'NONE',  ( 1.364683531249990311, 2.634375000341422801, 1.214306433183764966E-14 ) ) ;
#125513 = CARTESIAN_POINT ( 'NONE',  ( 1.646283778714407342, 0.6915601415973006150, 2.079641132013386517 ) ) ;
#125512 = B_SPLINE_CURVE_WITH_KNOTS ( 'NONE', 3,
 ( #179934, #48870, #114986, #180986, #32607, #20599, #120330, #150640 ),
 .UNSPECIFIED., .F., .F.,
 ( 4, 2, 2, 4 ),
 ( 1.563658610346381350E-18, 0.001552951981419670906, 0.003105903962839340511, 0.006211807925678679287 ),
 .UNSPECIFIED. ) ;
#125514 = CARTESIAN_POINT ( 'NONE',  ( 6.883263157960376688, 2.059069814638575302, 2.260828084523508252 ) ) ;
#125515 = CARTESIAN_POINT ( 'NONE',  ( 3.608526635699527141, -0.9147260449715814978, -2.069530211360113725 ) ) ;
#125516 = CARTESIAN_POINT ( 'NONE',  ( -5.682838942422375084, 9.781729199468104596, 0.000000000000000000 ) ) ;
#125517 = CARTESIAN_POINT ( 'NONE',  ( 4.469935555517978720, -0.9463019959239076240, 1.780667052345537238 ) ) ;
#125518 = CARTESIAN_POINT ( 'NONE',  ( 0.6823417656249917140, 5.405208333674749177, 1.181850606188765695 ) ) ;
#125519 = CARTESIAN_POINT ( 'NONE',  ( 6.174897528274166270, 6.957956273452501783, 0.8961316764096085574 ) ) ;
#125520 = CARTESIAN_POINT ( 'NONE',  ( -1.500000000000015099, 11.97916666666666785, -0.8660254037844309360 ) ) ;
#125521 = CARTESIAN_POINT ( 'NONE',  ( 5.370438244788902971, 9.279612028980123384, -0.7216878364870458196 ) ) ;
#125522 = EDGE_CURVE ( 'NONE', #60515, #85555, #60404, .T. ) ;
#125523 = CARTESIAN_POINT ( 'NONE',  ( 4.270580540438973394, -1.650736559713336771, -0.6384287733962620282 ) ) ;
#125524 = CIRCLE ( 'NONE', #132443, 10.99999999999999112 ) ;
#125525 = CARTESIAN_POINT ( 'NONE',  ( 9.447334110624092673, 9.916311305349925220, -0.7998128361456281477 ) ) ;
#125526 = CARTESIAN_POINT ( 'NONE',  ( 1.061710303787483989, 0.4109483673962707750, -2.065292405001526443 ) ) ;
#125527 = STYLED_ITEM ( 'NONE', ( #118316 ), #53802 ) ;
#125529 = CARTESIAN_POINT ( 'NONE',  ( -1.500000000000013101, 1.379166666666689745, -0.8660254037844313801 ) ) ;
#125528 = CARTESIAN_POINT ( 'NONE',  ( -1.364683531250014514, 10.33854166700806765, -0.7879004041258335089 ) ) ;
#125530 = CARTESIAN_POINT ( 'NONE',  ( -5.646044625448194410, 5.551749915969804938, 0.000000000000000000 ) ) ;
#125531 = FACE_OUTER_BOUND ( 'NONE', #178334, .T. ) ;
#125532 = VERTEX_POINT ( 'NONE', #85741 ) ;
#125533 = CARTESIAN_POINT ( 'NONE',  ( 6.643132081016117851, 8.773406732650713025, 1.443375672974076540 ) ) ;
#125534 = CARTESIAN_POINT ( 'NONE',  ( 8.615316546479974136, 12.13862083994696839, 1.199719254218450271 ) ) ;
#125535 = CARTESIAN_POINT ( 'NONE',  ( 3.871829239884491791, 1.038646522470688671, 1.555605274479121114 ) ) ;
#125536 = CARTESIAN_POINT ( 'NONE',  ( 4.557524383921963462, 1.659614545607337677, 1.237363147772299721 ) ) ;
#125537 = CARTESIAN_POINT ( 'NONE',  ( -5.248414861821563804, 9.137251415518218067, 0.7216878364870267237 ) ) ;
#125538 = CARTESIAN_POINT ( 'NONE',  ( 8.402302512167096893, 10.82577223566020841, -1.599625672291268286 ) ) ;
#125539 = CARTESIAN_POINT ( 'NONE',  ( -9.398826802771548472, 11.98838390803207865, -1.599625672291263179 ) ) ;
#125540 = CARTESIAN_POINT ( 'NONE',  ( 6.505933609711257226, 8.683618192786854095, -1.599625672291281386 ) ) ;
#125541 = CARTESIAN_POINT ( 'NONE',  ( 5.086602265255201871, 4.915193406792433883, -0.1714109360824608297 ) ) ;
#125542 = ADVANCED_FACE ( 'NONE', ( #153951 ), #3398, .F. ) ;
#125543 = CARTESIAN_POINT ( 'NONE',  ( 0.6823417656249917140, 5.405208333674749177, 1.181850606188765695 ) ) ;
#125544 = CARTESIAN_POINT ( 'NONE',  ( 3.842202535371820993, -0.9690557767615382012, 1.705768119890891610 ) ) ;
#125545 = EDGE_CURVE ( 'NONE', #198714, #175863, #192410, .T. ) ;
#125546 = CARTESIAN_POINT ( 'NONE',  ( 1.686874821769188237, -1.117660090026689979, -1.677749154088927774 ) ) ;
#125547 = CARTESIAN_POINT ( 'NONE',  ( -2.823841133396259639, 6.516508098929413961, -0.7998128361456481317 ) ) ;
#125548 = CARTESIAN_POINT ( 'NONE',  ( 6.639320575229278099, 0.5905802482995252678, 1.949996947996739172 ) ) ;
#125549 = CARTESIAN_POINT ( 'NONE',  ( 0.5966796567213605851, 1.558732183387041781, -1.033768272189788950 ) ) ;
#125550 = CARTESIAN_POINT ( 'NONE',  ( -1.364683531250012516, 3.988541667008088876, -0.7879004041258300672 ) ) ;
#125551 = CARTESIAN_POINT ( 'NONE',  ( 3.023692480417307316, -0.3885771752702297799, 1.975188976417296072 ) ) ;
#125553 = CARTESIAN_POINT ( 'NONE',  ( 3.691103677939993499, 1.816986910410453682, 1.086596289330623799 ) ) ;
#125552 = CARTESIAN_POINT ( 'NONE',  ( -6.724481002698130538, 7.907944593645035880, -1.082531754730544860 ) ) ;
#125554 = CARTESIAN_POINT ( 'NONE',  ( 0.000000000000000000, 0.5999999999999998668, 0.000000000000000000 ) ) ;
#125555 = CARTESIAN_POINT ( 'NONE',  ( 5.020015195830264787, 2.048331326439792210, -0.3003445753073652469 ) ) ;
#125556 = CARTESIAN_POINT ( 'NONE',  ( 5.481239241674765950, 9.616805891921051952, -0.7998128361456481317 ) ) ;
#125558 = CARTESIAN_POINT ( 'NONE',  ( 2.866659414285625651, 5.431854185720147221, -1.199719254218446718 ) ) ;
#125557 = CARTESIAN_POINT ( 'NONE',  ( 0.1168898295945815374, -0.09829507837614966104, 2.088553102151818219 ) ) ;
#125560 = ORIENTED_EDGE ( 'NONE', *, *, #69557, .T. ) ;
#125559 = CARTESIAN_POINT ( 'NONE',  ( 4.998959831394860664, 1.517082468864182632, -1.015166198912627049 ) ) ;
#125561 = CARTESIAN_POINT ( 'NONE',  ( 9.023114925094663619, 10.48572115315399245, 1.199719254218453823 ) ) ;
#125562 = CARTESIAN_POINT ( 'NONE',  ( 3.697672731464857421, 7.367968498737394789, -2.499999999999995115 ) ) ;
#125564 = VECTOR ( 'NONE', #6911, 1000.000000000000000 ) ;
#125563 = CARTESIAN_POINT ( 'NONE',  ( 9.703911172298809618, 13.32558040432908619, 8.137536601084995880 ) ) ;
#125565 = CARTESIAN_POINT ( 'NONE',  ( -10.83017591827266557, 4.360326817186668258, 4.636531744782178777 ) ) ;
#125566 = CARTESIAN_POINT ( 'NONE',  ( -8.012344526598182026E-15, 12.60937500034139802, -1.575800808251669460 ) ) ;
#125567 = CARTESIAN_POINT ( 'NONE',  ( 6.639320575229252341, 0.005161017367553630275, 1.896863882003448021 ) ) ;
#125568 = CARTESIAN_POINT ( 'NONE',  ( -8.995998617867369873, 10.45408546138876993, 1.199719254218462483 ) ) ;
#125569 = CARTESIAN_POINT ( 'NONE',  ( 6.819914962873951936, 7.915321197229798322, -1.199719254218446718 ) ) ;
#125570 = CARTESIAN_POINT ( 'NONE',  ( -1.360316468750038865, 2.901041667008071645, -0.7853790794159161148 ) ) ;
#125571 = CARTESIAN_POINT ( 'NONE',  ( 4.541618270453549044, 5.361271406026338227, -1.082531754730548412 ) ) ;
#125572 = CARTESIAN_POINT ( 'NONE',  ( 9.536979704252619428, -7.995840219786838787, -0.1489494290324772929 ) ) ;
#125573 = CARTESIAN_POINT ( 'NONE',  ( 5.020596955762157698, 4.751784624677624080, 1.040834085586084257E-14 ) ) ;
#125574 = ORIENTED_EDGE ( 'NONE', *, *, #80137, .T. ) ;
#125575 = CARTESIAN_POINT ( 'NONE',  ( -6.936931872047518155, 8.122117267924091166, 1.199719254218452047 ) ) ;
#125577 = CARTESIAN_POINT ( 'NONE',  ( 6.505933609711257226, 8.683618192786854095, -1.599625672291281386 ) ) ;
#125576 = CARTESIAN_POINT ( 'NONE',  ( 0.1817359287054975125, -9.181675805132181623, -9.625413980971190497 ) ) ;
#125578 = CARTESIAN_POINT ( 'NONE',  ( -7.721398836998378812, -6.134628647623499909, 7.721398836998403681 ) ) ;
#125579 = CIRCLE ( 'NONE', #73537, 3.150000000000000799 ) ;
#125580 = AXIS2_PLACEMENT_3D ( 'NONE', #153923, #108434, #5492 ) ;
#125581 = LINE ( 'NONE', #88746, #92277 ) ;
#125582 = CARTESIAN_POINT ( 'NONE',  ( -4.582292731738899505, 8.289832587096611860, 0.7216878364870458196 ) ) ;
#125583 = CARTESIAN_POINT ( 'NONE',  ( 3.063252641683779753, 5.661212951017999373, 1.199719254218450271 ) ) ;
#125584 = CARTESIAN_POINT ( 'NONE',  ( 1.938274800925225527, -1.057869798513750847, 1.661026717510836637 ) ) ;
#125585 = CARTESIAN_POINT ( 'NONE',  ( 3.796500049179197589, 1.423950305759081214, -1.427950143821264506 ) ) ;
#125586 = CARTESIAN_POINT ( 'NONE',  ( -6.021792782764022078, 10.17717534653336209, -0.7998128361456291469 ) ) ;
#125587 = CARTESIAN_POINT ( 'NONE',  ( 6.727182134110194056, 3.682851444631680682, 2.702965647100654234 ) ) ;
#125588 = CARTESIAN_POINT ( 'NONE',  ( 3.574349206294104242, -2.111947977397998777, -0.5846811180381800144 ) ) ;
#125589 =( NAMED_UNIT ( * ) PLANE_ANGLE_UNIT ( ) SI_UNIT ( $, .RADIAN. ) );
#125590 = CARTESIAN_POINT ( 'NONE',  ( 1.905176762840081528, 1.600281962709374062, 1.072135106281972616 ) ) ;
#125591 = CARTESIAN_POINT ( 'NONE',  ( -8.188234707649510113, 11.64035869464474082, -1.199719254218446718 ) ) ;
#125592 =( NAMED_UNIT ( * ) PLANE_ANGLE_UNIT ( ) SI_UNIT ( $, .RADIAN. ) );
#125593 = CARTESIAN_POINT ( 'NONE',  ( 0.2331563151865451988, 4.092570554693980789, -2.500672995626152861 ) ) ;
#125594 = CARTESIAN_POINT ( 'NONE',  ( 7.096803341749390981, 10.36702210109460154, -1.199719254218441611 ) ) ;
#125595 = AXIS2_PLACEMENT_3D ( 'NONE', #185211, #36835, #133323 ) ;
#125596 = CARTESIAN_POINT ( 'NONE',  ( 5.281064527722868718, 6.119995689553514140, 1.199719254218462483 ) ) ;
#125597 = CARTESIAN_POINT ( 'NONE',  ( -6.661184041420952440, -7.473374494058216300, 6.773376349083141790 ) ) ;
#125598 = CARTESIAN_POINT ( 'NONE',  ( 4.584065335196252811, 8.362176967788721882, 0.7216878364870328300 ) ) ;
#125599 = ORIENTED_EDGE ( 'NONE', *, *, #25593, .T. ) ;
#125601 = CARTESIAN_POINT ( 'NONE',  ( 2.631496214491501728, -0.1952657482040425496, 2.003584891602292473 ) ) ;
#125600 = CARTESIAN_POINT ( 'NONE',  ( 5.513187957602974976, -1.795010045117376496, 0.4093405989887277663 ) ) ;
#125602 = CARTESIAN_POINT ( 'NONE',  ( 4.218341386676929261, -1.908100849112413178, -1.281069462185228325 ) ) ;
#125604 = CARTESIAN_POINT ( 'NONE',  ( 2.992830011424299830, 0.2227009285440742226, 1.847472864794322156 ) ) ;
#125603 = CARTESIAN_POINT ( 'NONE',  ( -0.1291982275798625457, 6.946856551170387029, -2.669038260222480918 ) ) ;
#125605 = CARTESIAN_POINT ( 'NONE',  ( 6.556249800660121529, 9.806652646482286073, 1.199719254218452047 ) ) ;
#125606 = DIRECTION ( 'NONE',  ( 2.949029909160572061E-17, 1.000000000000000000, -8.673600428462391266E-15 ) ) ;
#125607 = CARTESIAN_POINT ( 'NONE',  ( 6.381121926128928479, -1.751337275642101510, -0.7685668267764720341 ) ) ;
#125608 = B_SPLINE_CURVE_WITH_KNOTS ( 'NONE', 3,
 ( #27336, #68347, #115059, #184239, #198354, #119319 ),
 .UNSPECIFIED., .F., .F.,
 ( 4, 2, 4 ),
 ( 0.000000000000000000, 0.0003157158648874033901, 0.0006314317297748067801 ),
 .UNSPECIFIED. ) ;
#125609 = CARTESIAN_POINT ( 'NONE',  ( -6.821723845970312894, 11.11042825360738284, 0.000000000000000000 ) ) ;
#125610 = CARTESIAN_POINT ( 'NONE',  ( -4.773879485787619892, 7.623257595843924150, 1.082531754730549967 ) ) ;
#125611 = CARTESIAN_POINT ( 'NONE',  ( 5.548407312280490444, -1.647412313956169605, 1.287198389022710998 ) ) ;
#125612 = CARTESIAN_POINT ( 'NONE',  ( 5.151735183512854199, 8.954182114166247430, -0.7216878364870257245 ) ) ;
#125613 = ORIENTED_EDGE ( 'NONE', *, *, #156316, .T. ) ;
#125614 = CARTESIAN_POINT ( 'NONE',  ( 2.976681210565074842, 6.504977021307106533, -0.5719620471287272245 ) ) ;
#125615 = CARTESIAN_POINT ( 'NONE',  ( -2.788906526875773208E-15, 13.18750000000000000, -1.499999999999998446 ) ) ;
#125616 = CARTESIAN_POINT ( 'NONE',  ( 5.865779507164840645, 1.698138087647281358, -0.3015940010741220978 ) ) ;
#125617 = CARTESIAN_POINT ( 'NONE',  ( -5.382750679825375251, 6.238629533673094585, -1.199719254218446718 ) ) ;
#125618 = CARTESIAN_POINT ( 'NONE',  ( 1.863478119473166439, -0.08537559288352389308, -1.732189446134152266 ) ) ;
#125619 = CARTESIAN_POINT ( 'NONE',  ( -0.8965205372419083885, 14.55264382554858038, 11.93046248445855007 ) ) ;
#125620 = CARTESIAN_POINT ( 'NONE',  ( 6.604641253243924481, -6.414086731524403007, 7.221001870987142190 ) ) ;
#125621 = EDGE_CURVE ( 'NONE', #149864, #144610, #122257, .T. ) ;
#125622 = DIRECTION ( 'NONE',  ( 0.000000000000000000, 0.000000000000000000, -1.000000000000000000 ) ) ;
#125623 = CARTESIAN_POINT ( 'NONE',  ( 5.735278773323231327, -0.04571225511484919291, -2.170743740471086980 ) ) ;
#125624 = CARTESIAN_POINT ( 'NONE',  ( 4.775911370473768791, 1.053640644303525331, 1.490772598166143048 ) ) ;
#125625 = CARTESIAN_POINT ( 'NONE',  ( 2.694135368495911731, 0.9291169126603683326, -1.727816930623335745 ) ) ;
#125626 = CARTESIAN_POINT ( 'NONE',  ( 9.574755873860459232, 4.231292704880496025, 7.158835545600457095 ) ) ;
#125627 = CARTESIAN_POINT ( 'NONE',  ( -1.201851678989727383E-14, 5.587500000000021672, -1.732050807568863648 ) ) ;
#125628 = CARTESIAN_POINT ( 'NONE',  ( 6.740374924288304648, 11.01552117831172062, 1.040834085586084257E-14 ) ) ;
#125629 = CARTESIAN_POINT ( 'NONE',  ( 2.121885542695590487, -0.4617877489709980576, 2.069441001874790409 ) ) ;
#125630 = CARTESIAN_POINT ( 'NONE',  ( -4.121315508874280553, 3.910548969882488901, -0.7216878364870207285 ) ) ;
#125631 = CARTESIAN_POINT ( 'NONE',  ( -5.266540691475234404, 6.417032612176464923, -1.150853802781536039 ) ) ;
#125632 = CARTESIAN_POINT ( 'NONE',  ( 0.5497785174156321064, 1.531638494488884339, 1.392999266381978130 ) ) ;
#125634 = CARTESIAN_POINT ( 'NONE',  ( -6.009258394948636914E-15, 14.21875000068279782, -1.732050807568875195 ) ) ;
#125633 = DIRECTION ( 'NONE',  ( 0.000000000000000000, 0.000000000000000000, 1.000000000000000000 ) ) ;
#125636 = EDGE_LOOP ( 'NONE', ( #78409, #119485, #65580, #152717, #109854 ) ) ;
#125635 = CARTESIAN_POINT ( 'NONE',  ( 3.299698294838341539, 2.007417196159299255, -0.9513305067451423014 ) ) ;
#125637 = CARTESIAN_POINT ( 'NONE',  ( 1.055823836731560439, -1.452736638576918038, 1.781478128903237756 ) ) ;
#125639 = CARTESIAN_POINT ( 'NONE',  ( 6.825054090417398633, -1.883341039872712397, -0.8414091007707087400 ) ) ;
#125638 = CARTESIAN_POINT ( 'NONE',  ( 3.195971524519376494, 4.751719416737803847, -1.599625672291262513 ) ) ;
#125641 = CARTESIAN_POINT ( 'NONE',  ( -3.475000000000000533, -1.079166666666665941, -2.006292185433948827 ) ) ;
#125640 = CARTESIAN_POINT ( 'NONE',  ( 4.309512724297349884, 6.121127159803966933, 1.599625672291261402 ) ) ;
#125642 = CARTESIAN_POINT ( 'NONE',  ( 3.449547071718269020, -1.000000000000000888, 2.024999999999999023 ) ) ;
#125643 = CARTESIAN_POINT ( 'NONE',  ( 6.356982874815331641, 0.3076174260261410054, -1.815216213958574132 ) ) ;
#125644 = CARTESIAN_POINT ( 'NONE',  ( -0.2104748580754201015, 5.720428293583295520, -2.697747842008205943 ) ) ;
#125645 = CARTESIAN_POINT ( 'NONE',  ( 2.484998412088899489, 1.578176246201369093, -0.6962595882179720697 ) ) ;
#125646 = CARTESIAN_POINT ( 'NONE',  ( 0.7609543035823238544, -0.05432987398422234326, -2.015980609757315190 ) ) ;
#125647 = CARTESIAN_POINT ( 'NONE',  ( 3.182589804937531852, 1.813683736837278460, 1.412227471172630588 ) ) ;
#125648 = CARTESIAN_POINT ( 'NONE',  ( 2.970297248839429027, 1.207737455218102829, 1.912895951805194894 ) ) ;
#125649 = CARTESIAN_POINT ( 'NONE',  ( 5.602208710206744158, -2.106257355024013567, -0.001338375500582050358 ) ) ;
#125650 = CARTESIAN_POINT ( 'NONE',  ( -6.997416678428844072, 8.296645891989347987, 1.082531754730549078 ) ) ;
#125651 = CARTESIAN_POINT ( 'NONE',  ( 4.024454502147566615, 1.679793015868607409, 0.5571282570626963082 ) ) ;
#125653 = CARTESIAN_POINT ( 'NONE',  ( 6.374598633881160659, -0.1077809834691043772, -2.289980472931157252 ) ) ;
#125652 = CARTESIAN_POINT ( 'NONE',  ( 5.045042557616584489, 5.058506870073687267, 0.000000000000000000 ) ) ;
#125654 = CARTESIAN_POINT ( 'NONE',  ( 5.806566994037906326, 1.625791660643903791, 0.8640615347050364381 ) ) ;
#125655 = CARTESIAN_POINT ( 'NONE',  ( -3.262708522383007903, 6.958243709422141876, 1.040834085586084257E-14 ) ) ;
#125656 = CARTESIAN_POINT ( 'NONE',  ( 5.517805330637495231, 6.500156309574290248, -1.082531754730543083 ) ) ;
#125657 = CARTESIAN_POINT ( 'NONE',  ( 0.7499999999999885647, 3.566666666666690411, -1.299038105676658228 ) ) ;
#125658 = CARTESIAN_POINT ( 'NONE',  ( 4.541096662771787251, -1.693051203114638525, -1.391418086139440957 ) ) ;
#125659 = CARTESIAN_POINT ( 'NONE',  ( -3.216308754939891212, 4.775446185561722956, -1.599625672291262513 ) ) ;
#125660 = DIRECTION ( 'NONE',  ( -0.000000000000000000, 1.000000000000000000, -0.000000000000000000 ) ) ;
#125661 = CARTESIAN_POINT ( 'NONE',  ( 6.144996677366851401, -0.2998803957653916608, -2.048400609436632269 ) ) ;
#125662 = CARTESIAN_POINT ( 'NONE',  ( 0.3215004009857677092, -1.429452135790244549, -1.422604240635255479 ) ) ;
#125663 = CARTESIAN_POINT ( 'NONE',  ( -1.364683531249997417, 4.259375000341424133, 1.214306433183764966E-14 ) ) ;
#125664 = CARTESIAN_POINT ( 'NONE',  ( 3.352094138168077553, 1.926676517159428670, -0.0006976933946620245131 ) ) ;
#125665 = CARTESIAN_POINT ( 'NONE',  ( 0.6823417656249969321, 10.02604166700806587, -1.181850606188757036 ) ) ;
#125666 = CARTESIAN_POINT ( 'NONE',  ( -3.551873057100300990, 5.166937871415542283, 1.443375672974064550 ) ) ;
#125667 = CARTESIAN_POINT ( 'NONE',  ( -0.1750823283547575382, -0.9565501389544858180, -2.002587789130043205 ) ) ;
#125668 = ORIENTED_EDGE ( 'NONE', *, *, #136122, .T. ) ;
#125671 = AXIS2_PLACEMENT_3D ( 'NONE', #16232, #98586, #149461 ) ;
#125670 = SURFACE_STYLE_FILL_AREA ( #205759 ) ;
#125669 = CARTESIAN_POINT ( 'NONE',  ( -3.851925040058345573, 5.587274861525073355, -1.443375672974078761 ) ) ;
#125672 = CARTESIAN_POINT ( 'NONE',  ( 3.357615597678655917, 7.068968630600412695, 0.7998128361456321445 ) ) ;
#125673 = CARTESIAN_POINT ( 'NONE',  ( -9.569358774149646862, 4.446947634372958369, 7.167287524840457280 ) ) ;
#125674 = LINE ( 'NONE', #7553, #56021 ) ;
#125675 = CARTESIAN_POINT ( 'NONE',  ( 3.922984035321162022, 2.804646012044671899, -0.7749999999999935829 ) ) ;
#125676 = CARTESIAN_POINT ( 'NONE',  ( 10.68346185744421462, 11.56638637654751989, 0.000000000000000000 ) ) ;
#125678 = EDGE_CURVE ( 'NONE', #145532, #94342, #49635, .T. ) ;
#125677 = CARTESIAN_POINT ( 'NONE',  ( 0.9066075625437097774, 0.5660373911110065936, 1.878450800843839419 ) ) ;
#125679 = CARTESIAN_POINT ( 'NONE',  ( -0.6823417656250212460, 1.113541667008083325, 1.181850606188755259 ) ) ;
#125680 = CARTESIAN_POINT ( 'NONE',  ( 9.499668754385636404, -7.473374494045003757, 0.07933194154488391880 ) ) ;
#125681 = EDGE_CURVE ( 'NONE', #10371, #83814, #147450, .T. ) ;
#125682 = CARTESIAN_POINT ( 'NONE',  ( 5.107842384611220865, 0.6171798735227496113, -1.862306164846748491 ) ) ;
#125683 = CARTESIAN_POINT ( 'NONE',  ( -8.239604668803112375, 10.63595808506888396, -1.599625672291263179 ) ) ;
#125684 = CARTESIAN_POINT ( 'NONE',  ( -4.839897649954225223, 7.630002444046455778, 1.082531754730560403 ) ) ;
#125685 = CARTESIAN_POINT ( 'NONE',  ( 6.385629968321593353, 1.486944277142748572, 1.569300510047972219 ) ) ;
#125687 = VERTEX_POINT ( 'NONE', #157161 ) ;
#125686 = CARTESIAN_POINT ( 'NONE',  ( -8.879134602965971013, 3.426985321572576737, -7.474367077670519777 ) ) ;
#125688 = CARTESIAN_POINT ( 'NONE',  ( -1.001543065824772872E-14, 5.071875000341421469, 1.575800808251672791 ) ) ;
#125689 = CARTESIAN_POINT ( 'NONE',  ( 6.714144427970111906, -0.9273952116407166990, -1.739565242892411545 ) ) ;
#125690 = CARTESIAN_POINT ( 'NONE',  ( 6.643864291637132879, -0.08952462543848457854, -1.731637005886511593 ) ) ;
#125692 = CARTESIAN_POINT ( 'NONE',  ( 2.718528139169604341, 2.064530135181973591, 0.7356957861901700646 ) ) ;
#125691 = CARTESIAN_POINT ( 'NONE',  ( 0.6801582343749813520, 0.2239583336747300035, 1.178068619123796568 ) ) ;
#125693 = CARTESIAN_POINT ( 'NONE',  ( 4.981611329956401768, 2.155202031093924830, -0.8251229701327715826 ) ) ;
#125694 = CARTESIAN_POINT ( 'NONE',  ( 6.432896526414161542, 0.1972406338010060101, 2.051297006214629182 ) ) ;
#125695 = CARTESIAN_POINT ( 'NONE',  ( 1.851409727902778357, 1.936748846533197677, -0.1429498737708263245 ) ) ;
#125696 = CARTESIAN_POINT ( 'NONE',  ( -6.222829318548141586, 6.362315081168691044, 0.7216878364870317197 ) ) ;
#125697 = CARTESIAN_POINT ( 'NONE',  ( 11.84668730067608244, 10.90000000000000036, -1.320000000000001616 ) ) ;
#125699 = EDGE_CURVE ( 'NONE', #159480, #99453, #2212, .T. ) ;
#125698 = CARTESIAN_POINT ( 'NONE',  ( 5.220985865760717992, 1.604251394084664550, -1.386888226476624242 ) ) ;
#125700 = CARTESIAN_POINT ( 'NONE',  ( -0.3869524901764175295, 1.970899860167975914, 11.77270853017065377 ) ) ;
#125701 = CARTESIAN_POINT ( 'NONE',  ( 3.902970337090125863, -1.038992709432768891, -1.728002613881730598 ) ) ;
#125702 = CARTESIAN_POINT ( 'NONE',  ( -4.677199806590235376, 7.440188293455128665, 1.082531754730560403 ) ) ;
#125703 = CARTESIAN_POINT ( 'NONE',  ( -7.605197822622922210, 7.837428646007010613, -0.7998128361456362523 ) ) ;
#125704 = CARTESIAN_POINT ( 'NONE',  ( 9.398826802771546696, 11.98838390803207865, -1.599625672291262513 ) ) ;
#125705 = CARTESIAN_POINT ( 'NONE',  ( -5.000000000000000888, 0.2350621082554960051, -0.7749999999999935829 ) ) ;
#125706 = CARTESIAN_POINT ( 'NONE',  ( -7.286581212701773502, 7.465709267765667789, 0.7998128361456341429 ) ) ;
#125707 = CARTESIAN_POINT ( 'NONE',  ( -6.317173229324657413, 6.334733287159020954, 0.000000000000000000 ) ) ;
#125708 = CARTESIAN_POINT ( 'NONE',  ( -10.10575425844435138, 4.358269247758318699, 5.859476710806498900 ) ) ;
#125709 = ORIENTED_EDGE ( 'NONE', *, *, #88206, .T. ) ;
#125710 = CARTESIAN_POINT ( 'NONE',  ( 6.086805585656668960, -0.2997611930264115765, -2.038837977671539736 ) ) ;
#125711 = CARTESIAN_POINT ( 'NONE',  ( -7.878696662872776812, 8.364436659539265406, -0.7216878364870338292 ) ) ;
#125712 = CARTESIAN_POINT ( 'NONE',  ( 6.007671464186812749, 10.02305078494439883, 0.7216878364870317197 ) ) ;
#125713 = CARTESIAN_POINT ( 'NONE',  ( -4.776550190716183586, 4.467063398790632966, 1.214306433183764966E-14 ) ) ;
#125714 = CARTESIAN_POINT ( 'NONE',  ( -5.470505178835490590, 6.436924650462506392, 1.307677400191203709 ) ) ;
#125715 = CARTESIAN_POINT ( 'NONE',  ( 4.494788958170754078, -1.959534436568559190, -0.4887017053271830447 ) ) ;
#125717 = ORIENTED_EDGE ( 'NONE', *, *, #78734, .T. ) ;
#125716 = CARTESIAN_POINT ( 'NONE',  ( 0.7499999999999885647, 0.9833333333333569293, 1.299038105676657340 ) ) ;
#125719 = CARTESIAN_POINT ( 'NONE',  ( 8.215877900201359552, 11.56864606933486606, -1.082531754730543083 ) ) ;
#125718 = CARTESIAN_POINT ( 'NONE',  ( -3.980200614063634568, 6.801261928786307642, 1.199719254218452935 ) ) ;
#125720 = AXIS2_PLACEMENT_3D ( 'NONE', #4725, #149963, #54583 ) ;
#125721 = CARTESIAN_POINT ( 'NONE',  ( 6.602984505055297326, 7.662235663108029726, 1.199719254218462483 ) ) ;
#125722 = CARTESIAN_POINT ( 'NONE',  ( 4.557529213136806590, 0.4535224272249741562, -2.010195360780684393 ) ) ;
#125723 = CARTESIAN_POINT ( 'NONE',  ( 2.707657903872981553, 1.899618770239443366, 0.6767133375917554483 ) ) ;
#125724 = EDGE_LOOP ( 'NONE', ( #206617, #10354, #123185 ) ) ;
#125725 = DIRECTION ( 'NONE',  ( 0.000000000000000000, 0.000000000000000000, -1.000000000000000000 ) ) ;
#125726 = CARTESIAN_POINT ( 'NONE',  ( 5.352771719296971042, 5.139321848801576387, 0.7998128361456341429 ) ) ;
#125728 = EDGE_LOOP ( 'NONE', ( #76003, #131636, #81408, #32621 ) ) ;
#125727 = CARTESIAN_POINT ( 'NONE',  ( 0.006800380015300722461, 7.009756401597622144, -1.999988438675401881 ) ) ;
#125729 = CARTESIAN_POINT ( 'NONE',  ( 3.110703712691643918, 0.7282687159771012997, -1.880146464672841411 ) ) ;
#125730 = CARTESIAN_POINT ( 'NONE',  ( 2.325889007780062023, 1.785771638016835361, 0.4476198290149570602 ) ) ;
#125731 = CARTESIAN_POINT ( 'NONE',  ( 1.436587813502993249, 1.134030013130071346, -2.009770128656597876 ) ) ;
#125732 = CARTESIAN_POINT ( 'NONE',  ( 5.737035277238070385, 6.722237907313067140, -1.199719254218452047 ) ) ;
#125733 = CARTESIAN_POINT ( 'NONE',  ( 4.200566210393744448, -0.6737006675727378324, -2.054019326127386691 ) ) ;
#125734 = CARTESIAN_POINT ( 'NONE',  ( -7.400052914960538963, 7.527816577075747695, 1.040834085586084257E-14 ) ) ;
#125735 = CARTESIAN_POINT ( 'NONE',  ( 3.620768967900461099, 0.5618574718093732878, -2.228542275653460969 ) ) ;
#125736 = VERTEX_POINT ( 'NONE', #74834 ) ;
#125737 = DIRECTION ( 'NONE',  ( 0.000000000000000000, 0.000000000000000000, -1.000000000000000000 ) ) ;
#125738 = VECTOR ( 'NONE', #87525, 1000.000000000000000 ) ;
#125739 = CARTESIAN_POINT ( 'NONE',  ( 1.041631754505952134, 0.7616270086890539748, -1.708776438048253077 ) ) ;
#125740 = CIRCLE ( 'NONE', #59939, 1.250000000000000888 ) ;
#125741 = CARTESIAN_POINT ( 'NONE',  ( 5.418811373015061328, 1.821287777658405549, 0.7551675066918785983 ) ) ;
#125743 = CARTESIAN_POINT ( 'NONE',  ( 9.219181267168295335, 9.858059021225592744, 1.040834085586084257E-14 ) ) ;
#125742 = CARTESIAN_POINT ( 'NONE',  ( -0.6823417656249969321, 4.967708333674755394, -1.181850606188749264 ) ) ;
#125745 = CARTESIAN_POINT ( 'NONE',  ( 0.7334016978863610037, 0.1661181961954381059, 2.200687262777756725 ) ) ;
#125744 = CARTESIAN_POINT ( 'NONE',  ( -4.889686956022917919, 8.856385215335397021, 1.214306433183764966E-14 ) ) ;
#125746 = DIRECTION ( 'NONE',  ( -0.000000000000000000, 1.000000000000000000, -0.000000000000000000 ) ) ;
#125747 = CARTESIAN_POINT ( 'NONE',  ( 5.705283713252285338, 5.550585841749444249, -0.7998128361456211532 ) ) ;
#125748 = CARTESIAN_POINT ( 'NONE',  ( -5.225778143063529946, 8.184159369294361497, 1.199719254218452047 ) ) ;
#125749 = CARTESIAN_POINT ( 'NONE',  ( -0.4355862708379995563, -6.583980363595115293, -9.606148981167580203 ) ) ;
#125750 = CARTESIAN_POINT ( 'NONE',  ( 5.155133900154169169, -1.665016652684460530, -1.055383500247959461 ) ) ;
#125751 = CARTESIAN_POINT ( 'NONE',  ( 5.110162711920646750, -2.297000869944005430, 0.2220405423442091408 ) ) ;
#125752 = CARTESIAN_POINT ( 'NONE',  ( 6.039480578167179203, 1.719269793624801590, -0.7129749698730929452 ) ) ;
#125753 = CARTESIAN_POINT ( 'NONE',  ( 3.204023084367659813, 0.7466497159868844546, -1.922840047214324333 ) ) ;
#125754 = CARTESIAN_POINT ( 'NONE',  ( 5.829642864196157070, 8.784705193995428374, 1.082531754730558626 ) ) ;
#125755 = EDGE_CURVE ( 'NONE', #213959, #150697, #134824, .T. ) ;
#125757 = CARTESIAN_POINT ( 'NONE',  ( 5.879395890181562834, 6.888325289080478697, -1.199719254218452047 ) ) ;
#125756 = AXIS2_PLACEMENT_3D ( 'NONE', #36847, #167930, #100787 ) ;
#125758 = CARTESIAN_POINT ( 'NONE',  ( 3.627688620108284745, 6.389997935838436227, 1.199719254218452047 ) ) ;
#125759 = CARTESIAN_POINT ( 'NONE',  ( -0.6823417656250212460, 2.363541667008084435, 1.181850606188767472 ) ) ;
#125760 = CARTESIAN_POINT ( 'NONE',  ( -3.448037578273754011, 14.48027471475642081, 11.50286700577156651 ) ) ;
#125761 = CARTESIAN_POINT ( 'NONE',  ( 6.954969613686092345, 7.216478758829655504, -0.7216878364870257245 ) ) ;
#125762 = CARTESIAN_POINT ( 'NONE',  ( 5.828641854062238892, -1.381805371539744698, 1.674691576451936781 ) ) ;
#125764 = CARTESIAN_POINT ( 'NONE',  ( 3.931074656914943954, -1.272613488525012659, -1.330884258478791438 ) ) ;
#125763 = CARTESIAN_POINT ( 'NONE',  ( -3.795919822146293754, 4.491289883001181593, -1.082531754730549967 ) ) ;
#125766 = CARTESIAN_POINT ( 'NONE',  ( 6.720655732516628511, 2.062125556784020652, 2.233254568942647733 ) ) ;
#125765 = CARTESIAN_POINT ( 'NONE',  ( -1.364683531250010295, 5.738541667008088432, -0.7879004041258300672 ) ) ;
#125767 = CARTESIAN_POINT ( 'NONE',  ( 6.321842903100939104, 1.263506803105146847, -1.790488031206059372 ) ) ;
#125768 = DIRECTION ( 'NONE',  ( 2.949029909160572061E-17, 1.000000000000000000, -8.673600428462579015E-15 ) ) ;
#125769 = CARTESIAN_POINT ( 'NONE',  ( 6.825078400183548055, -0.008500281443135982926, 2.244262395727573356 ) ) ;
#125771 = CARTESIAN_POINT ( 'NONE',  ( -4.127707017443506210, 7.650024674618332021, -0.8198546088712642677 ) ) ;
#125770 = AXIS2_PLACEMENT_3D ( 'NONE', #91483, #22146, #153252 ) ;
#125772 = SURFACE_STYLE_USAGE ( .BOTH. , #91077 ) ;
#125773 = CARTESIAN_POINT ( 'NONE',  ( 6.509182584184366682, 6.829728176725765820, 0.5468608461018635847 ) ) ;
#125774 = CARTESIAN_POINT ( 'NONE',  ( -3.458738584817664385, 7.049295759013638474, 0.7216878364870338292 ) ) ;
#125775 = CARTESIAN_POINT ( 'NONE',  ( -3.231779075379149546, 6.036511184309975242, 0.9899555337401846344 ) ) ;
#125776 = CARTESIAN_POINT ( 'NONE',  ( 0.6019893773144822102, -0.5904995772347610972, -1.668576399176853853 ) ) ;
#125777 = CARTESIAN_POINT ( 'NONE',  ( 5.373694559265936199, 0.3904673514037678150, -1.974700560916352154 ) ) ;
#125778 = CARTESIAN_POINT ( 'NONE',  ( 4.794779880727245036, 8.745660294157122649, -0.7998128361456281477 ) ) ;
#125779 = CARTESIAN_POINT ( 'NONE',  ( 4.295997052264050708, -0.8081792604435251715, 1.944918383092561376 ) ) ;
#125780 = CARTESIAN_POINT ( 'NONE',  ( 3.655789272196503514, 1.066996606607173659, 1.590710377612122750 ) ) ;
#125781 = CARTESIAN_POINT ( 'NONE',  ( -11.84668730067608600, 10.89999999999998259, 1.319999999999998286 ) ) ;
#125782 = CARTESIAN_POINT ( 'NONE',  ( 4.475032023839897732, 1.799880929630924165, 0.8001706733358445733 ) ) ;
#125783 = CARTESIAN_POINT ( 'NONE',  ( 5.871354875427445386, -1.734483768580237673, -1.034654692648151464 ) ) ;
#125784 = CARTESIAN_POINT ( 'NONE',  ( 1.797508989346347619, -0.6330400025267440833, 1.760413054629046625 ) ) ;
#125787 = ORIENTED_EDGE ( 'NONE', *, *, #77070, .T. ) ;
#125786 = CARTESIAN_POINT ( 'NONE',  ( 1.564566645345835116, 0.6029492335615972420, 1.814891859350221459 ) ) ;
#125785 = CARTESIAN_POINT ( 'NONE',  ( 4.687984124052484880, -0.8092498044112338418, 1.523260386444349468 ) ) ;
#125789 = CARTESIAN_POINT ( 'NONE',  ( 5.355107487717867265, 5.349972945200037522, 1.040834085586084257E-14 ) ) ;
#125788 = CARTESIAN_POINT ( 'NONE',  ( 2.139570144280181108, -1.970530345926827742, 0.9937953903183869286 ) ) ;
#125790 = CARTESIAN_POINT ( 'NONE',  ( 0.6823417656249899377, 1.655208333674752730, 1.181850606188755259 ) ) ;
#125791 = CARTESIAN_POINT ( 'NONE',  ( 6.812952578306354035, -1.517200236233799071, 1.243500037895750143 ) ) ;
#125792 = CARTESIAN_POINT ( 'NONE',  ( 8.426556166093362776, 9.789735934319136135, -1.199719254218446718 ) ) ;
#125793 = CARTESIAN_POINT ( 'NONE',  ( -6.956180625285975694, -6.372104534813817445, 6.956180625285645291 ) ) ;
#125794 = CARTESIAN_POINT ( 'NONE',  ( -3.445171926680890451, 6.328521679139374356, -0.9347783054773143308 ) ) ;
#125795 = CARTESIAN_POINT ( 'NONE',  ( -4.283486466913726254, 7.084819080452935403, -1.199719254218452047 ) ) ;
#125796 = CARTESIAN_POINT ( 'NONE',  ( 0.000000000000000000, 11.37999999999999901, 0.000000000000000000 ) ) ;
#125797 =( BOUNDED_SURFACE ( )  B_SPLINE_SURFACE ( 1, 2, ( 
 ( #149805, #70645, #136755, #164975, #36030, #67440, #201715, #54434, #181219, #16567, #82650, #148734, #133585, #302, #66373, #132521, #34958, #198519, #101029, #167120, #73883, #156214, #56570, #105336, #76012, #40328, #170300, #91219, #25116, #6719, #26184, #204917, #203850, #8869, #208128, #39244, #124844, #7790, #157280, #108580, #55495, #106433, #121649, #139976, #205998, #122729, #142115, #188692, #207066, #57634, #71716, #190810, #104254, #174608, #74948, #123793, #21888, #137829, #141059, #41403, #172455, #120576, #189751, #24042, #107513, #173542, #90146, #171373, #186553, #58696, #87998, #42470, #92299, #72798, #158343, #9937, #187616, #38182, #154070, #22966, #5635, #89081, #155138, #138898, #146101, #48588, #212112, #164455, #82125, #213182, #84268, #64811, #149270, #16042, #10991, #66914, #43536, #116826, #181748, #65849, #175661, #77066, #99460, #198007, #49634, #133055, #849, #199056, #196948, #63749, #125917, #34443, #130958, #83187, #147157, #81071, #180699, #27248, #50702, #150353, #163400, #109659, #129908, #182828, #100517, #131998, #32323, #148218, #115758, #191876, #114704, #33379, #166592, #165517, #98391, #179648, #18181, #59757, #214220 ),
 ( #93355, #159392, #17109, #195892, #47530, #113643, #31268, #97343, #14975, #170854, #168719, #135179, #200134, #187094, #105903, #52833, #87481, #202259, #201194, #102661, #118970, #117904, #2992, #4055, #89629, #184948, #36575, #171927, #20322, #69059, #88555, #204390, #67982, #37656, #151418, #103733, #104809, #120045, #138372, #39796, #72264, #86408, #54978, #154616, #1924, #152475, #153547, #167654, #136237, #22444, #56045, #101586, #21373, #6195, #122201, #134125, #35509, #70125, #38728, #188163, #53910, #186019, #19255, #203326, #51787, #23523, #183897, #85336, #169784, #5116, #71193, #137310, #121131, #193507, #45148, #9421, #93903, #57109, #207610, #92833, #155681, #190292, #174087, #75492, #139442, #111260, #177263, #141603, #25660, #127535, #208668, #43018, #110194, #91769, #59229, #40879, #61378, #157825, #28878, #143740, #60299, #205477, #142658, #124332, #192421, #7263, #125387, #191353, #126457, #109132, #44075, #123278, #73340, #108062, #189240, #176204, #27805, #175145, #10473, #77617, #159942, #26731, #11547, #41949, #209734, #106984, #173009, #8347, #24590, #90697, #74432, #158877, #156760, #76547, #140532, #206544, #58174, #116566, #33131 ) ),
 .UNSPECIFIED., .F., .F., .T. ) 
 B_SPLINE_SURFACE_WITH_KNOTS ( ( 2, 2 ),
 ( 3, 2, 2, 2, 2, 2, 2, 2, 2, 2, 2, 2, 2, 2, 2, 2, 2, 2, 2, 2, 2, 2, 2, 2, 2, 2, 2, 2, 2, 2, 2, 2, 2, 2, 2, 2, 2, 2, 2, 2, 2, 2, 2, 2, 2, 2, 2, 2, 2, 2, 2, 2, 2, 2, 2, 2, 2, 2, 2, 2, 2, 2, 2, 2, 2, 2, 2, 2, 2, 3 ),
 ( 0.000000000000000000, 1.000000000000000000 ),
 ( 0.000000000000000000, 0.01388888888888888812, 0.02777777777777777624, 0.04166666666666666435, 0.05555555555555555247, 0.06944444444444444753, 0.08333333333333332871, 0.09722222222222222376, 0.1111111111111111049, 0.1250000000000000000, 0.1388888888888888951, 0.1527777777777777901, 0.1666666666666666574, 0.1805555555555555525, 0.1944444444444444475, 0.2083333333333333426, 0.2222222222222222099, 0.2361111111111111049, 0.2500000000000000000, 0.2638888888888888951, 0.2777777777777777901, 0.2916666666666666852, 0.3055555555555555802, 0.3194444444444444198, 0.3333333333333333148, 0.3472222222222222099, 0.3611111111111111049, 0.3750000000000000000, 0.3888888888888888951, 0.4027777777777777901, 0.4166666666666666852, 0.4305555555555555802, 0.4444444444444444198, 0.4583333333333333148, 0.4722222222222222099, 0.4861111111111111049, 0.5000000000000000000, 0.5138888888888888395, 0.5277777777777777901, 0.5416666666666666297, 0.5555555555555555802, 0.5694444444444444198, 0.5833333333333333703, 0.5972222222222222099, 0.6111111111111111605, 0.6250000000000000000, 0.6388888888888888395, 0.6527777777777777901, 0.6666666666666666297, 0.6805555555555555802, 0.6944444444444444198, 0.7083333333333333703, 0.7222222222222222099, 0.7361111111111111605, 0.7500000000000000000, 0.7638888888888888395, 0.7777777777777777901, 0.7916666666666666297, 0.8055555555555555802, 0.8194444444444444198, 0.8333333333333333703, 0.8472222222222222099, 0.8611111111111111605, 0.8750000000000000000, 0.8888888888888888395, 0.9027777777777777901, 0.9166666666666666297, 0.9305555555555555802, 0.9444444444444444198, 0.9523586353390159909 ),
 .UNSPECIFIED. ) 
 GEOMETRIC_REPRESENTATION_ITEM ( )  RATIONAL_B_SPLINE_SURFACE ( (
 ( 1.000000000000000000, 0.8660254037844387076, 1.000000000000000000, 0.8660254037844387076, 1.000000000000000000, 0.8660254037844387076, 1.000000000000000000, 0.8660254037844387076, 1.000000000000000000, 0.8660254037844387076, 1.000000000000000000, 0.8660254037844387076, 1.000000000000000000, 0.8660254037844387076, 1.000000000000000000, 0.8660254037844387076, 1.000000000000000000, 0.8660254037844387076, 1.000000000000000000, 0.8660254037844387076, 1.000000000000000000, 0.8660254037844387076, 1.000000000000000000, 0.8660254037844387076, 1.000000000000000000, 0.8660254037844387076, 1.000000000000000000, 0.8660254037844387076, 1.000000000000000000, 0.8660254037844387076, 1.000000000000000000, 0.8660254037844387076, 1.000000000000000000, 0.8660254037844387076, 1.000000000000000000, 0.8660254037844387076, 1.000000000000000000, 0.8660254037844387076, 1.000000000000000000, 0.8660254037844387076, 1.000000000000000000, 0.8660254037844387076, 1.000000000000000000, 0.8660254037844387076, 1.000000000000000000, 0.8660254037844387076, 1.000000000000000000, 0.8660254037844387076, 1.000000000000000000, 0.8660254037844387076, 1.000000000000000000, 0.8660254037844387076, 1.000000000000000000, 0.8660254037844387076, 1.000000000000000000, 0.8660254037844387076, 1.000000000000000000, 0.8660254037844387076, 1.000000000000000000, 0.8660254037844387076, 1.000000000000000000, 0.8660254037844387076, 1.000000000000000000, 0.8660254037844387076, 1.000000000000000000, 0.8660254037844387076, 1.000000000000000000, 0.8660254037844387076, 1.000000000000000000, 0.8660254037844387076, 1.000000000000000000, 0.8660254037844387076, 1.000000000000000000, 0.8660254037844387076, 1.000000000000000000, 0.8660254037844387076, 1.000000000000000000, 0.8660254037844387076, 1.000000000000000000, 0.8660254037844387076, 1.000000000000000000, 0.8660254037844387076, 1.000000000000000000, 0.8660254037844387076, 1.000000000000000000, 0.8660254037844387076, 1.000000000000000000, 0.8660254037844387076, 1.000000000000000000, 0.8660254037844387076, 1.000000000000000000, 0.8660254037844387076, 1.000000000000000000, 0.8660254037844387076, 1.000000000000000000, 0.8660254037844387076, 1.000000000000000000, 0.8660254037844387076, 1.000000000000000000, 0.8660254037844387076, 1.000000000000000000, 0.8660254037844387076, 1.000000000000000000, 0.8660254037844387076, 1.000000000000000000, 0.8660254037844387076, 1.000000000000000000, 0.8660254037844387076, 1.000000000000000000, 0.8660254037844387076, 1.000000000000000000, 0.8660254037844387076, 1.000000000000000000, 0.8660254037844387076, 1.000000000000000000, 0.8660254037844387076, 1.000000000000000000, 0.8660254037844387076, 1.000000000000000000, 0.8660254037844387076, 1.000000000000000000, 0.8660254037844387076, 1.000000000000000000, 0.8660254037844387076, 1.000000000000000000, 0.8660254037844387076, 1.000000000000000000, 0.8660254037844387076, 1.000000000000000000, 0.8660254037844387076, 1.000000000000000000, 0.8660254037844387076, 1.000000000000000000, 0.8660254037844387076, 1.000000000000000000, 0.8660254037844387076, 1.000000000000000000, 0.9236583618779372618, 0.9343189745674063129),
 ( 1.000000000000000000, 0.8660254037844387076, 1.000000000000000000, 0.8660254037844387076, 1.000000000000000000, 0.8660254037844387076, 1.000000000000000000, 0.8660254037844387076, 1.000000000000000000, 0.8660254037844387076, 1.000000000000000000, 0.8660254037844387076, 1.000000000000000000, 0.8660254037844387076, 1.000000000000000000, 0.8660254037844387076, 1.000000000000000000, 0.8660254037844387076, 1.000000000000000000, 0.8660254037844387076, 1.000000000000000000, 0.8660254037844387076, 1.000000000000000000, 0.8660254037844387076, 1.000000000000000000, 0.8660254037844387076, 1.000000000000000000, 0.8660254037844387076, 1.000000000000000000, 0.8660254037844387076, 1.000000000000000000, 0.8660254037844387076, 1.000000000000000000, 0.8660254037844387076, 1.000000000000000000, 0.8660254037844387076, 1.000000000000000000, 0.8660254037844387076, 1.000000000000000000, 0.8660254037844387076, 1.000000000000000000, 0.8660254037844387076, 1.000000000000000000, 0.8660254037844387076, 1.000000000000000000, 0.8660254037844387076, 1.000000000000000000, 0.8660254037844387076, 1.000000000000000000, 0.8660254037844387076, 1.000000000000000000, 0.8660254037844387076, 1.000000000000000000, 0.8660254037844387076, 1.000000000000000000, 0.8660254037844387076, 1.000000000000000000, 0.8660254037844387076, 1.000000000000000000, 0.8660254037844387076, 1.000000000000000000, 0.8660254037844387076, 1.000000000000000000, 0.8660254037844387076, 1.000000000000000000, 0.8660254037844387076, 1.000000000000000000, 0.8660254037844387076, 1.000000000000000000, 0.8660254037844387076, 1.000000000000000000, 0.8660254037844387076, 1.000000000000000000, 0.8660254037844387076, 1.000000000000000000, 0.8660254037844387076, 1.000000000000000000, 0.8660254037844387076, 1.000000000000000000, 0.8660254037844387076, 1.000000000000000000, 0.8660254037844387076, 1.000000000000000000, 0.8660254037844387076, 1.000000000000000000, 0.8660254037844387076, 1.000000000000000000, 0.8660254037844387076, 1.000000000000000000, 0.8660254037844387076, 1.000000000000000000, 0.8660254037844387076, 1.000000000000000000, 0.8660254037844387076, 1.000000000000000000, 0.8660254037844387076, 1.000000000000000000, 0.8660254037844387076, 1.000000000000000000, 0.8660254037844387076, 1.000000000000000000, 0.8660254037844387076, 1.000000000000000000, 0.8660254037844387076, 1.000000000000000000, 0.8660254037844387076, 1.000000000000000000, 0.8660254037844387076, 1.000000000000000000, 0.8660254037844387076, 1.000000000000000000, 0.8660254037844387076, 1.000000000000000000, 0.8660254037844387076, 1.000000000000000000, 0.8660254037844387076, 1.000000000000000000, 0.8660254037844387076, 1.000000000000000000, 0.8660254037844387076, 1.000000000000000000, 0.8660254037844387076, 1.000000000000000000, 0.8660254037844387076, 1.000000000000000000, 0.8660254037844387076, 1.000000000000000000, 0.8660254037844387076, 1.000000000000000000, 0.8660254037844387076, 1.000000000000000000, 0.8660254037844387076, 1.000000000000000000, 0.8660254037844387076, 1.000000000000000000, 0.8660254037844387076, 1.000000000000000000, 0.9236583618779372618, 0.9343189745674063129) ) ) 
 REPRESENTATION_ITEM ( '' )  SURFACE ( )  );
#125798 = ORIENTED_EDGE ( 'NONE', *, *, #174533, .F. ) ;
#125799 = CARTESIAN_POINT ( 'NONE',  ( 1.785682506433339478, -1.950172559450613852, 0.6955597780969878796 ) ) ;
#125800 = CARTESIAN_POINT ( 'NONE',  ( 1.499999999999989120, 3.525000000000021227, 1.214306433183764966E-14 ) ) ;
#125801 = CARTESIAN_POINT ( 'NONE',  ( 5.449487677688982679, 8.445153826357429949, -1.199719254218446718 ) ) ;
#125802 = CARTESIAN_POINT ( 'NONE',  ( -6.015013705957189316, 10.16926642359206134, 0.7998128361456481317 ) ) ;
#125803 = CARTESIAN_POINT ( 'NONE',  ( 4.553559489343365740, 6.405848385690952718, -1.599625672291269396 ) ) ;
#125804 = CARTESIAN_POINT ( 'NONE',  ( 0.06511101446048017660, -1.620675302784078786, 1.204964419619258376 ) ) ;
#125805 = CARTESIAN_POINT ( 'NONE',  ( 7.439168848973994663, -6.893137084989842123, 8.103009739378013165 ) ) ;
#125806 = ADVANCED_FACE ( 'NONE', ( #9815 ), #57610, .F. ) ;
#125807 = CARTESIAN_POINT ( 'NONE',  ( -1.402160292154681736E-14, 1.946875000341422579, -1.575800808251660134 ) ) ;
#125809 = CARTESIAN_POINT ( 'NONE',  ( 2.523789150438203510, 6.096171108819874007, 0.7998128361456462443 ) ) ;
#125808 = CARTESIAN_POINT ( 'NONE',  ( -11.52463353791760348, 11.38000000000000078, -3.346594096177641475 ) ) ;
#125810 = CARTESIAN_POINT ( 'NONE',  ( 5.764999918528635803, -2.016288307888712161, -0.002809016773450134351 ) ) ;
#125811 = CARTESIAN_POINT ( 'NONE',  ( 4.452287505575288407, -1.246817998045848697, 1.454578644467845017 ) ) ;
#125812 = CARTESIAN_POINT ( 'NONE',  ( 2.753686713869853531, 2.180749500395392282, -0.2175628297749406803 ) ) ;
#125813 = CARTESIAN_POINT ( 'NONE',  ( 5.996449078994045223, 10.21788403546024782, 0.7998128361456331437 ) ) ;
#125814 = CARTESIAN_POINT ( 'NONE',  ( -1.201851678989727383E-14, 0.7437500006828187127, 1.732050807568877637 ) ) ;
#125815 = CARTESIAN_POINT ( 'NONE',  ( 5.150644359860614863, 1.984129689857921486, 0.3399971717471597654 ) ) ;
#125816 = CARTESIAN_POINT ( 'NONE',  ( 1.107505169401588274, 1.450017293480215352, 1.247013401884336403 ) ) ;
#125817 = CARTESIAN_POINT ( 'NONE',  ( -7.067878151425722955, 7.140279352951794500, 0.7998128361456341429 ) ) ;
#125818 = EDGE_CURVE ( 'NONE', #93819, #186231, #123412, .T. ) ;
#125820 = CARTESIAN_POINT ( 'NONE',  ( 6.485961931490698440, -2.116758087377061504, 0.05204923864161013075 ) ) ;
#125819 = CARTESIAN_POINT ( 'NONE',  ( -2.168941388506379742, 5.474256019991960542, -0.7216878364870267237 ) ) ;
#125821 = CARTESIAN_POINT ( 'NONE',  ( 1.364683531250000303, 10.31770833367473195, -0.7879004041258355073 ) ) ;
#125823 = CARTESIAN_POINT ( 'NONE',  ( -6.038177310039794854, 8.137902509836795417, -1.599625672291271394 ) ) ;
#125822 = CARTESIAN_POINT ( 'NONE',  ( 3.843375017719421916, 0.7025675959630849343, -1.969317001441653670 ) ) ;
#125825 = ORIENTED_EDGE ( 'NONE', *, *, #88823, .F. ) ;
#125824 = CARTESIAN_POINT ( 'NONE',  ( 1.711479192339813382, -1.712302428074402583, 0.2063632002643790431 ) ) ;
#125826 = CARTESIAN_POINT ( 'NONE',  ( 4.462605117192430804, 8.358123070033169455, 1.040834085586084257E-14 ) ) ;
#125827 = CARTESIAN_POINT ( 'NONE',  ( -7.834948825496944380, -6.307829212974244371, -7.720982897393569466 ) ) ;
#125828 = CARTESIAN_POINT ( 'NONE',  ( -0.9311234436981532525, -2.334380368602567035, 3.474999999999999201 ) ) ;
#125829 = CARTESIAN_POINT ( 'NONE',  ( 0.000000000000000000, 1.551257596039481879, 0.000000000000000000 ) ) ;
#125830 = CARTESIAN_POINT ( 'NONE',  ( 4.873266149108180123, 7.772895376346490970, 1.199719254218462483 ) ) ;
#125831 = ORIENTED_EDGE ( 'NONE', *, *, #79219, .T. ) ;
#125833 = VECTOR ( 'NONE', #83673, 1000.000000000000000 ) ;
#125832 = CARTESIAN_POINT ( 'NONE',  ( -11.91292854676703605, 13.61481529673005397, -1.446370920797322102 ) ) ;
#125834 = CARTESIAN_POINT ( 'NONE',  ( 2.683996807801437789, 0.9705641499191748345, 1.529316921005590357 ) ) ;
#125835 = ORIENTED_EDGE ( 'NONE', *, *, #72672, .F. ) ;
#125836 = CARTESIAN_POINT ( 'NONE',  ( 3.379006598303866848, 4.965260336153046516, -1.599625672291262513 ) ) ;
#125837 = AXIS2_PLACEMENT_3D ( 'NONE', #192243, #12428, #208490 ) ;
#125838 = CARTESIAN_POINT ( 'NONE',  ( 3.901714345682657292, 7.774026846596938434, 0.7998128361456271485 ) ) ;
#125839 = CARTESIAN_POINT ( 'NONE',  ( 3.984856247070994506, -1.691632632888851351, -0.6484230535298250997 ) ) ;
#125840 = DIRECTION ( 'NONE',  ( -1.561251128379126077E-17, -1.301042606982605475E-17, -1.000000000000000000 ) ) ;
#125841 = CARTESIAN_POINT ( 'NONE',  ( -10.96381302404150482, -7.750949308401941629, 0.4891431138945980250 ) ) ;
#125842 = CARTESIAN_POINT ( 'NONE',  ( 5.290189798603822879, 6.367883502209223501, 1.128355864069837455 ) ) ;
#125843 = CARTESIAN_POINT ( 'NONE',  ( 4.035495103658576888, 1.752908062920730092, -0.6255878229263853729 ) ) ;
#125844 = CARTESIAN_POINT ( 'NONE',  ( 1.528765853866232538, -1.617345627753681514, 1.026210199876474105 ) ) ;
#125845 = CARTESIAN_POINT ( 'NONE',  ( 0.4459769555512117511, 1.820297760642339391, 0.1397589855641478973 ) ) ;
#125846 = PRESENTATION_STYLE_ASSIGNMENT (( #5570 ) ) ;
#125847 = CARTESIAN_POINT ( 'NONE',  ( -9.868259782058050433, 3.553064995558723904, -6.768212174838916795 ) ) ;
#125848 = ADVANCED_FACE ( 'NONE', ( #58577, #88961 ), #190691, .T. ) ;
#125849 = PRESENTATION_LAYER_ASSIGNMENT (  '', '', ( #139542 ) ) ;
#125850 = CARTESIAN_POINT ( 'NONE',  ( 6.198956711081595294, 6.941498593865138567, 0.8670033951987624610 ) ) ;
#125851 = CARTESIAN_POINT ( 'NONE',  ( -1.500000000000001110, 8.520833333333337478, 0.8660254037844418162 ) ) ;
#125852 = CARTESIAN_POINT ( 'NONE',  ( -10.99943592164173012, -9.901472394401615418, 0.1113975120799921142 ) ) ;
#125853 = FACE_OUTER_BOUND ( 'NONE', #138672, .T. ) ;
#125854 = CARTESIAN_POINT ( 'NONE',  ( 6.453317930424781856, 10.47269531889685545, -0.7216878364870267237 ) ) ;
#125855 = CARTESIAN_POINT ( 'NONE',  ( 6.227403457816463650, 0.1483525144864000778, -1.963943935631215165 ) ) ;
#125856 = CARTESIAN_POINT ( 'NONE',  ( -5.603597561149804562, 5.431951997629870910, 0.7998128361456341429 ) ) ;
#125857 = CARTESIAN_POINT ( 'NONE',  ( -0.2462715347619852391, 7.026474760181363521, 3.914608670279890568 ) ) ;
#125858 = CARTESIAN_POINT ( 'NONE',  ( 0.005962723626575306898, -0.8962717426808585186, -1.887145544106306083 ) ) ;
#125859 = CARTESIAN_POINT ( 'NONE',  ( 7.527801604085637699, 9.805521176231838609, 1.599625672291281386 ) ) ;
#125860 = CARTESIAN_POINT ( 'NONE',  ( 5.825206220505295462, -0.04701585971965925592, 1.925982856303788182 ) ) ;
#125861 = CARTESIAN_POINT ( 'NONE',  ( -4.869349725602420520, 8.832658446511480577, 1.040834085586084257E-14 ) ) ;
#125862 = CARTESIAN_POINT ( 'NONE',  ( 1.360069071312763223, 0.7361036424862777983, 1.670779996689908398 ) ) ;
#125863 = CARTESIAN_POINT ( 'NONE',  ( 1.664966938652842954, -1.558911317520403239, 1.562347339584921002 ) ) ;
#125864 = CYLINDRICAL_SURFACE ( 'NONE', #44726, 1.500000000000000222 ) ;
#125865 = CARTESIAN_POINT ( 'NONE',  ( 0.5801457039020865292, 0.9447208859736742070, 1.662703529197881558 ) ) ;
#125866 = CARTESIAN_POINT ( 'NONE',  ( 0.4144234639597261238, 0.7504023841088992564, 1.821203888109582447 ) ) ;
#125867 = CARTESIAN_POINT ( 'NONE',  ( 2.647912457843327960, 0.6564901929842799078, 1.827849683178353057 ) ) ;
#125868 = ORIENTED_EDGE ( 'NONE', *, *, #133443, .T. ) ;
#125869 = CARTESIAN_POINT ( 'NONE',  ( 0.5618747747782488755, 1.677749815653075460, -1.117659098820653174 ) ) ;
#125871 = CARTESIAN_POINT ( 'NONE',  ( 6.086726144739807332, 1.793049480792831440, 0.4976782122840143763 ) ) ;
#125870 = CARTESIAN_POINT ( 'NONE',  ( -4.118644803501354978, 8.027112380718707030, 0.7998128361456352531 ) ) ;
#125872 = CARTESIAN_POINT ( 'NONE',  ( 5.357406976055401948, 6.279338222599979424, 1.199719254218452935 ) ) ;
#125873 = DIRECTION ( 'NONE',  ( 0.000000000000000000, 0.000000000000000000, 1.000000000000000000 ) ) ;
#125874 = CARTESIAN_POINT ( 'NONE',  ( 8.401248741962376698, 12.95320729893149370, 0.7998128361456462443 ) ) ;
#125875 = CARTESIAN_POINT ( 'NONE',  ( -3.906720819032141190, 7.709591388846142479, -0.7998128361456281477 ) ) ;
#125876 = CARTESIAN_POINT ( 'NONE',  ( -6.934069218746458318, 7.054445274817795486, -0.7998128361456362523 ) ) ;
#125877 = CARTESIAN_POINT ( 'NONE',  ( 2.665787806004877414, 1.174844384069907655, 1.849873475113596566 ) ) ;
#125878 = CARTESIAN_POINT ( 'NONE',  ( 2.846849069189655967, 5.304779099821139710, -1.082531754730543083 ) ) ;
#125879 = CARTESIAN_POINT ( 'NONE',  ( 10.99970480893081692, -6.134628647623513231, 0.08058608058608254798 ) ) ;
#125880 = DIRECTION ( 'NONE',  ( 0.000000000000000000, 0.000000000000000000, 1.000000000000000000 ) ) ;
#125881 = CARTESIAN_POINT ( 'NONE',  ( 2.402731849113007190, 1.466575434288765800, -1.087121784572639527 ) ) ;
#125882 = FACE_OUTER_BOUND ( 'NONE', #1732, .T. ) ;
#125883 = CARTESIAN_POINT ( 'NONE',  ( -4.711622075948912247, 5.455646162483875017, -1.199719254218446718 ) ) ;
#125884 =( BOUNDED_SURFACE ( )  B_SPLINE_SURFACE ( 3, 2, ( 
 ( #170666, #138188, #154429 ),
 ( #75307, #8163, #88363 ),
 ( #72077, #6007, #156568 ),
 ( #4929, #125206, #7074 ) ),
 .UNSPECIFIED., .F., .F., .T. ) 
 B_SPLINE_SURFACE_WITH_KNOTS ( ( 4, 4 ),
 ( 3, 3 ),
 ( 4.082329036714114956, 4.712388980384689674 ),
 ( 0.000000000000000000, 1.000000000000000000 ),
 .UNSPECIFIED. ) 
 GEOMETRIC_REPRESENTATION_ITEM ( )  RATIONAL_B_SPLINE_SURFACE ( (
 ( 1.000000000000000000, 0.8226529996940167289, 1.000000000000000000),
 ( 1.000000000000000000, 0.7917671131328077871, 1.000000000000000000),
 ( 1.000000000000000000, 0.7517196685946685442, 1.000000000000000000),
 ( 1.000000000000000000, 0.7071067811865475727, 1.000000000000000000) ) ) 
 REPRESENTATION_ITEM ( '' )  SURFACE ( )  );
#125885 = CARTESIAN_POINT ( 'NONE',  ( -5.393601776927423153, 7.665310133586674901, -1.338224700579364379 ) ) ;
#125886 = CARTESIAN_POINT ( 'NONE',  ( -0.02968770228140015649, 0.7448490463385791793, -1.910291535987144629 ) ) ;
#125887 = CARTESIAN_POINT ( 'NONE',  ( 9.738834413317897898, 10.25639499182604730, 0.000000000000000000 ) ) ;
#125888 = CARTESIAN_POINT ( 'NONE',  ( 1.189925737956001095, -0.8670580458889056708, 1.720419655784347412 ) ) ;
#125889 = CARTESIAN_POINT ( 'NONE',  ( 5.664887785843471413, 1.487927489739076181, -1.278645765186999128 ) ) ;
#125890 = CARTESIAN_POINT ( 'NONE',  ( -1.500000000000008216, 15.00000000000000000, 3.469446951953614189E-15 ) ) ;
#125891 = CARTESIAN_POINT ( 'NONE',  ( -7.714753101375940503, 8.959299025482085455, 1.199719254218462483 ) ) ;
#125892 = CARTESIAN_POINT ( 'NONE',  ( 3.988069740714122791, 7.804498464141805592, 0.7998128361456321445 ) ) ;
#125893 = CARTESIAN_POINT ( 'NONE',  ( 5.302338810847701644, 1.659911028786088538, -1.431018553749352051 ) ) ;
#125894 = AXIS2_PLACEMENT_3D ( 'NONE', #8053, #74142, #155382 ) ;
#125895 = CARTESIAN_POINT ( 'NONE',  ( 4.334856428067314305, 6.080418470877079429, -1.599625672291256517 ) ) ;
#125896 = CARTESIAN_POINT ( 'NONE',  ( 4.223533608758993196, 0.2584441732129874603, -2.054024224480345939 ) ) ;
#125898 = CARTESIAN_POINT ( 'NONE',  ( -1.364683531250000748, 2.321875000341422357, 1.214306433183764966E-14 ) ) ;
#125897 = CARTESIAN_POINT ( 'NONE',  ( 8.767237390769398786, 13.41519500316246116, 8.126379486628986015 ) ) ;
#125900 = ORIENTED_EDGE ( 'NONE', *, *, #135617, .T. ) ;
#125899 = AXIS2_PLACEMENT_3D ( 'NONE', #86971, #51278, #153041 ) ;
#125901 = CARTESIAN_POINT ( 'NONE',  ( 3.850415763719742479, 0.2810032917593773272, -2.281380581095279858 ) ) ;
#125902 = CARTESIAN_POINT ( 'NONE',  ( 7.456621297836078632, 8.762108271306003004, 1.082531754730558626 ) ) ;
#125904 = LINE ( 'NONE', #8856, #139592 ) ;
#125903 = CARTESIAN_POINT ( 'NONE',  ( 5.072158865288233009, 7.010880990960010273, 1.443375672974065660 ) ) ;
#125905 = CARTESIAN_POINT ( 'NONE',  ( 0.02392203315931124008, -1.416205114373503715, -1.803417470570017000 ) ) ;
#125906 = FACE_OUTER_BOUND ( 'NONE', #162259, .T. ) ;
#125907 = CARTESIAN_POINT ( 'NONE',  ( -6.129167961829681488, 9.308390501180058507, -1.199719254218452047 ) ) ;
#125908 = CARTESIAN_POINT ( 'NONE',  ( 5.261643664715593971, 0.9589319835984220219, 1.688605554185283575 ) ) ;
#125909 = ORIENTED_EDGE ( 'NONE', *, *, #60148, .F. ) ;
#125910 = CARTESIAN_POINT ( 'NONE',  ( 10.20892648096591770, 11.01276177065614981, -0.7216878364870257245 ) ) ;
#125911 = ORIENTED_EDGE ( 'NONE', *, *, #18226, .F. ) ;
#125912 = CARTESIAN_POINT ( 'NONE',  ( 5.607647405131535479, 1.452367144367059826, 1.244281684088064166 ) ) ;
#125913 = CARTESIAN_POINT ( 'NONE',  ( 6.018504615762162224, 1.154743246034171555, -1.281328459571188239 ) ) ;
#125914 = CARTESIAN_POINT ( 'NONE',  ( 4.540250091716044878, 0.7762272601403925609, 1.861345588084816871 ) ) ;
#125916 = FACE_OUTER_BOUND ( 'NONE', #72246, .T. ) ;
#125915 = CARTESIAN_POINT ( 'NONE',  ( -10.15235809853472126, 10.73883929124566983, -0.7998128361456291469 ) ) ;
#125917 = CARTESIAN_POINT ( 'NONE',  ( -1.642778471875000035, -3.405208332855375275, -2.845375778867859751 ) ) ;
#125919 = CARTESIAN_POINT ( 'NONE',  ( 0.3734444151584931926, 1.013553851667288841, 1.450680648178425125 ) ) ;
#125918 = CARTESIAN_POINT ( 'NONE',  ( 1.394599547902091174, 1.708230453586807585, -1.204993862942314031 ) ) ;
#125920 = CARTESIAN_POINT ( 'NONE',  ( 5.309220276109914316, 1.198862193007979471, -1.621181151826488254 ) ) ;
#125922 = CARTESIAN_POINT ( 'NONE',  ( 3.504133162399528434, -0.9285911969159079682, -2.095928835653658062 ) ) ;
#125921 = CARTESIAN_POINT ( 'NONE',  ( 4.441177836928239309, 7.339068688795062911, 1.199719254218452047 ) ) ;
#125923 = B_SPLINE_CURVE_WITH_KNOTS ( 'NONE', 3,
 ( #114972, #19525, #70390, #48858, #20586, #164726, #200399, #49914, #184161, #86672, #151689, #85601, #18460, #197218, #3259, #117101, #119236, #199334 ),
 .UNSPECIFIED., .F., .F.,
 ( 4, 2, 2, 2, 2, 2, 2, 2, 4 ),
 ( 0.000000000000000000, 0.0002050783776814487280, 0.0004101567553628974560, 0.0006152351330443461570, 0.0008203135107257949121, 0.001025391888407243667, 0.001230470266088692314, 0.001435548643770141177, 0.001640627021451589824 ),
 .UNSPECIFIED. ) ;
#125924 = CARTESIAN_POINT ( 'NONE',  ( 2.132362993881876889, -1.555188906917738700, 0.7812613976432846163 ) ) ;
#125925 = CARTESIAN_POINT ( 'NONE',  ( 2.883181758455736432, -1.960942133159260692, -0.8077274430827171559 ) ) ;
#125926 = CARTESIAN_POINT ( 'NONE',  ( 2.495074604456462009, 1.680611355344446389, 0.4256512511701947554 ) ) ;
#125927 = CARTESIAN_POINT ( 'NONE',  ( -0.6801582343750265380, 1.463541667008072533, 1.178068619123799898 ) ) ;
#125928 = CARTESIAN_POINT ( 'NONE',  ( 1.609564491371988426, 0.5446964562696824386, -1.779540750359181800 ) ) ;
#125929 = CARTESIAN_POINT ( 'NONE',  ( 2.471331864234734610, 1.938535094165691142, 0.9779774689679074928 ) ) ;
#125930 = CARTESIAN_POINT ( 'NONE',  ( 3.467982673848205355, -0.9896861206786079501, 1.756853968756578066 ) ) ;
#125931 = CARTESIAN_POINT ( 'NONE',  ( 5.031250000000002665, -0.7852924748302606561, -1.895863743163967108 ) ) ;
#125932 = CARTESIAN_POINT ( 'NONE',  ( 1.499999999999989120, 2.035416667349480679, 0.8660254037844524744 ) ) ;
#125933 = CARTESIAN_POINT ( 'NONE',  ( 0.3758376374219556393, 1.106279473776916378, 1.576890456013874120 ) ) ;
#125934 = CARTESIAN_POINT ( 'NONE',  ( -1.364683531250014514, 14.33854166700806232, -0.7879004041258335089 ) ) ;
#125935 = CARTESIAN_POINT ( 'NONE',  ( 3.937882119624159127, -2.125045857649208614, 0.6470787896058221023 ) ) ;
#125936 = EDGE_LOOP ( 'NONE', ( #16675, #45810, #124771, #23859, #102381, #142215, #19286, #129191 ) ) ;
#125937 = CARTESIAN_POINT ( 'NONE',  ( -0.2110808730066962846, 2.887681559854797797, -2.286017728802595350 ) ) ;
#125938 = CARTESIAN_POINT ( 'NONE',  ( -1.402160292154681736E-14, 0.8375000000000232259, -1.732050807568863648 ) ) ;
#125939 = CARTESIAN_POINT ( 'NONE',  ( 9.077347539549325717, 10.54899253668443393, -1.199719254218446718 ) ) ;
#125940 = CARTESIAN_POINT ( 'NONE',  ( -0.6823417656250246877, -0.9489583329919115684, 1.181850606188755259 ) ) ;
#125941 = CARTESIAN_POINT ( 'NONE',  ( 6.012022869640524014, -0.7491050530544652863, 2.091446645375413027 ) ) ;
#125943 = EDGE_CURVE ( 'NONE', #22427, #108500, #43716, .T. ) ;
#125942 = CARTESIAN_POINT ( 'NONE',  ( 4.264078424595136418, -1.956757550135434620, 0.1421211968542570592 ) ) ;
#125944 = PRODUCT_RELATED_PRODUCT_CATEGORY ( 'part', '', ( #121435 ) ) ;
#125946 = CARTESIAN_POINT ( 'NONE',  ( -5.910991785878170646, 7.919243054989755670, -1.443375672974059665 ) ) ;
#125945 = CARTESIAN_POINT ( 'NONE',  ( 3.602716132929354664, 5.226254793216122074, 1.599625672291267398 ) ) ;
#125947 = CARTESIAN_POINT ( 'NONE',  ( 0.000000000000000000, 13.49999999999999822, -1.500000000000000222 ) ) ;
#125948 = CARTESIAN_POINT ( 'NONE',  ( 6.116559975520791781, 1.526041019664432508, -1.670398689176689544 ) ) ;
#125949 = CARTESIAN_POINT ( 'NONE',  ( 2.699736158553706300, -1.526808845971421968, -1.387057796406083732 ) ) ;
#125950 = CARTESIAN_POINT ( 'NONE',  ( -5.555090253297260361, 7.504024600312024340, 1.599625672291269396 ) ) ;
#125951 = EDGE_LOOP ( 'NONE', ( #193965, #156078 ) ) ;
#125952 = CARTESIAN_POINT ( 'NONE',  ( -1.499999999999997780, 2.431250000682817713, 1.214306433183764966E-14 ) ) ;
#125953 = CARTESIAN_POINT ( 'NONE',  ( 4.024554299415397551, 1.775361691451295520, 0.5892213400080713592 ) ) ;
#125954 = CARTESIAN_POINT ( 'NONE',  ( 3.006226939181593227, -1.670314528538990873, 0.4657782236400943021 ) ) ;
#125955 = CARTESIAN_POINT ( 'NONE',  ( 6.480031355044912900, -2.148842909532014289, -0.4297212958329286736 ) ) ;
#125956 = CARTESIAN_POINT ( 'NONE',  ( 1.114635189304619356, -0.9934212416997322270, -1.970578525975318573 ) ) ;
#125957 = CARTESIAN_POINT ( 'NONE',  ( 6.158146451363091245, -1.371594178524730534, 1.374984930127883143 ) ) ;
#125959 = ORIENTED_EDGE ( 'NONE', *, *, #195251, .T. ) ;
#125958 = CARTESIAN_POINT ( 'NONE',  ( 9.338271064545565991, 13.87258202181963362, 7.537100060026529214 ) ) ;
#125960 = CARTESIAN_POINT ( 'NONE',  ( -0.05211191391743182078, -1.802403943428915412, -0.9041556775107384425 ) ) ;
#125962 = EDGE_CURVE ( 'NONE', #21587, #28791, #73757, .T. ) ;
#125961 = SURFACE_STYLE_USAGE ( .BOTH. , #157324 ) ;
#125963 = CARTESIAN_POINT ( 'NONE',  ( 6.381482430641396419, -0.5404875331735843336, -1.942542459342583294 ) ) ;
#125964 = CARTESIAN_POINT ( 'NONE',  ( -10.01677656239806247, 10.58066083241955901, 0.7998128361456462443 ) ) ;
#125965 = CARTESIAN_POINT ( 'NONE',  ( 5.770966940911189447, 9.884545197705074671, -0.7998128361456291469 ) ) ;
#125966 = CARTESIAN_POINT ( 'NONE',  ( 2.674941732306341358, -0.4431148209949172800, -0.1136209127918897804 ) ) ;
#125967 = CARTESIAN_POINT ( 'NONE',  ( 4.195794211080963620, -0.6966935528937777677, 1.687730213881050600 ) ) ;
#125968 = CARTESIAN_POINT ( 'NONE',  ( 2.169229845753062325, -2.017539712319418310, -0.8944986170207609444 ) ) ;
#125969 = ORIENTED_EDGE ( 'NONE', *, *, #203174, .T. ) ;
#125970 = CARTESIAN_POINT ( 'NONE',  ( -5.908321080505254841, 10.11506803722328129, 0.7998128361456291469 ) ) ;
#125971 = CARTESIAN_POINT ( 'NONE',  ( -3.285556943750000514, -1.976041666188710577, -1.896917185911906500 ) ) ;
#125972 = CARTESIAN_POINT ( 'NONE',  ( -7.344766530301162000, 9.591980256816594164, 1.599625672291295375 ) ) ;
#125973 = CARTESIAN_POINT ( 'NONE',  ( 1.388932113579334660, -1.919223592974130588, -0.6296790815572687050 ) ) ;
#125974 = CARTESIAN_POINT ( 'NONE',  ( -2.081668171172168513E-14, 6.468705557303652931, 4.925226524755076163 ) ) ;
#125975 = CARTESIAN_POINT ( 'NONE',  ( -4.960304097753355457, 6.880383762169266504, 1.599625672291263179 ) ) ;
#125976 = CARTESIAN_POINT ( 'NONE',  ( 2.430303444995636664, -1.149418499707482999, 1.463420418157684422 ) ) ;
#125977 = CARTESIAN_POINT ( 'NONE',  ( 2.517010073631369860, 6.088262185878572375, -0.7998128361456281477 ) ) ;
#125978 = CARTESIAN_POINT ( 'NONE',  ( 5.818982467333652764, 0.9914020171761170896, -1.755767668913270407 ) ) ;
#125979 = ORIENTED_EDGE ( 'NONE', *, *, #20075, .T. ) ;
#125980 = CARTESIAN_POINT ( 'NONE',  ( -8.483651433849100698, 10.92067931095586886, 1.599625672291269396 ) ) ;
#125981 = CARTESIAN_POINT ( 'NONE',  ( 3.844227010333609584, 1.817057058749595777, 0.1772887374331885701 ) ) ;
#125984 = ORIENTED_EDGE ( 'NONE', *, *, #17814, .T. ) ;
#125983 = CARTESIAN_POINT ( 'NONE',  ( -4.957984823605727343, 6.829280066411827832, -1.450623857674667283 ) ) ;
#125982 = CARTESIAN_POINT ( 'NONE',  ( -3.630551273409382329, 7.457669928944732796, 0.7998128361456352531 ) ) ;
#125985 = CARTESIAN_POINT ( 'NONE',  ( 5.586791213849657822, 7.504901977030062454, -1.335864709735144817 ) ) ;
#125986 = CARTESIAN_POINT ( 'NONE',  ( 6.345077344222471716, -1.080897578067066878, 1.701688803805063266 ) ) ;
#125987 = CARTESIAN_POINT ( 'NONE',  ( 5.578019757025042047, -1.797138167560994759, -0.3993771437491022702 ) ) ;
#125988 = CARTESIAN_POINT ( 'NONE',  ( 4.512551404143492206, -0.9841529367882025925, -2.087457756972084244 ) ) ;
#125989 = CARTESIAN_POINT ( 'NONE',  ( 6.378184920586140727, 6.405913593630768510, 0.000000000000000000 ) ) ;
#125990 = CARTESIAN_POINT ( 'NONE',  ( 0.5970370245043071789, 1.714778692204623312, -1.142632759096851913 ) ) ;
#125991 = CARTESIAN_POINT ( 'NONE',  ( 1.909617033088998328, -0.9174269660217245770, -1.711723090954318405 ) ) ;
#125992 = CARTESIAN_POINT ( 'NONE',  ( 5.852921341749488526, -1.041456137194999521, 2.048983711149698461 ) ) ;
#125993 = CARTESIAN_POINT ( 'NONE',  ( -0.07602376731355095507, -7.154544010627095219, 9.579698345292692707 ) ) ;
#125994 = CARTESIAN_POINT ( 'NONE',  ( -4.462568837553487100, 5.235360394347691404, -1.199719254218453823 ) ) ;
#125995 = CARTESIAN_POINT ( 'NONE',  ( 4.135518821028766112, -1.289757458839156934, -1.355179912160727085 ) ) ;
#125996 = VERTEX_POINT ( 'NONE', #22846 ) ;
#125999 = CARTESIAN_POINT ( 'NONE',  ( -5.309953438407606363, 6.223975762010839574, 1.199719254218452935 ) ) ;
#125998 = CARTESIAN_POINT ( 'NONE',  ( -1.500000000000013101, 0.9520833340161557468, 0.8660254037844403729 ) ) ;
#125997 = CARTESIAN_POINT ( 'NONE',  ( 2.425908952446104827, -1.891012092455180760, 0.2844710172774585488 ) ) ;
#126000 = CARTESIAN_POINT ( 'NONE',  ( 3.950008152305323428, 0.7444041667201054535, -2.077678867657362538 ) ) ;
#126001 = CARTESIAN_POINT ( 'NONE',  ( -3.555477883677943599E-14, 6.828200129012236763E-10, -1.414508159514579644 ) ) ;
#126002 = CARTESIAN_POINT ( 'NONE',  ( 6.883263157960371359, 7.052674735402435502, 2.544342468817725855 ) ) ;
#126003 = CARTESIAN_POINT ( 'NONE',  ( 4.028181036591620412, 7.713645286083276709, -0.7216878364870338292 ) ) ;
#126004 = CARTESIAN_POINT ( 'NONE',  ( -4.611181641979265500, 8.393812659035525314, 0.000000000000000000 ) ) ;
#126005 = CARTESIAN_POINT ( 'NONE',  ( 1.950399328871486704, 0.6145138020485548802, 1.873222726689319106 ) ) ;
#126006 = CARTESIAN_POINT ( 'NONE',  ( 2.257223126251302947, -1.783628160338263768, 1.464130300071916135 ) ) ;
#126007 = CARTESIAN_POINT ( 'NONE',  ( 2.945700582358207864, 1.385421296276163838, 1.389331660621349274 ) ) ;
#126008 = CARTESIAN_POINT ( 'NONE',  ( 11.44779965693276225, 10.99686076798702317, 3.599999932275867121 ) ) ;
#126009 = CARTESIAN_POINT ( 'NONE',  ( 6.069198595068595381, 1.816300881853601723, 0.9774375683993684616 ) ) ;
#126010 = CARTESIAN_POINT ( 'NONE',  ( 3.172244755917638770, 5.684407401003788607, -1.082531754730543083 ) ) ;
#126011 = CARTESIAN_POINT ( 'NONE',  ( 3.977750132953357998, -0.7672935630990398437, 1.865046046545227654 ) ) ;
#126012 = CARTESIAN_POINT ( 'NONE',  ( 5.388439706788500594, 5.251210844200210559, 0.7998128361456352531 ) ) ;
#126013 = ORIENTED_EDGE ( 'NONE', *, *, #30361, .F. ) ;
#126014 = CARTESIAN_POINT ( 'NONE',  ( 4.206267736153862735, 1.236801365491456028, -1.592660703826812352 ) ) ;
#126015 = CARTESIAN_POINT ( 'NONE',  ( -9.110189153378817295, 12.71597221466224603, 1.199719254218462483 ) ) ;
#126016 = CARTESIAN_POINT ( 'NONE',  ( -4.489157070319179432, 8.251450656689856444, 5.811111664500048210E-05 ) ) ;
#126017 = DIRECTION ( 'NONE',  ( -1.000000000000000000, 0.000000000000000000, 4.440892098500751393E-16 ) ) ;
#126018 = CARTESIAN_POINT ( 'NONE',  ( 10.23370702021670020, 10.83374636654133383, 0.7998128361456462443 ) ) ;
#126019 = CARTESIAN_POINT ( 'NONE',  ( 2.290094988384860919, -1.415387839477784571, -1.646397135256922661 ) ) ;
#126020 = CARTESIAN_POINT ( 'NONE',  ( 6.201928923608456046, 6.200281597156833691, 0.7998128361456350310 ) ) ;
#126021 = CARTESIAN_POINT ( 'NONE',  ( 2.846779338809723559, -1.557328454271855955, 1.035869100625155692 ) ) ;
#126022 = CARTESIAN_POINT ( 'NONE',  ( 0.2454759580562664856, -1.591291808662575580, -1.309149871672641297 ) ) ;
#126024 = CARTESIAN_POINT ( 'NONE',  ( 6.727182134110200273, 2.469373133786161745, 2.195552656936059055 ) ) ;
#126023 = CARTESIAN_POINT ( 'NONE',  ( 0.000000000000000000, 15.00000000000000000, 0.000000000000000000 ) ) ;
#126025 = CARTESIAN_POINT ( 'NONE',  ( -1.201851678989727383E-14, 0.8218750003414171390, 1.575800808251672791 ) ) ;
#126026 = DIRECTION ( 'NONE',  ( 2.078337502098293044E-13, 0.000000000000000000, -1.000000000000000000 ) ) ;
#126027 = CARTESIAN_POINT ( 'NONE',  ( 3.932203299393256302, -0.9856607118853939475, -1.638553295466014026 ) ) ;
#126028 = CARTESIAN_POINT ( 'NONE',  ( 3.731107905939319735, -1.635417248454105854, 0.6770700851450436319 ) ) ;
#126029 = CARTESIAN_POINT ( 'NONE',  ( 2.227084300891319035, 1.708885092217244051, 0.8583199515034345417 ) ) ;
#126030 = CARTESIAN_POINT ( 'NONE',  ( -3.567766978690493307, 7.314145241780881435, 1.040834085586084257E-14 ) ) ;
#126032 = CARTESIAN_POINT ( 'NONE',  ( -0.1357414145864926924, -1.858833624763186032, -0.4630600859806994762 ) ) ;
#126031 = CARTESIAN_POINT ( 'NONE',  ( -2.817581654649482292, 6.509205373724840982, -0.4305581727225830102 ) ) ;
#126033 = CARTESIAN_POINT ( 'NONE',  ( 0.7499999999999867883, -0.4333333333333133641, -1.299038105676652899 ) ) ;
#126034 = CARTESIAN_POINT ( 'NONE',  ( 0.9243811426856913815, 1.018911950503737174, 1.802186752163869699 ) ) ;
#126035 = CARTESIAN_POINT ( 'NONE',  ( -1.500000000000011324, 5.420833333333356485, 0.8660254037844403729 ) ) ;
#126036 = CARTESIAN_POINT ( 'NONE',  ( 6.139502064137229986, -1.356240498024411600, -1.288626068300227523 ) ) ;
#126037 = CARTESIAN_POINT ( 'NONE',  ( 1.224926655537651676, -0.04696546880481740349, 1.825250005322680780 ) ) ;
#126039 = CARTESIAN_POINT ( 'NONE',  ( 4.789099507923308963, 8.141322699134850183, 0.8117711051834965996 ) ) ;
#126038 = CARTESIAN_POINT ( 'NONE',  ( 6.147136880733683917, -1.866598994669689926, 1.177069016086537356 ) ) ;
#126040 = CARTESIAN_POINT ( 'NONE',  ( -1.364683531250014514, -0.7197916663252461600, 0.7879004041258379498 ) ) ;
#126041 = CARTESIAN_POINT ( 'NONE',  ( 3.473143217414649708, 1.863520296645693186, 0.8845801619412340111 ) ) ;
#126043 = CARTESIAN_POINT ( 'NONE',  ( -6.744291347794091784, 9.955758108146730123, -1.199719254218440723 ) ) ;
#126042 = AXIS2_PLACEMENT_3D ( 'NONE', #68277, #100796, #186306 ) ;
#126044 = CARTESIAN_POINT ( 'NONE',  ( -1.224999999999741851, 0.02083333333336212859, 0.7072540797574373705 ) ) ;
#126045 = CARTESIAN_POINT ( 'NONE',  ( 8.809047120577066181, 11.30030761213851953, 1.599625672291281386 ) ) ;
#126046 = CARTESIAN_POINT ( 'NONE',  ( 1.493932498646918683, 3.368187994538051733, -0.1507059531854390566 ) ) ;
#126047 = DIRECTION ( 'NONE',  ( -0.7366372490351829061, 1.218064704987765655E-12, 0.6762880771785629852 ) ) ;
#126048 = CARTESIAN_POINT ( 'NONE',  ( 7.015418140428412386, 7.149352350113456822, 0.7998128361456331437 ) ) ;
#126049 = EDGE_CURVE ( 'NONE', #176746, #23806, #85265, .T. ) ;
#126050 = ORIENTED_EDGE ( 'NONE', *, *, #36008, .F. ) ;
#126051 = CARTESIAN_POINT ( 'NONE',  ( 5.846161131210033446, -0.9342735719010831774, 1.847668428805064655 ) ) ;
#126053 = CARTESIAN_POINT ( 'NONE',  ( -0.6823417656250246877, -0.1364583329919108468, 1.181850606188755259 ) ) ;
#126052 = AXIS2_PLACEMENT_3D ( 'NONE', #6058, #135042, #183763 ) ;
#126054 = CARTESIAN_POINT ( 'NONE',  ( 3.163507678178357541, 0.3205598832158839118, -2.137589075770351066 ) ) ;
#126055 = CARTESIAN_POINT ( 'NONE',  ( -4.683575932806860465, 8.284415941318199472, -0.5487617172068790516 ) ) ;
#126056 = CARTESIAN_POINT ( 'NONE',  ( 2.789718171214683462, 1.917044005781431748, -0.6357942740662542169 ) ) ;
#126057 = CARTESIAN_POINT ( 'NONE',  ( 7.724608556409205740, -5.759585062615360407, 7.735357998705606697 ) ) ;
#126060 = CARTESIAN_POINT ( 'NONE',  ( 7.470179451449751262, 7.817556902887268677, 1.040834085586084257E-14 ) ) ;
#126059 = CARTESIAN_POINT ( 'NONE',  ( -3.475000000000000533, -0.7291666666666675178, -2.006292185433948827 ) ) ;
#126058 = FILL_AREA_STYLE_COLOUR ( '', #93998 ) ;
#126061 = CARTESIAN_POINT ( 'NONE',  ( -5.271087860662956537, 9.371629280740593870, 0.000000000000000000 ) ) ;
#126062 = CARTESIAN_POINT ( 'NONE',  ( 1.762908039156896978, -0.1037823317905466058, -2.014007988105172231 ) ) ;
#126064 = CARTESIAN_POINT ( 'NONE',  ( 5.618738332679400038, -0.05485954975367920983, 2.191026952110195491 ) ) ;
#126063 = CARTESIAN_POINT ( 'NONE',  ( -4.741601036477307574, 6.554953847355395880, 1.599625672291267398 ) ) ;
#126065 =( BOUNDED_CURVE ( )  B_SPLINE_CURVE ( 3, ( #67197, #17386, #152743, #4324 ),
 .UNSPECIFIED., .F., .T. ) 
 B_SPLINE_CURVE_WITH_KNOTS ( ( 4, 4 ),
 ( 0.5000000000000017764, 1.000000000000000000 ),
 .UNSPECIFIED. ) 
 CURVE ( )  GEOMETRIC_REPRESENTATION_ITEM ( )  RATIONAL_B_SPLINE_CURVE ( ( 0.9999999999999976685, 0.3333333333333333703, 0.3333333333333357573, 1.000000000000000000 ) ) 
 REPRESENTATION_ITEM ( '' )  );
#126066 = CARTESIAN_POINT ( 'NONE',  ( -0.3999999999999993006, 3.949999999999967315, 0.4999999999999674705 ) ) ;
#126067 = CARTESIAN_POINT ( 'NONE',  ( 4.675980034926481288, 1.890745994642643479, -0.2862527531290667837 ) ) ;
#126068 = DIRECTION ( 'NONE',  ( 0.6507913734559640506, -0.7592566023653003482, 0.000000000000000000 ) ) ;
#126069 = EDGE_CURVE ( 'NONE', #156791, #193127, #23934, .T. ) ;
#126070 = CARTESIAN_POINT ( 'NONE',  ( 5.951666246274807115, 6.045958163516475636, 0.7216878364870317197 ) ) ;
#126072 = CARTESIAN_POINT ( 'NONE',  ( 3.251577527157409886, 1.966640965408305686, -0.4445242805125593222 ) ) ;
#126071 = CARTESIAN_POINT ( 'NONE',  ( -9.625925875578284163, 10.33259439770390564, 1.040834085586084257E-14 ) ) ;
#126073 = CARTESIAN_POINT ( 'NONE',  ( 1.364683531249996529, 13.27604166700806410, 0.7879004041258405033 ) ) ;
#126074 = CARTESIAN_POINT ( 'NONE',  ( 5.807552366672524613, -0.4147409827905921831, 1.674012740457442305 ) ) ;
#126075 = CARTESIAN_POINT ( 'NONE',  ( 5.352436782344940802, 9.466536356036257871, 0.000000000000000000 ) ) ;
#126076 = CARTESIAN_POINT ( 'NONE',  ( 8.703971430293332645, 12.13808852110884118, -1.082531754730543083 ) ) ;
#126077 = CARTESIAN_POINT ( 'NONE',  ( -0.3000000002818530298, 3.198312376128904067, 0.5146719259195894347 ) ) ;
#126078 = CARTESIAN_POINT ( 'NONE',  ( 4.059713336928523653, 1.856696190431494475, -0.2264497139414511362 ) ) ;
#126079 = DIRECTION ( 'NONE',  ( -0.6507913734559641616, -0.7592566023653004592, 0.000000000000000000 ) ) ;
#126080 = CARTESIAN_POINT ( 'NONE',  ( 1.463825199929311260, -0.5068179562870354093, 2.007114080642191656 ) ) ;
#126081 = CARTESIAN_POINT ( 'NONE',  ( 0.2442642247113699094, -5.209160580580716626, 10.99754090108938342 ) ) ;
#126082 = VERTEX_POINT ( 'NONE', #138776 ) ;
#126083 = CARTESIAN_POINT ( 'NONE',  ( 6.111934181110398434, -0.6035781192351510338, 1.708109960999981469 ) ) ;
#126084 = CARTESIAN_POINT ( 'NONE',  ( 4.716257332707354699, 6.595662536282280719, -1.599625672291269396 ) ) ;
#126085 = CARTESIAN_POINT ( 'NONE',  ( -0.1234324464992678227, -0.4448297287729073846, -1.973926538189611835 ) ) ;
#126086 = CARTESIAN_POINT ( 'NONE',  ( 0.5624193892179689680, 0.5266301872345402479, 1.733300928327138113 ) ) ;
#126087 = CARTESIAN_POINT ( 'NONE',  ( 5.899206235277530297, 7.015400374979486209, -1.082531754730548412 ) ) ;
#126088 = CARTESIAN_POINT ( 'NONE',  ( 11.28392429091624649, 8.882752594160487902, 4.087434772561983287 ) ) ;
#126089 = ORIENTED_EDGE ( 'NONE', *, *, #180308, .F. ) ;
#126090 = CARTESIAN_POINT ( 'NONE',  ( 8.229436053370667636, 11.58446391469906267, 1.082531754730558626 ) ) ;
#126092 = CARTESIAN_POINT ( 'NONE',  ( 8.046927864910717432, 9.346836249606042202, 1.199719254218462483 ) ) ;
#126091 = CARTESIAN_POINT ( 'NONE',  ( 0.8362905744919849615, -1.092891352686057527, 1.629061181365853539 ) ) ;
#126093 = CARTESIAN_POINT ( 'NONE',  ( 4.534732036847580083, -1.536008458380673458, 1.144414559590371638 ) ) ;
#126094 = DIRECTION ( 'NONE',  ( 0.000000000000000000, -1.000000000000000000, 0.000000000000000000 ) ) ;
#126095 = CARTESIAN_POINT ( 'NONE',  ( -6.490830876026181251, 6.764709549658621590, 0.1777360701797660314 ) ) ;
#126096 = EDGE_CURVE ( 'NONE', #162715, #213175, #207312, .T. ) ;
#126097 = AXIS2_PLACEMENT_3D ( 'NONE', #135263, #203407, #71276 ) ;
#126098 = CARTESIAN_POINT ( 'NONE',  ( -1.387358672534890536, 7.315968950354793776, -4.254625267136668221 ) ) ;
#126100 = ORIENTED_EDGE ( 'NONE', *, *, #27925, .T. ) ;
#126099 = CARTESIAN_POINT ( 'NONE',  ( 3.362058906508953449, 6.866226457661676719, -0.7216878364870267237 ) ) ;
#126101 = CARTESIAN_POINT ( 'NONE',  ( -7.809133291791416909, 11.09411069285655493, 1.082531754730549967 ) ) ;
#126102 = CARTESIAN_POINT ( 'NONE',  ( 1.815512348505427642, -0.2646426633909418347, 2.145385951886819242 ) ) ;
#126103 = CARTESIAN_POINT ( 'NONE',  ( -5.171509248969888617, 4.998125310078441075, 0.7998128361456281477 ) ) ;
#126104 = CARTESIAN_POINT ( 'NONE',  ( 7.539742822975472158, 7.968990512992423447, -0.7216878364870317197 ) ) ;
#126105 = CARTESIAN_POINT ( 'NONE',  ( -0.1049925189658337810, -2.058569791948822392, -0.5088776734372552069 ) ) ;
#126106 = CARTESIAN_POINT ( 'NONE',  ( 4.260648785556298890, -1.352668379831567069, 1.226179085325199258 ) ) ;
#126107 = CARTESIAN_POINT ( 'NONE',  ( 8.368688605668825886, 13.06099974637745298, -8.528945119623642768 ) ) ;
#126108 = CARTESIAN_POINT ( 'NONE',  ( 0.9484320465981105341, 0.5679970104440315026, 1.887783002132171539 ) ) ;
#126109 = CARTESIAN_POINT ( 'NONE',  ( 3.990413957267644474, -1.096855775730350757, 1.566394476586838724 ) ) ;
#126110 = ORIENTED_EDGE ( 'NONE', *, *, #187034, .F. ) ;
#126111 = CARTESIAN_POINT ( 'NONE',  ( 9.469892045836674654, -6.532648833121171172, -0.4294077647110511320 ) ) ;
#126112 = CARTESIAN_POINT ( 'NONE',  ( 4.176189586714727398, -1.010410353755032409, -1.690456409470885824 ) ) ;
#126113 = ORIENTED_EDGE ( 'NONE', *, *, #167075, .F. ) ;
#126114 = CARTESIAN_POINT ( 'NONE',  ( 5.530791563722144311, -1.753914071513791528, 0.8342105869050663314 ) ) ;
#126115 = VERTEX_POINT ( 'NONE', #123673 ) ;
#126116 = CARTESIAN_POINT ( 'NONE',  ( -5.749539660647037032, 8.865490816466966351, 1.199719254218454489 ) ) ;
#126118 = CARTESIAN_POINT ( 'NONE',  ( 6.117454236943913770, 1.763945953808215394, 1.176740244630887222 ) ) ;
#126117 = CARTESIAN_POINT ( 'NONE',  ( -5.984998465789844069, 5.947196063035064206, 0.7998128361456281477 ) ) ;
#126119 = CARTESIAN_POINT ( 'NONE',  ( 7.648208051440442468, 8.095533279534887328, 0.000000000000000000 ) ) ;
#126120 = CARTESIAN_POINT ( 'NONE',  ( 4.125576785117724299, -0.3237648511281773778, 1.884507068624697190 ) ) ;
#126121 = LINE ( 'NONE', #45879, #14810 ) ;
#126122 = CARTESIAN_POINT ( 'NONE',  ( 0.2005908178989434243, -2.206344910233990486, -0.05143828380192031619 ) ) ;
#126123 = CARTESIAN_POINT ( 'NONE',  ( 7.624693973552425952, -5.341768514962141445, 7.882977371602010841 ) ) ;
#126124 = CARTESIAN_POINT ( 'NONE',  ( 5.162748661275342599, 0.5863960615675645194, 1.925778112416365317 ) ) ;
#126125 = DIRECTION ( 'NONE',  ( 1.276756478318932585E-15, -1.000000000000000000, 1.665334536937738262E-16 ) ) ;
#126127 = CARTESIAN_POINT ( 'NONE',  ( 5.788296071918774821, -0.7303023681345042206, -1.879805717804765353 ) ) ;
#126126 = CARTESIAN_POINT ( 'NONE',  ( 5.690036971771410101, -0.8169618954828453683, 1.632782195682795257 ) ) ;
#126128 = CARTESIAN_POINT ( 'NONE',  ( 1.451716722110554025, 1.566445173006292935, 1.353826630019476562 ) ) ;
#126129 = CARTESIAN_POINT ( 'NONE',  ( -6.995644074971465010, 10.14503993989993091, 1.082531754730549967 ) ) ;
#126130 = CARTESIAN_POINT ( 'NONE',  ( -5.018153416333300143, 7.915986710968343054, -1.079799343345327234 ) ) ;
#126131 = CARTESIAN_POINT ( 'NONE',  ( -0.3282377607281391496, 2.011164550367436465, -1.225000000000030287 ) ) ;
#126132 = CARTESIAN_POINT ( 'NONE',  ( 0.000000000000000000, -2.996874999522043392, -3.793834371823813445 ) ) ;
#126133 = CARTESIAN_POINT ( 'NONE',  ( 5.717788096661236885, 7.693838750903348789, 1.599625672291267398 ) ) ;
#126134 = CARTESIAN_POINT ( 'NONE',  ( 5.614485009834906393, 6.683225611963085733, -1.082531754730548412 ) ) ;
#126135 = CARTESIAN_POINT ( 'NONE',  ( 2.191614386903386613, 5.708633884695917260, -0.7998128361456281477 ) ) ;
#126136 = CARTESIAN_POINT ( 'NONE',  ( -0.6823417656250003738, 11.46354166700806765, 1.181850606188754593 ) ) ;
#126137 = CARTESIAN_POINT ( 'NONE',  ( -5.271422797614987665, 5.044414773505913274, -0.7998128361456221525 ) ) ;
#126139 = CARTESIAN_POINT ( 'NONE',  ( -6.607619761813764647, 8.802252036906432764, 1.599625672291269396 ) ) ;
#126138 = CARTESIAN_POINT ( 'NONE',  ( 1.907519672996875082, 3.236073672982398008, -0.4612874649729831744 ) ) ;
#126140 = CARTESIAN_POINT ( 'NONE',  ( 3.709331991548686425, 1.648016779243220320, 0.5399856063554776542 ) ) ;
#126141 = CLOSED_SHELL ( 'NONE', ( #12150, #80575, #17406, #177874, #133711, #168316, #136448, #166027, #202760, #123786, #13658, #211476, #42407, #11168, #45691, #121111, #120415, #83806, #185742, #172089, #145525, #164115, #196170, #132795, #136347 ) ) ;
#126142 = CARTESIAN_POINT ( 'NONE',  ( -3.391510981712833939, 7.108513245306943062, 0.7998128361456341429 ) ) ;
#126143 = CARTESIAN_POINT ( 'NONE',  ( 2.166927730644189420, 1.536898783757352005, -1.387270004372019416 ) ) ;
#126144 = CARTESIAN_POINT ( 'NONE',  ( 3.603210856581297694, -0.1536155211374414797, 2.111693916904446855 ) ) ;
#126145 = CARTESIAN_POINT ( 'NONE',  ( 6.577677080924314801, 10.82570702772039262, 1.040834085586084257E-14 ) ) ;
#126146 = CARTESIAN_POINT ( 'NONE',  ( 0.09196683552161016850, -9.918146503183461249, 10.99961570984664583 ) ) ;
#126147 = CARTESIAN_POINT ( 'NONE',  ( 1.217558188649459527, 0.3894938459214473125, -1.930362121600463610 ) ) ;
#126148 = CARTESIAN_POINT ( 'NONE',  ( 5.936406840065503232, 6.128608848081334770, 0.7476236741628620175 ) ) ;
#126149 = CARTESIAN_POINT ( 'NONE',  ( 4.392478581147586603, 4.226905887534702977, -0.7216878364870188411 ) ) ;
#126151 = CARTESIAN_POINT ( 'NONE',  ( -1.734723475976807094E-15, 2.999999999999988898, -6.938893903907228378E-15 ) ) ;
#126150 = CARTESIAN_POINT ( 'NONE',  ( 1.737499999999999378, -1.866666666666665808, -3.009438278150925683 ) ) ;
#126152 = CARTESIAN_POINT ( 'NONE',  ( 3.486539624822242889, -0.4467316994782115636, -2.248153690150441975 ) ) ;
#126153 = CARTESIAN_POINT ( 'NONE',  ( 0.2404813148422607350, 0.3085585699703840001, 1.799268721412583094 ) ) ;
#126154 = CARTESIAN_POINT ( 'NONE',  ( 2.812653035604309348, -0.5591599321941118639, -1.828790038765286452 ) ) ;
#126155 = CARTESIAN_POINT ( 'NONE',  ( 5.397027666691686321, 8.454226823519094935, 1.199719254218451159 ) ) ;
#126156 = CARTESIAN_POINT ( 'NONE',  ( 7.090551149822739596, 8.335026431957096804, 1.082531754730558626 ) ) ;
#126157 = CARTESIAN_POINT ( 'NONE',  ( -8.995998617867369873, 10.45408546138876993, 1.199719254218462483 ) ) ;
#126158 = CARTESIAN_POINT ( 'NONE',  ( 2.267839937129061401, 0.5327387516648759425, -1.941401684534331817 ) ) ;
#126159 = CARTESIAN_POINT ( 'NONE',  ( 2.096468001391890823, 1.939661435718213811, 0.2929505381348077031 ) ) ;
#126160 = CARTESIAN_POINT ( 'NONE',  ( -9.318531651294266638, 9.766041769465124034, -0.7998128361456291469 ) ) ;
#126161 = CARTESIAN_POINT ( 'NONE',  ( -5.391338639728555648, 9.441645512991978961, -0.7998128361456231517 ) ) ;
#126162 = CARTESIAN_POINT ( 'NONE',  ( 0.07516593201273896740, 4.087024598281757015, -2.598925129725014660 ) ) ;
#126164 = CARTESIAN_POINT ( 'NONE',  ( 3.361912448646987794, 0.7947379027260987883, 1.581431320561203169 ) ) ;
#126163 = CARTESIAN_POINT ( 'NONE',  ( 5.279275078172800839, 1.403616728028998395, 1.549557787628618399 ) ) ;
#126165 = CARTESIAN_POINT ( 'NONE',  ( 1.000000047849772367, 16.00000000000000711, 11.64874984998672325 ) ) ;
#126166 = CARTESIAN_POINT ( 'NONE',  ( 6.615150229029130635, -2.225211831249251482, 0.5499996461680799476 ) ) ;
#126167 = CARTESIAN_POINT ( 'NONE',  ( 5.753775850233431299, 0.7111499035084413167, 1.588595604753391122 ) ) ;
#126168 = CARTESIAN_POINT ( 'NONE',  ( 8.776205506747620788, 9.133327934160710981, -0.7998128361456221525 ) ) ;
#126169 = CARTESIAN_POINT ( 'NONE',  ( 6.065094409921147900, -1.233312222785312384, 1.939673083280533783 ) ) ;
#126170 = DIRECTION ( 'NONE',  ( 1.000000000000000000, -0.000000000000000000, -0.000000000000000000 ) ) ;
#126171 = CARTESIAN_POINT ( 'NONE',  ( 5.255145817263100483, -1.720984288211702795, -0.2101651147246290929 ) ) ;
#126172 = CARTESIAN_POINT ( 'NONE',  ( 6.092256315220226703, 1.075607590566488803, -1.885974292122821527 ) ) ;
#126173 = CARTESIAN_POINT ( 'NONE',  ( -0.7500000000000179856, 11.29166666666666430, 1.299038105676658228 ) ) ;
#126174 = CARTESIAN_POINT ( 'NONE',  ( 6.438686429976131720, -1.555646628146038157, 1.282773817382940384 ) ) ;
#126175 = CARTESIAN_POINT ( 'NONE',  ( 5.187500000000002665, -1.451031289060905172, 1.451031289061322838 ) ) ;
#126176 = CARTESIAN_POINT ( 'NONE',  ( 1.499999999999991118, 5.535416667349481123, 0.8660254037844524744 ) ) ;
#126177 = CARTESIAN_POINT ( 'NONE',  ( 3.012629298554883484, 1.396463203792638996, -1.327218363718547511 ) ) ;
#126178 = CARTESIAN_POINT ( 'NONE',  ( -1.500000000000008216, 11.28125000068279427, 3.469446951953614189E-15 ) ) ;
#126179 = CARTESIAN_POINT ( 'NONE',  ( 0.2236696677372449760, 1.935810370009845460, 1.089285801332658732 ) ) ;
#126180 = ORIENTED_EDGE ( 'NONE', *, *, #179393, .F. ) ;
#126181 = CARTESIAN_POINT ( 'NONE',  ( -1.499999999999997780, 3.900000000000021672, 1.214306433183764966E-14 ) ) ;
#126182 = CARTESIAN_POINT ( 'NONE',  ( 6.257251587906815793, 7.258880593101466161, 1.199719254218462483 ) ) ;
#126183 = CARTESIAN_POINT ( 'NONE',  ( 5.795220594837462436, 8.848508896363995291, -1.199719254218440723 ) ) ;
#126184 = CARTESIAN_POINT ( 'NONE',  ( 2.350487294161308860, 1.044453463271700633, -1.960417310804033031 ) ) ;
#126186 = EDGE_CURVE ( 'NONE', #26009, #74902, #209980, .T. ) ;
#126185 =( NAMED_UNIT ( * ) PLANE_ANGLE_UNIT ( ) SI_UNIT ( $, .RADIAN. ) );
#126187 = CARTESIAN_POINT ( 'NONE',  ( 6.426201623197458801, 9.480690412830290015, -1.082531754730537088 ) ) ;
#126188 = CARTESIAN_POINT ( 'NONE',  ( -8.798878505144648088, 12.24881344176869469, -1.082531754730543083 ) ) ;
#126189 = AXIS2_PLACEMENT_3D ( 'NONE', #126954, #192913, #40289 ) ;
#126190 = CARTESIAN_POINT ( 'NONE',  ( 7.539742822975472158, 7.968990512992423447, -0.7216878364870317197 ) ) ;
#126191 = CARTESIAN_POINT ( 'NONE',  ( 1.160779977835691312, 1.203355533934968635, 1.617816888933524710 ) ) ;
#126193 = CARTESIAN_POINT ( 'NONE',  ( 6.039522989413334209, 1.907243403200251208, -0.7859975451465596175 ) ) ;
#126192 = CARTESIAN_POINT ( 'NONE',  ( 7.865701674222579598, 12.32840238656838139, -0.7998128361456352531 ) ) ;
#126194 = FILL_AREA_STYLE ('',( #60041 ) ) ;
#126195 = CARTESIAN_POINT ( 'NONE',  ( -3.521367211247373508, 5.131347717920458962, -1.599625672291256295 ) ) ;
#126196 = EDGE_CURVE ( 'NONE', #144319, #150870, #119533, .T. ) ;
#126197 = CIRCLE ( 'NONE', #171095, 0.07999999999999933553 ) ;
#126198 = CARTESIAN_POINT ( 'NONE',  ( -2.400879090975684971, 3.975933801733733564, 11.29524806062143760 ) ) ;
#126199 = CARTESIAN_POINT ( 'NONE',  ( 0.6823417656249899377, 1.342708333674752508, 1.181850606188755259 ) ) ;
#126200 = CARTESIAN_POINT ( 'NONE',  ( 0.2448899766094528307, -1.362147681959727574, -1.129672978174221631 ) ) ;
#126201 = CARTESIAN_POINT ( 'NONE',  ( 5.994686951402704800, -1.719894441074249158, 0.2214109503040090354 ) ) ;
#126202 = CARTESIAN_POINT ( 'NONE',  ( 5.636210787324313465, 0.3477544615747550361, 1.705165986005853229 ) ) ;
#126203 = CARTESIAN_POINT ( 'NONE',  ( 2.788958495631514545, 1.964664059585927491, -1.180940832111162520 ) ) ;
#126204 = CARTESIAN_POINT ( 'NONE',  ( 1.364683531249986537, 0.1135416670080857532, 0.7879004041258500513 ) ) ;
#126205 = CARTESIAN_POINT ( 'NONE',  ( 2.220424023188283247, -0.0004634451795330202239, 1.841320589463534052 ) ) ;
#126206 = CARTESIAN_POINT ( 'NONE',  ( 8.387690588348714726, 12.93738945304888333, 1.040834085586084257E-14 ) ) ;
#126207 = CARTESIAN_POINT ( 'NONE',  ( -10.09116860393517534, 4.085811977184856225, -6.504559477715052829 ) ) ;
#126208 = CARTESIAN_POINT ( 'NONE',  ( 2.555444900642935391, 0.4891320457309326075, -1.758753460580727790 ) ) ;
#126209 = CARTESIAN_POINT ( 'NONE',  ( 3.516250148862578584, -1.862017090670412767, 0.7743150488077471527 ) ) ;
#126210 = CARTESIAN_POINT ( 'NONE',  ( -4.582292731294565158, 4.448355729372827305, 1.214306433183764966E-14 ) ) ;
#126211 = CARTESIAN_POINT ( 'NONE',  ( 5.802526556524483681, 5.871961858807763335, 1.040834085586084257E-14 ) ) ;
#126212 = CARTESIAN_POINT ( 'NONE',  ( 5.825249245718299385, -0.05505390245461554838, 2.105416907300653673 ) ) ;
#126213 = CARTESIAN_POINT ( 'NONE',  ( -4.713430959045263435, 8.650753218861462202, 0.7998128361456481317 ) ) ;
#126214 = CARTESIAN_POINT ( 'NONE',  ( 7.319456789301566957, 16.00157973104908393, 10.35127506063409264 ) ) ;
#126215 = AXIS2_PLACEMENT_3D ( 'NONE', #26946, #192640, #41102 ) ;
#126216 = CARTESIAN_POINT ( 'NONE',  ( 2.436061438456170958, 1.271862942251865691, 1.633573898902056731 ) ) ;
#126217 = CARTESIAN_POINT ( 'NONE',  ( 3.517450787741589036, 6.191110788085444128, -1.199719254218446718 ) ) ;
#126218 = CARTESIAN_POINT ( 'NONE',  ( -1.360316468750038643, 1.192708333674735721, 0.7853790794158880262 ) ) ;
#126219 = CARTESIAN_POINT ( 'NONE',  ( 4.653055333535057514, 0.3633016933833124185, 2.088981207656291250 ) ) ;
#126220 = CARTESIAN_POINT ( 'NONE',  ( 1.506341009219732907, -0.6927896466909737594, -1.797792356224122923 ) ) ;
#126221 = ORIENTED_EDGE ( 'NONE', *, *, #167761, .T. ) ;
#126222 = CARTESIAN_POINT ( 'NONE',  ( -5.438755897737433287, 6.374245297895642537, -1.199719254218453823 ) ) ;
#126223 = CARTESIAN_POINT ( 'NONE',  ( 7.964525173024008531, 11.37936423758166526, 1.199719254218460707 ) ) ;
#126224 = CARTESIAN_POINT ( 'NONE',  ( 5.194182247366868843, 8.113610817686430110, 1.082531754730548412 ) ) ;
#126225 = CARTESIAN_POINT ( 'NONE',  ( -3.475000000000000533, -1.356249999044083943, 0.000000000000000000 ) ) ;
#126226 = CARTESIAN_POINT ( 'NONE',  ( -5.687809136132860210, 6.594531066031826150, -1.199719254218446718 ) ) ;
#126227 = CARTESIAN_POINT ( 'NONE',  ( 5.765915565743810589, 0.6138260544302427402, -2.029845472315944921 ) ) ;
#126228 = CARTESIAN_POINT ( 'NONE',  ( 2.590967463960031303, -0.3587740299011917267, -2.075001757462133778 ) ) ;
#126229 = CARTESIAN_POINT ( 'NONE',  ( -3.955946960137363799, 7.837298230127379917, 0.7998128361456352531 ) ) ;
#126230 = CARTESIAN_POINT ( 'NONE',  ( 7.456094412511537151, 10.78619501698377370, 1.199719254218460707 ) ) ;
#126231 = CARTESIAN_POINT ( 'NONE',  ( 6.280112003059028503, -1.032894792506684034, -1.547752956576850858 ) ) ;
#126232 = CARTESIAN_POINT ( 'NONE',  ( 8.423693512792301163, 8.722063941212843119, 0.7998128361456481317 ) ) ;
#126233 = FACE_BOUND ( 'NONE', #154820, .T. ) ;
#126234 = VERTEX_POINT ( 'NONE', #31415 ) ;
#126235 = CARTESIAN_POINT ( 'NONE',  ( -2.986538976760251263, 6.706322249520737522, -0.7998128361456481317 ) ) ;
#126236 = CARTESIAN_POINT ( 'NONE',  ( -9.869972641068651242, 11.57768483841065787, 1.082531754730558626 ) ) ;
#126237 = CARTESIAN_POINT ( 'NONE',  ( -3.188928480291423728, 8.980740528189222971, 2.451733079074398969 ) ) ;
#126239 = CARTESIAN_POINT ( 'NONE',  ( 2.383191274269541360, -0.003000794896521400724, 1.962046632024143866 ) ) ;
#126238 = CARTESIAN_POINT ( 'NONE',  ( 0.6801582343750022241, 2.838541667008094738, -1.178068619123834759 ) ) ;
#126240 = CARTESIAN_POINT ( 'NONE',  ( 1.481558191429487970, 1.997200094811113491, -0.8276061316847342919 ) ) ;
#126241 = VECTOR ( 'NONE', #128231, 1000.000000000000000 ) ;
#126243 = CARTESIAN_POINT ( 'NONE',  ( -5.903366504444580443, 6.144480293219754863, 0.8539384941207116553 ) ) ;
#126242 = CARTESIAN_POINT ( 'NONE',  ( -3.311934663488232733, 7.085950550703385531, -0.7998128361456481317 ) ) ;
#126245 = EDGE_CURVE ( 'NONE', #189420, #42278, #22185, .T. ) ;
#126244 = CARTESIAN_POINT ( 'NONE',  ( 0.6823417656249882723, 1.176041667008083325, -1.181850606188749264 ) ) ;
#126246 = CARTESIAN_POINT ( 'NONE',  ( 3.672919734203412112, -0.7009596788165352033, -1.586013134846143480 ) ) ;
#126247 = CARTESIAN_POINT ( 'NONE',  ( 2.413636602577839518, 1.137377966863511780, -1.317326450295707607 ) ) ;
#126248 = CARTESIAN_POINT ( 'NONE',  ( 7.144783764721768904, 7.437928601704619780, 1.040834085586084257E-14 ) ) ;
#126250 = CARTESIAN_POINT ( 'NONE',  ( -11.34342368903357290, 5.311043228906556557, 5.661199053045820051 ) ) ;
#126249 = B_SPLINE_CURVE_WITH_KNOTS ( 'NONE', 3,
 ( #105587, #38426, #103427, #138072 ),
 .UNSPECIFIED., .F., .F.,
 ( 4, 4 ),
 ( 3.313539133636207956E-16, 0.0001949197170424516140 ),
 .UNSPECIFIED. ) ;
#126251 = CARTESIAN_POINT ( 'NONE',  ( 2.179064334209149578, -0.9478932651061505732, -1.779355105811925020 ) ) ;
#126252 = DIRECTION ( 'NONE',  ( 1.214306433183764966E-17, 1.000000000000000000, 5.200010849845536803E-32 ) ) ;
#126253 = CARTESIAN_POINT ( 'NONE',  ( -3.637330350216213759, 7.465578851886037093, -0.7998128361456481317 ) ) ;
#126254 = CARTESIAN_POINT ( 'NONE',  ( 1.780087957478289074, -1.056366978776434484, 1.664393130878606852 ) ) ;
#126255 = EDGE_CURVE ( 'NONE', #55892, #89074, #106049, .T. ) ;
#126257 = CARTESIAN_POINT ( 'NONE',  ( -6.794044374223859428, 7.099008989448849505, 0.000000000000000000 ) ) ;
#126256 = CARTESIAN_POINT ( 'NONE',  ( 5.748291730981218706, 0.9368611416523886515, -1.667099895225135686 ) ) ;
#126259 = EDGE_CURVE ( 'NONE', #116165, #14896, #113035, .T. ) ;
#126258 = CARTESIAN_POINT ( 'NONE',  ( -6.441532379824190357, 6.687744995982559892, 0.7216878364870257245 ) ) ;
#126260 = CARTESIAN_POINT ( 'NONE',  ( 6.723917837734620484, 6.809268663637336516, 0.000000000000000000 ) ) ;
#126261 = AXIS2_PLACEMENT_3D ( 'NONE', #181408, #78578, #99112 ) ;
#126262 = CARTESIAN_POINT ( 'NONE',  ( -5.908321080505254841, 10.11506803722328129, 0.7998128361456291469 ) ) ;
#126263 = CARTESIAN_POINT ( 'NONE',  ( 1.488931934708405569, -1.918476728873222070, -0.6315473366199951810 ) ) ;
#126264 = SURFACE_STYLE_USAGE ( .BOTH. , #129469 ) ;
#126265 = CARTESIAN_POINT ( 'NONE',  ( 6.159233218726320125, -1.974841252017808468, -1.193533401095113300 ) ) ;
#126266 = CARTESIAN_POINT ( 'NONE',  ( 5.758247127753066685, -1.962046631956643195, -0.001586170976335121285 ) ) ;
#126267 = CARTESIAN_POINT ( 'NONE',  ( 2.940231979924610162, -1.012623612260230566, 1.680088604585870060 ) ) ;
#126268 = CARTESIAN_POINT ( 'NONE',  ( 7.235247531187115833, 11.59287255302699648, -0.7998128361456291469 ) ) ;
#126269 = CARTESIAN_POINT ( 'NONE',  ( 0.6158615555539398434, 0.1511424999406512648, 2.010826230049263863 ) ) ;
#126270 = ORIENTED_EDGE ( 'NONE', *, *, #96537, .F. ) ;
#126271 = CARTESIAN_POINT ( 'NONE',  ( 1.323616076398025587, -1.537765720040217055, -1.455736727087880489 ) ) ;
#126273 = CARTESIAN_POINT ( 'NONE',  ( -7.881367368245678406, 8.089350105908421185, 0.7998128361456602331 ) ) ;
#126272 = CARTESIAN_POINT ( 'NONE',  ( -3.002240950422295995, 5.590032644546251817, -1.199719254218452935 ) ) ;
#126274 = CARTESIAN_POINT ( 'NONE',  ( 1.534833434108737515, -1.332603482217321389, -1.270662175854364362 ) ) ;
#126275 = VERTEX_POINT ( 'NONE', #76943 ) ;
#126276 = CARTESIAN_POINT ( 'NONE',  ( 11.33572747117623791, 8.723673349139550837, 3.942066673117861519 ) ) ;
#126277 = CARTESIAN_POINT ( 'NONE',  ( 2.584367824843319283, 1.138156186954141003, 1.789115803205274080 ) ) ;
#126278 = CARTESIAN_POINT ( 'NONE',  ( 0.7499999999999902300, 4.347916667349481123, -1.299038105676658228 ) ) ;
#126279 = CARTESIAN_POINT ( 'NONE',  ( 6.076025397218672630, 10.24044673006381245, -0.7998128361456291469 ) ) ;
#126280 = CARTESIAN_POINT ( 'NONE',  ( 6.176621499477501054, 9.363752961769195693, -1.199719254218452047 ) ) ;
#126281 = CARTESIAN_POINT ( 'NONE',  ( 3.602854949731192136, 1.626725521824391230, -1.265059968925500211 ) ) ;
#126283 = CARTESIAN_POINT ( 'NONE',  ( 0.4328342922346357646, -1.301571265828086688, -1.302605208699902928 ) ) ;
#126282 = CARTESIAN_POINT ( 'NONE',  ( -8.148614017013223076, 9.465470093725620870, -1.199719254218446718 ) ) ;
#126284 = CARTESIAN_POINT ( 'NONE',  ( -1.201851678989727383E-14, 4.196875000341417028, -1.575800808251660134 ) ) ;
#126285 = CARTESIAN_POINT ( 'NONE',  ( 1.409285775387288941, 4.214549824816848478, 0.5173959003036813220 ) ) ;
#126286 = CARTESIAN_POINT ( 'NONE',  ( 0.7860941533469123499, 1.484900681275106438, 1.632775826992872492 ) ) ;
#126287 = CARTESIAN_POINT ( 'NONE',  ( 2.566018446761752170, 2.219231934913689308, -0.4390887803658559130 ) ) ;
#126288 = CARTESIAN_POINT ( 'NONE',  ( -9.327646496521992958, 9.984601788804893019, -0.7216878364870267237 ) ) ;
#126289 = CARTESIAN_POINT ( 'NONE',  ( 2.039049738775432719, 0.002999869061550211602, 1.811767226593180569 ) ) ;
#126290 = CARTESIAN_POINT ( 'NONE',  ( 3.626117945992116898, 1.907004414510531598, 0.1821707851048308124 ) ) ;
#126291 = CARTESIAN_POINT ( 'NONE',  ( 4.492674960910642667, 2.029786422369950216, 0.4070406814440513665 ) ) ;
#126292 = CARTESIAN_POINT ( 'NONE',  ( 1.364683531249988535, 3.426041667008085323, 0.7879004041258500513 ) ) ;
#126293 = CARTESIAN_POINT ( 'NONE',  ( 2.237131214483905950, -1.761753319436863086, 0.8849394531919276830 ) ) ;
#126294 = CARTESIAN_POINT ( 'NONE',  ( 6.674445239480702341, -1.183187502913226608, 1.521125075997560527 ) ) ;
#126295 = CARTESIAN_POINT ( 'NONE',  ( 2.975316878787794828, 1.776827963633962559, -0.5852370025475408521 ) ) ;
#126297 = CARTESIAN_POINT ( 'NONE',  ( 4.613585901703492809, 8.466914752176691650, -0.2784627230535564046 ) ) ;
#126296 = CARTESIAN_POINT ( 'NONE',  ( 1.735461890456877487, 0.2295834678119219041, 2.296248630371207966 ) ) ;
#126298 = CARTESIAN_POINT ( 'NONE',  ( 2.646735056387524043, -0.3148485976074810733, -1.834047879892097388 ) ) ;
#126299 = CARTESIAN_POINT ( 'NONE',  ( -0.6823417656250003738, 2.717708333674753618, -1.181850606188749264 ) ) ;
#126300 = CARTESIAN_POINT ( 'NONE',  ( 6.602015036461629904, 0.7930265726678319416, -1.904331891608399996 ) ) ;
#126301 = TOROIDAL_SURFACE ( 'NONE', #84770, 0.8300000000000010703, 0.08000000000000000167 ) ;
#126302 = CARTESIAN_POINT ( 'NONE',  ( -3.588104209110990706, 7.337872010604796991, 1.040834085586084257E-14 ) ) ;
#126303 = CARTESIAN_POINT ( 'NONE',  ( 5.991813822235618758, 9.077867661661846554, 1.199719254218462483 ) ) ;
#126304 = CARTESIAN_POINT ( 'NONE',  ( -1.264550565627408973, 3.789027290228661027, 0.5006333728358381974 ) ) ;
#126305 = CARTESIAN_POINT ( 'NONE',  ( 0.3640743269037312602, 2.082829956593022835, -0.3111531555848711106 ) ) ;
#126306 = CARTESIAN_POINT ( 'NONE',  ( 0.6823417656249917140, 3.905208333674754950, 1.181850606188765695 ) ) ;
#126307 = CARTESIAN_POINT ( 'NONE',  ( 6.151685507011436904, 0.6340151041426717038, -2.066508600247290772 ) ) ;
#126308 = CARTESIAN_POINT ( 'NONE',  ( -0.1930879795662324705, -0.4444491470046680326, -1.977061965688177825 ) ) ;
#126309 = CARTESIAN_POINT ( 'NONE',  ( 1.364683531249986537, -0.8447916663252468261, -0.7879004041258309554 ) ) ;
#126310 = CARTESIAN_POINT ( 'NONE',  ( -4.609409038966248318, 5.440360635957812718, -1.082531754730544860 ) ) ;
#126313 = CARTESIAN_POINT ( 'NONE',  ( 3.551873057100283226, 6.127307085716883428, 1.082531754730558626 ) ) ;
#126312 = CARTESIAN_POINT ( 'NONE',  ( -3.285556943749998737, -0.4302083328553760744, 1.896917185911908499 ) ) ;
#126311 = CARTESIAN_POINT ( 'NONE',  ( 6.821687566331318564, 7.987665577921906568, 1.199719254218452935 ) ) ;
#126314 = CARTESIAN_POINT ( 'NONE',  ( -5.191846479390389568, 5.021852078902356631, 0.7998128361456281477 ) ) ;
#126315 = CARTESIAN_POINT ( 'NONE',  ( 4.575407832915947104, 1.497500392235491029, 1.350737390116145242 ) ) ;
#126317 = CARTESIAN_POINT ( 'NONE',  ( -5.424670858799220063, 9.342883411992149334, 0.000000000000000000 ) ) ;
#126316 = CARTESIAN_POINT ( 'NONE',  ( -8.351459436338023679, 12.68719374246231624, -0.7216878364870267237 ) ) ;
#126319 = CARTESIAN_POINT ( 'NONE',  ( 0.6823417656249934904, 10.44270833367473550, 1.181850606188764807 ) ) ;
#126318 = CARTESIAN_POINT ( 'NONE',  ( 6.069229152942410721, 0.1638285306290178100, -2.155560115052157055 ) ) ;
#126320 = CARTESIAN_POINT ( 'NONE',  ( 10.43625799253445408, 3.019799309333367265, -6.025376361322313024 ) ) ;
#126321 = CARTESIAN_POINT ( 'NONE',  ( -11.13909472336046136, 5.782604485667383720, 4.477913003530919589 ) ) ;
#126323 = EDGE_CURVE ( 'NONE', #37173, #4671, #140671, .T. ) ;
#126322 = AXIS2_PLACEMENT_3D ( 'NONE', #89908, #40077, #57384 ) ;
#126325 = CARTESIAN_POINT ( 'NONE',  ( 0.3510145263703016716, 0.1867627727243931779, -1.906451055755745250 ) ) ;
#126324 = CARTESIAN_POINT ( 'NONE',  ( -6.358410854684793279, 7.480862754296137673, -1.082531754730543083 ) ) ;
#126326 = CARTESIAN_POINT ( 'NONE',  ( -1.402160292154681736E-14, 0.3843750003414230232, 1.575800808251672791 ) ) ;
#126327 = CARTESIAN_POINT ( 'NONE',  ( 1.556029036868112669, 0.4000000000000010214, -1.827231139298829188 ) ) ;
#126328 = CARTESIAN_POINT ( 'NONE',  ( 1.499999999999997113, 8.895833333333339255, -0.8660254037844378194 ) ) ;
#126329 = CARTESIAN_POINT ( 'NONE',  ( 1.259898821826772819, 0.6958341084943464594, 1.578493908868659146 ) ) ;
#126330 = CARTESIAN_POINT ( 'NONE',  ( 8.005163354226054295, 8.304055099544019214, 0.000000000000000000 ) ) ;
#126331 = CARTESIAN_POINT ( 'NONE',  ( 6.717138760927786834, 6.801359740696030443, -0.7998128361456481317 ) ) ;
#126332 = CARTESIAN_POINT ( 'NONE',  ( -0.6823417656250246877, -0.1364583329919108468, 1.181850606188755259 ) ) ;
#126333 = CARTESIAN_POINT ( 'NONE',  ( 0.7898890640410756170, -1.755383811729524624, -0.2245491444978504059 ) ) ;
#126334 = CARTESIAN_POINT ( 'NONE',  ( 2.367839801511921305, 0.5346396131555611886, -1.940748983941695371 ) ) ;
#126335 = CARTESIAN_POINT ( 'NONE',  ( 0.000000000000000000, 2.999999999999999112, -2.420000000000000373 ) ) ;
#126336 = CARTESIAN_POINT ( 'NONE',  ( 3.874219531129017291, 1.223701582695544854, 1.836212042189053761 ) ) ;
#126337 = CARTESIAN_POINT ( 'NONE',  ( 5.366168305121062687, -2.161276524852562275, 0.2057630808787509757 ) ) ;
#126338 = ORIENTED_EDGE ( 'NONE', *, *, #18978, .T. ) ;
#126339 = CARTESIAN_POINT ( 'NONE',  ( -0.7500000000000249800, -0.3083333333333132531, 1.299038105676659116 ) ) ;
#126340 = CARTESIAN_POINT ( 'NONE',  ( 6.765155463094740362, 10.83650577367847667, 0.7216878364870438212 ) ) ;
#126342 = CARTESIAN_POINT ( 'NONE',  ( 3.357046149680571023, 0.04665894677104672622, -2.016035383867887276 ) ) ;
#126341 = CARTESIAN_POINT ( 'NONE',  ( 2.754661888675050019, 2.104750880745378083, 0.2572054321872129790 ) ) ;
#126344 = EDGE_LOOP ( 'NONE', ( #93972, #107875, #188219, #95645, #60436 ) ) ;
#126343 = CARTESIAN_POINT ( 'NONE',  ( 3.533306822026711647, -0.1277962806783480842, 1.807111865170844656 ) ) ;
#126345 = CARTESIAN_POINT ( 'NONE',  ( 7.198453214212898743, 7.362893269528701268, 0.7998128361456291469 ) ) ;
#126346 = VERTEX_POINT ( 'NONE', #112727 ) ;
#126347 = CARTESIAN_POINT ( 'NONE',  ( 0.5494049127674709432, 0.5909524230637287490, -1.774924738581270089 ) ) ;
#126348 = COLOUR_RGB ( '', 0.09019608, 0.27058824, 0.51372549) ;
#126349 = CARTESIAN_POINT ( 'NONE',  ( 4.462605117192430804, 8.358123070033169455, 1.040834085586084257E-14 ) ) ;
#126350 = CARTESIAN_POINT ( 'NONE',  ( 6.270122753791413928, 0.9430518052575274091, 1.563124558401955300 ) ) ;
#126352 = CARTESIAN_POINT ( 'NONE',  ( 1.903404652330241476, -1.857121539659777998, 0.4695605108672970540 ) ) ;
#126351 = CARTESIAN_POINT ( 'NONE',  ( -4.288456660624211381, 3.897620947016656956, 1.214306433183764966E-14 ) ) ;
#126353 = FACE_BOUND ( 'NONE', #26298, .T. ) ;
#126354 = CARTESIAN_POINT ( 'NONE',  ( -2.788906526875773208E-15, 8.718750000682796042, -1.499999999999998446 ) ) ;
#126355 = AXIS2_PLACEMENT_3D ( 'NONE', #150562, #83400, #68198 ) ;
#126356 = CARTESIAN_POINT ( 'NONE',  ( 0.6823417656249882723, 2.238541667008084435, -1.181850606188749264 ) ) ;
#126357 = B_SPLINE_CURVE_WITH_KNOTS ( 'NONE', 3,
 ( #54029, #88676, #89754, #168837 ),
 .UNSPECIFIED., .F., .F.,
 ( 4, 4 ),
 ( 0.0006335992342243043293, 0.001020988003094174239 ),
 .UNSPECIFIED. ) ;
#126358 = CARTESIAN_POINT ( 'NONE',  ( 5.787991602622606813, -0.9759734195362681497, 1.928925553883020338 ) ) ;
#126359 = CARTESIAN_POINT ( 'NONE',  ( -5.153507786970275006, 7.105788066255672497, -1.443375672974066548 ) ) ;
#126360 = CARTESIAN_POINT ( 'NONE',  ( -7.937372586157736443, 8.224965870130965584, 0.7998128361456341429 ) ) ;
#126361 = CARTESIAN_POINT ( 'NONE',  ( 3.515986968957810266, -0.6120941298391361363, 2.030368431519948391 ) ) ;
#126363 = CARTESIAN_POINT ( 'NONE',  ( -9.979842676043658045, 5.589819607760295739, 5.978770845575332338 ) ) ;
#126362 = CARTESIAN_POINT ( 'NONE',  ( -0.1296875068448159751, 0.001480089298542403009, -1.826395826379861864 ) ) ;
#126364 = CARTESIAN_POINT ( 'NONE',  ( 4.534422775129973715, 1.932726017421485976, 0.3875534085790635630 ) ) ;
#126365 = CARTESIAN_POINT ( 'NONE',  ( 6.064708884584704585, 0.6063723501847050334, 1.813766235492550560 ) ) ;
#126366 = ORIENTED_EDGE ( 'NONE', *, *, #19563, .T. ) ;
#126367 = CARTESIAN_POINT ( 'NONE',  ( 5.981681833671104620, -0.7110503908294771858, 1.994531755910114112 ) ) ;
#126368 = CARTESIAN_POINT ( 'NONE',  ( -0.2527754068639477270, 7.036719836771394121, -4.015626449028464329 ) ) ;
#126369 = CARTESIAN_POINT ( 'NONE',  ( 0.6958625912084138720, -1.462932864358768459, -1.465259690088885014 ) ) ;
#126370 = CARTESIAN_POINT ( 'NONE',  ( 2.783070106938976274, 1.373617692895822806, 1.372961415081490610 ) ) ;
#126371 = EDGE_LOOP ( 'NONE', ( #196372, #53279, #11974, #130091, #13202, #126221, #41612, #158033 ) ) ;
#126372 = CARTESIAN_POINT ( 'NONE',  ( 5.448397627845284141, 7.449826213943242514, 1.599625672291268286 ) ) ;
#126373 = CARTESIAN_POINT ( 'NONE',  ( 7.374709211190586089, 7.568525266002632534, 0.000000000000000000 ) ) ;
#126375 = CARTESIAN_POINT ( 'NONE',  ( 5.686755365928134687, 8.721966129303114101, 1.199719254218462483 ) ) ;
#126374 = CARTESIAN_POINT ( 'NONE',  ( 3.732441334599644556, 0.3067963083541249691, 2.067875747930392638 ) ) ;
#126376 = CARTESIAN_POINT ( 'NONE',  ( 3.973948422136968084, 5.729635473950147606, -1.443375672974068769 ) ) ;
#126378 = ORIENTED_EDGE ( 'NONE', *, *, #179502, .T. ) ;
#126377 = CARTESIAN_POINT ( 'NONE',  ( 0.3986853379376364415, -0.2198743563824180347, -1.798016573952045283 ) ) ;
#126379 = CARTESIAN_POINT ( 'NONE',  ( 5.074942902252104204, -2.077123540546990110, -0.7459609299403435756 ) ) ;
#126380 = CARTESIAN_POINT ( 'NONE',  ( -0.03415196713899504993, -6.453216945989382225, -10.89423718502886373 ) ) ;
#126381 = CARTESIAN_POINT ( 'NONE',  ( 2.573496151666111231, 0.1090403232480302298, -2.204208057042057245 ) ) ;
#126382 = CARTESIAN_POINT ( 'NONE',  ( -5.249999999999987566, 0.000000000000000000, 1.599999999999997202 ) ) ;
#126383 = CARTESIAN_POINT ( 'NONE',  ( 1.471198412684338264, -1.640640410176617658, -0.9821394255850326438 ) ) ;
#126384 = CARTESIAN_POINT ( 'NONE',  ( 9.206149998879153529, 10.69926207256923689, 1.199719254218453823 ) ) ;
#126385 = CARTESIAN_POINT ( 'NONE',  ( 5.740704066448026666, -2.019076491677873619, -0.4572469816465085657 ) ) ;
#126386 = AXIS2_PLACEMENT_3D ( 'NONE', #68435, #167034, #183269 ) ;
#126388 = CARTESIAN_POINT ( 'NONE',  ( 2.993221558690632556, 1.854768100113469265, -1.110066390340218367 ) ) ;
#126387 = CARTESIAN_POINT ( 'NONE',  ( -0.007772928215657127701, 8.279395425053859725, -2.079985476292311564 ) ) ;
#126389 = CARTESIAN_POINT ( 'NONE',  ( 4.827760788416924242, 1.126602223531171898, -1.879657820484957664 ) ) ;
#126390 = ORIENTED_EDGE ( 'NONE', *, *, #81808, .F. ) ;
#126391 = CARTESIAN_POINT ( 'NONE',  ( 10.57266086055835075, 11.22919251360659310, 0.000000000000000000 ) ) ;
#126392 = SURFACE_SIDE_STYLE ('',( #136440 ) ) ;
#126393 = CARTESIAN_POINT ( 'NONE',  ( 4.764381983412778688E-15, 12.93749999999999645, -1.499999999999998446 ) ) ;
#126394 = CARTESIAN_POINT ( 'NONE',  ( 4.706615602599436343, 5.520081620234675412, 1.199719254218452935 ) ) ;
#126395 = CARTESIAN_POINT ( 'NONE',  ( 3.285556943750000514, -3.201041666188709112, 1.896917185911906722 ) ) ;
#126397 = CARTESIAN_POINT ( 'NONE',  ( -8.297226821883391779, 11.66355314463053006, 1.082531754730549967 ) ) ;
#126396 = MECHANICAL_DESIGN_GEOMETRIC_PRESENTATION_REPRESENTATION (  '', ( #105616 ), #212733 ) ;
#126398 = CARTESIAN_POINT ( 'NONE',  ( 5.411639590510088027, 6.342609606130419131, -1.199719254218452047 ) ) ;
#126399 = CARTESIAN_POINT ( 'NONE',  ( 6.016483110937820733, 0.8336820848486149460, 1.895147399281302825 ) ) ;
#126400 = CARTESIAN_POINT ( 'NONE',  ( 3.844294682379956640, 1.917307101836130512, 0.1879692045662837430 ) ) ;
#126401 = CARTESIAN_POINT ( 'NONE',  ( 0.3687678296072604556, -0.2496303596870551866, -2.000855358883571800 ) ) ;
#126402 = CARTESIAN_POINT ( 'NONE',  ( 4.961394147597008697, 7.875711374583454827, -1.199719254218452047 ) ) ;
#126403 = DIRECTION ( 'NONE',  ( 0.000000000000000000, 0.000000000000000000, -1.000000000000000000 ) ) ;
#126404 = CARTESIAN_POINT ( 'NONE',  ( 4.961744348476156752, -0.5292939252423340957, 1.896881419486784681 ) ) ;
#126405 = CARTESIAN_POINT ( 'NONE',  ( 0.4280004979528989617, 1.123059939108238314, -1.881669248891951085 ) ) ;
#126406 = CARTESIAN_POINT ( 'NONE',  ( 3.861776535121093090, 1.811678901967550326, -0.2252020330209548171 ) ) ;
#126407 = STYLED_ITEM ( 'NONE', ( #111738 ), #135185 ) ;
#126408 = CARTESIAN_POINT ( 'NONE',  ( 6.482206841109512396, 9.616306177052839743, -1.082531754730548412 ) ) ;
#126409 = CARTESIAN_POINT ( 'NONE',  ( 2.860407222358956503, 6.280966159486672140, 0.7216878364870338292 ) ) ;
#126410 = CARTESIAN_POINT ( 'NONE',  ( -7.279802135894939852, 7.457800344824362604, -0.7998128361456362523 ) ) ;
#126411 = CARTESIAN_POINT ( 'NONE',  ( 5.391302360089590628, 6.318882837306503575, -1.199719254218452047 ) ) ;
#126412 = ORIENTED_EDGE ( 'NONE', *, *, #144259, .T. ) ;
#126414 = CARTESIAN_POINT ( 'NONE',  ( 5.220952493833380004, 1.521736800665099976, -1.318127947290965052 ) ) ;
#126413 = CARTESIAN_POINT ( 'NONE',  ( 3.157574601152390414, 0.8305207305269333151, 1.643389852989694200 ) ) ;
#126415 = CARTESIAN_POINT ( 'NONE',  ( 1.054597461939084768, 2.025951976169305890, -1.085350914182762638 ) ) ;
#126416 = CARTESIAN_POINT ( 'NONE',  ( 5.805508902378371694, -1.544246397408255866, -1.209716981170713357 ) ) ;
#126417 = CARTESIAN_POINT ( 'NONE',  ( -5.687809136132860210, 6.594531066031826150, -1.199719254218446718 ) ) ;
#126418 = CARTESIAN_POINT ( 'NONE',  ( 9.501690547401153708, -8.186910008819950235, -0.4655726814551008896 ) ) ;
#126419 = CARTESIAN_POINT ( 'NONE',  ( -2.788173145904702555, 6.404619103530779789, -0.7998128361456281477 ) ) ;
#126420 = CARTESIAN_POINT ( 'NONE',  ( 0.4321921490204432281, 1.190796696626210682, 1.693455153822187587 ) ) ;
#126421 = CARTESIAN_POINT ( 'NONE',  ( -3.610214042988883598, 7.433943160120816351, 0.7998128361456352531 ) ) ;
#126423 = CARTESIAN_POINT ( 'NONE',  ( 0.5142528298564854605, 1.293200884458247657, -1.351890787750304135 ) ) ;
#126422 = CARTESIAN_POINT ( 'NONE',  ( 1.593426000515285157, -0.7013512306414200204, 1.969750900790192549 ) ) ;
#126424 = CARTESIAN_POINT ( 'NONE',  ( -1.084637062511556005, 2.932371192708034702, 1.105835307554803082 ) ) ;
#126425 = ORIENTED_EDGE ( 'NONE', *, *, #169231, .T. ) ;
#126426 = CARTESIAN_POINT ( 'NONE',  ( -0.1102773484824015326, 7.629137130509110243, -2.803480817674379288 ) ) ;
#126427 = CARTESIAN_POINT ( 'NONE',  ( 1.680815414582544243, 1.200268842161634097, 1.260572391871515263 ) ) ;
#126428 = CARTESIAN_POINT ( 'NONE',  ( 5.015626762051672571, 7.938982758113895422, 1.199719254218462483 ) ) ;
#126430 = CARTESIAN_POINT ( 'NONE',  ( 0.000000000000000000, 7.250000000000006217, 0.000000000000000000 ) ) ;
#126429 = SURFACE_STYLE_FILL_AREA ( #128571 ) ;
#126431 = CARTESIAN_POINT ( 'NONE',  ( 3.070621489812708660, -1.593986286245190565, -0.6595977741803840111 ) ) ;
#126432 = CARTESIAN_POINT ( 'NONE',  ( 2.753686713869853531, 2.180749500395392282, -0.2175628297749406803 ) ) ;
#126433 = CARTESIAN_POINT ( 'NONE',  ( 5.672569038193632451, -1.402732290180560337, 1.703733612381942653 ) ) ;
#126434 = CARTESIAN_POINT ( 'NONE',  ( -10.14898710519052649, 3.000029897349846930, -7.601419320309957151 ) ) ;
#126435 = CARTESIAN_POINT ( 'NONE',  ( 2.465899347143265086, -0.4792435138091205027, 2.117354166282244599 ) ) ;
#126436 = CARTESIAN_POINT ( 'NONE',  ( 1.084280211047653264, -1.780658692889337091, -0.4022698149812459212 ) ) ;
#126437 = CARTESIAN_POINT ( 'NONE',  ( 3.081382859721363499, 1.672078201027054734, 1.298909159995583318 ) ) ;
#126438 = CARTESIAN_POINT ( 'NONE',  ( 6.639320575229240795, 2.471732717405307422, 2.181477732991484064 ) ) ;
#126439 = EDGE_CURVE ( 'NONE', #188860, #1110, #39284, .T. ) ;
#126440 = VERTEX_POINT ( 'NONE', #45545 ) ;
#126442 = CARTESIAN_POINT ( 'NONE',  ( 1.364683531249986537, 1.176041667008082658, 0.7879004041258500513 ) ) ;
#126441 = CARTESIAN_POINT ( 'NONE',  ( 4.019262574452024062, -2.193609252165360513, 0.6655472109698862271 ) ) ;
#126443 = CARTESIAN_POINT ( 'NONE',  ( -3.486133158594716510E-16, 2.687500000000001332, -1.225000000000008749 ) ) ;
#126444 = CARTESIAN_POINT ( 'NONE',  ( 4.162516854595432747, 4.815023404238158555, 1.199719254218464037 ) ) ;
#126445 = CARTESIAN_POINT ( 'NONE',  ( 6.112022827852052309, -0.7509524718064889415, 2.090657394127520163 ) ) ;
#126446 = CARTESIAN_POINT ( 'NONE',  ( -6.778713617152821058, 7.971215977175476475, 1.082531754730549967 ) ) ;
#126447 = EDGE_CURVE ( 'NONE', #197822, #62722, #47270, .T. ) ;
#126448 = CARTESIAN_POINT ( 'NONE',  ( 4.704316114261903436, 4.590716342834741504, 1.214306433183764966E-14 ) ) ;
#126449 = CARTESIAN_POINT ( 'NONE',  ( -5.694061327615147050, 9.586895948952255608, 0.000000000000000000 ) ) ;
#126450 = DIRECTION ( 'NONE',  ( -0.000000000000000000, -1.000000000000000000, -0.000000000000000000 ) ) ;
#126451 = ORIENTED_EDGE ( 'NONE', *, *, #59704, .F. ) ;
#126452 = CARTESIAN_POINT ( 'NONE',  ( 4.184220324914634581, 1.621181886760931778, 1.198861198883696799 ) ) ;
#126454 = CARTESIAN_POINT ( 'NONE',  ( 2.061455334089828284, 1.712470851095546642, 1.149345886162132402 ) ) ;
#126453 = CARTESIAN_POINT ( 'NONE',  ( 6.972971076130050072, 7.029554431773520129, 1.040834085586084257E-14 ) ) ;
#126455 = DIRECTION ( 'NONE',  ( 5.551115123125764213E-17, 0.000000000000000000, -1.000000000000000000 ) ) ;
#126456 = CARTESIAN_POINT ( 'NONE',  ( 5.840530312436913007, 10.03597880781023299, 0.000000000000000000 ) ) ;
#126457 = CARTESIAN_POINT ( 'NONE',  ( -3.285556943750000070, -3.259374999522044014, 0.000000000000000000 ) ) ;
#126458 = CARTESIAN_POINT ( 'NONE',  ( -1.364683531250012516, 4.738541667008091096, -0.7879004041258300672 ) ) ;
#126459 = CARTESIAN_POINT ( 'NONE',  ( 5.173855182012670362, -1.219361875273092366, 1.820681821249593657 ) ) ;
#126460 = CARTESIAN_POINT ( 'NONE',  ( 2.496720397819631732, -1.994071314890283553, 0.2986276487200872354 ) ) ;
#126461 = CARTESIAN_POINT ( 'NONE',  ( 1.962219809069129184, -1.683971100191889336, -0.7449956418128443891 ) ) ;
#126462 = ADVANCED_FACE ( 'NONE', ( #162488 ), #182210, .T. ) ;
#126463 = CARTESIAN_POINT ( 'NONE',  ( 6.795661308947685164, 8.951357498570873261, -1.599625672291262513 ) ) ;
#126464 = CARTESIAN_POINT ( 'NONE',  ( 6.317409609008933558, -0.2203418483949574069, 1.812181760327068680 ) ) ;
#126465 = CARTESIAN_POINT ( 'NONE',  ( -6.551614543901706611, 8.666636272683888365, 1.599625672291283607 ) ) ;
#126467 = CARTESIAN_POINT ( 'NONE',  ( -4.736594563127865420, 6.619389305106191834, -1.599625672291271394 ) ) ;
#126466 = CARTESIAN_POINT ( 'NONE',  ( 5.436487035374818255, 2.228047177662040301, 0.3926572465528885281 ) ) ;
#126468 = CARTESIAN_POINT ( 'NONE',  ( 1.875742097524640384, 2.014971663898405652, -0.6126918839576761533 ) ) ;
#126469 = CARTESIAN_POINT ( 'NONE',  ( -6.611536185319534908, 7.742488966741438716, 1.199719254218452047 ) ) ;
#126470 = CARTESIAN_POINT ( 'NONE',  ( 9.399880572976245574, 9.860948844760784482, 0.7998128361456462443 ) ) ;
#126471 = DIRECTION ( 'NONE',  ( -1.000000000000000000, 0.000000000000000000, 0.000000000000000000 ) ) ;
#126472 = DIRECTION ( 'NONE',  ( 0.8106342104461916609, -0.3810727638831868380, 0.4445848911970676220 ) ) ;
#126473 = CARTESIAN_POINT ( 'NONE',  ( -6.744291347794091784, 9.955758108146730123, -1.199719254218440723 ) ) ;
#126474 = CARTESIAN_POINT ( 'NONE',  ( 11.97929049433705373, 12.22000000000000064, 0.7046979865771783036 ) ) ;
#126475 = CARTESIAN_POINT ( 'NONE',  ( 7.578644679914713578, 8.904468883731073703, 1.082531754730558626 ) ) ;
#126476 = CARTESIAN_POINT ( 'NONE',  ( 4.033840454514115770, 7.781623563118116316, -0.4120627063678127255 ) ) ;
#126477 = CARTESIAN_POINT ( 'NONE',  ( -9.653042183249970876, 11.32459930428888306, -1.082531754730539753 ) ) ;
#126479 = CARTESIAN_POINT ( 'NONE',  ( 2.777807369331359411, 0.3217554308703252652, -2.197856884423950774 ) ) ;
#126478 = CARTESIAN_POINT ( 'NONE',  ( 1.687894460584405731, 2.027760172737497424, -0.6205009303206151516 ) ) ;
#126480 = CARTESIAN_POINT ( 'NONE',  ( 0.000000000000000000, -1.500000000000001332, 0.000000000000000000 ) ) ;
#126481 = CARTESIAN_POINT ( 'NONE',  ( -5.773793314573309132, 7.829454515125894964, 1.599625672291263179 ) ) ;
#126482 = CARTESIAN_POINT ( 'NONE',  ( 4.822949958159288286, 6.649860922651058992, -1.599625672291256295 ) ) ;
#126483 = CARTESIAN_POINT ( 'NONE',  ( 4.053139552913617827, 1.658577106941661272, -1.047563642765911185 ) ) ;
#126484 = CARTESIAN_POINT ( 'NONE',  ( 7.879259827836241570, 12.34422023245099176, 1.040834085586084257E-14 ) ) ;
#126486 =( BOUNDED_CURVE ( )  B_SPLINE_CURVE ( 2, ( #120400, #39076, #105162, #196513, #6547, #171201, #22792 ),
 .UNSPECIFIED., .F., .T. ) 
 B_SPLINE_CURVE_WITH_KNOTS ( ( 3, 2, 2, 3 ),
 ( 0.2142857142857144681, 0.2202380952380953438, 0.2261904761904762196, 0.2321428571428570953 ),
 .UNSPECIFIED. ) 
 CURVE ( )  GEOMETRIC_REPRESENTATION_ITEM ( )  RATIONAL_B_SPLINE_CURVE ( ( 0.9999999999999956701, 0.8660254037844430375, 1.000000000000000000, 0.8660254037844387076, 1.000000000000000000, 0.8660254037844399289, 0.9999999999999987788 ) ) 
 REPRESENTATION_ITEM ( '' )  );
#126485 = CARTESIAN_POINT ( 'NONE',  ( -5.590496338642190643, 6.198678163000841401, 0.8915474099989786350 ) ) ;
#126487 = CARTESIAN_POINT ( 'NONE',  ( 2.737856954955798727, 5.281584649835344258, 1.199719254218452047 ) ) ;
#126488 = CARTESIAN_POINT ( 'NONE',  ( -1.364683531250000748, 0.7593750003414210248, 0.000000000000000000 ) ) ;
#126489 = CARTESIAN_POINT ( 'NONE',  ( -6.129694847154231852, 6.323934541200937787, -0.7216878364870338292 ) ) ;
#126491 = VERTEX_POINT ( 'NONE', #11946 ) ;
#126490 = CARTESIAN_POINT ( 'NONE',  ( -5.531363484695544841, 8.436712584578003771, 1.082531754730548412 ) ) ;
#126492 = CARTESIAN_POINT ( 'NONE',  ( 2.953504815971871977, -1.868289524550557523, 1.003269902519101864 ) ) ;
#126493 = CARTESIAN_POINT ( 'NONE',  ( -5.472651281771599763, 6.413789912602166687, 1.199719254218452935 ) ) ;
#126494 = CARTESIAN_POINT ( 'NONE',  ( 4.821240550277555492, -0.1094919189667045711, 2.159058991224649393 ) ) ;
#126495 = CARTESIAN_POINT ( 'NONE',  ( 4.370544011308346910, -0.004580445953385886559, -1.841430844414258861 ) ) ;
#126496 = CARTESIAN_POINT ( 'NONE',  ( -4.728240158028945928, 6.838416746360681309, 1.235430216343525567 ) ) ;
#126497 = CARTESIAN_POINT ( 'NONE',  ( 0.6823417656249882723, 0.4052083336747516751, 1.181850606188755259 ) ) ;
#126498 = CARTESIAN_POINT ( 'NONE',  ( 6.193256023596829252, -0.5794974496134881470, 1.641157367357688246 ) ) ;
#126499 = CARTESIAN_POINT ( 'NONE',  ( 10.88266508516665532, 3.691791674785631194, -3.942622913914296312 ) ) ;
#126500 = CARTESIAN_POINT ( 'NONE',  ( 2.399429999938675007, 5.743159399996332404, 0.000000000000000000 ) ) ;
#126501 = CARTESIAN_POINT ( 'NONE',  ( 11.70084472423419797, 7.007359388644037068, -2.672842359620002384 ) ) ;
#126502 = CARTESIAN_POINT ( 'NONE',  ( 3.081113354808207916, -0.1575343947536785305, -2.156009052512488200 ) ) ;
#126503 = STYLED_ITEM ( 'NONE', ( #52587 ), #121375 ) ;
#126504 = CARTESIAN_POINT ( 'NONE',  ( 6.151720201709268920, -0.2930281871833945173, -1.994563951915592881 ) ) ;
#126505 = CARTESIAN_POINT ( 'NONE',  ( -8.853111119599343937, 10.39134639669645566, 1.082531754730558626 ) ) ;
#126506 = CARTESIAN_POINT ( 'NONE',  ( 2.588937169860201504, -0.3686131662095324946, -2.129881858774537395 ) ) ;
#126507 = CARTESIAN_POINT ( 'NONE',  ( 4.112542095708375811, 1.396345452295008727, -1.391819494878621111 ) ) ;
#126508 = MECHANICAL_DESIGN_GEOMETRIC_PRESENTATION_REPRESENTATION (  '', ( #212833 ), #150555 ) ;
#126509 = EDGE_CURVE ( 'NONE', #211752, #19657, #189173, .T. ) ;
#126510 = CARTESIAN_POINT ( 'NONE',  ( -0.04112450405316381286, -1.960553898366865555, -0.9795403211517728082 ) ) ;
#126511 = CARTESIAN_POINT ( 'NONE',  ( 0.1129635547038260190, -0.9897495874401724958, -2.082026327295583012 ) ) ;
#126512 = CARTESIAN_POINT ( 'NONE',  ( 4.651864714057460048, 0.7465859729765094155, 1.793013943324140769 ) ) ;
#126515 = ORIENTED_EDGE ( 'NONE', *, *, #16540, .F. ) ;
#126514 = SURFACE_STYLE_USAGE ( .BOTH. , #64625 ) ;
#126513 = CARTESIAN_POINT ( 'NONE',  ( -9.788623718942277563, 10.52240854829523187, 1.040834085586084257E-14 ) ) ;
#126517 = EDGE_CURVE ( 'NONE', #66184, #174777, #109190, .T. ) ;
#126516 = CARTESIAN_POINT ( 'NONE',  ( -5.284646014276622950, 9.387447126623207794, -0.7998128361456362523 ) ) ;
#126518 = CARTESIAN_POINT ( 'NONE',  ( 3.469446951953614189E-15, 0.2401923788623722134, 6.938893903907228378E-15 ) ) ;
#126520 = ORIENTED_EDGE ( 'NONE', *, *, #154299, .T. ) ;
#126519 = CARTESIAN_POINT ( 'NONE',  ( -4.685224601974262271, 7.623789914682047808, -1.199719254218453823 ) ) ;
#126521 = CARTESIAN_POINT ( 'NONE',  ( -7.497295758232712437, 11.69066945133944380, -0.7216878364870267237 ) ) ;
#126522 = CARTESIAN_POINT ( 'NONE',  ( 2.731697238759897672, -2.059418846490802313, 0.7933392487004319316 ) ) ;
#126523 = CARTESIAN_POINT ( 'NONE',  ( -3.285556943750000070, -1.509374999522042238, 0.000000000000000000 ) ) ;
#126524 = CARTESIAN_POINT ( 'NONE',  ( 6.772321408939014020, -0.9219223515295159599, -1.731591420108986812 ) ) ;
#126525 = CARTESIAN_POINT ( 'NONE',  ( 1.364683531249992088, 5.446875000341417916, 1.214306433183764966E-14 ) ) ;
#126526 = CARTESIAN_POINT ( 'NONE',  ( -0.7499999999999972244, 4.389583334016150751, -1.299038105676652899 ) ) ;
#126527 = CARTESIAN_POINT ( 'NONE',  ( 5.232446707518059625, 6.618332276934084213, -1.382299536160000120 ) ) ;
#126529 = DIRECTION ( 'NONE',  ( -0.04520447523801534445, 0.000000000000000000, 0.9989777552170296948 ) ) ;
#126528 = CARTESIAN_POINT ( 'NONE',  ( 0.07499057489260704812, 2.034159190454051913, -2.372362849262329210 ) ) ;
#126530 = CARTESIAN_POINT ( 'NONE',  ( 5.560457619783242933, -1.666209093894938764, -0.7835883864039174806 ) ) ;
#126531 = ORIENTED_EDGE ( 'NONE', *, *, #182196, .F. ) ;
#126532 = CARTESIAN_POINT ( 'NONE',  ( 1.360316468749978469, -0.4843749996586016460, -3.816391647148975608E-14 ) ) ;
#126533 = CARTESIAN_POINT ( 'NONE',  ( -7.344766530301162000, 9.591980256816594164, 1.599625672291295375 ) ) ;
#126534 = DIRECTION ( 'NONE',  ( -5.578564026256490882E-16, -1.000000000000000000, -9.066213480720158442E-32 ) ) ;
#126535 = CARTESIAN_POINT ( 'NONE',  ( 5.994406619193555663, -1.133004004027007294, 1.792352430775605798 ) ) ;
#126536 = CARTESIAN_POINT ( 'NONE',  ( -2.324999999999998845, 0.000000000000000000, -0.5000000000000004441 ) ) ;
#126537 = CARTESIAN_POINT ( 'NONE',  ( 5.769158057814842699, 6.689438141327490150, 1.199719254218462483 ) ) ;
#126538 = CARTESIAN_POINT ( 'NONE',  ( 6.221960870361377793, -1.141027836104959281, -1.715851070140647527 ) ) ;
#126541 = CARTESIAN_POINT ( 'NONE',  ( 5.073706409418358376, -1.018251046719556685, 1.533866337327425278 ) ) ;
#126540 = CARTESIAN_POINT ( 'NONE',  ( 2.365471783816187834, -0.4113058309756181807, 1.814853103561973935 ) ) ;
#126539 = DIRECTION ( 'NONE',  ( -0.5773502691896091887, 0.000000000000000000, 0.8164965809277375808 ) ) ;
#126542 = CARTESIAN_POINT ( 'NONE',  ( 6.771407655021410399, 9.987393799911945536, -1.199719254218441611 ) ) ;
#126543 = CARTESIAN_POINT ( 'NONE',  ( -4.911894908834722351, 4.738238661368090909, 0.4458799699701230246 ) ) ;
#126544 = CARTESIAN_POINT ( 'NONE',  ( -5.433785704026946384, 9.561443431331920095, 0.000000000000000000 ) ) ;
#126546 = ORIENTED_EDGE ( 'NONE', *, *, #43966, .T. ) ;
#126545 = DIRECTION ( 'NONE',  ( 0.000000000000000000, 1.000000000000000000, 0.000000000000000000 ) ) ;
#126547 = CIRCLE ( 'NONE', #60739, 0.07999999999999907185 ) ;
#126548 = CARTESIAN_POINT ( 'NONE',  ( 4.178501018151202118, -1.271701901513167421, 1.803451139310302986 ) ) ;
#126549 = CARTESIAN_POINT ( 'NONE',  ( 5.606774309801295431, 1.718512474747270868, -1.471603694038286836 ) ) ;
#126550 = CARTESIAN_POINT ( 'NONE',  ( -4.433153041988574294, 8.115836282387899558, 1.040834085586084257E-14 ) ) ;
#126551 = CARTESIAN_POINT ( 'NONE',  ( 5.924035771748266122, -1.796794102754266431, 0.2306889152782486963 ) ) ;
#126552 = CARTESIAN_POINT ( 'NONE',  ( 6.368375084315238688, -1.880202862833039834, -0.3662410793365057926 ) ) ;
#126553 = DIRECTION ( 'NONE',  ( -1.000000000000000000, 0.000000000000000000, 0.000000000000000000 ) ) ;
#126554 = CARTESIAN_POINT ( 'NONE',  ( 8.927850118614284014, 14.71571904887444049, -8.019635469902768321 ) ) ;
#126555 = CARTESIAN_POINT ( 'NONE',  ( 5.918603479541379997, -0.6925943527147163659, -1.782627650866043911 ) ) ;
#126556 = CARTESIAN_POINT ( 'NONE',  ( 11.33772463945036968, 12.59097530385349728, -3.600000000000000977 ) ) ;
#126557 = CARTESIAN_POINT ( 'NONE',  ( 0.1802491246630563426, -1.813337052076903877, -0.4591185353455888296 ) ) ;
#126558 = AXIS2_PLACEMENT_3D ( 'NONE', #126640, #107175, #109319 ) ;
#126559 = CARTESIAN_POINT ( 'NONE',  ( 0.8840003597419334724, -2.016708404047353742, 0.004841148455551891328 ) ) ;
#126561 = CARTESIAN_POINT ( 'NONE',  ( 3.528042858452341335, -1.254676591636105121, -1.691379958841844111 ) ) ;
#126560 = CARTESIAN_POINT ( 'NONE',  ( -10.49131193887636826, 11.13428543831092909, 1.040834085586084257E-14 ) ) ;
#126562 = CARTESIAN_POINT ( 'NONE',  ( 8.910733272679570049, 11.41894145625809820, -1.599625672291255185 ) ) ;
#126564 = CARTESIAN_POINT ( 'NONE',  ( -8.799405390469187793, 10.22472669609091689, -1.199719254218446718 ) ) ;
#126563 = CARTESIAN_POINT ( 'NONE',  ( -1.402160292154681736E-14, -0.7874999999999764411, 1.732050807568877637 ) ) ;
#126565 = CARTESIAN_POINT ( 'NONE',  ( 3.199477664157297063, 1.824241505505564964, -0.8673461216518009165 ) ) ;
#126566 = CARTESIAN_POINT ( 'NONE',  ( -1.201851678989727383E-14, 2.946875000341419248, -1.575800808251660134 ) ) ;
#126567 = AXIS2_PLACEMENT_3D ( 'NONE', #156459, #40577, #155375 ) ;
#126568 = CARTESIAN_POINT ( 'NONE',  ( 3.195971524519376494, 4.751719416737803847, -1.599625672291262513 ) ) ;
#126569 = CARTESIAN_POINT ( 'NONE',  ( 3.901784996602038813, -0.6316019492740264640, 2.067237329103743804 ) ) ;
#126570 = CARTESIAN_POINT ( 'NONE',  ( -1.737500000000000266, -1.764583332377417380, -3.009438278150923907 ) ) ;
#126571 = CARTESIAN_POINT ( 'NONE',  ( -1.499999999999997780, 5.150000000000022560, 1.214306433183764966E-14 ) ) ;
#126573 = DIRECTION ( 'NONE',  ( -0.9988044021632734859, 0.000000000000000000, 0.04888523518676873847 ) ) ;
#126572 = CARTESIAN_POINT ( 'NONE',  ( 5.318541398310776103, 9.426991741329731056, -0.7998128361456481317 ) ) ;
#126574 = CARTESIAN_POINT ( 'NONE',  ( 7.741342523278692767, 11.01502146292508044, 1.082531754730558626 ) ) ;
#126576 = DIRECTION ( 'NONE',  ( 1.598721155460225418E-14, 0.000000000000000000, 1.000000000000000000 ) ) ;
#126575 = CARTESIAN_POINT ( 'NONE',  ( 1.029994877853340762, 2.092549206400303063, -0.5788440209302682105 ) ) ;
#126578 = CARTESIAN_POINT ( 'NONE',  ( 0.9074547957551477584, -0.8278116715597811925, -1.644758345054016191 ) ) ;
#126577 = CARTESIAN_POINT ( 'NONE',  ( -6.561783159334137139, 8.678499657355050800, -1.443375672974059665 ) ) ;
#126579 = CARTESIAN_POINT ( 'NONE',  ( -1.364683531250012516, 2.030208333674750953, 0.7879004041258379498 ) ) ;
#126580 = CARTESIAN_POINT ( 'NONE',  ( 1.874823134854076923, -0.1115055541827478930, -2.188858692977871279 ) ) ;
#126581 = CARTESIAN_POINT ( 'NONE',  ( 6.364460139928007187, 6.849615385491503616, 0.6807898044721304442 ) ) ;
#126582 = CARTESIAN_POINT ( 'NONE',  ( 3.098750496328426252, -0.6552482397011113457, -2.165565034296774272 ) ) ;
#126583 = CARTESIAN_POINT ( 'NONE',  ( -6.612626235163205024, 8.737816579155630592, -1.599625672291263179 ) ) ;
#126584 = CARTESIAN_POINT ( 'NONE',  ( 1.364683531249988535, 4.217708333674752730, -0.7879004041258239610 ) ) ;
#126585 = CARTESIAN_POINT ( 'NONE',  ( 5.234661009243278151, 7.693064604033777343, 1.208367059251337361 ) ) ;
#126586 = CARTESIAN_POINT ( 'NONE',  ( -6.009258394948636914E-15, 12.18750000000000178, -1.732050807568875195 ) ) ;
#126587 = CARTESIAN_POINT ( 'NONE',  ( 5.560252395380198998, 9.501061871336672127, 0.7216878364870317197 ) ) ;
#126588 = CARTESIAN_POINT ( 'NONE',  ( 4.077242326343363032, 1.667005924876462597, -0.5946135600440533020 ) ) ;
#126589 = CARTESIAN_POINT ( 'NONE',  ( 7.913155211870404493, 12.38376484715752213, 0.7998128361456462443 ) ) ;
#126590 = CARTESIAN_POINT ( 'NONE',  ( 1.290213853529555976, -0.9470325862265884798, 1.881093767389901750 ) ) ;
#126592 = CARTESIAN_POINT ( 'NONE',  ( 1.499999999999987121, 1.795833333333355819, -0.8660254037844253849 ) ) ;
#126591 = CARTESIAN_POINT ( 'NONE',  ( 0.6823417656249969321, 10.02604166700806587, -1.181850606188757036 ) ) ;
#126593 = CARTESIAN_POINT ( 'NONE',  ( -5.041653019435350380, 6.975290837464928728, -1.599625672291271394 ) ) ;
#126594 = CARTESIAN_POINT ( 'NONE',  ( 6.169546029190324354, 1.392557221580101201, 1.458547251757099428 ) ) ;
#126596 = ORIENTED_EDGE ( 'NONE', *, *, #209460, .F. ) ;
#126595 = CARTESIAN_POINT ( 'NONE',  ( 5.062699594374425516, 0.5334270428436416189, 1.731249764757249343 ) ) ;
#126597 = CARTESIAN_POINT ( 'NONE',  ( 3.186256133050053840, -1.842714570631575510, -0.3211874441736498054 ) ) ;
#126598 = CARTESIAN_POINT ( 'NONE',  ( 4.610256228194366201, 2.069909489248497714, -0.04556564433023241323 ) ) ;
#126599 = CARTESIAN_POINT ( 'NONE',  ( -5.383996397958228819, 8.335060660042973524, 1.082531754730550855 ) ) ;
#126600 = CARTESIAN_POINT ( 'NONE',  ( -1.734723475976807094E-15, 2.999999999999988898, -6.938893903907228378E-15 ) ) ;
#126601 = CARTESIAN_POINT ( 'NONE',  ( 9.562578416340237197, 10.05076299535211781, 0.7998128361456462443 ) ) ;
#126602 = CARTESIAN_POINT ( 'NONE',  ( -8.642432853707342488, 12.17025653171218558, 1.199719254218462483 ) ) ;
#126603 = CARTESIAN_POINT ( 'NONE',  ( 7.503511670520385479, 7.718794801887437274, 0.7998128361456281477 ) ) ;
#126604 = CARTESIAN_POINT ( 'NONE',  ( -5.609475307034339053, 6.101878995311609266, -0.7682545557971790506 ) ) ;
#126605 = CARTESIAN_POINT ( 'NONE',  ( 1.364683531249984538, -1.094791666325247936, -0.7879004041258309554 ) ) ;
#126606 = CARTESIAN_POINT ( 'NONE',  ( 3.666413850373055006, -0.7928392042928497085, -1.794698522912529182 ) ) ;
#126607 = CARTESIAN_POINT ( 'NONE',  ( 0.8607036144342284922, -0.7282710370301350711, 1.880145570116364073 ) ) ;
#126608 = CARTESIAN_POINT ( 'NONE',  ( -3.634467696915153034, 6.397906858779740524, 1.199719254218452935 ) ) ;
#126610 = CARTESIAN_POINT ( 'NONE',  ( 0.4635785636673654952, -6.836568542495036205, 10.85353573482952250 ) ) ;
#126609 = CARTESIAN_POINT ( 'NONE',  ( 8.446893396513862839, 9.813462703143045474, -1.199719254218445830 ) ) ;
#126611 = CARTESIAN_POINT ( 'NONE',  ( 1.194370141144196706, -0.4488658031855938813, -1.815784161679114384 ) ) ;
#126612 = CARTESIAN_POINT ( 'NONE',  ( -1.364683531250010295, 4.030208333674751842, 0.7879004041258379498 ) ) ;
#126613 = CARTESIAN_POINT ( 'NONE',  ( 3.445567785929729343, -1.858493022056451949, 0.7744065704922193927 ) ) ;
#126615 = CARTESIAN_POINT ( 'NONE',  ( 3.603210856581297694, -0.1536155211374414797, 2.111693916904446855 ) ) ;
#126614 = CARTESIAN_POINT ( 'NONE',  ( -6.073689629242165822, 7.148687991279732756, -1.082531754730544860 ) ) ;
#126616 = CARTESIAN_POINT ( 'NONE',  ( 3.559858690238754342, 7.375195248579016649, -0.1711817872153587328 ) ) ;
#126617 = CARTESIAN_POINT ( 'NONE',  ( 5.283670394142272464, -1.967056725255760474, 0.6460906113585006549 ) ) ;
#126618 = CARTESIAN_POINT ( 'NONE',  ( 4.598150373690133463, 5.393538853173795111, -1.199719254218452047 ) ) ;
#126620 = CARTESIAN_POINT ( 'NONE',  ( 11.91826849282518630, 13.39999999999998259, 1.399999999999996581 ) ) ;
#126619 = CARTESIAN_POINT ( 'NONE',  ( 6.632766914392992597, -1.868179159523954302, 0.9385789683672930428 ) ) ;
#126622 = EDGE_LOOP ( 'NONE', ( #197732, #186269, #146430, #99136, #141572 ) ) ;
#126621 = CARTESIAN_POINT ( 'NONE',  ( 5.579063851370913873, -0.04688903583028104782, -1.825137680102270288 ) ) ;
#126623 = CARTESIAN_POINT ( 'NONE',  ( 8.426556166093362776, 9.789735934319136135, -1.199719254218446718 ) ) ;
#126624 = CARTESIAN_POINT ( 'NONE',  ( 4.839532526265843515, 5.050905555379832990, 0.6780825091596712761 ) ) ;
#126625 = CARTESIAN_POINT ( 'NONE',  ( 9.808998241650231265, 12.88675894182173387, 8.003755498086194464 ) ) ;
#126626 = CARTESIAN_POINT ( 'NONE',  ( 6.159228477734898455, -1.889628185881117695, -1.139594184263223120 ) ) ;
#126627 = CARTESIAN_POINT ( 'NONE',  ( -0.6823417656250039265, 11.63020833367473017, -1.181850606188755259 ) ) ;
#126628 = CARTESIAN_POINT ( 'NONE',  ( 5.057238878282278804, -1.638088962530854786, 0.9864336689310859718 ) ) ;
#126629 = CARTESIAN_POINT ( 'NONE',  ( -7.160677686311960777, 11.50587440067263678, -0.7998128361456291469 ) ) ;
#126630 = CARTESIAN_POINT ( 'NONE',  ( 4.794779880727245036, 8.745660294157122649, -0.7998128361456281477 ) ) ;
#126631 = DIRECTION ( 'NONE',  ( 0.000000000000000000, 0.000000000000000000, -1.000000000000000000 ) ) ;
#126632 = CARTESIAN_POINT ( 'NONE',  ( 2.670593071767634719, 6.059516317130127838, -0.7216878364870267237 ) ) ;
#126633 = CARTESIAN_POINT ( 'NONE',  ( 9.512045263456261779, -8.176568542494926817, -0.4655551865852028404 ) ) ;
#126634 = CARTESIAN_POINT ( 'NONE',  ( 5.508690485854129903, 5.321227076451600091, 1.040834085586084257E-14 ) ) ;
#126635 = VERTEX_POINT ( 'NONE', #139473 ) ;
#126636 = CARTESIAN_POINT ( 'NONE',  ( -6.587282531393266360, 8.778525268082516320, 1.599625672291269396 ) ) ;
#126637 = EDGE_CURVE ( 'NONE', #139360, #57181, #61162, .T. ) ;
#126638 = CARTESIAN_POINT ( 'NONE',  ( -0.3861634464758929020, -3.134276582748693585, -3.366986391098497400 ) ) ;
#126639 = CARTESIAN_POINT ( 'NONE',  ( 6.047819040147648373, 9.213483425884394507, 1.199719254218452047 ) ) ;
#126640 = CARTESIAN_POINT ( 'NONE',  ( 0.000000000000000000, 13.49999999999999822, 0.000000000000000000 ) ) ;
#126641 = CARTESIAN_POINT ( 'NONE',  ( 0.1399997263886037790, 2.025166351305721868, -2.415484119839182320 ) ) ;
#126642 = CARTESIAN_POINT ( 'NONE',  ( -4.907688418466881863, 8.669460888279271416, 0.7216878364870458196 ) ) ;
#126643 = CARTESIAN_POINT ( 'NONE',  ( 4.630273154266905777, 5.360739087188218122, 1.199719254218464037 ) ) ;
#126644 = CARTESIAN_POINT ( 'NONE',  ( 2.237097273892864724, -0.09148514208244534762, -1.967424487969974711 ) ) ;
#126645 = CARTESIAN_POINT ( 'NONE',  ( 3.357046149680571023, 0.04665894677104672622, -2.016035383867887276 ) ) ;
#126646 = CARTESIAN_POINT ( 'NONE',  ( -5.994676475536691029, 10.14553965476814845, 0.7998128361456481317 ) ) ;
#126647 = CARTESIAN_POINT ( 'NONE',  ( 5.876533236880477240, 5.820653295974182129, 0.7998128361456352531 ) ) ;
#126648 = CARTESIAN_POINT ( 'NONE',  ( 6.827182134110167055, 4.690515317746113411, 2.651606140002475076 ) ) ;
#126649 = CARTESIAN_POINT ( 'NONE',  ( 3.750093249908572623, 0.7883579158753216687, 2.044908353623323016 ) ) ;
#126650 = CARTESIAN_POINT ( 'NONE',  ( 4.517520595836055364, 8.499999999998847144, 0.1397284385386432237 ) ) ;
#126651 = CARTESIAN_POINT ( 'NONE',  ( 1.729391032145210394, -1.814785505609041838, 0.6465514451386763506 ) ) ;
#126652 = CARTESIAN_POINT ( 'NONE',  ( -7.700141177557535244, 11.07091624287075859, -1.199719254218446718 ) ) ;
#126653 = CARTESIAN_POINT ( 'NONE',  ( 1.244150428498994376, 3.053773246564666977, 0.7750000000000100142 ) ) ;
#126654 = CARTESIAN_POINT ( 'NONE',  ( 0.2329586101569320611, 0.7537478099126624365, -1.931748487665209124 ) ) ;
#126655 = CARTESIAN_POINT ( 'NONE',  ( -10.33433454857960321, 4.766519530047388820, -5.444264161973041638 ) ) ;
#126656 = CARTESIAN_POINT ( 'NONE',  ( 7.958799866421889746, 9.244020251369077457, -1.199719254218441611 ) ) ;
#126657 = CARTESIAN_POINT ( 'NONE',  ( 5.178324605415663306, 8.128796908705222535, 1.199719254218462483 ) ) ;
#126658 =( BOUNDED_CURVE ( )  B_SPLINE_CURVE ( 2, ( #212832, #160907, #12504, #144698, #64470 ),
 .UNSPECIFIED., .F., .T. ) 
 B_SPLINE_CURVE_WITH_KNOTS ( ( 3, 2, 3 ),
 ( 0.1232094925783373957, 0.1250000000000000000, 0.1270731450466760504 ),
 .UNSPECIFIED. ) 
 CURVE ( )  GEOMETRIC_REPRESENTATION_ITEM ( )  RATIONAL_B_SPLINE_CURVE ( ( 0.9343361104663525651, 0.9424281978788288106, 1.000000000000000000, 0.9333402950740685711, 0.9330143039465762511 ) ) 
 REPRESENTATION_ITEM ( '' )  );
#126659 = CARTESIAN_POINT ( 'NONE',  ( -5.736990052180565236, 5.898621588815100125, -2.499999999999995115 ) ) ;
#126660 = CARTESIAN_POINT ( 'NONE',  ( 4.719646871332936477, 8.520355426614829142, -0.7216878364870357165 ) ) ;
#126661 = ORIENTED_EDGE ( 'NONE', *, *, #191584, .T. ) ;
#126663 = CARTESIAN_POINT ( 'NONE',  ( 3.440093027223433797, -1.200828029685986786, -1.615568007891918789 ) ) ;
#126662 = CARTESIAN_POINT ( 'NONE',  ( 6.515202330376022921, -1.784155196879381622, 0.4545711315065634195 ) ) ;
#126664 = CARTESIAN_POINT ( 'NONE',  ( 4.376513399274863936, -0.3984044028133710835, 2.263477716089700387 ) ) ;
#126666 = CARTESIAN_POINT ( 'NONE',  ( 2.500643731865523023, 0.4022941478849762498, 1.816780921579076225 ) ) ;
#126665 = CARTESIAN_POINT ( 'NONE',  ( -0.1290005225502641184, 1.996213967822700663, -2.587563282167547385 ) ) ;
#126668 = CARTESIAN_POINT ( 'NONE',  ( -1.642778471875000035, -2.267708332855375541, -2.845375778867859751 ) ) ;
#126667 = APPLICATION_CONTEXT ( 'automotive_design' ) ;
#126669 = CARTESIAN_POINT ( 'NONE',  ( 11.94105721237522921, 11.02740784401788865, -1.187919463087249605 ) ) ;
#126670 = FILL_AREA_STYLE_COLOUR ( '', #26264 ) ;
#126671 = CARTESIAN_POINT ( 'NONE',  ( -7.212047647465563038, 10.50147379109678880, -1.199719254218446718 ) ) ;
#126672 = CARTESIAN_POINT ( 'NONE',  ( -6.129694847154231852, 6.323934541200937787, -0.7216878364870338292 ) ) ;
#126674 = CARTESIAN_POINT ( 'NONE',  ( 3.643291952642300213, -1.415932857957047375, -1.222571138756740838 ) ) ;
#126673 = CARTESIAN_POINT ( 'NONE',  ( 5.056232447125663221, -1.513354532948107956, 1.442795048270538727 ) ) ;
#126675 = CARTESIAN_POINT ( 'NONE',  ( 7.307481608085759639, 7.627742752295940676, 1.040834085586084257E-14 ) ) ;
#126676 = ORIENTED_EDGE ( 'NONE', *, *, #148262, .F. ) ;
#126677 = EDGE_CURVE ( 'NONE', #130349, #15288, #106201, .T. ) ;
#126678 = CARTESIAN_POINT ( 'NONE',  ( 2.972033609136344623, 6.549060441754430251, -0.4946758370507741698 ) ) ;
#126679 = LINE ( 'NONE', #44294, #79063 ) ;
#126680 = CARTESIAN_POINT ( 'NONE',  ( 5.848237035817564156, 1.723274176396558888, 0.07769637638467204177 ) ) ;
#126681 = CARTESIAN_POINT ( 'NONE',  ( -5.819474248763749635, 7.812472595022922128, -1.599625672291256295 ) ) ;
#126682 = CARTESIAN_POINT ( 'NONE',  ( 1.424001084297383146, -1.255706242181073851, -1.196294345734474129 ) ) ;
#126683 = CARTESIAN_POINT ( 'NONE',  ( -7.093286029333435216, 14.55189876998235832, 9.634085594043046541 ) ) ;
#126684 = CARTESIAN_POINT ( 'NONE',  ( 6.661184041420940005, -7.473374494058216300, -6.773376349083132908 ) ) ;
#126685 = CONICAL_SURFACE ( 'NONE', #202649, 1.903066852858540603, 0.4537856055185301996 ) ;
#126686 = CARTESIAN_POINT ( 'NONE',  ( 5.541899213757757181, 1.452536422000339611, 1.613792965789240696 ) ) ;
#126687 = CARTESIAN_POINT ( 'NONE',  ( 4.441915170580639227, 0.7783198120194650960, -1.651611053696280695 ) ) ;
#126688 = CARTESIAN_POINT ( 'NONE',  ( 2.500770564479499303, 0.4249116886347775734, 1.915039037836663738 ) ) ;
#126689 = CARTESIAN_POINT ( 'NONE',  ( 0.2459221440733790898, 2.093483123843339122, -0.3155690596675052584 ) ) ;
#126690 = CARTESIAN_POINT ( 'NONE',  ( 9.476364169157013961, 3.602179700984872390, 7.289721614627932667 ) ) ;
#126691 = CARTESIAN_POINT ( 'NONE',  ( -9.130526383799315582, 12.73969898348616070, 1.199719254218462483 ) ) ;
#126692 = CARTESIAN_POINT ( 'NONE',  ( 7.995557903757111617, 10.35123685918189729, 1.599625672291281386 ) ) ;
#126693 = CARTESIAN_POINT ( 'NONE',  ( 2.491022521637117570, -2.029929026191950481, -0.6131127883793398015 ) ) ;
#126694 = CARTESIAN_POINT ( 'NONE',  ( -3.687454593236990430, 4.364747115940301292, 1.082531754730560403 ) ) ;
#126695 = CARTESIAN_POINT ( 'NONE',  ( 1.237941840314000785, 1.374772708486753370, 1.500000000000001332 ) ) ;
#126696 = CARTESIAN_POINT ( 'NONE',  ( -4.775553520644376881, 6.797630844710244702, -1.243162211532616857 ) ) ;
#126697 = CARTESIAN_POINT ( 'NONE',  ( 1.112269271232646739, 2.068042923180101411, -0.09779880236997220977 ) ) ;
#126699 = CARTESIAN_POINT ( 'NONE',  ( -1.500000000000008216, 14.03125000068279604, 3.469446951953614189E-15 ) ) ;
#126698 = DIRECTION ( 'NONE',  ( -1.000000000000000000, 4.336808689942017736E-16, 8.881784197001260212E-16 ) ) ;
#126701 = ORIENTED_EDGE ( 'NONE', *, *, #4201, .F. ) ;
#126700 = CARTESIAN_POINT ( 'NONE',  ( 3.563320577568354075, -1.815308083731239419, 1.279909030408127091 ) ) ;
#126702 = CARTESIAN_POINT ( 'NONE',  ( 0.6338907866723633155, 0.6742984703760960263, 2.197570948669794966 ) ) ;
#126704 = CARTESIAN_POINT ( 'NONE',  ( 5.524308913217452321, 1.011932313297726038, 1.797175476313887188 ) ) ;
#126703 = CARTESIAN_POINT ( 'NONE',  ( 3.009020027229115879, 5.597941567487558778, -1.199719254218446718 ) ) ;
#126706 = CARTESIAN_POINT ( 'NONE',  ( 1.737500000000001155, -1.983333333333333393, 3.009438278150922130 ) ) ;
#126705 = CARTESIAN_POINT ( 'NONE',  ( 4.390861645979372341, 6.216034235099629157, -1.599625672291269396 ) ) ;
#126707 = CARTESIAN_POINT ( 'NONE',  ( 0.1331565106231606399, 5.723858289613107608, -2.539976893513963052 ) ) ;
#126708 = CARTESIAN_POINT ( 'NONE',  ( 5.530750200611445067, -1.661959182355336795, 0.7928504710919548337 ) ) ;
#126710 = CARTESIAN_POINT ( 'NONE',  ( 5.554837709854577810, 5.910988393603817670, -0.7721120281754164649 ) ) ;
#126709 = CIRCLE ( 'NONE', #60922, 0.08000000000000001554 ) ;
#126711 = EDGE_CURVE ( 'NONE', #157478, #116214, #102594, .T. ) ;
#126712 = CARTESIAN_POINT ( 'NONE',  ( -0.1106727585415836906, 0.7252806920327293794, -2.087287528096515299 ) ) ;
#126713 = CARTESIAN_POINT ( 'NONE',  ( 3.065164753754692661, 0.2545988855646770244, -1.705743084088023664 ) ) ;
#126714 = CARTESIAN_POINT ( 'NONE',  ( 1.305875433988498813, -1.124247956386617231, -1.673852571057246053 ) ) ;
#126715 = CARTESIAN_POINT ( 'NONE',  ( 3.164923336591000336, 1.459680849325554197, 1.775737417650694816 ) ) ;
#126716 = CARTESIAN_POINT ( 'NONE',  ( 2.583610768588519235, 2.069371435550710459, -0.9147937799905188072 ) ) ;
#126717 = CARTESIAN_POINT ( 'NONE',  ( 5.496739094006439785, -0.5105849265115348645, -2.043105244204785453 ) ) ;
#126718 = CARTESIAN_POINT ( 'NONE',  ( -7.132998214565509087, 7.494455136514109661, 0.7216878364870317197 ) ) ;
#126719 = CARTESIAN_POINT ( 'NONE',  ( 3.250976011129117715, -1.444759545231928843, -1.021753751062564497 ) ) ;
#126721 = CARTESIAN_POINT ( 'NONE',  ( 6.550320078384911149, -1.775227793318678415, 1.449923619939506025 ) ) ;
#126720 = CARTESIAN_POINT ( 'NONE',  ( 4.543390873910906791, 6.393985001019784953, 1.443375672974065660 ) ) ;
#126722 = CARTESIAN_POINT ( 'NONE',  ( 4.277188459880359339, 1.204364621523913437, 1.392669941884729035 ) ) ;
#126723 = CARTESIAN_POINT ( 'NONE',  ( -4.436542580169821726, 6.199052314996659874, 1.599625672291267398 ) ) ;
#126724 = CARTESIAN_POINT ( 'NONE',  ( 6.304178240230120522, 6.457222156464352381, -0.7216878364870257245 ) ) ;
#126725 = CARTESIAN_POINT ( 'NONE',  ( 0.7499999999999885647, 3.316666666666689967, -1.299038105676658228 ) ) ;
#126726 = CARTESIAN_POINT ( 'NONE',  ( 4.558633756138521065, -1.956834287480881285, -0.9866608250781593314 ) ) ;
#126727 = CARTESIAN_POINT ( 'NONE',  ( -4.029797971759847997, 5.724516938518342535, -1.599625672291256295 ) ) ;
#126728 = CARTESIAN_POINT ( 'NONE',  ( 0.3006164276378255340, 8.220220202720884828, -1.980250916746227441 ) ) ;
#126729 = EDGE_CURVE ( 'NONE', #171149, #71186, #147868, .T. ) ;
#126730 = CARTESIAN_POINT ( 'NONE',  ( 5.301260566756325510, -1.777534899005998481, 1.061244097098137606 ) ) ;
#126731 = CARTESIAN_POINT ( 'NONE',  ( 0.4621254960020632074, -1.116205757145168231, 1.679226196708947239 ) ) ;
#126732 = CARTESIAN_POINT ( 'NONE',  ( -1.364683531250012516, 4.988541667008084879, -0.7879004041258300672 ) ) ;
#126733 = CARTESIAN_POINT ( 'NONE',  ( 3.141151230849213327, -1.698683669661217754, 0.9087857633808916757 ) ) ;
#126734 = CARTESIAN_POINT ( 'NONE',  ( 1.364683531250000303, 9.005208333674731946, -0.7879004041258355073 ) ) ;
#126735 = CARTESIAN_POINT ( 'NONE',  ( -3.850152436600983386, 4.554561266531622188, 1.082531754730560403 ) ) ;
#126736 = CARTESIAN_POINT ( 'NONE',  ( 0.3346308043965214307, -1.195296165414746037, -1.872270659723746622 ) ) ;
#126737 = ORIENTED_EDGE ( 'NONE', *, *, #148914, .F. ) ;
#126739 = CARTESIAN_POINT ( 'NONE',  ( -6.471393748265563239, 5.229711127717889596, 2.419999999999998597 ) ) ;
#126738 = CARTESIAN_POINT ( 'NONE',  ( -4.177320726786328819, 5.966903162707725805, -1.443375672974066548 ) ) ;
#126740 = CARTESIAN_POINT ( 'NONE',  ( 5.217190183160311356, 4.981143389975473568, -0.7998128361456211532 ) ) ;
#126741 = DIRECTION ( 'NONE',  ( 1.000000000000000000, 1.045014142154703195E-15, 0.000000000000000000 ) ) ;
#126742 =( NAMED_UNIT ( * ) SI_UNIT ( $, .STERADIAN. ) SOLID_ANGLE_UNIT ( ) );
#126743 = CARTESIAN_POINT ( 'NONE',  ( 0.04971382200798128703, 7.069534788352777710, -4.059379717803641263 ) ) ;
#126744 = CARTESIAN_POINT ( 'NONE',  ( -2.494940289813118994, 3.038492715500545227, 11.73777120880565583 ) ) ;
#126745 = CARTESIAN_POINT ( 'NONE',  ( 1.381223342121252085, -0.05156877537583307025, 1.961363007973878858 ) ) ;
#126746 = CARTESIAN_POINT ( 'NONE',  ( -1.201851678989727383E-14, 1.384375000341419693, 1.575800808251672791 ) ) ;
#126747 = CARTESIAN_POINT ( 'NONE',  ( 6.737200384369169903, -1.933438233944267060, 0.9670071574134844195 ) ) ;
#126748 = CARTESIAN_POINT ( 'NONE',  ( 5.459412808053472510, 1.602871733476991079, 1.130958114227413436 ) ) ;
#126749 = CARTESIAN_POINT ( 'NONE',  ( -7.947050595904583403, 12.42330946186405249, 0.7998128361456481317 ) ) ;
#126750 = CARTESIAN_POINT ( 'NONE',  ( -6.697364695026446491, 6.915939687060050467, 1.040834085586084257E-14 ) ) ;
#126751 = CARTESIAN_POINT ( 'NONE',  ( 5.875883356151954118, 1.283970044810868849, 1.738936680771227206 ) ) ;
#126753 = ORIENTED_EDGE ( 'NONE', *, *, #128643, .T. ) ;
#126752 = CARTESIAN_POINT ( 'NONE',  ( -0.1376292675369459595, -5.401429653175759071, -10.96107445065240249 ) ) ;
#126754 = CARTESIAN_POINT ( 'NONE',  ( -1.201851678989727383E-14, 3.946875000341423689, -1.575800808251660134 ) ) ;
#126755 = CARTESIAN_POINT ( 'NONE',  ( 0.3857445262360514882, -0.8876765639535091346, 1.646530163845527195 ) ) ;
#126756 = CARTESIAN_POINT ( 'NONE',  ( 6.309869086801066729, -1.462580435118435496, 0.9307709330467325293 ) ) ;
#126757 = ADVANCED_FACE ( 'NONE', ( #43048 ), #10504, .F. ) ;
#126759 = CARTESIAN_POINT ( 'NONE',  ( 2.964592600559623037, -2.025863808726846127, -0.8364240203130177687 ) ) ;
#126758 = CARTESIAN_POINT ( 'NONE',  ( 0.6801582343749831283, 1.057291667008075642, -1.178068619123862515 ) ) ;
#126760 = CARTESIAN_POINT ( 'NONE',  ( 4.507023749723728656, 1.786828103088284658, -1.460221407940938798 ) ) ;
#126761 = CARTESIAN_POINT ( 'NONE',  ( 6.116494506269664733, 1.387434351230539598, -1.523912472565646770 ) ) ;
#126762 = CARTESIAN_POINT ( 'NONE',  ( 0.9900592867461569524, -0.4711592545371501295, -1.883805795384153381 ) ) ;
#126763 = CARTESIAN_POINT ( 'NONE',  ( -5.544921637864824504, 8.452530429942200385, -1.082531754730543971 ) ) ;
#126764 = PRODUCT_DEFINITION_SHAPE ( 'NONE', 'NONE',  #57493 ) ;
#126765 = EDGE_CURVE ( 'NONE', #116972, #72298, #88851, .T. ) ;
#126766 = PLANE ( 'NONE',  #16024 ) ;
#126767 = CARTESIAN_POINT ( 'NONE',  ( 4.588201236890728119, 1.223260742344203900, 1.732012071221388450 ) ) ;
#126768 = DIRECTION ( 'NONE',  ( 1.000000000000000000, -0.000000000000000000, -0.000000000000000000 ) ) ;
#126769 = CARTESIAN_POINT ( 'NONE',  ( 2.127577483945505055, 0.4445034925110411539, 1.966644524931899563 ) ) ;
#126770 = CARTESIAN_POINT ( 'NONE',  ( -5.707619481228834779, 5.761236937629489852, -0.7216878364870197293 ) ) ;
#126771 = CARTESIAN_POINT ( 'NONE',  ( 5.262800499965147871, -1.601618428465928057, 1.518362080380669221 ) ) ;
#126772 = CARTESIAN_POINT ( 'NONE',  ( -5.610041701004606196, 9.767075427805856691, -0.7998128361456362523 ) ) ;
#126773 = CARTESIAN_POINT ( 'NONE',  ( -3.398092380850382455, -3.087907399781644191, -0.5045427134251018186 ) ) ;
#126774 = CARTESIAN_POINT ( 'NONE',  ( 0.2932112110246976044, 1.350478442433366677, 1.228755397233910696 ) ) ;
#126775 = LINE ( 'NONE', #112642, #203254 ) ;
#126778 = CIRCLE ( 'NONE', #195796, 10.97656854249491509 ) ;
#126777 = CARTESIAN_POINT ( 'NONE',  ( 3.863710590214593399, 7.451486755318259547, 1.040834085586084257E-14 ) ) ;
#126776 = CARTESIAN_POINT ( 'NONE',  ( -4.662743238902972820, 8.402825839448235357, 0.5650157067484343765 ) ) ;
#126779 = CARTESIAN_POINT ( 'NONE',  ( 1.474093356799754062, 8.744500914157981697, -2.533844564144165812 ) ) ;
#126780 = ORIENTED_EDGE ( 'NONE', *, *, #70214, .T. ) ;
#126781 = CARTESIAN_POINT ( 'NONE',  ( 5.155176885484381799, -1.739861089072095357, -1.104300716835506346 ) ) ;
#126782 = CARTESIAN_POINT ( 'NONE',  ( -7.065207446052809814, 9.336104335185325453, -1.443375672974066548 ) ) ;
#126783 = UNCERTAINTY_MEASURE_WITH_UNIT (LENGTH_MEASURE( 1.000000000000000082E-05 ), #1300, 'distance_accuracy_value', 'NONE');
#126784 = CARTESIAN_POINT ( 'NONE',  ( -0.2108831679770960255, 0.2438762813419328990, -1.931650693707862132 ) ) ;
#126785 = CARTESIAN_POINT ( 'NONE',  ( -3.090368948911150770, 5.692848642783215674, 1.199719254218462483 ) ) ;
#126786 = CARTESIAN_POINT ( 'NONE',  ( -4.625266680917477835, 5.425174544939014964, -1.199719254218453823 ) ) ;
#126787 = CARTESIAN_POINT ( 'NONE',  ( 5.022131231807676066, -2.009760515157756444, 0.1999713455246488469 ) ) ;
#126789 = EDGE_LOOP ( 'NONE', ( #177604, #172927, #56519, #43989 ) ) ;
#126788 = CARTESIAN_POINT ( 'NONE',  ( -1.201851678989727383E-14, 1.462500000000018119, 1.732050807568877637 ) ) ;
#126791 = CARTESIAN_POINT ( 'NONE',  ( 9.598809568795314107, 10.30095870645710754, -0.7216878364870257245 ) ) ;
#126790 = CARTESIAN_POINT ( 'NONE',  ( -5.004894982100124068, 5.868074229652107121, 1.199719254218452935 ) ) ;
#126792 = CARTESIAN_POINT ( 'NONE',  ( 7.820355676984174664, 8.018169799436671852, -0.7998128361456281477 ) ) ;
#126793 = CARTESIAN_POINT ( 'NONE',  ( 3.731368383135937883, -1.904846641313600708, 0.7871492865094924518 ) ) ;
#126794 = CARTESIAN_POINT ( 'NONE',  ( 2.531875153343257523, -1.674887184936912909, 1.122499117612890673 ) ) ;
#126795 = VERTEX_POINT ( 'NONE', #110225 ) ;
#126796 = CARTESIAN_POINT ( 'NONE',  ( 6.727182134110200273, 7.629137130509069387, 2.789055895399249696 ) ) ;
#126797 = CARTESIAN_POINT ( 'NONE',  ( 4.005544317833563461, 6.760553239859419250, -1.199719254218452047 ) ) ;
#126799 = ORIENTED_EDGE ( 'NONE', *, *, #8140, .F. ) ;
#126798 = CARTESIAN_POINT ( 'NONE',  ( -6.084577077482911101, 10.32070003369722144, 0.000000000000000000 ) ) ;
#126800 = CARTESIAN_POINT ( 'NONE',  ( 2.952499795743710020, 1.423742661936340470, 1.427719607385954381 ) ) ;
#126801 = CARTESIAN_POINT ( 'NONE',  ( 2.589598559577494186, -1.836209955096680613, -0.1354230481333124070 ) ) ;
#126802 = CARTESIAN_POINT ( 'NONE',  ( 0.7862591250819307431, 1.553807182831347777, 1.706378029075397151 ) ) ;
#126803 = CARTESIAN_POINT ( 'NONE',  ( 3.576318658954677598, 7.394398545414291313, 0.7998128361456281477 ) ) ;
#126804 = CARTESIAN_POINT ( 'NONE',  ( 3.040462492942562545, 2.144887288335277198, 0.2678724578094940356 ) ) ;
#126805 = CARTESIAN_POINT ( 'NONE',  ( -7.250913225210214641, 7.353820272367037170, 0.7998128361456341429 ) ) ;
#126806 = ORIENTED_EDGE ( 'NONE', *, *, #100563, .F. ) ;
#126807 = DIRECTION ( 'NONE',  ( -0.000000000000000000, 1.000000000000000000, -0.000000000000000000 ) ) ;
#126808 = CARTESIAN_POINT ( 'NONE',  ( 0.9713206009373563932, 1.803875226702996049, -0.4951341686536685494 ) ) ;
#126809 = ORIENTED_EDGE ( 'NONE', *, *, #35863, .T. ) ;
#126810 = CARTESIAN_POINT ( 'NONE',  ( 5.893431036533754330, 1.492594341498763466, 1.288039297220463730 ) ) ;
#126812 = CARTESIAN_POINT ( 'NONE',  ( 7.714226216051361718, 11.94375498546120795, -0.7216878364870267237 ) ) ;
#126811 = CARTESIAN_POINT ( 'NONE',  ( -1.201851678989727383E-14, 3.446875000341421469, -1.575800808251660134 ) ) ;
#126814 = CARTESIAN_POINT ( 'NONE',  ( 0.3291288957359936318, 2.113116833900237967, 0.6364493931270903682 ) ) ;
#126813 = CARTESIAN_POINT ( 'NONE',  ( -7.901704598666176693, 8.113076874732334076, 0.7998128361456602331 ) ) ;
#126815 = CARTESIAN_POINT ( 'NONE',  ( 6.514133371570012265, 2.065101995627930620, -0.1482383472809906122 ) ) ;
#126816 = CARTESIAN_POINT ( 'NONE',  ( 4.632082037363250748, 8.555846143565791095, -0.7998128361456231517 ) ) ;
#126817 = CARTESIAN_POINT ( 'NONE',  ( -6.762819695118240659, 6.784377820593065600, 0.7998128361456341429 ) ) ;
#126818 = DIRECTION ( 'NONE',  ( 1.040834085586084257E-15, 1.000000000000000000, -4.622230424712076367E-32 ) ) ;
#126819 = CARTESIAN_POINT ( 'NONE',  ( 5.172717120832922788, -1.856099020970953806, -0.6648386725634397587 ) ) ;
#126820 = CARTESIAN_POINT ( 'NONE',  ( 6.187761630889374587, 1.931537729788906477, -0.5904018810464291001 ) ) ;
#126821 = CARTESIAN_POINT ( 'NONE',  ( -1.402160292154681736E-14, 0.6187500006828180465, -1.732050807568863648 ) ) ;
#126822 = CARTESIAN_POINT ( 'NONE',  ( 4.811288673970230967, 2.006026520401600788, 1.140621419682581239 ) ) ;
#126823 = CARTESIAN_POINT ( 'NONE',  ( 1.797792903779442009, -1.491087995953117140, -1.425289625791379411 ) ) ;
#126824 = CARTESIAN_POINT ( 'NONE',  ( 6.805829924380105034, 9.923590097543378619, 1.082531754730558626 ) ) ;
#126825 = CARTESIAN_POINT ( 'NONE',  ( 5.041653019435334393, 6.975290837464928728, -1.599625672291269396 ) ) ;
#126826 = CARTESIAN_POINT ( 'NONE',  ( 4.655245641445829641, 6.524482229810530498, 1.599625672291269396 ) ) ;
#126827 = CARTESIAN_POINT ( 'NONE',  ( 0.6823417656249899377, 2.655208333674753618, 1.181850606188767472 ) ) ;
#126828 = CARTESIAN_POINT ( 'NONE',  ( 3.715816618597135523, 6.492813934075403637, -1.199719254218453823 ) ) ;
#126829 = CARTESIAN_POINT ( 'NONE',  ( 5.246642258364164313, 8.104537820524768676, -1.082531754730549078 ) ) ;
#126830 = CARTESIAN_POINT ( 'NONE',  ( 5.564936049989869460, 1.647787920686558438, -1.413916910601682897 ) ) ;
#126831 = DIRECTION ( 'NONE',  ( 0.9982742078614211811, 0.000000000000000000, -0.05872483221476467591 ) ) ;
#126833 = CARTESIAN_POINT ( 'NONE',  ( 3.878315922200573862, -0.1843894689829879696, -1.832007427040844183 ) ) ;
#126832 = CARTESIAN_POINT ( 'NONE',  ( -4.609409038966248318, 5.440360635957812718, -1.082531754730544860 ) ) ;
#126835 = CARTESIAN_POINT ( 'NONE',  ( 6.620655732516672387, 6.040129668214249570, 2.321170174800915031 ) ) ;
#126834 = CARTESIAN_POINT ( 'NONE',  ( -0.1604749557937330817, 7.629137130509052511, -2.703579865625728385 ) ) ;
#126836 = CARTESIAN_POINT ( 'NONE',  ( 5.601184584505256581, -0.5335315006234629953, 2.125516261704554211 ) ) ;
#126837 = LINE ( 'NONE', #61750, #53140 ) ;
#126838 = CARTESIAN_POINT ( 'NONE',  ( 6.209908689894510836, -2.246332978858367468, 0.2696892186580777673 ) ) ;
#126839 = CARTESIAN_POINT ( 'NONE',  ( -4.043597078347817231, 7.757176853022865082, 0.5683662157932849457 ) ) ;
#126840 = CARTESIAN_POINT ( 'NONE',  ( 5.057296774772758852, 7.978757421411086348, 1.172581024337983724 ) ) ;
#126841 = CARTESIAN_POINT ( 'NONE',  ( -5.777182852754558340, 5.912670547734647286, 0.000000000000000000 ) ) ;
#126842 = CARTESIAN_POINT ( 'NONE',  ( 3.390947817193682656, 6.009837315817661008, -1.082531754730549967 ) ) ;
#126844 = EDGE_CURVE ( 'NONE', #26788, #120076, #37401, .T. ) ;
#126843 = CARTESIAN_POINT ( 'NONE',  ( 0.6371259318241145886, -1.247223858821765230, -1.255979444004810430 ) ) ;
#126845 = AXIS2_PLACEMENT_3D ( 'NONE', #55408, #25029, #104169 ) ;
#126846 = CARTESIAN_POINT ( 'NONE',  ( 5.022139790744326149, -2.003173700978663874, 0.1997323756105211789 ) ) ;
#126847 = CARTESIAN_POINT ( 'NONE',  ( 5.819474248763732760, 7.812472595022922128, -1.599625672291262513 ) ) ;
#126848 = CARTESIAN_POINT ( 'NONE',  ( 3.610471823009605341, -0.8516972358460070947, -1.926234778997274244 ) ) ;
#126849 = CARTESIAN_POINT ( 'NONE',  ( 3.286649939900693429, 1.508079230315559016, -1.181058552281685659 ) ) ;
#126850 = CARTESIAN_POINT ( 'NONE',  ( 11.94105721237523277, 19.00000000000000000, 1.187919463087248273 ) ) ;
#126851 = CARTESIAN_POINT ( 'NONE',  ( 4.299236425489592506, -1.714783525531939690, 0.9686585690476202659 ) ) ;
#126852 = CARTESIAN_POINT ( 'NONE',  ( 5.836196223694859242, -1.125476168604349514, -1.676936384952235404 ) ) ;
#126853 = CARTESIAN_POINT ( 'NONE',  ( 1.938157646728836614, 1.849873822469105145, 0.2772664081076986475 ) ) ;
#126856 = ORIENTED_EDGE ( 'NONE', *, *, #162518, .T. ) ;
#126855 = CARTESIAN_POINT ( 'NONE',  ( 1.089939655121434203, 1.141396045679959004, 1.534244836814010693 ) ) ;
#126854 = CARTESIAN_POINT ( 'NONE',  ( 4.600069218058569831, -1.724633479392148949, -0.03822871362766516734 ) ) ;
#126858 = CARTESIAN_POINT ( 'NONE',  ( 4.039966587192257208, 6.696749537490852333, 1.082531754730558626 ) ) ;
#126857 = CARTESIAN_POINT ( 'NONE',  ( 1.559489335033688251, -1.894147805384650995, -1.132260830144316888 ) ) ;
#126859 = VECTOR ( 'NONE', #150720, 1000.000000000000000 ) ;
#126860 = CARTESIAN_POINT ( 'NONE',  ( 0.6823417656249882723, 1.488541667008083547, -1.181850606188749264 ) ) ;
#126861 = CARTESIAN_POINT ( 'NONE',  ( 9.101601193475611140, 9.512956235343358102, -0.7998128361456221525 ) ) ;
#126862 = DIRECTION ( 'NONE',  ( 3.347138415753903010E-16, 0.6000000000000019762, -0.7999999999999986011 ) ) ;
#126863 = DIRECTION ( 'NONE',  ( -0.5996521035822321988, -0.8002608041566222630, 0.000000000000000000 ) ) ;
#126864 = CARTESIAN_POINT ( 'NONE',  ( -3.893162665418476109, 7.693773542963529444, 1.040834085586084257E-14 ) ) ;
#126865 = DIRECTION ( 'NONE',  ( 1.000000000000000000, 0.000000000000000000, 0.000000000000000000 ) ) ;
#126866 = ORIENTED_EDGE ( 'NONE', *, *, #114896, .F. ) ;
#126867 = CARTESIAN_POINT ( 'NONE',  ( 2.541538742049511246, 1.893869637037654208, -0.8368498079355383146 ) ) ;
#126868 = CARTESIAN_POINT ( 'NONE',  ( -1.201851678989727383E-14, 2.962500000000025224, 1.732050807568877637 ) ) ;
#126869 = CARTESIAN_POINT ( 'NONE',  ( 6.582647274634798151, 7.638508894284114170, 1.199719254218462483 ) ) ;
#126870 = CARTESIAN_POINT ( 'NONE',  ( -6.418895661066105873, 9.576129806964074120, -1.199719254218440723 ) ) ;
#126871 = CARTESIAN_POINT ( 'NONE',  ( 5.239300017038202917, 5.077214539491492928, 0.000000000000000000 ) ) ;
#126872 = CARTESIAN_POINT ( 'NONE',  ( 6.164709077089638001, 0.6648188651474650213, 2.013622499735030491 ) ) ;
#126873 = CARTESIAN_POINT ( 'NONE',  ( 0.7499999999999902300, 5.816666666666685082, -1.299038105676658228 ) ) ;
#126874 = CARTESIAN_POINT ( 'NONE',  ( -1.201851678989727383E-14, 2.571875000341417472, 1.575800808251672791 ) ) ;
#126875 = CIRCLE ( 'NONE', #16045, 0.07999999999999993228 ) ;
#126877 = CARTESIAN_POINT ( 'NONE',  ( 4.695201269034174452, 4.372156323494968966, 1.214306433183764966E-14 ) ) ;
#126876 = CARTESIAN_POINT ( 'NONE',  ( -0.4019237886466802689, 11.69866454968463287, -1.500000000000002887 ) ) ;
#126878 = CARTESIAN_POINT ( 'NONE',  ( 4.639999869408336863, 0.002810260262744306969, -2.016288307263448321 ) ) ;
#126879 = CARTESIAN_POINT ( 'NONE',  ( 4.645656780685024856, 1.893963204498310571, -0.2871864570129621375 ) ) ;
#126880 = CARTESIAN_POINT ( 'NONE',  ( 2.489988787850425656, -2.185901284972164405, -0.1580625509675498419 ) ) ;
#126881 = CARTESIAN_POINT ( 'NONE',  ( 0.1335669894368343991, 6.947499997881672940, -2.748639729795236963 ) ) ;
#126882 = CARTESIAN_POINT ( 'NONE',  ( -0.7500000000000215383, 0.9729166673494854534, 1.299038105676659116 ) ) ;
#126883 = CARTESIAN_POINT ( 'NONE',  ( 5.273694575261410833, 0.3885250917745143862, -1.975199337908732256 ) ) ;
#126884 = CARTESIAN_POINT ( 'NONE',  ( -7.705111371268023923, 7.883718109434487253, 1.040834085586084257E-14 ) ) ;
#126886 = CARTESIAN_POINT ( 'NONE',  ( 6.415624682135008250, -1.382911306069923407, -1.603242893440869343 ) ) ;
#126885 = CARTESIAN_POINT ( 'NONE',  ( -3.389175213736311587, 4.977123720824209840, 1.443375672974064550 ) ) ;
#126887 = CARTESIAN_POINT ( 'NONE',  ( 0.6823417656249969321, 10.33854166700806587, -1.181850606188757036 ) ) ;
#126889 = CARTESIAN_POINT ( 'NONE',  ( 0.4999999999999900080, 3.949999999999995293, -0.4000000000000339950 ) ) ;
#126888 = CARTESIAN_POINT ( 'NONE',  ( 3.439088004391201991, -1.584594249056283877, -1.364047514679037620 ) ) ;
#126891 = ORIENTED_EDGE ( 'NONE', *, *, #122971, .T. ) ;
#126890 = CARTESIAN_POINT ( 'NONE',  ( 2.133451061308448526, -1.123891114067215424, -1.308414479858905022 ) ) ;
#126892 = CARTESIAN_POINT ( 'NONE',  ( 6.187751663909415001, 2.028806014889028120, -0.6170373231123224000 ) ) ;
#126893 = CARTESIAN_POINT ( 'NONE',  ( 5.799137018343234473, 7.788745826199009237, -1.599625672291262513 ) ) ;
#126894 = ADVANCED_FACE ( 'NONE', ( #8373 ), #156361, .T. ) ;
#126895 = CARTESIAN_POINT ( 'NONE',  ( -1.507347117465284603, 13.24758771607280572, 0.07965694612802574903 ) ) ;
#126896 = LINE ( 'NONE', #192853, #200218 ) ;
#126897 = CARTESIAN_POINT ( 'NONE',  ( 6.849430810391395674, -7.996947095390812166, -6.637758778446690933 ) ) ;
#126898 = CARTESIAN_POINT ( 'NONE',  ( 5.632522751473472589, 8.658694745772667289, -1.199719254218440723 ) ) ;
#126899 = ORIENTED_EDGE ( 'NONE', *, *, #91211, .T. ) ;
#126900 = CARTESIAN_POINT ( 'NONE',  ( -11.88156762547253997, 13.87999991545968292, -1.686557021358706443 ) ) ;
#126901 = CARTESIAN_POINT ( 'NONE',  ( 2.262115610809340094, 1.811117530136572285, 0.04320712765945587674 ) ) ;
#126902 = CARTESIAN_POINT ( 'NONE',  ( -6.124532705071231931, 8.168374127381657246, -1.599625672291263179 ) ) ;
#126903 = ORIENTED_EDGE ( 'NONE', *, *, #36635, .F. ) ;
#126904 = CARTESIAN_POINT ( 'NONE',  ( 5.040934186182656873, 4.775511393501539636, 1.040834085586084257E-14 ) ) ;
#126905 = ORIENTED_EDGE ( 'NONE', *, *, #212736, .T. ) ;
#126906 = CARTESIAN_POINT ( 'NONE',  ( 4.603875680292229156, 7.528882839386387360, 1.199719254218452047 ) ) ;
#126907 = CARTESIAN_POINT ( 'NONE',  ( 3.861793950654641261, 0.6069239149280086787, -1.706917045096454366 ) ) ;
#126908 = CARTESIAN_POINT ( 'NONE',  ( 6.539320575229251808, 0.004279804010676873348, 1.996977849922920267 ) ) ;
#126909 = CARTESIAN_POINT ( 'NONE',  ( -10.98194350564911481, -7.699999999999996625, 0.6300133639306312316 ) ) ;
#126910 = CARTESIAN_POINT ( 'NONE',  ( 4.062392026992976746, 7.509557588607558287, 0.5198811075141016591 ) ) ;
#126911 = EDGE_CURVE ( 'NONE', #140339, #19327, #29193, .T. ) ;
#126912 = CARTESIAN_POINT ( 'NONE',  ( 3.894834723524211118, 0.2711828204805393772, 1.841042229387960472 ) ) ;
#126913 = EDGE_CURVE ( 'NONE', #201094, #177962, #171858, .T. ) ;
#126914 = CARTESIAN_POINT ( 'NONE',  ( 1.212342387966048651, 1.846533033048233463, 0.5095510818057205071 ) ) ;
#126915 = CARTESIAN_POINT ( 'NONE',  ( 0.7272432748211544729, -1.735090175422876246, 0.5678700757711930835 ) ) ;
#126916 = CARTESIAN_POINT ( 'NONE',  ( -1.250000000000039302, 8.500000000000000000, -10.85702537530423228 ) ) ;
#126917 = CARTESIAN_POINT ( 'NONE',  ( 6.830415307812257808, 7.849261790823902629, 6.717278222822394618 ) ) ;
#126918 = CARTESIAN_POINT ( 'NONE',  ( 5.685886686578042415, 7.314606927785019863, 1.221034997698521307 ) ) ;
#126919 = CARTESIAN_POINT ( 'NONE',  ( -11.33772463945037146, 10.19999999999998153, 3.599999999999999201 ) ) ;
#126920 = CARTESIAN_POINT ( 'NONE',  ( 0.000000000000000000, 3.799999999999998046, 6.249999999999995559 ) ) ;
#126921 = CARTESIAN_POINT ( 'NONE',  ( 7.375272376154084597, 9.627570410311676596, -1.443375672974057666 ) ) ;
#126922 = CARTESIAN_POINT ( 'NONE',  ( 5.418793955257063644, -1.429144796294969932, 1.355356204701572143 ) ) ;
#126923 = B_SPLINE_CURVE_WITH_KNOTS ( 'NONE', 3,
 ( #213205, #144011, #145070, #45414 ),
 .UNSPECIFIED., .F., .F.,
 ( 4, 4 ),
 ( 0.000000000000000000, 0.0002939798689656232381 ),
 .UNSPECIFIED. ) ;
#126924 = CARTESIAN_POINT ( 'NONE',  ( -5.199715606040888005, 6.025088614257851027, -1.199719254218446718 ) ) ;
#126925 = CARTESIAN_POINT ( 'NONE',  ( 4.800089777832203808, 5.120415418395356077, -0.7784788408505428636 ) ) ;
#126926 = CARTESIAN_POINT ( 'NONE',  ( 0.2344723086637650333, 0.3594713984965206000, 2.059332689821891105 ) ) ;
#126927 = CARTESIAN_POINT ( 'NONE',  ( 8.620286740190458374, 8.951422706510690830, 1.040834085586084257E-14 ) ) ;
#126928 = CARTESIAN_POINT ( 'NONE',  ( 5.684577344524033293, -1.879503395548718148, -0.4217397607521166103 ) ) ;
#126929 = CARTESIAN_POINT ( 'NONE',  ( -6.891622154448065807, 6.934647356477856128, 1.040834085586084257E-14 ) ) ;
#126930 = CARTESIAN_POINT ( 'NONE',  ( 0.9557436305893591832, 1.823730570757614800, -0.08488363409227266121 ) ) ;
#126931 = CARTESIAN_POINT ( 'NONE',  ( 2.104404934925046877, -2.206339196854599116, 0.05594281105186085790 ) ) ;
#126932 = CARTESIAN_POINT ( 'NONE',  ( 11.94105721839851952, 12.57301656658866662, 1.187919402540718927 ) ) ;
#126933 = CARTESIAN_POINT ( 'NONE',  ( 0.4395310841842986482, -1.815173276516975243, 0.6020934215927520317 ) ) ;
#126934 = EDGE_LOOP ( 'NONE', ( #99793, #197426, #28183, #191077, #205737 ) ) ;
#126935 = CARTESIAN_POINT ( 'NONE',  ( 0.8714670931111346830, -0.2923345663568870378, 1.947617037577647592 ) ) ;
#126936 = CARTESIAN_POINT ( 'NONE',  ( 2.384236373620087335, -0.3343274798127248149, -1.912924682550071864 ) ) ;
#126937 = MECHANICAL_DESIGN_GEOMETRIC_PRESENTATION_REPRESENTATION (  '', ( #147580 ), #12718 ) ;
#126938 = CARTESIAN_POINT ( 'NONE',  ( 0.9485920322965735174, 1.351945250224910744, 1.495824703658617416 ) ) ;
#126940 = CARTESIAN_POINT ( 'NONE',  ( 5.541811466629937399, 1.248470921604339923, 1.380218479220591155 ) ) ;
#126939 = CARTESIAN_POINT ( 'NONE',  ( -6.981522756394290319, 7.109807735406931783, 0.7998128361456341429 ) ) ;
#126941 = CARTESIAN_POINT ( 'NONE',  ( 5.435893244436359240, 5.306573304789342416, -0.7998128361456481317 ) ) ;
#126942 = CARTESIAN_POINT ( 'NONE',  ( -11.44779965693221335, 13.49686076798708889, -3.599999932276612746 ) ) ;
#126943 = CARTESIAN_POINT ( 'NONE',  ( -7.523999700038797478, -5.166862915010145940, -8.024744567526228778 ) ) ;
#126944 = CARTESIAN_POINT ( 'NONE',  ( -5.199715606040888005, 6.025088614257851027, -1.199719254218446718 ) ) ;
#126945 = CARTESIAN_POINT ( 'NONE',  ( -5.752402313948099533, 9.933162809573264695, -0.7998128361456362523 ) ) ;
#126946 = CARTESIAN_POINT ( 'NONE',  ( 1.013517375116283592, -2.137022957946862700, 0.4851717564131745597 ) ) ;
#126947 = CARTESIAN_POINT ( 'NONE',  ( 4.582292731738905722, 5.408724944192588424, -1.082531754730548412 ) ) ;
#126948 = CARTESIAN_POINT ( 'NONE',  ( 7.876360894896227371, 8.153785563659219804, -0.7998128361456341429 ) ) ;
#126949 = DIRECTION ( 'NONE',  ( 0.000000000000000000, 1.000000000000000000, 0.000000000000000000 ) ) ;
#126950 = CARTESIAN_POINT ( 'NONE',  ( 2.877373901574116211, 1.733520850877915187, -0.5729475677913041798 ) ) ;
#126951 = CARTESIAN_POINT ( 'NONE',  ( -4.298098390732130625, 4.973201863064262263, 1.199719254218462483 ) ) ;
#126952 = CARTESIAN_POINT ( 'NONE',  ( -3.144601563365788444, 5.756120026313656268, -1.199719254218452935 ) ) ;
#126953 = CARTESIAN_POINT ( 'NONE',  ( -5.929989559956849732, 7.234276776666978215, -1.248630897662094563 ) ) ;
#126954 = CARTESIAN_POINT ( 'NONE',  ( 0.000000000000000000, 1.000000000000000888, 0.000000000000000000 ) ) ;
#126955 = CARTESIAN_POINT ( 'NONE',  ( 8.191097360950562845, 12.70803068775103739, -0.7998128361456352531 ) ) ;
#126956 = CARTESIAN_POINT ( 'NONE',  ( 1.312975575179779586, 1.698600376263710743, 0.9089255565387382996 ) ) ;
#126957 = CARTESIAN_POINT ( 'NONE',  ( 5.489096970993415425, 0.1405823987245969631, 1.956747174436481274 ) ) ;
#126958 = CARTESIAN_POINT ( 'NONE',  ( 1.499999999999997113, 15.39583333333333748, -0.8660254037844378194 ) ) ;
#126959 = CARTESIAN_POINT ( 'NONE',  ( -6.093499974338126179, 9.196501505781426999, -1.199719254218440723 ) ) ;
#126960 = CARTESIAN_POINT ( 'NONE',  ( 5.769158057814842699, 6.689438141327490150, 1.199719254218462483 ) ) ;
#126961 = CARTESIAN_POINT ( 'NONE',  ( 4.968408144156593487, -2.063508908063705238, -0.7385586828293493333 ) ) ;
#126962 = CIRCLE ( 'NONE', #116557, 0.4999999999999995559 ) ;
#126963 = TOROIDAL_SURFACE ( 'NONE', #95830, 0.05000000000000000278, 0.05000000000000000278 ) ;
#126964 = CARTESIAN_POINT ( 'NONE',  ( 5.522248639467795428, 5.337044922334209573, -0.7998128361456231517 ) ) ;
#126965 = CARTESIAN_POINT ( 'NONE',  ( 4.153231765667256603, 1.751622898902647663, -1.103220242290925190 ) ) ;
#126967 = CARTESIAN_POINT ( 'NONE',  ( 1.364683531249988535, 1.426041667008083991, 0.7879004041258500513 ) ) ;
#126966 = DIRECTION ( 'NONE',  ( -0.000000000000000000, -1.000000000000000000, -0.000000000000000000 ) ) ;
#126968 = ORIENTED_EDGE ( 'NONE', *, *, #166950, .F. ) ;
#126969 = CARTESIAN_POINT ( 'NONE',  ( 4.272342533241332063, 2.053246469231550630, -1.033699615426456830 ) ) ;
#126971 = ORIENTED_EDGE ( 'NONE', *, *, #95161, .F. ) ;
#126970 = CARTESIAN_POINT ( 'NONE',  ( 6.127922243696800386, 10.09306701771420656, -0.7216878364870267237 ) ) ;
#126973 = CARTESIAN_POINT ( 'NONE',  ( -1.642778471875000035, -0.5177083328553738761, -2.845375778867859751 ) ) ;
#126972 = CARTESIAN_POINT ( 'NONE',  ( 4.529832720741620022, 7.338536369956936589, -1.082531754730548412 ) ) ;
#126974 = CARTESIAN_POINT ( 'NONE',  ( -7.547231044119362409, -5.251137252134767230, -7.967649405165816212 ) ) ;
#126975 = DIRECTION ( 'NONE',  ( 0.000000000000000000, 1.000000000000000000, -3.330669073875479482E-16 ) ) ;
#126976 = CARTESIAN_POINT ( 'NONE',  ( 3.943253339372253308, 0.6530871051511869529, -1.828966769512891277 ) ) ;
#126977 = VERTEX_POINT ( 'NONE', #180269 ) ;
#126978 = CARTESIAN_POINT ( 'NONE',  ( 9.531018800282605952, 11.18223869082697597, 1.082531754730548412 ) ) ;
#126979 = ADVANCED_FACE ( 'NONE', ( #31893 ), #5734, .T. ) ;
#126980 = ORIENTED_EDGE ( 'NONE', *, *, #141538, .T. ) ;
#126981 = CARTESIAN_POINT ( 'NONE',  ( 4.974826827724895928, -1.381046924789817831, 1.323090558688621909 ) ) ;
#126982 = CARTESIAN_POINT ( 'NONE',  ( 6.704117942027653321, -1.724248281341285827, 0.04880198193529976941 ) ) ;
#126983 = CARTESIAN_POINT ( 'NONE',  ( 4.891814693739657827, -2.006371927678828104, 0.2024599332275459629 ) ) ;
#126984 = CARTESIAN_POINT ( 'NONE',  ( -2.065088895208807340, 8.523968132013855836, 2.459875961809343092 ) ) ;
#126985 = CARTESIAN_POINT ( 'NONE',  ( 1.418904949497600487, 1.480075412272121582, -1.637148382315711359 ) ) ;
#126987 = DIRECTION ( 'NONE',  ( 5.578564026256490882E-16, 1.000000000000000000, 9.066213480720158442E-32 ) ) ;
#126986 = CARTESIAN_POINT ( 'NONE',  ( -3.894504475113999664, 7.459775595827967898, -0.4024148884765280654 ) ) ;
#126989 = CARTESIAN_POINT ( 'NONE',  ( 6.925078400183545035, 0.003529629153843985134, 1.755452343125718073 ) ) ;
#126988 = CARTESIAN_POINT ( 'NONE',  ( 1.447338344653009701, 0.6056102050338266762, -2.000996673686726179 ) ) ;
#126990 = CARTESIAN_POINT ( 'NONE',  ( 5.660779783930850684, 1.203351582566011047, 1.617819807990819481 ) ) ;
#126992 = CARTESIAN_POINT ( 'NONE',  ( 3.047136720273002641, -1.874302040764055599, -1.319397901421492714 ) ) ;
#126991 = CARTESIAN_POINT ( 'NONE',  ( 4.549643065837591038, 7.465611455855944101, -1.199719254218452047 ) ) ;
#126993 = CARTESIAN_POINT ( 'NONE',  ( 1.411604581429444893, 1.170971978790593448, -1.287647580301202410 ) ) ;
#126994 = CARTESIAN_POINT ( 'NONE',  ( 2.619513681940002670, 1.793805257907291395, 1.130712135851599465 ) ) ;
#126995 = CARTESIAN_POINT ( 'NONE',  ( 11.84668729035180590, 11.00518580017410386, -1.400000000000001688 ) ) ;
#126996 = CARTESIAN_POINT ( 'NONE',  ( 1.580929310206186100, 1.169321551402967119, -1.280364243709716243 ) ) ;
#126997 = CARTESIAN_POINT ( 'NONE',  ( -1.360316468750038643, 1.192708333674735721, 0.7853790794158880262 ) ) ;
#126998 = CARTESIAN_POINT ( 'NONE',  ( 2.224856516622634395, -1.700045390792026989, -0.7576570785256631080 ) ) ;
#126999 = CARTESIAN_POINT ( 'NONE',  ( 1.715514515588032030, -1.861668902569445283, -1.117036959414873465 ) ) ;
#127000 = CARTESIAN_POINT ( 'NONE',  ( 2.923064838257955156, -1.776166165677966591, 0.9548571111624851726 ) ) ;
#127002 = CIRCLE ( 'NONE', #137286, 6.249999999999995559 ) ;
#127001 = CARTESIAN_POINT ( 'NONE',  ( 4.968750000000002665, 0.7852924748297213098, -1.895863743164188042 ) ) ;
#127003 = CARTESIAN_POINT ( 'NONE',  ( 0.7499999999999885647, 1.847916667349486231, -1.299038105676652899 ) ) ;
#127004 = CARTESIAN_POINT ( 'NONE',  ( 6.428350398238483088, 1.106843121268024976, -1.576624894639609309 ) ) ;
#127005 = CARTESIAN_POINT ( 'NONE',  ( -0.6823417656250039265, 13.56770833367473195, -1.181850606188755259 ) ) ;
#127006 = CARTESIAN_POINT ( 'NONE',  ( 3.551236150222897958, 0.3290391446359001715, 2.196816492004387111 ) ) ;
#127007 = ORIENTED_EDGE ( 'NONE', *, *, #147272, .F. ) ;
#127008 = CARTESIAN_POINT ( 'NONE',  ( 6.663994888585877518, -7.154544010627095219, -6.770610912236881163 ) ) ;
#127009 = CARTESIAN_POINT ( 'NONE',  ( -1.500000000000015099, -0.8291666666666407393, 0.8660254037844403729 ) ) ;
#127010 = CARTESIAN_POINT ( 'NONE',  ( 8.911787042884274257, 9.291506392986812912, 0.7998128361456462443 ) ) ;
#127011 = CARTESIAN_POINT ( 'NONE',  ( -1.364683531250014514, -0.2197916663252438285, 0.7879004041258379498 ) ) ;
#127012 = CARTESIAN_POINT ( 'NONE',  ( 6.075711799444424521, -0.9231013878284710650, 1.475285791177717076 ) ) ;
#127013 = CARTESIAN_POINT ( 'NONE',  ( 4.193769882565239193, -1.351282707657221582, -1.422545440481419510 ) ) ;
#127015 = CARTESIAN_POINT ( 'NONE',  ( -5.422898255786186006, 9.270539031818461950, -0.7216878364870207285 ) ) ;
#127014 = CARTESIAN_POINT ( 'NONE',  ( 8.581948047770334043, 12.95609712246668899, 0.000000000000000000 ) ) ;
#127016 = CARTESIAN_POINT ( 'NONE',  ( -1.400363088670474765, 4.350706060076355186, 0.06128031220415256636 ) ) ;
#127017 = CARTESIAN_POINT ( 'NONE',  ( 5.975896723952917711, 1.340560379189212226, 1.822362705929107429 ) ) ;
#127018 = CARTESIAN_POINT ( 'NONE',  ( 2.418490130824833440, 0.8798743164511336756, 1.865715637115851866 ) ) ;
#127019 = CARTESIAN_POINT ( 'NONE',  ( -6.018930129462987999, 9.109503353427070849, 1.199719254218452047 ) ) ;
#127020 = VERTEX_POINT ( 'NONE', #69682 ) ;
#127021 = CARTESIAN_POINT ( 'NONE',  ( -1.500000000000001332, 1.431250000682816825, 0.000000000000000000 ) ) ;
#127022 = CARTESIAN_POINT ( 'NONE',  ( 3.848780967690920374, -1.530814235938406931, 1.074699354247290017 ) ) ;
#127023 = CARTESIAN_POINT ( 'NONE',  ( 2.971044740931504613, -1.708945904174772989, -0.2933555621278273184 ) ) ;
#127024 = ADVANCED_FACE ( 'NONE', ( #185575 ), #136855, .T. ) ;
#127025 = CARTESIAN_POINT ( 'NONE',  ( 0.1876184131640425135, 1.704306722208508873, 1.533282888375518960 ) ) ;
#127026 = CARTESIAN_POINT ( 'NONE',  ( 0.6400319944965120467, -1.562016764346199960, -1.559085968200937256 ) ) ;
#127027 = CARTESIAN_POINT ( 'NONE',  ( 3.590839768554392908, -0.4196827604958653923, -2.120402733634827452 ) ) ;
#127028 = CARTESIAN_POINT ( 'NONE',  ( 5.173749199105643903, -1.077276334994947460, 1.615559063095718839 ) ) ;
#127029 = CIRCLE ( 'NONE', #161434, 4.021913119055696484 ) ;
#127030 = CARTESIAN_POINT ( 'NONE',  ( 8.347919278768385354, 15.09740922415466358, 8.560103915482137893 ) ) ;
#127031 = EDGE_CURVE ( 'NONE', #8301, #75305, #213275, .T. ) ;
#127032 = DIRECTION ( 'NONE',  ( 0.000000000000000000, 0.000000000000000000, 1.000000000000000000 ) ) ;
#127033 = CARTESIAN_POINT ( 'NONE',  ( 6.029922689959810178, -1.701949372586025744, 1.081063231324945528 ) ) ;
#127034 = CARTESIAN_POINT ( 'NONE',  ( -7.641992139597101108, 12.06740792950531649, 0.7998128361456481317 ) ) ;
#127035 = CARTESIAN_POINT ( 'NONE',  ( 6.096362627639171805, 10.26417349888772179, -0.7998128361456291469 ) ) ;
#127036 = CARTESIAN_POINT ( 'NONE',  ( 0.4999999999999987232, 3.999999999999996447, -0.4499999999999972911 ) ) ;
#127037 = CARTESIAN_POINT ( 'NONE',  ( 3.281694405262673087, 1.158851912627656189, 1.410738560442346801 ) ) ;
#127038 = CARTESIAN_POINT ( 'NONE',  ( 1.677102584378454608, -2.095606157416990190, -0.6917391671936305997 ) ) ;
#127039 = ORIENTED_EDGE ( 'NONE', *, *, #198453, .F. ) ;
#127040 = CARTESIAN_POINT ( 'NONE',  ( -5.004368096775595021, 5.971422546727199077, 1.082531754730549078 ) ) ;
#127041 = CARTESIAN_POINT ( 'NONE',  ( 1.001543065824772753E-15, -3.259374999522042682, 3.793834371823811669 ) ) ;
#127042 = CARTESIAN_POINT ( 'NONE',  ( -7.426115451983156923, 9.686887332112256388, -1.599625672291263179 ) ) ;
#127043 = CARTESIAN_POINT ( 'NONE',  ( 1.511979465466501527, -0.6765842426028411127, 1.903255196800458071 ) ) ;
#127044 = CARTESIAN_POINT ( 'NONE',  ( 1.401209248766785542, -0.3145075555085960484, -2.096923750572597722 ) ) ;
#127045 = CARTESIAN_POINT ( 'NONE',  ( -1.264911064067349100, 3.883875966818681302, 0.5000000000000055511 ) ) ;
#127046 = EDGE_LOOP ( 'NONE', ( #196150, #65528, #3326, #22359 ) ) ;
#127047 = CARTESIAN_POINT ( 'NONE',  ( -5.635349125135588721, 6.603604063193491136, 1.199719254218452935 ) ) ;
#127048 = CARTESIAN_POINT ( 'NONE',  ( 2.025991663365491746, 0.9512761431412205537, 1.599265494891942030 ) ) ;
#127049 = CARTESIAN_POINT ( 'NONE',  ( 5.203632029546647608, 4.965325544092860532, 1.040834085586084257E-14 ) ) ;
#127050 = CARTESIAN_POINT ( 'NONE',  ( 0.9894095316701527754, 1.906041449620498929, -1.019753361306941386 ) ) ;
#127051 = CARTESIAN_POINT ( 'NONE',  ( 5.713517581197447015, 1.944070655204039433, 0.5350908816983344085 ) ) ;
#127052 = ORIENTED_EDGE ( 'NONE', *, *, #58359, .T. ) ;
#127053 = ORIENTED_EDGE ( 'NONE', *, *, #161821, .T. ) ;
#127054 = FACE_BOUND ( 'NONE', #33263, .T. ) ;
#127055 = CARTESIAN_POINT ( 'NONE',  ( 4.512205841073367196, -0.7830535718562798841, -1.649371741558727678 ) ) ;
#127058 = ORIENTED_EDGE ( 'NONE', *, *, #103355, .F. ) ;
#127057 = CARTESIAN_POINT ( 'NONE',  ( -4.922147708203060468, 6.858988491581952118, -1.449652397630277756 ) ) ;
#127056 = CARTESIAN_POINT ( 'NONE',  ( -4.308458954092677651, 8.248562223075252220, -0.7998128361456362523 ) ) ;
#127059 = CARTESIAN_POINT ( 'NONE',  ( 6.425920342564602983, 6.885296541689900351, -0.7293792964763821107 ) ) ;
#127060 = CARTESIAN_POINT ( 'NONE',  ( 6.186875009713125984, -1.117664052418202658, -1.677746505241828334 ) ) ;
#127061 = CARTESIAN_POINT ( 'NONE',  ( 5.331922971087851515, 1.814509544241477146, 0.3110680438872318043 ) ) ;
#127062 = CARTESIAN_POINT ( 'NONE',  ( -0.02299388927992032997, 1.367829385570513923, -2.164798317653505944 ) ) ;
#127063 = CARTESIAN_POINT ( 'NONE',  ( 4.020403473283917783, -1.184823721361260018, -1.980193191683382148 ) ) ;
#127064 = CARTESIAN_POINT ( 'NONE',  ( 6.099189001301251523, 8.209082816308541197, 1.599625672291268286 ) ) ;
#127065 = CARTESIAN_POINT ( 'NONE',  ( 5.835289683280778128, -1.956920075724715602, 0.9183947573421016308 ) ) ;
#127066 = CARTESIAN_POINT ( 'NONE',  ( 1.786567547031367775, 1.688677558619257058, -0.9590575663266877049 ) ) ;
#127067 = CARTESIAN_POINT ( 'NONE',  ( 4.604990120689349098, 0.9883660700816098155, -2.075160223314168828 ) ) ;
#127068 = CARTESIAN_POINT ( 'NONE',  ( -0.3000000000000085931, 3.372708439410163184, 0.4999999999999657496 ) ) ;
#127069 = CARTESIAN_POINT ( 'NONE',  ( -5.901542003698421190, 10.10715911428198055, 0.000000000000000000 ) ) ;
#127070 = EDGE_CURVE ( 'NONE', #59550, #153466, #126962, .T. ) ;
#127071 = CARTESIAN_POINT ( 'NONE',  ( 4.434354141042872399, 1.834536173243521917, 0.3649259964926266364 ) ) ;
#127072 = ORIENTED_EDGE ( 'NONE', *, *, #129019, .F. ) ;
#127073 =( BOUNDED_CURVE ( )  B_SPLINE_CURVE ( 3, ( #53542, #71900, #153177, #119674 ),
 .UNSPECIFIED., .F., .T. ) 
 B_SPLINE_CURVE_WITH_KNOTS ( ( 4, 4 ),
 ( 1.570796326794896114, 2.200856270471019283 ),
 .UNSPECIFIED. ) 
 CURVE ( )  GEOMETRIC_REPRESENTATION_ITEM ( )  RATIONAL_B_SPLINE_CURVE ( ( 1.000000000000000000, 0.9671913951452630887, 0.9671913951452630887, 1.000000000000000000 ) ) 
 REPRESENTATION_ITEM ( '' )  );
#127076 = CARTESIAN_POINT ( 'NONE',  ( -6.120580001926503755, 6.105374521861167914, -0.7998128361456362523 ) ) ;
#127075 = CARTESIAN_POINT ( 'NONE',  ( -1.402160292154681736E-14, 0.3687500006828169363, -1.732050807568870754 ) ) ;
#127074 = CARTESIAN_POINT ( 'NONE',  ( 2.513799616133075343, -0.5961229146635020903, 1.817204401178821760 ) ) ;
#127077 = CARTESIAN_POINT ( 'NONE',  ( 4.301547675229603129, 1.771612934706376707, 1.315755017190944676 ) ) ;
#127078 = CARTESIAN_POINT ( 'NONE',  ( -1.598423149421388523, 8.713846000020799565, -2.500000000000119016 ) ) ;
#127079 = CARTESIAN_POINT ( 'NONE',  ( 4.977251789548238214, 7.860525283564661514, -1.082531754730548412 ) ) ;
#127080 = CARTESIAN_POINT ( 'NONE',  ( -5.058600711230246461, 7.955432358860325515, 1.082531754730549967 ) ) ;
#127081 = CARTESIAN_POINT ( 'NONE',  ( 1.405477211469996934, -0.4828617686813937993, 1.911177332403845464 ) ) ;
#127082 = CARTESIAN_POINT ( 'NONE',  ( 1.273011573350724568, -1.461848840328241694, 1.785463964174689000 ) ) ;
#127083 = CARTESIAN_POINT ( 'NONE',  ( 3.016010921186715432, 1.952665002612500533, -0.1895750030070641190 ) ) ;
#127084 = DIRECTION ( 'NONE',  ( -0.1674078377062507283, 3.252606517456525293E-14, 0.9858877298529065136 ) ) ;
#127085 = CARTESIAN_POINT ( 'NONE',  ( 6.350444629809289587, -2.052082384739264409, -0.2080662788188895607 ) ) ;
#127086 = CARTESIAN_POINT ( 'NONE',  ( 4.121315508874254796, 5.831287398485176077, -1.443375672974051449 ) ) ;
#127087 = CARTESIAN_POINT ( 'NONE',  ( 4.118375227313908482, 1.978554835517082555, 0.3886342876525810119 ) ) ;
#127088 = CARTESIAN_POINT ( 'NONE',  ( 4.797606254389322089, 6.690569611577942943, 1.599625672291268286 ) ) ;
#127089 = VERTEX_POINT ( 'NONE', #68613 ) ;
#127090 = CARTESIAN_POINT ( 'NONE',  ( -9.541187415715041809, 12.15447128979948310, -1.599625672291263179 ) ) ;
#127091 =( BOUNDED_SURFACE ( )  B_SPLINE_SURFACE ( 1, 2, ( 
 ( #54967, #187084, #38717, #200120, #116813, #51774, #104797, #84255, #170844, #167642, #135167, #1909, #22434, #182814, #85323, #151406, #201183, #67968, #134111, #117892, #183884, #35496, #101574, #52821, #156747, #190283, #154606, #27796, #157814, #8337, #74422, #91760, #89618, #6185, #140522, #41940, #138361, #208658, #125378, #189230, #26722, #204379, #109120, #76538, #172999, #23513, #24580, #206535, #126448, #9412, #108053, #123266, #58165, #72254, #174077, #142649, #110184, #25649, #124323, #40869, #56035, #75483, #43008, #122188, #155671, #191342, #192411, #92823, #175135, #188154, #141594, #60289, #7253, #90687, #158868, #10464, #207601, #39786, #44066, #59220, #176195, #57099, #73329, #105892, #106974, #171917, #139431, #205466, #209724, #31014, #146906, #63497, #210801, #94953, #62424, #193497, #181493, #197742, #177254, #127526, #64560, #212925, #194555, #93894, #11536, #47271, #32061, #147955, #28866, #161001, #128589, #178331, #180445, #130704, #213968, #77606, #49380, #46198, #81870, #65588, #12595, #196695, #211860, #48335, #114445, #112316, #159933, #143730, #113385, #98148, #131736, #78668, #144794, #29939, #96024, #164197, #15784, #115498, #61368, #45139, #162076, #111251, #13665, #79737, #145853, #129652, #195637, #179394, #97088, #163141, #14724, #80815, #185743, #52563, #17905, #82926, #83991, #119764, #116558, #153262, #199866, #101308, #132786, #36301, #102378, #51509, #117634, #183625, #134908, #103452, #69848, #168447, #151147, #120848, #148999, #35233, #68789, #33122, #99201, #20046, #167389, #18979, #184679, #182551, #165251, #85062, #200915, #16844, #87198, #3773, #67708, #37377, #576, #201974, #169512, #2716, #34175, #118694, #86133, #4837, #152205, #135959, #1650, #53631, #66642, #21094, #70916, #203053, #137026, #54697, #133857, #198789, #50438, #100247, #166315, #150078, #157554, #158612, #125124, #9149, #88271, #172732, #108855, #39514, #56834, #191083, #42751, #173817, #22156, #174881, #188960, #75224, #89352, #55762, #8073, #155401, #40601, #140253, #141336, #154338, #124063, #25395, #156484, #6984, #187886, #73064, #71988, #60034, #76284, #121918, #5914, #139163, #26461, #90414, #57898, #206275, #190028, #38449, #41680, #91494, #106707, #186821, #104529, #207350, #170574, #58970, #205193, #123005, #138099, #24309, #74159, #107791, #92570, #10210, #142392, #208401, #204110, #105613, #171643, #23240, #126187, #194302, #210545, #127264, #78416, #31818, #193235, #176993, #143464, #211600, #163954, #80555, #96835, #160740, #178065, #45945, #15531, #209461, #12335, #64308, #27533, #61105, #159671, #29683, #110988, #146653, #161822, #130454, #212667, #43814, #162884, #147700, #192150, #97894, #93629, #129399, #44883, #113126, #81616, #196442, #14464, #13410, #213718, #179131, #112065, #48086, #128338, #114199, #180197, #144536, #95767, #195378, #28610, #11273, #109927, #79486, #145605, #63236, #47010, #77351, #94700, #175938, #62180, #30755, #185506, #165001, #101057, #329, #1404, #33930, #119518, #118452, #151964, #183381, #50191, #52323, #169270, #68542, #66400, #134671, #65341, #16593, #82675, #69609, #148759, #115252, #37129, #98947, #36056, #49135, #200674, #184439, #85888, #103208, #86955, #102137, #132546, #131489, #198545, #20856, #2466, #3536, #84816, #116311, #181243, #182302, #135716, #100005, #153023, #17659, #133611, #166071, #168205, #19804, #83742, #149835, #67465, #167146, #201742, #53383, #197494, #34987, #32871, #199615, #51260, #18733, #117384, #150905, #7818, #6747, #72825, #156241, #154095, #4598, #138928, #40357, #202811, #58722, #189781, #39271, #91245, #54460, #173574, #141084, #22993, #88023, #89110, #204945, #190838, #73911, #106461, #187643, #56596, #136782, #24072, #207094, #174634, #172485, #122758, #105365, #120603, #90178, #107540, #186580, #5664, #41432, #42499, #157305, #25143, #38209, #188719, #124873, #71743, #155164, #8895, #74975, #206025, #104282, #108606, #140004, #26210, #121678, #137858, #57663, #171402, #123821, #92328, #70672, #170327, #21914, #203878, #55523, #60851, #159419, #127014, #43563, #31565, #47835, #27275, #191901, #129148 ),
 ( #130198, #179941, #62979, #109683, #9962, #175686, #44625, #162631, #61926, #29431, #177815, #95522, #76039, #161572, #176740, #28354, #94449, #45695, #14206, #195124, #13159, #128085, #158369, #59786, #160488, #194042, #142142, #208156, #79236, #12095, #78163, #145354, #93382, #125945, #144293, #111810, #11019, #212412, #46762, #192973, #30502, #77094, #112873, #80301, #210286, #143221, #211355, #178888, #196192, #96583, #146398, #110740, #64055, #209211, #113946, #19547, #53124, #51002, #149567, #132285, #147446, #117122, #200421, #213470, #98689, #68285, #69348, #35802, #134417, #65093, #83484, #85625, #164746, #182041, #101880, #167946, #84558, #131250, #151712, #99747, #52068, #75, #180992, #133348, #66140, #165817, #183125, #118194, #197237, #34731, #150647, #67213, #198290, #16338, #49932, #48876, #185242, #201482, #32612, #114994, #184182, #2208, #116053, #97640, #15279, #100803, #3281, #135459, #82419, #148508, #33672, #17400, #119257, #163697, #81366, #1150, #199354, #166889, #18479, #159968, #120338, #158904, #157850, #126482, #86692, #71485, #10500, #209759, #191378, #192446, #59254, #21654, #152761, #87761, #44101, #186314, #11573, #203615, #105099, #136528, #43044, #77643, #20606, #61400, #55267, #27831, #143765, #37949, #76573, #9444, #110221, #4343, #137598, #142685, #127563, #109157, #176229, #125412, #153837, #70410, #5407, #93927, #104021, #36864, #121414, #171140, #202548, #175169, #26756, #187386, #39017, #22732, #141627, #102948, #208695, #92857, #75515, #169008, #54198, #88848, #207636, #170068, #60322, #196731, #195673, #47309, #130738, #128625, #193532, #113423, #14763, #177292, #33159, #164233, #13702, #65626, #28906, #147994, #115536, #211898, #62463, #63535, #179429, #165289, #48372, #80853, #162112, #31050, #111286, #212959, #181531, #149038, #146944, #97126, #79775, #94991, #64597, #81906, #161037, #194592, #15821, #16883, #131775, #214004, #12632, #163178, #99240, #46236, #129690, #197778, #49416, #180481, #78703, #82965, #114484, #613, #96059, #112353, #32100, #145887, #98185, #66681, #45174, #144829, #210837, #178366, #29974, #35272, #133898, #101350, #17945, #5957, #22203, #1694, #166355, #103494, #185784, #19021, #132828, #50477, #86174, #70959, #186863, #67748, #199905, #167429, #2758, #4880, #37418, #203094, #134949, #21137, #85101, #51551, #168487, #151186, #200956, #152244, #169555, #34215, #69888, #87240, #102419, #68827, #117676, #52604, #84032, #198832, #88316, #183669, #150121, #153305, #137069, #118733, #116598, #182592, #3817, #54739, #38493, #184717, #36341, #20086, #136001, #120889, #104571, #170616, #100288, #154380, #202014, #53673, #119805, #155442, #191124, #190069, #158652, #121959, #106748, #42790, #27573, #9192, #10250, #91538, #56875, #187926, #123051, #76326, #7027, #192191, #24349, #140298, #171685, #75263, #141377, #90459, #156525, #8116, #173856, #142432, #108899, #207388, #41721, #159714, #39556, #74204, #107831, #72028, #138140, #59009, #206317, #57941, #125165, #73103, #204149, #124106, #25432, #55805, #126230, #174922, #172775, #208440, #105657, #26502, #60074, #157597, #139204, #92609, #43855, #109969, #175980, #93671, #40645, #23282, #89394, #205234, #189002, #181283, #179173, #63278, #45985, #61143, #30797, #114238, #127305, #12377, #196484, #197530, #163993, #48126, #193276, #211643, #147742, #78457, #95807, #15568, #81655, #212710, #44921, #129440, #210589, #180236, #47053, #213758, #97935, #143506, #31860, #32910, #77390, #131527, #111029, #14507, #144575, #64351, #115292, #65381, #49175, #113169, #98987, #130497, #145647, #11312, #13453, #209503, #177034, #29725, #195423, #80598, #62219, #28651, #94738, #96876, #162926, #146694, #160784, #128376, #194344, #112106, #178109, #161863, #79529, #50228, #200709, #100043, #101093, #133650, #4632, #3570, #37167, #68578, #149871, #151999, #54493, #168240, #166106, #19839, #165040, #116348, #182338, #169305, #33966, #364, #70704, #198582, #135753, #148794, #85925, #69644, #185539, #136817, #186615, #201776, #17692, #16633, #83779, #51296, #20890, #134704, #36089, #184472, #102173, #82717, #53416 ) ),
 .UNSPECIFIED., .F., .F., .F. ) 
 B_SPLINE_SURFACE_WITH_KNOTS ( ( 2, 2 ),
 ( 3, 2, 2, 2, 2, 2, 2, 2, 2, 2, 2, 2, 2, 2, 2, 2, 2, 2, 2, 2, 2, 2, 2, 2, 2, 2, 2, 2, 2, 2, 2, 2, 2, 2, 2, 2, 2, 2, 2, 2, 2, 2, 2, 2, 2, 2, 2, 2, 2, 2, 2, 2, 2, 2, 2, 2, 2, 2, 2, 2, 2, 2, 2, 2, 2, 2, 2, 2, 2, 2, 2, 2, 2, 2, 2, 2, 2, 2, 2, 2, 2, 2, 2, 2, 2, 2, 2, 2, 2, 2, 2, 2, 2, 2, 2, 2, 2, 2, 2, 2, 2, 2, 2, 2, 2, 2, 2, 2, 2, 2, 2, 2, 2, 2, 2, 2, 2, 2, 2, 2, 2, 2, 2, 2, 2, 2, 2, 2, 2, 2, 2, 2, 2, 2, 2, 2, 2, 2, 2, 2, 2, 2, 2, 2, 2, 2, 2, 2, 2, 2, 2, 2, 2, 2, 2, 2, 2, 2, 2, 2, 2, 2, 2, 2, 2, 2, 2, 2, 2, 2, 2, 2, 2, 2, 2, 2, 2, 2, 2, 2, 2, 2, 2, 2, 2, 2, 2, 2, 2, 2, 2, 2, 2, 2, 2, 2, 2, 2, 2, 2, 2, 2, 2, 2, 2, 2, 2, 2, 2, 2, 2, 2, 2, 2, 2, 2, 2, 2, 2, 2, 2, 2, 2, 2, 2, 2, 2, 2, 2, 2, 2, 2, 2, 2, 2, 2, 2, 2, 2, 2, 3 ),
 ( 0.000000000000000000, 1.000000000000000000 ),
 ( 0.000000000000000000, 0.004166666666666666609, 0.008333333333333333218, 0.01250000000000000069, 0.01666666666666666644, 0.02083333333333333218, 0.02500000000000000139, 0.02916666666666666713, 0.03333333333333333287, 0.03749999999999999861, 0.04166666666666666435, 0.04583333333333333010, 0.05000000000000000278, 0.05416666666666666852, 0.05833333333333333426, 0.06250000000000000000, 0.06666666666666666574, 0.07083333333333333148, 0.07499999999999999722, 0.07916666666666666297, 0.08333333333333332871, 0.08749999999999999445, 0.09166666666666666019, 0.09583333333333333981, 0.1000000000000000056, 0.1041666666666666713, 0.1083333333333333370, 0.1125000000000000028, 0.1166666666666666685, 0.1208333333333333343, 0.1250000000000000000, 0.1291666666666666796, 0.1333333333333333315, 0.1375000000000000111, 0.1416666666666666630, 0.1458333333333333426, 0.1499999999999999944, 0.1541666666666666741, 0.1583333333333333259, 0.1625000000000000056, 0.1666666666666666574, 0.1708333333333333370, 0.1749999999999999889, 0.1791666666666666685, 0.1833333333333333204, 0.1875000000000000000, 0.1916666666666666796, 0.1958333333333333315, 0.2000000000000000111, 0.2041666666666666630, 0.2083333333333333426, 0.2124999999999999944, 0.2166666666666666741, 0.2208333333333333259, 0.2250000000000000056, 0.2291666666666666574, 0.2333333333333333370, 0.2374999999999999889, 0.2416666666666666685, 0.2458333333333333204, 0.2500000000000000000, 0.2541666666666666519, 0.2583333333333333592, 0.2625000000000000111, 0.2666666666666666630, 0.2708333333333333148, 0.2750000000000000222, 0.2791666666666666741, 0.2833333333333333259, 0.2874999999999999778, 0.2916666666666666852, 0.2958333333333333370, 0.2999999999999999889, 0.3041666666666666408, 0.3083333333333333481, 0.3125000000000000000, 0.3166666666666666519, 0.3208333333333333592, 0.3250000000000000111, 0.3291666666666666630, 0.3333333333333333148, 0.3375000000000000222, 0.3416666666666666741, 0.3458333333333333259, 0.3499999999999999778, 0.3541666666666666852, 0.3583333333333333370, 0.3624999999999999889, 0.3666666666666666408, 0.3708333333333333481, 0.3750000000000000000, 0.3791666666666666519, 0.3833333333333333592, 0.3875000000000000111, 0.3916666666666666630, 0.3958333333333333148, 0.4000000000000000222, 0.4041666666666666741, 0.4083333333333333259, 0.4124999999999999778, 0.4166666666666666852, 0.4208333333333333370, 0.4249999999999999889, 0.4291666666666666408, 0.4333333333333333481, 0.4375000000000000000, 0.4416666666666666519, 0.4458333333333333592, 0.4500000000000000111, 0.4541666666666666630, 0.4583333333333333148, 0.4625000000000000222, 0.4666666666666666741, 0.4708333333333333259, 0.4749999999999999778, 0.4791666666666666852, 0.4833333333333333370, 0.4874999999999999889, 0.4916666666666666408, 0.4958333333333333481, 0.5000000000000000000, 0.5041666666666666519, 0.5083333333333333037, 0.5124999999999999556, 0.5166666666666667185, 0.5208333333333333703, 0.5250000000000000222, 0.5291666666666666741, 0.5333333333333333259, 0.5374999999999999778, 0.5416666666666666297, 0.5458333333333332815, 0.5500000000000000444, 0.5541666666666666963, 0.5583333333333333481, 0.5625000000000000000, 0.5666666666666666519, 0.5708333333333333037, 0.5749999999999999556, 0.5791666666666667185, 0.5833333333333333703, 0.5875000000000000222, 0.5916666666666666741, 0.5958333333333333259, 0.5999999999999999778, 0.6041666666666666297, 0.6083333333333332815, 0.6125000000000000444, 0.6166666666666666963, 0.6208333333333333481, 0.6250000000000000000, 0.6291666666666666519, 0.6333333333333333037, 0.6374999999999999556, 0.6416666666666667185, 0.6458333333333333703, 0.6500000000000000222, 0.6541666666666666741, 0.6583333333333333259, 0.6624999999999999778, 0.6666666666666666297, 0.6708333333333332815, 0.6750000000000000444, 0.6791666666666666963, 0.6833333333333333481, 0.6875000000000000000, 0.6916666666666666519, 0.6958333333333333037, 0.6999999999999999556, 0.7041666666666667185, 0.7083333333333333703, 0.7125000000000000222, 0.7166666666666666741, 0.7208333333333333259, 0.7249999999999999778, 0.7291666666666666297, 0.7333333333333332815, 0.7375000000000000444, 0.7416666666666666963, 0.7458333333333333481, 0.7500000000000000000, 0.7541666666666666519, 0.7583333333333333037, 0.7624999999999999556, 0.7666666666666667185, 0.7708333333333333703, 0.7750000000000000222, 0.7791666666666666741, 0.7833333333333333259, 0.7874999999999999778, 0.7916666666666666297, 0.7958333333333332815, 0.8000000000000000444, 0.8041666666666666963, 0.8083333333333333481, 0.8125000000000000000, 0.8166666666666666519, 0.8208333333333333037, 0.8249999999999999556, 0.8291666666666667185, 0.8333333333333333703, 0.8375000000000000222, 0.8416666666666666741, 0.8458333333333333259, 0.8499999999999999778, 0.8541666666666666297, 0.8583333333333332815, 0.8625000000000000444, 0.8666666666666666963, 0.8708333333333333481, 0.8750000000000000000, 0.8791666666666666519, 0.8833333333333333037, 0.8874999999999999556, 0.8916666666666667185, 0.8958333333333333703, 0.9000000000000000222, 0.9041666666666666741, 0.9083333333333333259, 0.9124999999999999778, 0.9166666666666666297, 0.9208333333333332815, 0.9250000000000000444, 0.9291666666666666963, 0.9333333333333333481, 0.9375000000000000000, 0.9416666666666666519, 0.9458333333333333037, 0.9499999999999999556, 0.9541666666666667185, 0.9583333333333333703, 0.9625000000000000222, 0.9666666666666666741, 0.9708333333333333259, 0.9749999999999999778, 0.9791666666666666297, 0.9833333333333332815, 0.9875000000000000444, 0.9916666666666666963, 0.9958333333333333481, 1.000000000000000000 ),
 .UNSPECIFIED. ) 
 GEOMETRIC_REPRESENTATION_ITEM ( )  RATIONAL_B_SPLINE_SURFACE ( (
 ( 1.000000000000000000, 0.8660254037844387076, 1.000000000000000000, 0.8660254037844387076, 1.000000000000000000, 0.8660254037844387076, 1.000000000000000000, 0.8660254037844387076, 1.000000000000000000, 0.8660254037844387076, 1.000000000000000000, 0.8660254037844387076, 1.000000000000000000, 0.8660254037844387076, 1.000000000000000000, 0.8660254037844387076, 1.000000000000000000, 0.8660254037844387076, 1.000000000000000000, 0.8660254037844387076, 1.000000000000000000, 0.8660254037844387076, 1.000000000000000000, 0.8660254037844387076, 1.000000000000000000, 0.8660254037844387076, 1.000000000000000000, 0.8660254037844387076, 1.000000000000000000, 0.8660254037844387076, 1.000000000000000000, 0.8660254037844387076, 1.000000000000000000, 0.8660254037844387076, 1.000000000000000000, 0.8660254037844387076, 1.000000000000000000, 0.8660254037844387076, 1.000000000000000000, 0.8660254037844387076, 1.000000000000000000, 0.8660254037844387076, 1.000000000000000000, 0.8660254037844387076, 1.000000000000000000, 0.8660254037844387076, 1.000000000000000000, 0.8660254037844387076, 1.000000000000000000, 0.8660254037844387076, 1.000000000000000000, 0.8660254037844387076, 1.000000000000000000, 0.8660254037844387076, 1.000000000000000000, 0.8660254037844387076, 1.000000000000000000, 0.8660254037844387076, 1.000000000000000000, 0.8660254037844387076, 1.000000000000000000, 0.8660254037844387076, 1.000000000000000000, 0.8660254037844387076, 1.000000000000000000, 0.8660254037844387076, 1.000000000000000000, 0.8660254037844387076, 1.000000000000000000, 0.8660254037844387076, 1.000000000000000000, 0.8660254037844387076, 1.000000000000000000, 0.8660254037844387076, 1.000000000000000000, 0.8660254037844387076, 1.000000000000000000, 0.8660254037844387076, 1.000000000000000000, 0.8660254037844387076, 1.000000000000000000, 0.8660254037844387076, 1.000000000000000000, 0.8660254037844387076, 1.000000000000000000, 0.8660254037844387076, 1.000000000000000000, 0.8660254037844387076, 1.000000000000000000, 0.8660254037844387076, 1.000000000000000000, 0.8660254037844387076, 1.000000000000000000, 0.8660254037844387076, 1.000000000000000000, 0.8660254037844387076, 1.000000000000000000, 0.8660254037844387076, 1.000000000000000000, 0.8660254037844387076, 1.000000000000000000, 0.8660254037844387076, 1.000000000000000000, 0.8660254037844387076, 1.000000000000000000, 0.8660254037844387076, 1.000000000000000000, 0.8660254037844387076, 1.000000000000000000, 0.8660254037844387076, 1.000000000000000000, 0.8660254037844387076, 1.000000000000000000, 0.8660254037844387076, 1.000000000000000000, 0.8660254037844387076, 1.000000000000000000, 0.8660254037844387076, 1.000000000000000000, 0.8660254037844387076, 1.000000000000000000, 0.8660254037844387076, 1.000000000000000000, 0.8660254037844387076, 1.000000000000000000, 0.8660254037844387076, 1.000000000000000000, 0.8660254037844387076, 1.000000000000000000, 0.8660254037844387076, 1.000000000000000000, 0.8660254037844387076, 1.000000000000000000, 0.8660254037844387076, 1.000000000000000000, 0.8660254037844387076, 1.000000000000000000, 0.8660254037844387076, 1.000000000000000000, 0.8660254037844387076, 1.000000000000000000, 0.8660254037844387076, 1.000000000000000000, 0.8660254037844387076, 1.000000000000000000, 0.8660254037844387076, 1.000000000000000000, 0.8660254037844387076, 1.000000000000000000, 0.8660254037844387076, 1.000000000000000000, 0.8660254037844387076, 1.000000000000000000, 0.8660254037844387076, 1.000000000000000000, 0.8660254037844387076, 1.000000000000000000, 0.8660254037844387076, 1.000000000000000000, 0.8660254037844387076, 1.000000000000000000, 0.8660254037844387076, 1.000000000000000000, 0.8660254037844387076, 1.000000000000000000, 0.8660254037844387076, 1.000000000000000000, 0.8660254037844387076, 1.000000000000000000, 0.8660254037844387076, 1.000000000000000000, 0.8660254037844387076, 1.000000000000000000, 0.8660254037844387076, 1.000000000000000000, 0.8660254037844387076, 1.000000000000000000, 0.8660254037844387076, 1.000000000000000000, 0.8660254037844387076, 1.000000000000000000, 0.8660254037844387076, 1.000000000000000000, 0.8660254037844387076, 1.000000000000000000, 0.8660254037844387076, 1.000000000000000000, 0.8660254037844387076, 1.000000000000000000, 0.8660254037844387076, 1.000000000000000000, 0.8660254037844387076, 1.000000000000000000, 0.8660254037844387076, 1.000000000000000000, 0.8660254037844387076, 1.000000000000000000, 0.8660254037844387076, 1.000000000000000000, 0.8660254037844387076, 1.000000000000000000, 0.8660254037844387076, 1.000000000000000000, 0.8660254037844387076, 1.000000000000000000, 0.8660254037844387076, 1.000000000000000000, 0.8660254037844387076, 1.000000000000000000, 0.8660254037844387076, 1.000000000000000000, 0.8660254037844387076, 1.000000000000000000, 0.8660254037844387076, 1.000000000000000000, 0.8660254037844387076, 1.000000000000000000, 0.8660254037844387076, 1.000000000000000000, 0.8660254037844387076, 1.000000000000000000, 0.8660254037844387076, 1.000000000000000000, 0.8660254037844387076, 1.000000000000000000, 0.8660254037844387076, 1.000000000000000000, 0.8660254037844387076, 1.000000000000000000, 0.8660254037844387076, 1.000000000000000000, 0.8660254037844387076, 1.000000000000000000, 0.8660254037844387076, 1.000000000000000000, 0.8660254037844387076, 1.000000000000000000, 0.8660254037844387076, 1.000000000000000000, 0.8660254037844387076, 1.000000000000000000, 0.8660254037844387076, 1.000000000000000000, 0.8660254037844387076, 1.000000000000000000, 0.8660254037844387076, 1.000000000000000000, 0.8660254037844387076, 1.000000000000000000, 0.8660254037844387076, 1.000000000000000000, 0.8660254037844387076, 1.000000000000000000, 0.8660254037844387076, 1.000000000000000000, 0.8660254037844387076, 1.000000000000000000, 0.8660254037844387076, 1.000000000000000000, 0.8660254037844387076, 1.000000000000000000, 0.8660254037844387076, 1.000000000000000000, 0.8660254037844387076, 1.000000000000000000, 0.8660254037844387076, 1.000000000000000000, 0.8660254037844387076, 1.000000000000000000, 0.8660254037844387076, 1.000000000000000000, 0.8660254037844387076, 1.000000000000000000, 0.8660254037844387076, 1.000000000000000000, 0.8660254037844387076, 1.000000000000000000, 0.8660254037844387076, 1.000000000000000000, 0.8660254037844387076, 1.000000000000000000, 0.8660254037844387076, 1.000000000000000000, 0.8660254037844387076, 1.000000000000000000, 0.8660254037844387076, 1.000000000000000000, 0.8660254037844387076, 1.000000000000000000, 0.8660254037844387076, 1.000000000000000000, 0.8660254037844387076, 1.000000000000000000, 0.8660254037844387076, 1.000000000000000000, 0.8660254037844387076, 1.000000000000000000, 0.8660254037844387076, 1.000000000000000000, 0.8660254037844387076, 1.000000000000000000, 0.8660254037844387076, 1.000000000000000000, 0.8660254037844387076, 1.000000000000000000, 0.8660254037844387076, 1.000000000000000000, 0.8660254037844387076, 1.000000000000000000, 0.8660254037844387076, 1.000000000000000000, 0.8660254037844387076, 1.000000000000000000, 0.8660254037844387076, 1.000000000000000000, 0.8660254037844387076, 1.000000000000000000, 0.8660254037844387076, 1.000000000000000000, 0.8660254037844387076, 1.000000000000000000, 0.8660254037844387076, 1.000000000000000000, 0.8660254037844387076, 1.000000000000000000, 0.8660254037844387076, 1.000000000000000000, 0.8660254037844387076, 1.000000000000000000, 0.8660254037844387076, 1.000000000000000000, 0.8660254037844387076, 1.000000000000000000, 0.8660254037844387076, 1.000000000000000000, 0.8660254037844387076, 1.000000000000000000, 0.8660254037844387076, 1.000000000000000000, 0.8660254037844387076, 1.000000000000000000, 0.8660254037844387076, 1.000000000000000000, 0.8660254037844387076, 1.000000000000000000, 0.8660254037844387076, 1.000000000000000000, 0.8660254037844387076, 1.000000000000000000, 0.8660254037844387076, 1.000000000000000000, 0.8660254037844387076, 1.000000000000000000, 0.8660254037844387076, 1.000000000000000000, 0.8660254037844387076, 1.000000000000000000, 0.8660254037844387076, 1.000000000000000000, 0.8660254037844387076, 1.000000000000000000, 0.8660254037844387076, 1.000000000000000000, 0.8660254037844387076, 1.000000000000000000, 0.8660254037844387076, 1.000000000000000000, 0.8660254037844387076, 1.000000000000000000, 0.8660254037844387076, 1.000000000000000000, 0.8660254037844387076, 1.000000000000000000, 0.8660254037844387076, 1.000000000000000000, 0.8660254037844387076, 1.000000000000000000, 0.8660254037844387076, 1.000000000000000000, 0.8660254037844387076, 1.000000000000000000, 0.8660254037844387076, 1.000000000000000000, 0.8660254037844387076, 1.000000000000000000, 0.8660254037844387076, 1.000000000000000000, 0.8660254037844387076, 1.000000000000000000, 0.8660254037844387076, 1.000000000000000000, 0.8660254037844387076, 1.000000000000000000, 0.8660254037844387076, 1.000000000000000000, 0.8660254037844387076, 1.000000000000000000, 0.8660254037844387076, 1.000000000000000000, 0.8660254037844387076, 1.000000000000000000, 0.8660254037844387076, 1.000000000000000000, 0.8660254037844387076, 1.000000000000000000, 0.8660254037844387076, 1.000000000000000000, 0.8660254037844387076, 1.000000000000000000, 0.8660254037844387076, 1.000000000000000000, 0.8660254037844387076, 1.000000000000000000, 0.8660254037844387076, 1.000000000000000000, 0.8660254037844387076, 1.000000000000000000, 0.8660254037844387076, 1.000000000000000000, 0.8660254037844387076, 1.000000000000000000, 0.8660254037844387076, 1.000000000000000000, 0.8660254037844387076, 1.000000000000000000, 0.8660254037844387076, 1.000000000000000000, 0.8660254037844387076, 1.000000000000000000, 0.8660254037844387076, 1.000000000000000000, 0.8660254037844387076, 1.000000000000000000, 0.8660254037844387076, 1.000000000000000000, 0.8660254037844387076, 1.000000000000000000, 0.8660254037844387076, 1.000000000000000000, 0.8660254037844387076, 1.000000000000000000, 0.8660254037844387076, 1.000000000000000000, 0.8660254037844387076, 1.000000000000000000, 0.8660254037844387076, 1.000000000000000000, 0.8660254037844387076, 1.000000000000000000, 0.8660254037844387076, 1.000000000000000000, 0.8660254037844387076, 1.000000000000000000, 0.8660254037844387076, 1.000000000000000000, 0.8660254037844387076, 1.000000000000000000, 0.8660254037844387076, 1.000000000000000000, 0.8660254037844387076, 1.000000000000000000, 0.8660254037844387076, 1.000000000000000000, 0.8660254037844387076, 1.000000000000000000, 0.8660254037844387076, 1.000000000000000000, 0.8660254037844387076, 1.000000000000000000, 0.8660254037844387076, 1.000000000000000000, 0.8660254037844387076, 1.000000000000000000, 0.8660254037844387076, 1.000000000000000000, 0.8660254037844387076, 1.000000000000000000, 0.8660254037844387076, 1.000000000000000000, 0.8660254037844387076, 1.000000000000000000),
 ( 1.000000000000000000, 0.8660254037844387076, 1.000000000000000000, 0.8660254037844387076, 1.000000000000000000, 0.8660254037844387076, 1.000000000000000000, 0.8660254037844387076, 1.000000000000000000, 0.8660254037844387076, 1.000000000000000000, 0.8660254037844387076, 1.000000000000000000, 0.8660254037844387076, 1.000000000000000000, 0.8660254037844387076, 1.000000000000000000, 0.8660254037844387076, 1.000000000000000000, 0.8660254037844387076, 1.000000000000000000, 0.8660254037844387076, 1.000000000000000000, 0.8660254037844387076, 1.000000000000000000, 0.8660254037844387076, 1.000000000000000000, 0.8660254037844387076, 1.000000000000000000, 0.8660254037844387076, 1.000000000000000000, 0.8660254037844387076, 1.000000000000000000, 0.8660254037844387076, 1.000000000000000000, 0.8660254037844387076, 1.000000000000000000, 0.8660254037844387076, 1.000000000000000000, 0.8660254037844387076, 1.000000000000000000, 0.8660254037844387076, 1.000000000000000000, 0.8660254037844387076, 1.000000000000000000, 0.8660254037844387076, 1.000000000000000000, 0.8660254037844387076, 1.000000000000000000, 0.8660254037844387076, 1.000000000000000000, 0.8660254037844387076, 1.000000000000000000, 0.8660254037844387076, 1.000000000000000000, 0.8660254037844387076, 1.000000000000000000, 0.8660254037844387076, 1.000000000000000000, 0.8660254037844387076, 1.000000000000000000, 0.8660254037844387076, 1.000000000000000000, 0.8660254037844387076, 1.000000000000000000, 0.8660254037844387076, 1.000000000000000000, 0.8660254037844387076, 1.000000000000000000, 0.8660254037844387076, 1.000000000000000000, 0.8660254037844387076, 1.000000000000000000, 0.8660254037844387076, 1.000000000000000000, 0.8660254037844387076, 1.000000000000000000, 0.8660254037844387076, 1.000000000000000000, 0.8660254037844387076, 1.000000000000000000, 0.8660254037844387076, 1.000000000000000000, 0.8660254037844387076, 1.000000000000000000, 0.8660254037844387076, 1.000000000000000000, 0.8660254037844387076, 1.000000000000000000, 0.8660254037844387076, 1.000000000000000000, 0.8660254037844387076, 1.000000000000000000, 0.8660254037844387076, 1.000000000000000000, 0.8660254037844387076, 1.000000000000000000, 0.8660254037844387076, 1.000000000000000000, 0.8660254037844387076, 1.000000000000000000, 0.8660254037844387076, 1.000000000000000000, 0.8660254037844387076, 1.000000000000000000, 0.8660254037844387076, 1.000000000000000000, 0.8660254037844387076, 1.000000000000000000, 0.8660254037844387076, 1.000000000000000000, 0.8660254037844387076, 1.000000000000000000, 0.8660254037844387076, 1.000000000000000000, 0.8660254037844387076, 1.000000000000000000, 0.8660254037844387076, 1.000000000000000000, 0.8660254037844387076, 1.000000000000000000, 0.8660254037844387076, 1.000000000000000000, 0.8660254037844387076, 1.000000000000000000, 0.8660254037844387076, 1.000000000000000000, 0.8660254037844387076, 1.000000000000000000, 0.8660254037844387076, 1.000000000000000000, 0.8660254037844387076, 1.000000000000000000, 0.8660254037844387076, 1.000000000000000000, 0.8660254037844387076, 1.000000000000000000, 0.8660254037844387076, 1.000000000000000000, 0.8660254037844387076, 1.000000000000000000, 0.8660254037844387076, 1.000000000000000000, 0.8660254037844387076, 1.000000000000000000, 0.8660254037844387076, 1.000000000000000000, 0.8660254037844387076, 1.000000000000000000, 0.8660254037844387076, 1.000000000000000000, 0.8660254037844387076, 1.000000000000000000, 0.8660254037844387076, 1.000000000000000000, 0.8660254037844387076, 1.000000000000000000, 0.8660254037844387076, 1.000000000000000000, 0.8660254037844387076, 1.000000000000000000, 0.8660254037844387076, 1.000000000000000000, 0.8660254037844387076, 1.000000000000000000, 0.8660254037844387076, 1.000000000000000000, 0.8660254037844387076, 1.000000000000000000, 0.8660254037844387076, 1.000000000000000000, 0.8660254037844387076, 1.000000000000000000, 0.8660254037844387076, 1.000000000000000000, 0.8660254037844387076, 1.000000000000000000, 0.8660254037844387076, 1.000000000000000000, 0.8660254037844387076, 1.000000000000000000, 0.8660254037844387076, 1.000000000000000000, 0.8660254037844387076, 1.000000000000000000, 0.8660254037844387076, 1.000000000000000000, 0.8660254037844387076, 1.000000000000000000, 0.8660254037844387076, 1.000000000000000000, 0.8660254037844387076, 1.000000000000000000, 0.8660254037844387076, 1.000000000000000000, 0.8660254037844387076, 1.000000000000000000, 0.8660254037844387076, 1.000000000000000000, 0.8660254037844387076, 1.000000000000000000, 0.8660254037844387076, 1.000000000000000000, 0.8660254037844387076, 1.000000000000000000, 0.8660254037844387076, 1.000000000000000000, 0.8660254037844387076, 1.000000000000000000, 0.8660254037844387076, 1.000000000000000000, 0.8660254037844387076, 1.000000000000000000, 0.8660254037844387076, 1.000000000000000000, 0.8660254037844387076, 1.000000000000000000, 0.8660254037844387076, 1.000000000000000000, 0.8660254037844387076, 1.000000000000000000, 0.8660254037844387076, 1.000000000000000000, 0.8660254037844387076, 1.000000000000000000, 0.8660254037844387076, 1.000000000000000000, 0.8660254037844387076, 1.000000000000000000, 0.8660254037844387076, 1.000000000000000000, 0.8660254037844387076, 1.000000000000000000, 0.8660254037844387076, 1.000000000000000000, 0.8660254037844387076, 1.000000000000000000, 0.8660254037844387076, 1.000000000000000000, 0.8660254037844387076, 1.000000000000000000, 0.8660254037844387076, 1.000000000000000000, 0.8660254037844387076, 1.000000000000000000, 0.8660254037844387076, 1.000000000000000000, 0.8660254037844387076, 1.000000000000000000, 0.8660254037844387076, 1.000000000000000000, 0.8660254037844387076, 1.000000000000000000, 0.8660254037844387076, 1.000000000000000000, 0.8660254037844387076, 1.000000000000000000, 0.8660254037844387076, 1.000000000000000000, 0.8660254037844387076, 1.000000000000000000, 0.8660254037844387076, 1.000000000000000000, 0.8660254037844387076, 1.000000000000000000, 0.8660254037844387076, 1.000000000000000000, 0.8660254037844387076, 1.000000000000000000, 0.8660254037844387076, 1.000000000000000000, 0.8660254037844387076, 1.000000000000000000, 0.8660254037844387076, 1.000000000000000000, 0.8660254037844387076, 1.000000000000000000, 0.8660254037844387076, 1.000000000000000000, 0.8660254037844387076, 1.000000000000000000, 0.8660254037844387076, 1.000000000000000000, 0.8660254037844387076, 1.000000000000000000, 0.8660254037844387076, 1.000000000000000000, 0.8660254037844387076, 1.000000000000000000, 0.8660254037844387076, 1.000000000000000000, 0.8660254037844387076, 1.000000000000000000, 0.8660254037844387076, 1.000000000000000000, 0.8660254037844387076, 1.000000000000000000, 0.8660254037844387076, 1.000000000000000000, 0.8660254037844387076, 1.000000000000000000, 0.8660254037844387076, 1.000000000000000000, 0.8660254037844387076, 1.000000000000000000, 0.8660254037844387076, 1.000000000000000000, 0.8660254037844387076, 1.000000000000000000, 0.8660254037844387076, 1.000000000000000000, 0.8660254037844387076, 1.000000000000000000, 0.8660254037844387076, 1.000000000000000000, 0.8660254037844387076, 1.000000000000000000, 0.8660254037844387076, 1.000000000000000000, 0.8660254037844387076, 1.000000000000000000, 0.8660254037844387076, 1.000000000000000000, 0.8660254037844387076, 1.000000000000000000, 0.8660254037844387076, 1.000000000000000000, 0.8660254037844387076, 1.000000000000000000, 0.8660254037844387076, 1.000000000000000000, 0.8660254037844387076, 1.000000000000000000, 0.8660254037844387076, 1.000000000000000000, 0.8660254037844387076, 1.000000000000000000, 0.8660254037844387076, 1.000000000000000000, 0.8660254037844387076, 1.000000000000000000, 0.8660254037844387076, 1.000000000000000000, 0.8660254037844387076, 1.000000000000000000, 0.8660254037844387076, 1.000000000000000000, 0.8660254037844387076, 1.000000000000000000, 0.8660254037844387076, 1.000000000000000000, 0.8660254037844387076, 1.000000000000000000, 0.8660254037844387076, 1.000000000000000000, 0.8660254037844387076, 1.000000000000000000, 0.8660254037844387076, 1.000000000000000000, 0.8660254037844387076, 1.000000000000000000, 0.8660254037844387076, 1.000000000000000000, 0.8660254037844387076, 1.000000000000000000, 0.8660254037844387076, 1.000000000000000000, 0.8660254037844387076, 1.000000000000000000, 0.8660254037844387076, 1.000000000000000000, 0.8660254037844387076, 1.000000000000000000, 0.8660254037844387076, 1.000000000000000000, 0.8660254037844387076, 1.000000000000000000, 0.8660254037844387076, 1.000000000000000000, 0.8660254037844387076, 1.000000000000000000, 0.8660254037844387076, 1.000000000000000000, 0.8660254037844387076, 1.000000000000000000, 0.8660254037844387076, 1.000000000000000000, 0.8660254037844387076, 1.000000000000000000, 0.8660254037844387076, 1.000000000000000000, 0.8660254037844387076, 1.000000000000000000, 0.8660254037844387076, 1.000000000000000000, 0.8660254037844387076, 1.000000000000000000, 0.8660254037844387076, 1.000000000000000000, 0.8660254037844387076, 1.000000000000000000, 0.8660254037844387076, 1.000000000000000000, 0.8660254037844387076, 1.000000000000000000, 0.8660254037844387076, 1.000000000000000000, 0.8660254037844387076, 1.000000000000000000, 0.8660254037844387076, 1.000000000000000000, 0.8660254037844387076, 1.000000000000000000, 0.8660254037844387076, 1.000000000000000000, 0.8660254037844387076, 1.000000000000000000, 0.8660254037844387076, 1.000000000000000000, 0.8660254037844387076, 1.000000000000000000, 0.8660254037844387076, 1.000000000000000000, 0.8660254037844387076, 1.000000000000000000, 0.8660254037844387076, 1.000000000000000000, 0.8660254037844387076, 1.000000000000000000, 0.8660254037844387076, 1.000000000000000000, 0.8660254037844387076, 1.000000000000000000, 0.8660254037844387076, 1.000000000000000000, 0.8660254037844387076, 1.000000000000000000, 0.8660254037844387076, 1.000000000000000000, 0.8660254037844387076, 1.000000000000000000, 0.8660254037844387076, 1.000000000000000000, 0.8660254037844387076, 1.000000000000000000, 0.8660254037844387076, 1.000000000000000000, 0.8660254037844387076, 1.000000000000000000, 0.8660254037844387076, 1.000000000000000000, 0.8660254037844387076, 1.000000000000000000, 0.8660254037844387076, 1.000000000000000000, 0.8660254037844387076, 1.000000000000000000, 0.8660254037844387076, 1.000000000000000000, 0.8660254037844387076, 1.000000000000000000, 0.8660254037844387076, 1.000000000000000000, 0.8660254037844387076, 1.000000000000000000, 0.8660254037844387076, 1.000000000000000000, 0.8660254037844387076, 1.000000000000000000, 0.8660254037844387076, 1.000000000000000000, 0.8660254037844387076, 1.000000000000000000, 0.8660254037844387076, 1.000000000000000000, 0.8660254037844387076, 1.000000000000000000, 0.8660254037844387076, 1.000000000000000000, 0.8660254037844387076, 1.000000000000000000) ) ) 
 REPRESENTATION_ITEM ( '' )  SURFACE ( )  );
#127092 = CARTESIAN_POINT ( 'NONE',  ( 8.723781775389312543, 12.26516360700784958, -1.199719254218446718 ) ) ;
#127094 = AXIS2_PLACEMENT_3D ( 'NONE', #156993, #24827, #107223 ) ;
#127093 = CARTESIAN_POINT ( 'NONE',  ( 1.797964266608031547, -1.570508639683061647, -1.499219477302183412 ) ) ;
#127095 = CARTESIAN_POINT ( 'NONE',  ( -1.772826578343097204, 3.950000000000001954, 0.3999999999999941380 ) ) ;
#127096 = CARTESIAN_POINT ( 'NONE',  ( -2.981281212289682792, 6.492261378021210838, -0.0003813922843012157449 ) ) ;
#127097 = CARTESIAN_POINT ( 'NONE',  ( 2.671000074538076863, 0.09590037325727870932, -1.868228684465601752 ) ) ;
#127098 = CARTESIAN_POINT ( 'NONE',  ( 6.766866382711775429, -1.973269837180600561, -0.8828958408187634888 ) ) ;
#127100 = CARTESIAN_POINT ( 'NONE',  ( 6.827182134110164391, 0.6048993162116442779, 1.764860727632423076 ) ) ;
#127099 = CARTESIAN_POINT ( 'NONE',  ( -11.33772463945036968, 13.40000000000000036, -3.600000000000002309 ) ) ;
#127101 = CARTESIAN_POINT ( 'NONE',  ( -1.364683531250014514, -1.011458332991911568, -0.7879004041258359514 ) ) ;
#127102 = CARTESIAN_POINT ( 'NONE',  ( -1.499902018610888899, 3.250213382348775770, -0.08390812002218206445 ) ) ;
#127103 =( BOUNDED_CURVE ( )  B_SPLINE_CURVE ( 3, ( #110363, #30107, #157999, #177429 ),
 .UNSPECIFIED., .F., .T. ) 
 B_SPLINE_CURVE_WITH_KNOTS ( ( 4, 4 ),
 ( 0.5000000000000022204, 1.000000000000000000 ),
 .UNSPECIFIED. ) 
 CURVE ( )  GEOMETRIC_REPRESENTATION_ITEM ( )  RATIONAL_B_SPLINE_CURVE ( ( 0.9999999999999972244, 0.3333333333333334259, 0.3333333333333363679, 1.000000000000000222 ) ) 
 REPRESENTATION_ITEM ( '' )  );
#127104 = CARTESIAN_POINT ( 'NONE',  ( 1.963391044528959073, -1.536740334223782645, -1.137898036029337812 ) ) ;
#127105 = CARTESIAN_POINT ( 'NONE',  ( 4.645211000723334926, -1.368906681764755939, -1.121767690593698186 ) ) ;
#127106 = CARTESIAN_POINT ( 'NONE',  ( 1.295406243800485635, 1.766531960031037407, -0.7327172462580702206 ) ) ;
#127107 = CARTESIAN_POINT ( 'NONE',  ( -4.741601036477307574, 6.554953847355395880, 1.599625672291267398 ) ) ;
#127109 = CARTESIAN_POINT ( 'NONE',  ( 6.310162246266422414, 1.098484216484491904, -1.569160930707512502 ) ) ;
#127108 = DIRECTION ( 'NONE',  ( 0.000000000000000000, 0.000000000000000000, 1.000000000000000000 ) ) ;
#127110 = CARTESIAN_POINT ( 'NONE',  ( -0.7500000000000006661, -0.1416666666666441254, -1.299038105676652011 ) ) ;
#127111 = CARTESIAN_POINT ( 'NONE',  ( 1.416557266959647787, 0.8372786474034592530, 1.893679232998768391 ) ) ;
#127112 = CARTESIAN_POINT ( 'NONE',  ( -0.7499999999999972244, 5.358333333333353821, -1.299038105676652011 ) ) ;
#127113 = SURFACE_STYLE_USAGE ( .BOTH. , #130305 ) ;
#127114 = CARTESIAN_POINT ( 'NONE',  ( 5.295714669793899709, -0.6724083694377264164, 1.745798414713333413 ) ) ;
#127115 = CARTESIAN_POINT ( 'NONE',  ( 1.365546509989667534, 1.798985258052044900, -0.3101867277976525505 ) ) ;
#127117 = CARTESIAN_POINT ( 'NONE',  ( 4.620579464570812256, 8.341333509328540785, -0.3192730525469981151 ) ) ;
#127116 = CARTESIAN_POINT ( 'NONE',  ( 6.182275136424624229, -1.184133725572718676, 1.862117674348878760 ) ) ;
#127118 = CARTESIAN_POINT ( 'NONE',  ( 1.364683531249992088, 5.696875000341418804, 1.214306433183764966E-14 ) ) ;
#127119 = CARTESIAN_POINT ( 'NONE',  ( 2.506364121320878713, 2.062161341495666100, 0.05312637652370164748 ) ) ;
#127120 = CARTESIAN_POINT ( 'NONE',  ( -7.004758919754800139, 11.32396917302262018, 0.000000000000000000 ) ) ;
#127121 = CARTESIAN_POINT ( 'NONE',  ( 1.465018125636654123, 3.329945466055602488, -0.3314627765801584358 ) ) ;
#127122 = CARTESIAN_POINT ( 'NONE',  ( 6.692885107001518286, 7.837396042037102717, -1.199719254218452047 ) ) ;
#127123 = VECTOR ( 'NONE', #97769, 1000.000000000000000 ) ;
#127124 = ORIENTED_EDGE ( 'NONE', *, *, #145579, .F. ) ;
#127125 = CARTESIAN_POINT ( 'NONE',  ( 5.459458695672200435, 1.690470114046587646, 1.195012289465044564 ) ) ;
#127126 = CARTESIAN_POINT ( 'NONE',  ( -1.364683531250014514, 0.3427083336747508424, 0.7879004041258379498 ) ) ;
#127127 = CARTESIAN_POINT ( 'NONE',  ( 2.372553944209778720, -1.331880425775422205, 1.702409713178254069 ) ) ;
#127128 = CARTESIAN_POINT ( 'NONE',  ( -4.964107424972056037, 7.970992240003957008, 1.031144368780096965 ) ) ;
#127129 = CARTESIAN_POINT ( 'NONE',  ( 3.404948832191158736, -0.3961486058311721736, -1.980257767865372109 ) ) ;
#127130 = CARTESIAN_POINT ( 'NONE',  ( -2.034713692888051373, 8.461455076002923903, 2.500000000000011102 ) ) ;
#127133 = CARTESIAN_POINT ( 'NONE',  ( 8.622622508611357262, 9.162073802909148412, -0.7216878364870197293 ) ) ;
#127132 = CARTESIAN_POINT ( 'NONE',  ( -3.475000000000000533, -1.079166666666665941, -2.006292185433948827 ) ) ;
#127131 = CARTESIAN_POINT ( 'NONE',  ( 9.796090618744123901, 3.974415841077565403, 6.102288299938424920 ) ) ;
#127134 = CARTESIAN_POINT ( 'NONE',  ( -2.997761361953021009, 6.511488999004883205, -0.7216878364870458196 ) ) ;
#127135 = CARTESIAN_POINT ( 'NONE',  ( 0.8840003597419334724, -2.016708404047353742, 0.004841148455551891328 ) ) ;
#127137 = CARTESIAN_POINT ( 'NONE',  ( 6.110890996357365879, -0.2699588104537915534, 2.174781792473476472 ) ) ;
#127136 = CARTESIAN_POINT ( 'NONE',  ( -6.240830780992103755, 6.175390754112560110, 1.040834085586084257E-14 ) ) ;
#127138 = CARTESIAN_POINT ( 'NONE',  ( -1.001543065824772872E-14, 4.743750000682822154, 1.732050807568877637 ) ) ;
#127139 = CARTESIAN_POINT ( 'NONE',  ( 4.746305163667582150, 0.9781546018433548983, -1.643150005489722787 ) ) ;
#127140 = CARTESIAN_POINT ( 'NONE',  ( -4.060830702492950195, 4.696389560118578999, -1.199719254218452047 ) ) ;
#127141 = CARTESIAN_POINT ( 'NONE',  ( 6.439759776366769550, 8.536139043893143707, 1.443375672974076540 ) ) ;
#127143 = CARTESIAN_POINT ( 'NONE',  ( 3.234000073275579812, 2.016598147164900823, -0.002828922958116042007 ) ) ;
#127142 = CARTESIAN_POINT ( 'NONE',  ( -9.042925270190641740, 11.57316545335434199, 1.443375672974064550 ) ) ;
#127144 = CARTESIAN_POINT ( 'NONE',  ( -0.6823417656250039265, 13.88020833367473195, -1.181850606188755259 ) ) ;
#127145 = CARTESIAN_POINT ( 'NONE',  ( -4.034433228518296666, 6.864533312316751790, -1.199719254218450271 ) ) ;
#127146 = CARTESIAN_POINT ( 'NONE',  ( 5.596639136713698726, -0.4230586844520961010, -1.671955901692462998 ) ) ;
#127147 = CARTESIAN_POINT ( 'NONE',  ( 6.688968683495743583, 8.897159112202094988, -1.599625672291283607 ) ) ;
#127148 = CARTESIAN_POINT ( 'NONE',  ( 10.54788032175191326, 11.40820791823982994, 0.7216878364870317197 ) ) ;
#127149 = DIRECTION ( 'NONE',  ( 0.000000000000000000, 1.000000000000000000, 0.000000000000000000 ) ) ;
#127150 = CARTESIAN_POINT ( 'NONE',  ( 3.831198023013999698, -1.729401117988647929, 0.7132991360168300377 ) ) ;
#127151 = CARTESIAN_POINT ( 'NONE',  ( 2.319698010557100343, 5.424362912284642846, 0.6383152452940642485 ) ) ;
#127152 = AXIS2_PLACEMENT_3D ( 'NONE', #66170, #179972, #13188 ) ;
#127154 =( BOUNDED_CURVE ( )  B_SPLINE_CURVE ( 2, ( #168537, #3866, #184767, #131820, #33205, #20135, #165336 ),
 .UNSPECIFIED., .F., .T. ) 
 B_SPLINE_CURVE_WITH_KNOTS ( ( 3, 2, 2, 3 ),
 ( 0.1750000000000002942, 0.1791666666666668628, 0.1833333333333334036, 0.1874999999999999722 ),
 .UNSPECIFIED. ) 
 CURVE ( )  GEOMETRIC_REPRESENTATION_ITEM ( )  RATIONAL_B_SPLINE_CURVE ( ( 0.9999999999999902300, 0.8660254037844484776, 1.000000000000000000, 0.8660254037844387076, 1.000000000000000000, 0.8660254037844395958, 0.9999999999999991118 ) ) 
 REPRESENTATION_ITEM ( '' )  );
#127153 = CARTESIAN_POINT ( 'NONE',  ( 1.235311698660218616, -0.04697018572753957483, -2.069874154031334790 ) ) ;
#127155 = CARTESIAN_POINT ( 'NONE',  ( -1.500000000000053513, 7.267697830503716538, -4.207111467970358731 ) ) ;
#127156 = ORIENTED_EDGE ( 'NONE', *, *, #92482, .T. ) ;
#127157 = CARTESIAN_POINT ( 'NONE',  ( 5.830666647502705580, 1.211628268937942066, -1.346810592849301047 ) ) ;
#127158 = CARTESIAN_POINT ( 'NONE',  ( 3.718679271898170491, 7.560485927181699317, 0.7998128361456271485 ) ) ;
#127159 = FACE_OUTER_BOUND ( 'NONE', #76685, .T. ) ;
#127160 = CARTESIAN_POINT ( 'NONE',  ( -0.1583346312582509796, -1.114004300041637974, -1.428896152673633013 ) ) ;
#127161 = CARTESIAN_POINT ( 'NONE',  ( 4.380693030546905398, 8.124909279031149012, 0.7216878364870247253 ) ) ;
#127162 = CARTESIAN_POINT ( 'NONE',  ( 9.502358067502351346, 13.11573065610559574, -7.329361613111205820 ) ) ;
#127163 = CARTESIAN_POINT ( 'NONE',  ( 3.539196308827243787, -1.659330947522210886, -1.431560661003590695 ) ) ;
#127164 = ORIENTED_EDGE ( 'NONE', *, *, #163961, .F. ) ;
#127165 = EDGE_CURVE ( 'NONE', #18470, #19630, #9210, .T. ) ;
#127167 = CARTESIAN_POINT ( 'NONE',  ( 9.565441069641300587, 11.11843498845840905, -1.199719254218440723 ) ) ;
#127166 = CARTESIAN_POINT ( 'NONE',  ( 0.9944974185457016169, 1.932217576897478528, 0.3389098420027157332 ) ) ;
#127168 = B_SPLINE_CURVE_WITH_KNOTS ( 'NONE', 3,
 ( #157162, #156086, #122607, #72681, #56448, #6601, #203730, #40202, #119375, #70525 ),
 .UNSPECIFIED., .F., .F.,
 ( 4, 1, 1, 1, 1, 1, 1, 4 ),
 ( 0.000000000000000000, 0.09790276019723312406, 0.1918320694002237370, 0.2608036337010187777, 0.3626611837559554630, 0.5214803378330250538, 0.7337833476510040587, 1.000000000000000000 ),
 .UNSPECIFIED. ) ;
#127169 = CARTESIAN_POINT ( 'NONE',  ( 5.097249261280999200, -0.2764669589378037085, 1.895409748447648202 ) ) ;
#127170 = FACE_OUTER_BOUND ( 'NONE', #105605, .T. ) ;
#127171 = CARTESIAN_POINT ( 'NONE',  ( -6.121671443416687453, 7.010146470470823843, 0.9629068762325782016 ) ) ;
#127172 = CARTESIAN_POINT ( 'NONE',  ( -10.18461545817740088, 3.956598013261175772, 5.433575010662861082 ) ) ;
#127173 = CARTESIAN_POINT ( 'NONE',  ( -1.364683531250000748, 0.009375000341420303140, 0.000000000000000000 ) ) ;
#127175 = ORIENTED_EDGE ( 'NONE', *, *, #193200, .T. ) ;
#127174 = CARTESIAN_POINT ( 'NONE',  ( 6.507550544879468823, 6.694489845221929691, -0.7216878364870257245 ) ) ;
#127176 = CARTESIAN_POINT ( 'NONE',  ( -7.510853912290736289, 11.70648729774046792, 0.7216878364870458196 ) ) ;
#127177 = CIRCLE ( 'NONE', #165121, 0.04999999999999985706 ) ;
#127178 = CARTESIAN_POINT ( 'NONE',  ( 1.340939272977889729, 0.4221563536682856332, 2.119910705745978508 ) ) ;
#127179 = CARTESIAN_POINT ( 'NONE',  ( -3.623772196602547346, 7.449761006003425834, 0.000000000000000000 ) ) ;
#127180 = CARTESIAN_POINT ( 'NONE',  ( 6.536439455564150514, 9.679577560583279450, 1.082531754730549078 ) ) ;
#127181 = CARTESIAN_POINT ( 'NONE',  ( 1.658932825283397250, -1.563847321437005666, -0.9416461389453802955 ) ) ;
#127182 = CARTESIAN_POINT ( 'NONE',  ( 0.1586465271753433603, 2.115359532055087310, 0.1496401998123952359 ) ) ;
#127183 = CARTESIAN_POINT ( 'NONE',  ( 5.209893869493905427, -1.816617279468687229, 0.1804919988709560719 ) ) ;
#127184 = EDGE_CURVE ( 'NONE', #72298, #197365, #73030, .T. ) ;
#127185 = CARTESIAN_POINT ( 'NONE',  ( 9.231638989588612176, 10.65826171540251366, -7.829156132265964629 ) ) ;
#127186 = CARTESIAN_POINT ( 'NONE',  ( 0.7023363917650466970, -0.6599406036866415359, -1.857761218813491988 ) ) ;
#127187 = CARTESIAN_POINT ( 'NONE',  ( 3.410326831400651404, -1.910418641682644969, -0.08914582809275289899 ) ) ;
#127188 = VERTEX_POINT ( 'NONE', #104353 ) ;
#127189 = CARTESIAN_POINT ( 'NONE',  ( 4.193778028305522376, -1.356587754280412339, -1.428115657216560974 ) ) ;
#127190 = ORIENTED_EDGE ( 'NONE', *, *, #113810, .F. ) ;
#127191 = CARTESIAN_POINT ( 'NONE',  ( 5.688998805639625012, 1.473442329711650345, 1.265259504309938610 ) ) ;
#127192 = ORIENTED_EDGE ( 'NONE', *, *, #86559, .F. ) ;
#127193 = CARTESIAN_POINT ( 'NONE',  ( -4.911796789900812144, 8.952456364851418158, 0.7998128361456291469 ) ) ;
#127195 = CARTESIAN_POINT ( 'NONE',  ( -0.3282377607281372622, 1.261164550367456672, -1.225000000000019851 ) ) ;
#127194 = CARTESIAN_POINT ( 'NONE',  ( -4.111865726694519552, 8.019203457777400956, 0.000000000000000000 ) ) ;
#127196 = CARTESIAN_POINT ( 'NONE',  ( 7.973603738168424826, 8.475161580717541554, 0.000000000000000000 ) ) ;
#127197 = CARTESIAN_POINT ( 'NONE',  ( 4.248624793116656306, 1.876006594227698221, 0.3698101955103145211 ) ) ;
#127198 = CARTESIAN_POINT ( 'NONE',  ( 5.634486230560368902, 6.328851001874927107, -1.145628596103397623 ) ) ;
#127199 = DIRECTION ( 'NONE',  ( 0.000000000000000000, 0.000000000000000000, -1.000000000000000000 ) ) ;
#127200 = CARTESIAN_POINT ( 'NONE',  ( 0.2181801407958559869, -2.163675782650812618, 0.4331315337846516900 ) ) ;
#127201 = CARTESIAN_POINT ( 'NONE',  ( 3.390947817193682656, 6.009837315817661008, -1.082531754730549967 ) ) ;
#127202 = CARTESIAN_POINT ( 'NONE',  ( 5.690095194620785612, 1.200872180055783112, 1.615535318972769474 ) ) ;
#127203 = DIRECTION ( 'NONE',  ( 1.000000000000000000, -0.000000000000000000, -0.000000000000000000 ) ) ;
#127204 = CARTESIAN_POINT ( 'NONE',  ( 5.654876981934024549, -1.436564326775534806, 1.126588154728463742 ) ) ;
#127205 = CARTESIAN_POINT ( 'NONE',  ( 2.471216696211364638, 1.848302923701108158, 0.9330170062570308787 ) ) ;
#127206 = CARTESIAN_POINT ( 'NONE',  ( -8.365017589951714072, 8.861534731139549592, 1.040834085586084257E-14 ) ) ;
#127207 = CARTESIAN_POINT ( 'NONE',  ( -6.374142478797011790, 6.840173217398676897, -0.5947513654121737714 ) ) ;
#127208 = CYLINDRICAL_SURFACE ( 'NONE', #15389, 1.224999999999996980 ) ;
#127209 = CARTESIAN_POINT ( 'NONE',  ( -1.642778471875000035, -2.967708332855374831, -2.845375778867859751 ) ) ;
#127210 = CARTESIAN_POINT ( 'NONE',  ( 5.913327553854682783, 10.05063257947248800, -0.7998128361456291469 ) ) ;
#127211 = DIRECTION ( 'NONE',  ( -0.000000000000000000, -8.546850786086437571E-32, -1.000000000000000000 ) ) ;
#127212 = CARTESIAN_POINT ( 'NONE',  ( 2.866659414285625651, 5.431854185720147221, -1.199719254218446718 ) ) ;
#127213 = CARTESIAN_POINT ( 'NONE',  ( -0.6823417656250039265, 11.88020833367473017, -1.181850606188755259 ) ) ;
#127214 = CARTESIAN_POINT ( 'NONE',  ( -4.948889764188092677, 5.732458465429559169, 1.199719254218462483 ) ) ;
#127216 = CARTESIAN_POINT ( 'NONE',  ( -5.921879234118920365, 10.13088588310589699, 0.000000000000000000 ) ) ;
#127215 = CARTESIAN_POINT ( 'NONE',  ( 7.362820735712270803, -5.796536394785693602, -7.362820735712300113 ) ) ;
#127217 = CARTESIAN_POINT ( 'NONE',  ( 4.148821288392518625, 0.8220224570679548481, 1.526945684688446381 ) ) ;
#127218 = CARTESIAN_POINT ( 'NONE',  ( -4.578903193113314174, 6.365139696764064325, 1.599625672291267398 ) ) ;
#127219 = CARTESIAN_POINT ( 'NONE',  ( 1.428671948192638208, -1.316369429293560156, 1.597808059233512656 ) ) ;
#127220 = CARTESIAN_POINT ( 'NONE',  ( 3.339577153505444151, 0.5119293057267596536, -2.054306502313862470 ) ) ;
#127221 = CARTESIAN_POINT ( 'NONE',  ( 3.897079088924235712, 6.634010472798538949, 1.199719254218462483 ) ) ;
#127222 = CARTESIAN_POINT ( 'NONE',  ( 8.076906825439115423, 10.44614393447756129, -1.599625672291262513 ) ) ;
#127223 = CARTESIAN_POINT ( 'NONE',  ( 2.449293598294706414E-16, 9.999999999999998224, 2.000000000000000000 ) ) ;
#127224 = CARTESIAN_POINT ( 'NONE',  ( 6.877786287229037399, -2.009644702432196617, 0.4970176993947388322 ) ) ;
#127225 = CARTESIAN_POINT ( 'NONE',  ( 4.815752433886056671, 6.955745678547994970, 1.411323681429425880 ) ) ;
#127226 = CARTESIAN_POINT ( 'NONE',  ( 4.907688418466886304, 5.788353245375237321, -1.082531754730548412 ) ) ;
#127228 = DIRECTION ( 'NONE',  ( -0.9999980456341538426, 0.000000000000000000, -0.001977050295967298574 ) ) ;
#127227 = CARTESIAN_POINT ( 'NONE',  ( 1.737499999999999378, -2.566666666666668650, -3.009438278150925683 ) ) ;
#127229 = CARTESIAN_POINT ( 'NONE',  ( 3.662334778960428139, -1.540015086033737601, 1.698051401694438800 ) ) ;
#127230 = CARTESIAN_POINT ( 'NONE',  ( 0.3459771380207553593, 1.820543102168985961, 0.1377627428671979182 ) ) ;
#127231 = CARTESIAN_POINT ( 'NONE',  ( 3.849791259674230748, -1.322437695595569673, -1.381667681676468140 ) ) ;
#127232 = CARTESIAN_POINT ( 'NONE',  ( 7.178115983792402233, 7.339166500704784823, 0.7998128361456281477 ) ) ;
#127233 = CARTESIAN_POINT ( 'NONE',  ( 5.761852095683461350, 9.665985178365305686, -0.7216878364870267237 ) ) ;
#127234 = CARTESIAN_POINT ( 'NONE',  ( -9.833741488613570780, 10.36711991300432345, 0.7998128361456462443 ) ) ;
#127235 = ADVANCED_FACE ( 'NONE', ( #119592, #170398 ), #54527, .T. ) ;
#127236 = CARTESIAN_POINT ( 'NONE',  ( 1.687745526430058263, 1.925312447093192825, -0.5882657090081342410 ) ) ;
#127237 = CARTESIAN_POINT ( 'NONE',  ( 2.342563710341159400, -1.922903400459201828, -0.3876519335672747313 ) ) ;
#127238 = CARTESIAN_POINT ( 'NONE',  ( -9.809487834687324437, 11.40315621434539395, 1.199719254218462483 ) ) ;
#127239 = CARTESIAN_POINT ( 'NONE',  ( -7.562750758324527922, 7.717630727667075696, 1.040834085586084257E-14 ) ) ;
#127240 = CARTESIAN_POINT ( 'NONE',  ( -5.273758565591545988, 6.215435083687305351, 1.082531754730546636 ) ) ;
#127242 = CARTESIAN_POINT ( 'NONE',  ( 3.080641367082480819, -0.1285219475026712632, -1.765225098288242256 ) ) ;
#127241 = CARTESIAN_POINT ( 'NONE',  ( 5.050766879278534738, -1.765858898356540196, -1.118837652998798005 ) ) ;
#127243 = CARTESIAN_POINT ( 'NONE',  ( 0.6674790882334069586, 14.00000000000000533, 11.66566053519463786 ) ) ;
#127245 = CARTESIAN_POINT ( 'NONE',  ( 5.947306879541199187, 0.6707566017311801243, -2.191947003353618584 ) ) ;
#127244 = CARTESIAN_POINT ( 'NONE',  ( -11.86145016429273191, 19.00000000000000000, 1.179999999999997051 ) ) ;
#127246 = CARTESIAN_POINT ( 'NONE',  ( 4.505614311517684101, -0.7474637548481823934, -1.571778613660354207 ) ) ;
#127247 = CARTESIAN_POINT ( 'NONE',  ( 7.377608144130607393, 11.75895993479440982, -0.7998128361456291469 ) ) ;
#127248 = CARTESIAN_POINT ( 'NONE',  ( 7.863746947443975621, -5.507058666270990166, -7.245729715095582613 ) ) ;
#127249 = CARTESIAN_POINT ( 'NONE',  ( 4.762897148713774342, -1.733524727309469382, -0.04171941676067019572 ) ) ;
#127250 = CARTESIAN_POINT ( 'NONE',  ( 4.897030219210679824, 0.3665305452156160659, 2.139867649710110786 ) ) ;
#127251 = FACE_OUTER_BOUND ( 'NONE', #46267, .T. ) ;
#127252 = CARTESIAN_POINT ( 'NONE',  ( -0.1704767588886099972, -1.641208087572191276, -1.337381612054800772 ) ) ;
#127253 = CARTESIAN_POINT ( 'NONE',  ( 5.906250000000004441, 1.895863743163945125, -0.7852924748303062863 ) ) ;
#127254 = CIRCLE ( 'NONE', #182493, 0.07999999999999998779 ) ;
#127255 = CARTESIAN_POINT ( 'NONE',  ( 2.977471715415116460, 1.829795069231574534, -0.6025905002205227401 ) ) ;
#127256 = CARTESIAN_POINT ( 'NONE',  ( -1.402160292154681736E-14, 11.34375000068279427, 1.732050807568881190 ) ) ;
#127257 = CARTESIAN_POINT ( 'NONE',  ( 0.5928132819080602633, -1.229099697874297181, 1.850090981381287358 ) ) ;
#127258 = EDGE_LOOP ( 'NONE', ( #128012, #5069, #180893, #184508 ) ) ;
#127259 = CARTESIAN_POINT ( 'NONE',  ( -0.1411974294641838990, 5.723166529328228336, -2.494358352568406545 ) ) ;
#127260 = CARTESIAN_POINT ( 'NONE',  ( -1.500000000000011324, 2.670833333333352044, 0.8660254037844403729 ) ) ;
#127261 = CARTESIAN_POINT ( 'NONE',  ( 5.449487677688982679, 8.445153826357429949, -1.199719254218446718 ) ) ;
#127262 = CARTESIAN_POINT ( 'NONE',  ( 2.825082509308895151, 1.607285200359307886, -1.533455307168646975 ) ) ;
#127263 = LINE ( 'NONE', #76283, #1092 ) ;
#127264 = CARTESIAN_POINT ( 'NONE',  ( 5.992340707560141588, 9.934888558888093968, 0.7216878364870438212 ) ) ;
#127265 = CARTESIAN_POINT ( 'NONE',  ( -8.771762197917311710, 13.17754696430482042, 0.7216878364870317197 ) ) ;
#127266 = CARTESIAN_POINT ( 'NONE',  ( 3.984117037569365305, 5.741498858621315371, 1.599625672291261402 ) ) ;
#127267 = CIRCLE ( 'NONE', #154856, 11.29999999999998828 ) ;
#127268 = CARTESIAN_POINT ( 'NONE',  ( 0.3697678102792775756, -0.2496098759999023087, -2.000856779379902139 ) ) ;
#127270 = CARTESIAN_POINT ( 'NONE',  ( 5.230950406320217461, -1.941087326682365832, -0.6980428833110083886 ) ) ;
#127269 = CARTESIAN_POINT ( 'NONE',  ( 8.540746701604824409, 12.05162268759261224, -1.199719254218446718 ) ) ;
#127271 = DIRECTION ( 'NONE',  ( 0.000000000000000000, 0.000000000000000000, 1.000000000000000000 ) ) ;
#127272 = CARTESIAN_POINT ( 'NONE',  ( 1.499999999999990896, 5.056250000682820378, 1.214306433183764966E-14 ) ) ;
#127273 = CARTESIAN_POINT ( 'NONE',  ( 1.364683531249988535, 1.613541667008084879, 0.7879004041258500513 ) ) ;
#127274 = CARTESIAN_POINT ( 'NONE',  ( 0.5086179708909451813, 1.535567861042252957, 0.8796773807029609760 ) ) ;
#127275 = CARTESIAN_POINT ( 'NONE',  ( 5.678250988984351544, 1.318717643421193575, 1.126304846749843769 ) ) ;
#127276 = CARTESIAN_POINT ( 'NONE',  ( 5.196709787541290204, 1.427093291641279293, 0.9959802872364865722 ) ) ;
#127277 = ADVANCED_FACE ( 'NONE', ( #169341 ), #52588, .T. ) ;
#127278 = CARTESIAN_POINT ( 'NONE',  ( 2.542860532589632960, -1.904047414228837942, 1.276277502183044810 ) ) ;
#127279 = CARTESIAN_POINT ( 'NONE',  ( -1.364683531250014514, 0.2385416670080863499, -0.7879004041258359514 ) ) ;
#127280 = CARTESIAN_POINT ( 'NONE',  ( 1.710644026344819046, -0.2265308078298749472, 1.827073587482845207 ) ) ;
#127281 = CARTESIAN_POINT ( 'NONE',  ( 10.42352117080803708, 11.05519620889787724, -0.7998128361456281477 ) ) ;
#127282 = CARTESIAN_POINT ( 'NONE',  ( 2.256629077056008015, -1.412982602626071671, 1.155960151518524937 ) ) ;
#127283 = CARTESIAN_POINT ( 'NONE',  ( 3.129529892704606464, 0.4926417352555876872, 1.955172657653013957 ) ) ;
#127284 = CARTESIAN_POINT ( 'NONE',  ( -2.453662613948990323, 5.806430783008362795, -0.7216878364870257245 ) ) ;
#127285 = CARTESIAN_POINT ( 'NONE',  ( 4.000000000000022204, 5.499999999999998224, 2.024999999999999023 ) ) ;
#127286 = CARTESIAN_POINT ( 'NONE',  ( 4.559663772078708988, 0.4639327178320976630, -2.054050964449795291 ) ) ;
#127287 = CARTESIAN_POINT ( 'NONE',  ( -5.876569516519495551, 8.943415971659659292, 1.199719254218452047 ) ) ;
#127288 = CARTESIAN_POINT ( 'NONE',  ( 7.861136941706560854, 14.80574585066181825, 8.642037812201863289 ) ) ;
#127289 = CARTESIAN_POINT ( 'NONE',  ( 2.014207461368537455, 2.064961549741591185, -0.1501100615294431728 ) ) ;
#127290 = CARTESIAN_POINT ( 'NONE',  ( 2.855963913973019963, 6.483708332943829866, 0.000000000000000000 ) ) ;
#127291 = CARTESIAN_POINT ( 'NONE',  ( -1.953008978358306879E-14, 0.2343750003414031002, 1.570758158831794260 ) ) ;
#127292 = CARTESIAN_POINT ( 'NONE',  ( 4.178469031319306914, 1.000645923475869559, 1.869553197578948334 ) ) ;
#127293 = CONTEXT_DEPENDENT_SHAPE_REPRESENTATION ( #99078, #95644 ) ;
#127295 = EDGE_CURVE ( 'NONE', #25627, #166389, #36868, .T. ) ;
#127294 = CARTESIAN_POINT ( 'NONE',  ( 6.463509179248937642, 0.3066564278407272748, -1.799597105106438777 ) ) ;
#127296 = ORIENTED_EDGE ( 'NONE', *, *, #5002, .T. ) ;
#127297 = CARTESIAN_POINT ( 'NONE',  ( -4.468294144155606773, 7.370704380560280100, 1.199719254218452935 ) ) ;
#127298 = CARTESIAN_POINT ( 'NONE',  ( 8.563946585326370098, 13.14302144952281814, 0.7998128361456462443 ) ) ;
#127299 = CARTESIAN_POINT ( 'NONE',  ( 5.031484404002878996, 7.923796667095108326, 1.082531754730548412 ) ) ;
#127300 = FACE_OUTER_BOUND ( 'NONE', #200321, .T. ) ;
#127301 = CARTESIAN_POINT ( 'NONE',  ( -5.473741331615264549, 7.409117525016355010, -1.599625672291256295 ) ) ;
#127302 = CARTESIAN_POINT ( 'NONE',  ( 6.135037582782754129, 1.979230198018981701, 0.7618025574447004900 ) ) ;
#127303 = CARTESIAN_POINT ( 'NONE',  ( 0.9386647947689167326, 2.074798300807283447, 0.3599966696490787266 ) ) ;
#127304 = CARTESIAN_POINT ( 'NONE',  ( -4.444040490229335560, 8.406740681901359480, 0.7998128361456352531 ) ) ;
#127305 = CARTESIAN_POINT ( 'NONE',  ( 8.860417081730671995, 10.29590700256267155, 1.199719254218453823 ) ) ;
#127306 = CARTESIAN_POINT ( 'NONE',  ( 6.262542430310119812, -0.6688554880303022587, -1.736790604091620560 ) ) ;
#127307 = CARTESIAN_POINT ( 'NONE',  ( 6.591235234537977661, 10.84152487360300299, 0.7998128361456462443 ) ) ;
#127308 = CARTESIAN_POINT ( 'NONE',  ( -0.5993104169204935827, 4.282419057637656401, 0.2596433605236394548 ) ) ;
#127309 = CARTESIAN_POINT ( 'NONE',  ( -4.659162064951642535, 5.464719159645540003, 1.199719254218452935 ) ) ;
#127311 = CARTESIAN_POINT ( 'NONE',  ( -3.735435015764967837, 4.316761258935923884, -1.199719254218452047 ) ) ;
#127310 = VECTOR ( 'NONE', #75862, 1000.000000000000000 ) ;
#127312 = CARTESIAN_POINT ( 'NONE',  ( -9.410012541129075814, 4.000000000000001776, 6.919867902370715917 ) ) ;
#127313 =( NAMED_UNIT ( * ) PLANE_ANGLE_UNIT ( ) SI_UNIT ( $, .RADIAN. ) );
#127315 = CARTESIAN_POINT ( 'NONE',  ( 2.576550507925364109, 1.283677811227203147, -1.483670167215108693 ) ) ;
#127314 = CARTESIAN_POINT ( 'NONE',  ( -6.021792782764022078, 10.17717534653336209, -0.7998128361456291469 ) ) ;
#127316 = CARTESIAN_POINT ( 'NONE',  ( 1.358524781292804517, 0.8764843271744371389, 1.976213614152767750 ) ) ;
#127318 = CARTESIAN_POINT ( 'NONE',  ( -6.133306371789854161, 5.998871118906519584, 0.1305517085098181207 ) ) ;
#127317 = CARTESIAN_POINT ( 'NONE',  ( -5.960744811863571968, 6.983232364376142698, 1.199719254218452935 ) ) ;
#127319 = CARTESIAN_POINT ( 'NONE',  ( 1.364683531249988757, 2.384375000341422357, 1.214306433183764966E-14 ) ) ;
#127320 = CARTESIAN_POINT ( 'NONE',  ( 3.198323437492247123, -1.162659817912135019, -1.286436312214979338 ) ) ;
#127321 = CARTESIAN_POINT ( 'NONE',  ( 2.396107360292961008, 1.398095582919863133, -1.036136137726038520 ) ) ;
#127322 = CARTESIAN_POINT ( 'NONE',  ( 7.185458225562760148, 8.445751353653788485, -1.082531754730543083 ) ) ;
#127323 = CARTESIAN_POINT ( 'NONE',  ( -12.26673246283585961, 6.254089313302478637, -3.851195297204758727 ) ) ;
#127324 = TOROIDAL_SURFACE ( 'NONE', #85791, 10.75000000000000000, 0.5000000000000007772 ) ;
#127325 = CARTESIAN_POINT ( 'NONE',  ( 2.319685276966905629, -1.560262528187049025, 1.276846253076675541 ) ) ;
#127326 = CARTESIAN_POINT ( 'NONE',  ( 6.825078400183572036, 7.051914997414900022, 2.742498282622223726 ) ) ;
#127327 = CARTESIAN_POINT ( 'NONE',  ( -3.311934663488232733, 7.085950550703385531, -0.7998128361456481317 ) ) ;
#127328 = EDGE_CURVE ( 'NONE', #137341, #10807, #80435, .T. ) ;
#127329 = CARTESIAN_POINT ( 'NONE',  ( 0.9539096209374531288, 1.969307747869667446, -0.09461285551524113713 ) ) ;
#127331 = CARTESIAN_POINT ( 'NONE',  ( -4.502716413514296079, 8.267269892493059658, -0.7216878364870338292 ) ) ;
#127330 = CARTESIAN_POINT ( 'NONE',  ( 6.117437049485344502, 1.593764408019750389, 1.056661447057717362 ) ) ;
#127332 = CARTESIAN_POINT ( 'NONE',  ( -6.143253000323532831, 7.300121600866474658, 1.082531754730548412 ) ) ;
#127333 = CARTESIAN_POINT ( 'NONE',  ( 5.189738938980948291, 9.276722205444929870, 0.000000000000000000 ) ) ;
#127334 = CARTESIAN_POINT ( 'NONE',  ( -5.094831863685302942, 9.165997284266655498, 0.7998128361456291469 ) ) ;
#127335 = CARTESIAN_POINT ( 'NONE',  ( 1.418624149192078576, -0.7290977765982089576, -1.883658722702468591 ) ) ;
#127336 = CARTESIAN_POINT ( 'NONE',  ( 4.823409937486792032, -0.1187154998047341425, 2.304658580708033533 ) ) ;
#127337 = CARTESIAN_POINT ( 'NONE',  ( 5.670351692713981429, -0.8806477319739226539, -1.753155087565357428 ) ) ;
#127338 = CARTESIAN_POINT ( 'NONE',  ( 2.869914117416060062, -1.941089286637355693, 0.2830422620509198128 ) ) ;
#127339 = CARTESIAN_POINT ( 'NONE',  ( 9.284636267260101050, 9.726497154758602548, -0.7998128361456281477 ) ) ;
#127340 = CARTESIAN_POINT ( 'NONE',  ( -9.367496997601303832, 14.53091781611831479, 7.499999999995374367 ) ) ;
#127341 = ORIENTED_EDGE ( 'NONE', *, *, #6236, .F. ) ;
#127342 = CARTESIAN_POINT ( 'NONE',  ( 0.9017390913304748068, -2.064370131783893392, 0.4699791444322827250 ) ) ;
#127344 = CARTESIAN_POINT ( 'NONE',  ( -5.994676475536691029, 10.14553965476814845, 0.7998128361456481317 ) ) ;
#127343 = CARTESIAN_POINT ( 'NONE',  ( -4.192495815123836955, 5.914331089109674089, -1.599625672291256295 ) ) ;
#127345 = CARTESIAN_POINT ( 'NONE',  ( 1.499689682683522207, -0.6613356838569836027, -1.718437284301529200 ) ) ;
#127346 = ORIENTED_EDGE ( 'NONE', *, *, #95199, .T. ) ;
#127347 = CARTESIAN_POINT ( 'NONE',  ( 3.134000194803722383, 2.016708403948695771, -0.004836970814638129855 ) ) ;
#127348 = CARTESIAN_POINT ( 'NONE',  ( 11.80555752044661944, 7.909119009004187184, 2.191159464515625821 ) ) ;
#127349 = CARTESIAN_POINT ( 'NONE',  ( 2.883181758455736432, -1.960942133159260692, -0.8077274430827171559 ) ) ;
#127350 = CARTESIAN_POINT ( 'NONE',  ( 1.499999999999990896, 4.806250000682819490, 1.214306433183764966E-14 ) ) ;
#127351 = CARTESIAN_POINT ( 'NONE',  ( 8.426556166093362776, 9.789735934319136135, -1.199719254218446718 ) ) ;
#127352 = CARTESIAN_POINT ( 'NONE',  ( 6.016786309414542622, 10.24161080428416426, 0.7998128361456341429 ) ) ;
#127353 = CARTESIAN_POINT ( 'NONE',  ( 3.128252755821586906, 1.147704512706015922, -1.711389856620056493 ) ) ;
#127355 = CARTESIAN_POINT ( 'NONE',  ( 0.2394788589213901198, 1.836227513651207177, 0.1364553164684492448 ) ) ;
#127354 = CARTESIAN_POINT ( 'NONE',  ( -6.842061076390810292, 11.13415502243129218, 0.000000000000000000 ) ) ;
#127356 = CARTESIAN_POINT ( 'NONE',  ( -1.201851678989727383E-14, 3.321875000341421025, 1.575800808251672791 ) ) ;
#127357 = CARTESIAN_POINT ( 'NONE',  ( -0.02244404828157658613, 7.629137130509074716, -2.789100637983293662 ) ) ;
#127358 = CARTESIAN_POINT ( 'NONE',  ( 1.491696246971093931, 4.432377618231712724, 0.1760465247046099635 ) ) ;
#127359 = CARTESIAN_POINT ( 'NONE',  ( 0.3291288957359936318, 2.113116833900237967, 0.6364493931270903682 ) ) ;
#127360 = CARTESIAN_POINT ( 'NONE',  ( 2.812116484403729633, -2.238188867732244791, 0.3292703641907517298 ) ) ;
#127361 = CARTESIAN_POINT ( 'NONE',  ( -10.00555417720528872, 10.77549408293541866, 0.7216878364870438212 ) ) ;
#127362 = CARTESIAN_POINT ( 'NONE',  ( 2.285178059325339461, 0.08539987017499665878, -1.809671756684204214 ) ) ;
#127363 = CARTESIAN_POINT ( 'NONE',  ( 3.010844082872287331, 0.05196181304293297915, 1.915202476457795511 ) ) ;
#127364 = CARTESIAN_POINT ( 'NONE',  ( 4.070807014193541740, 1.466255041752505539, -1.461937513464212079 ) ) ;
#127365 = CARTESIAN_POINT ( 'NONE',  ( -0.6823417656250003738, 2.280208333674753174, -1.181850606188749264 ) ) ;
#127366 = CARTESIAN_POINT ( 'NONE',  ( 1.569145635881466605, 0.1472162271188414695, -1.966034296795520664 ) ) ;
#127367 = CARTESIAN_POINT ( 'NONE',  ( 6.393193437440540805, 1.674708767708126045, -0.9521171982297592651 ) ) ;
#127368 = CARTESIAN_POINT ( 'NONE',  ( 3.133525119713890472, -1.255248497922526463, -1.387151338369890574 ) ) ;
#127370 = CARTESIAN_POINT ( 'NONE',  ( 4.617922728991994852, 8.461530327540957686, 0.3091873533234041904 ) ) ;
#127369 = CARTESIAN_POINT ( 'NONE',  ( 2.438448314377542392, 1.086391669559241047, -2.035977865114136254 ) ) ;
#127371 = CARTESIAN_POINT ( 'NONE',  ( 2.347915429038241353, -0.7989592750466242288, 1.680985684562475990 ) ) ;
#127372 = CARTESIAN_POINT ( 'NONE',  ( -0.6823417656250003738, 2.967708333674754062, -1.181850606188749264 ) ) ;
#127373 = CARTESIAN_POINT ( 'NONE',  ( 6.443808500197930833, 1.419581301535753015, 1.496705048937081006 ) ) ;
#127374 = CARTESIAN_POINT ( 'NONE',  ( -4.948889764188092677, 5.732458465429559169, 1.199719254218462483 ) ) ;
#127375 = CARTESIAN_POINT ( 'NONE',  ( 7.135668919494039031, 7.219368582364847242, 1.040834085586084257E-14 ) ) ;
#127376 = CARTESIAN_POINT ( 'NONE',  ( -1.499745039105467637, 3.350786858888608943, 0.07702037080406418101 ) ) ;
#127377 = CARTESIAN_POINT ( 'NONE',  ( 6.211965580189116487, -2.090513352778848422, 0.2539706045930691380 ) ) ;
#127378 = CARTESIAN_POINT ( 'NONE',  ( -1.001543065824772872E-14, 4.634375000341418804, 1.575800808251672791 ) ) ;
#127379 = CARTESIAN_POINT ( 'NONE',  ( 6.274726406708529325, -2.050348626090079840, -0.6846857035173321560 ) ) ;
#127380 = CARTESIAN_POINT ( 'NONE',  ( 6.498695841808301843, -1.981098178724240322, -0.3918999010058578092 ) ) ;
#127381 = CARTESIAN_POINT ( 'NONE',  ( 1.364683531249988757, -0.6156249996585803075, 0.000000000000000000 ) ) ;
#127382 = CARTESIAN_POINT ( 'NONE',  ( -3.782361668532609134, 7.356579680022602652, 1.040834085586084257E-14 ) ) ;
#127385 = CARTESIAN_POINT ( 'NONE',  ( 5.341549334104200852, 5.334155099317434257, 0.7216878364870317197 ) ) ;
#127384 = CARTESIAN_POINT ( 'NONE',  ( -3.285556943750000514, -0.4885416661887091450, -1.896917185911906500 ) ) ;
#127383 = CARTESIAN_POINT ( 'NONE',  ( 5.189738938980948291, 9.276722205444929870, 0.000000000000000000 ) ) ;
#127386 = CARTESIAN_POINT ( 'NONE',  ( -5.354544322754380303, 5.211666229493680191, 0.7998128361456281477 ) ) ;
#127387 = CARTESIAN_POINT ( 'NONE',  ( 4.768767694835816862, -0.2516295123269947642, -2.000731945836851544 ) ) ;
#127388 = CARTESIAN_POINT ( 'NONE',  ( -7.446452682403657874, 9.710614100936176385, -1.599625672291263179 ) ) ;
#127390 = CARTESIAN_POINT ( 'NONE',  ( -7.227905289416804102, 8.565549271475310533, -1.082531754730549967 ) ) ;
#127389 = CARTESIAN_POINT ( 'NONE',  ( -8.161645285746702783, 12.46574390010577105, 0.7216878364870478180 ) ) ;
#127391 = B_SPLINE_CURVE_WITH_KNOTS ( 'NONE', 3,
 ( #66931, #151433, #18197, #103749, #117920, #85352 ),
 .UNSPECIFIED., .F., .F.,
 ( 4, 1, 1, 4 ),
 ( 0.000000000000000000, 0.5978647917419361857, 0.6978647917419360525, 1.000000000000000000 ),
 .UNSPECIFIED. ) ;
#127392 = PLANE ( 'NONE',  #157059 ) ;
#127394 = CARTESIAN_POINT ( 'NONE',  ( 1.364683531250000748, 9.005208333674731946, -0.7879004041258355073 ) ) ;
#127393 = CARTESIAN_POINT ( 'NONE',  ( 5.805597153138060129, -0.5296426447994294628, 2.095691122003799478 ) ) ;
#127395 = DIRECTION ( 'NONE',  ( 0.000000000000000000, 0.000000000000000000, -1.000000000000000000 ) ) ;
#127396 = DIRECTION ( 'NONE',  ( 0.000000000000000000, -1.000000000000000000, 0.000000000000000000 ) ) ;
#127398 = CARTESIAN_POINT ( 'NONE',  ( 0.1752026701883572513, 1.419887415397131925, 1.286083148499452600 ) ) ;
#127397 = CARTESIAN_POINT ( 'NONE',  ( -6.602457619730773608, 8.725953194484466380, 1.443375672974078761 ) ) ;
#127399 = CARTESIAN_POINT ( 'NONE',  ( 0.6823417656249882723, 0.2385416670080825474, -1.181850606188749264 ) ) ;
#127400 = CARTESIAN_POINT ( 'NONE',  ( 1.441119962213327499, 8.287674021641846522, 3.161270278916411325 ) ) ;
#127401 = CARTESIAN_POINT ( 'NONE',  ( 1.998289267358617671, -0.4583927764671858474, -1.662768097037459869 ) ) ;
#127402 = CARTESIAN_POINT ( 'NONE',  ( 7.289443866002793371, 8.533381260871966134, 1.199719254218452047 ) ) ;
#127403 = CARTESIAN_POINT ( 'NONE',  ( 5.448397627845284141, 7.449826213943242514, 1.599625672291268286 ) ) ;
#127404 = CARTESIAN_POINT ( 'NONE',  ( -11.95482478513894087, 9.001061590107186206, -0.6098180090666859288 ) ) ;
#127405 = CARTESIAN_POINT ( 'NONE',  ( 0.9481069621972251227, 0.5063937300482551640, 1.695761627633844304 ) ) ;
#127406 = CARTESIAN_POINT ( 'NONE',  ( 1.629542719884415680, -0.2443838731654828789, 1.998128341252780604 ) ) ;
#127407 = CARTESIAN_POINT ( 'NONE',  ( 1.734723475976807094E-15, 2.499999999999998668, 0.000000000000000000 ) ) ;
#127408 = CARTESIAN_POINT ( 'NONE',  ( 4.137865722265689605, -1.519559189622637252, -1.600479987451455699 ) ) ;
#127409 = CIRCLE ( 'NONE', #151447, 11.09999999999999964 ) ;
#127410 = CARTESIAN_POINT ( 'NONE',  ( 4.909118719746323301, -1.747747579089290237, 1.287847701716714255 ) ) ;
#127411 = VERTEX_POINT ( 'NONE', #133351 ) ;
#127412 = CARTESIAN_POINT ( 'NONE',  ( 0.7499999999999867883, -0.9333333333333138082, -1.299038105676652011 ) ) ;
#127413 = CARTESIAN_POINT ( 'NONE',  ( 9.232739420781973294, 9.873876867108206667, -0.7216878364870257245 ) ) ;
#127415 = CARTESIAN_POINT ( 'NONE',  ( 3.409779952838042583, -1.203371721269937744, -1.617806234278630573 ) ) ;
#127414 = CARTESIAN_POINT ( 'NONE',  ( 3.018346832952636394, -2.117961878424143407, 0.1061830045200745365 ) ) ;
#127417 = EDGE_LOOP ( 'NONE', ( #35013, #171963, #57042, #97055, #71101, #136270, #146807, #131417, #210244, #41870, #166664, #122936, #114056, #7408, #207270, #98733, #191234, #185951 ) ) ;
#127416 = CARTESIAN_POINT ( 'NONE',  ( 2.953145165254339233, -1.595657772652997464, 0.8577772064107972438 ) ) ;
#127418 = CARTESIAN_POINT ( 'NONE',  ( 5.027041095616958444, 9.086908054853605421, 0.000000000000000000 ) ) ;
#127419 = ORIENTED_EDGE ( 'NONE', *, *, #82451, .F. ) ;
#127420 = EDGE_CURVE ( 'NONE', #109058, #168888, #165885, .T. ) ;
#127421 = DIRECTION ( 'NONE',  ( 0.000000000000000000, 1.000000000000000000, 0.000000000000000000 ) ) ;
#127422 = CARTESIAN_POINT ( 'NONE',  ( 4.473300617505036492, 7.306268922809479704, -1.199719254218452047 ) ) ;
#127423 = CARTESIAN_POINT ( 'NONE',  ( 5.900976575431972293, 1.489821718068456979, -1.054992404821846863 ) ) ;
#127425 = CARTESIAN_POINT ( 'NONE',  ( 1.446349702961244876, -1.352062789758176731, 1.357433777346368498 ) ) ;
#127424 = CARTESIAN_POINT ( 'NONE',  ( -4.548924232584923288, 5.265832011892554121, -1.199719254218446718 ) ) ;
#127427 = VECTOR ( 'NONE', #189976, 1000.000000000000000 ) ;
#127426 = CIRCLE ( 'NONE', #175747, 12.00000000000000178 ) ;
#127428 = DIRECTION ( 'NONE',  ( 0.000000000000000000, 0.000000000000000000, -1.000000000000000000 ) ) ;
#127429 = CARTESIAN_POINT ( 'NONE',  ( -4.880680834860089412, 4.940735376530475342, -0.5749358470996156489 ) ) ;
#127430 = B_SPLINE_CURVE_WITH_KNOTS ( 'NONE', 3,
 ( #39085, #26015, #138732, #92126 ),
 .UNSPECIFIED., .F., .F.,
 ( 4, 4 ),
 ( 0.0001555421464865875856, 0.0001737658007497212376 ),
 .UNSPECIFIED. ) ;
#127431 = CARTESIAN_POINT ( 'NONE',  ( 0.6823417656249899377, 1.655208333674752730, 1.181850606188755259 ) ) ;
#127432 = CARTESIAN_POINT ( 'NONE',  ( -4.733481511527885210, 4.890303307122107590, -0.5491554243041256722 ) ) ;
#127433 = CARTESIAN_POINT ( 'NONE',  ( -7.862839020921525091, 11.26073039346208660, -1.199719254218446718 ) ) ;
#127434 = CARTESIAN_POINT ( 'NONE',  ( 4.997027575558513846, 1.799266821141291661, -1.197868618907194316 ) ) ;
#127435 = CARTESIAN_POINT ( 'NONE',  ( -5.966997003790240228, 6.134120390609613338, -0.7216878364870338292 ) ) ;
#127436 = CARTESIAN_POINT ( 'NONE',  ( -5.749539660647037032, 8.865490816466966351, 1.199719254218454489 ) ) ;
#127437 = CARTESIAN_POINT ( 'NONE',  ( 3.551138032611600437, 0.3147205237276836653, 2.097014573754731881 ) ) ;
#127439 = CARTESIAN_POINT ( 'NONE',  ( -12.93484866278744150, 7.732355869717920882, 1.092763313629060873 ) ) ;
#127438 = CARTESIAN_POINT ( 'NONE',  ( 1.347111479062088799E-15, 0.000000000000000000, -11.00000000000000178 ) ) ;
#127440 = CARTESIAN_POINT ( 'NONE',  ( 4.077382496314372773, 1.857369029195341525, -0.6610406152272005897 ) ) ;
#127441 = CARTESIAN_POINT ( 'NONE',  ( 6.187759705938407073, 1.828009178079874841, -0.5617473972939349691 ) ) ;
#127442 = VERTEX_POINT ( 'NONE', #117126 ) ;
#127443 = CARTESIAN_POINT ( 'NONE',  ( 5.612555052430599822, 2.041346303960121400, 0.5620598648080311621 ) ) ;
#127444 = LINE ( 'NONE', #129570, #80493 ) ;
#127445 = CARTESIAN_POINT ( 'NONE',  ( 6.830521637698823589, -1.212721230272953754, 1.552361911452035503 ) ) ;
#127446 = CARTESIAN_POINT ( 'NONE',  ( 2.150241637240562831, -1.501185980473922488, 1.231905181128474691 ) ) ;
#127447 = VERTEX_POINT ( 'NONE', #85628 ) ;
#127448 = CARTESIAN_POINT ( 'NONE',  ( -2.986538976760251263, 6.706322249520737522, -0.7998128361456481317 ) ) ;
#127449 = CARTESIAN_POINT ( 'NONE',  ( 5.203297092594585393, 9.292540051327542017, 0.7998128361456341429 ) ) ;
#127451 = CARTESIAN_POINT ( 'NONE',  ( 5.282873410819217241, 9.315102745931094219, -0.7998128361456281477 ) ) ;
#127450 = CARTESIAN_POINT ( 'NONE',  ( 3.082061393860520138, -2.059794914563463308, -0.3567947225071969042 ) ) ;
#127452 = CARTESIAN_POINT ( 'NONE',  ( 6.016786309414542622, 10.24161080428416426, 0.7998128361456341429 ) ) ;
#127454 = ORIENTED_EDGE ( 'NONE', *, *, #79113, .F. ) ;
#127453 = CARTESIAN_POINT ( 'NONE',  ( 0.06471810551328219252, -1.456173922333989790, 1.077237379209189827 ) ) ;
#127455 = CARTESIAN_POINT ( 'NONE',  ( 5.110101661328442901, -2.196521081226535443, 0.2136625748923453583 ) ) ;
#127456 = CARTESIAN_POINT ( 'NONE',  ( -0.3891817118476354476, -6.836286050427575312, -10.85699613887067549 ) ) ;
#127457 = CARTESIAN_POINT ( 'NONE',  ( 3.663272223086514234, -1.945104670120747059, -1.042327912031751458 ) ) ;
#127458 = CARTESIAN_POINT ( 'NONE',  ( 8.772289083241844310, 10.19309100432570148, -1.199719254218446718 ) ) ;
#127459 = DIRECTION ( 'NONE',  ( -0.000000000000000000, -0.000000000000000000, -1.000000000000000000 ) ) ;
#127460 = CARTESIAN_POINT ( 'NONE',  ( 1.893074787327468700, -0.09523556418119562272, -1.910042277862213034 ) ) ;
#127461 = CIRCLE ( 'NONE', #155053, 0.05000000000000056483 ) ;
#127462 = CARTESIAN_POINT ( 'NONE',  ( 10.09812548408005384, 10.67556790771522124, -0.7998128361456281477 ) ) ;
#127463 = CARTESIAN_POINT ( 'NONE',  ( 5.775854211382815073, -2.020734006234246927, 0.4499205674863211990 ) ) ;
#127465 = CARTESIAN_POINT ( 'NONE',  ( 2.958072429731006370, 2.151414462573512765, -0.2105227563667099733 ) ) ;
#127464 = CARTESIAN_POINT ( 'NONE',  ( 1.550536438491937563, 8.693843051952859113, -2.505472492508726834 ) ) ;
#127466 = CARTESIAN_POINT ( 'NONE',  ( 5.179302069984247581, 1.471482994053765925, 1.624232740060495228 ) ) ;
#127467 = ORIENTED_EDGE ( 'NONE', *, *, #179709, .F. ) ;
#127468 = CARTESIAN_POINT ( 'NONE',  ( 10.58621901417202515, 11.24501035948919991, -0.7998128361456281477 ) ) ;
#127469 = AXIS2_PLACEMENT_3D ( 'NONE', #135612, #120496, #23963 ) ;
#127470 = CYLINDRICAL_SURFACE ( 'NONE', #110923, 11.10000000000000142 ) ;
#127471 = CARTESIAN_POINT ( 'NONE',  ( -0.3176981287468134685, 7.220460999378147449, 2.081427265489085521 ) ) ;
#127472 = CARTESIAN_POINT ( 'NONE',  ( 6.222266154028957885, 6.224008365980749247, 0.7998128361456352531 ) ) ;
#127473 = CARTESIAN_POINT ( 'NONE',  ( 3.285556943749998737, -2.792708332855373676, -1.896917185911906722 ) ) ;
#127474 = DIRECTION ( 'NONE',  ( 0.000000000000000000, 1.000000000000000000, 0.000000000000000000 ) ) ;
#127475 = CARTESIAN_POINT ( 'NONE',  ( 0.2467204944939948574, 1.994070950632735428, -0.2986300710981006357 ) ) ;
#127476 = CARTESIAN_POINT ( 'NONE',  ( -7.185458225562757484, 11.32685899655781903, 0.7216878364870458196 ) ) ;
#127477 = CARTESIAN_POINT ( 'NONE',  ( 4.376249722160992839, 8.327651452488305850, 0.000000000000000000 ) ) ;
#127478 = CARTESIAN_POINT ( 'NONE',  ( 5.155165671438199482, 1.724248240607465732, -1.145533019084030268 ) ) ;
#127479 = CARTESIAN_POINT ( 'NONE',  ( 3.035679594228014810, -1.294101122711612151, -1.427291446562365618 ) ) ;
#127480 = CARTESIAN_POINT ( 'NONE',  ( -0.1409997244346088141, -0.002808977843308038680, -2.000147647483838220 ) ) ;
#127481 = CARTESIAN_POINT ( 'NONE',  ( 4.689424523294686509, 8.358602041046323095, -0.7454045323363468478 ) ) ;
#127482 = CARTESIAN_POINT ( 'NONE',  ( 4.904298879841284098, 6.744767997946721216, 1.599625672291267398 ) ) ;
#127483 = CARTESIAN_POINT ( 'NONE',  ( -5.290478191143363595, 6.407017486086630242, -1.170018636208163043 ) ) ;
#127484 = CARTESIAN_POINT ( 'NONE',  ( 3.713681502677267154, 0.4829771288026918907, -1.909149233777557075 ) ) ;
#127485 = CARTESIAN_POINT ( 'NONE',  ( 0.006183538434290089709, -0.9405624870862170361, -1.977291442860461768 ) ) ;
#127486 = CARTESIAN_POINT ( 'NONE',  ( 3.844227010333609584, 1.817057058749595777, 0.1772887374331885701 ) ) ;
#127487 = CARTESIAN_POINT ( 'NONE',  ( 6.211043768836170820, 9.299949259400630552, 1.082531754730549967 ) ) ;
#127488 = CARTESIAN_POINT ( 'NONE',  ( 3.836594282542920009, 4.538743420130594508, 1.082531754730560403 ) ) ;
#127489 = CARTESIAN_POINT ( 'NONE',  ( -7.065734331377342414, 8.272386803808890576, -1.199719254218452047 ) ) ;
#127490 = CARTESIAN_POINT ( 'NONE',  ( 3.881377115262159894, 7.750300077773022878, 0.7998128361456271485 ) ) ;
#127491 = ORIENTED_EDGE ( 'NONE', *, *, #93697, .T. ) ;
#127493 = CARTESIAN_POINT ( 'NONE',  ( 4.623295736497193609, 1.753618999902604614, 0.9886709913553303197 ) ) ;
#127492 = CARTESIAN_POINT ( 'NONE',  ( 1.452429406588066740, -1.579491434881035827, -0.9459884711465746943 ) ) ;
#127494 = CARTESIAN_POINT ( 'NONE',  ( 0.5096300131263042932, 2.292432092913086361, 0.1664806320332279099 ) ) ;
#127495 = CARTESIAN_POINT ( 'NONE',  ( 5.700043108275813175, 0.7984002208856562088, -1.792138013221859394 ) ) ;
#127496 = CARTESIAN_POINT ( 'NONE',  ( -7.217017841176048165, 7.314275657660511243, 1.040834085586084257E-14 ) ) ;
#127497 = DIRECTION ( 'NONE',  ( 1.000000000000000000, -0.000000000000000000, -0.000000000000000000 ) ) ;
#127498 = CARTESIAN_POINT ( 'NONE',  ( -2.937312835655025101, 6.578615408239493867, 1.040834085586084257E-14 ) ) ;
#127499 = CARTESIAN_POINT ( 'NONE',  ( -8.064677165291197269, -5.223431457505076203, 7.446209719563364082 ) ) ;
#127500 = CARTESIAN_POINT ( 'NONE',  ( -6.134138155540168391, 6.121192367743780949, 0.000000000000000000 ) ) ;
#127502 = CARTESIAN_POINT ( 'NONE',  ( 6.491055376221456008, 1.537463663300852490, -0.8764918771043300749 ) ) ;
#127501 = CARTESIAN_POINT ( 'NONE',  ( 1.628582148955775910, 0.2080868244966528613, 2.080379227509927542 ) ) ;
#127503 = CARTESIAN_POINT ( 'NONE',  ( -8.966533317356066846, 1.405705671057797757, -7.975201661134190267 ) ) ;
#127504 = CARTESIAN_POINT ( 'NONE',  ( -0.2102771530458459603, 1.310786636098780544, -2.452585248267840967 ) ) ;
#127505 = CARTESIAN_POINT ( 'NONE',  ( 1.768729326414076430, 1.665373798791164317, -0.5055230280728554293 ) ) ;
#127506 =( GEOMETRIC_REPRESENTATION_CONTEXT ( 3 ) GLOBAL_UNCERTAINTY_ASSIGNED_CONTEXT ( ( #168477 ) ) GLOBAL_UNIT_ASSIGNED_CONTEXT ( ( #97201, #1774, #129766 ) ) REPRESENTATION_CONTEXT ( 'NONE', 'WORKASPACE' ) );
#127507 = CARTESIAN_POINT ( 'NONE',  ( 6.335737856287750880, 6.286115675290828264, -0.7998128361456281477 ) ) ;
#127509 = CARTESIAN_POINT ( 'NONE',  ( 1.527330013470509673, 8.693738994866436087, 2.519751708053329153 ) ) ;
#127508 = DIRECTION ( 'NONE',  ( 0.000000000000000000, 0.000000000000000000, -1.000000000000000000 ) ) ;
#127510 = CARTESIAN_POINT ( 'NONE',  ( 2.121340078736310364, -1.673401575455361723, 0.4176718278932553541 ) ) ;
#127511 = CARTESIAN_POINT ( 'NONE',  ( 1.945129482973105839, -1.762486321751283835, -1.302348873264857820 ) ) ;
#127512 = CARTESIAN_POINT ( 'NONE',  ( 4.319099500008596770, 2.017107695584336557, 0.8957252843501888329 ) ) ;
#127513 = DIRECTION ( 'NONE',  ( 0.000000000000000000, -8.673617379884026597E-16, -1.000000000000000000 ) ) ;
#127514 = CARTESIAN_POINT ( 'NONE',  ( 2.711994142844989408, 0.5828001693900261015, -2.091290491527279194 ) ) ;
#127515 = CARTESIAN_POINT ( 'NONE',  ( 1.137010146156680834, -1.651496384925277283, 0.7785749969668461778 ) ) ;
#127516 = CARTESIAN_POINT ( 'NONE',  ( 3.309862381128574338, -1.264700674563856264, -1.697971918580774675 ) ) ;
#127517 = CARTESIAN_POINT ( 'NONE',  ( 6.539320575229228716, 1.281788455817688188, 2.013036689384885225 ) ) ;
#127518 = ORIENTED_EDGE ( 'NONE', *, *, #153552, .F. ) ;
#127519 = CIRCLE ( 'NONE', #169005, 6.449999999999992184 ) ;
#127521 = CARTESIAN_POINT ( 'NONE',  ( -1.402160292154681736E-14, 1.759375000341421469, -1.575800808251659024 ) ) ;
#127520 = CARTESIAN_POINT ( 'NONE',  ( 3.140441720415044546, 0.5589363893779492054, 2.223061277538174174 ) ) ;
#127522 =( NAMED_UNIT ( * ) SI_UNIT ( $, .STERADIAN. ) SOLID_ANGLE_UNIT ( ) );
#127523 = CARTESIAN_POINT ( 'NONE',  ( 4.864678189204997949, 4.569879397027603929, 0.7998128361456341429 ) ) ;
#127524 = CARTESIAN_POINT ( 'NONE',  ( 5.760436963792294307, 2.218610086356072930, 0.1113587401332209043 ) ) ;
#127525 = CARTESIAN_POINT ( 'NONE',  ( -5.422898255786186006, 9.270539031818461950, -0.7216878364870207285 ) ) ;
#127526 = CARTESIAN_POINT ( 'NONE',  ( 4.446711195602238931, 6.210915699667823198, -1.443375672974051449 ) ) ;
#127527 = CARTESIAN_POINT ( 'NONE',  ( -5.653386866774179786, 8.579073197003079798, 1.082531754730548412 ) ) ;
#127528 = CARTESIAN_POINT ( 'NONE',  ( 6.825078400183575589, 7.629137130509070275, 2.455651831298297338 ) ) ;
#127529 = ORIENTED_EDGE ( 'NONE', *, *, #152899, .T. ) ;
#127530 = CARTESIAN_POINT ( 'NONE',  ( 3.727185537919291747, 2.006959858346604619, 0.1948421285040344286 ) ) ;
#127532 = CARTESIAN_POINT ( 'NONE',  ( 2.659094170149599368, 1.659314987522000795, -1.224949181800268017 ) ) ;
#127531 = CARTESIAN_POINT ( 'NONE',  ( 6.205881626753210867, 8.263281202677319470, 1.599625672291281386 ) ) ;
#127533 = CARTESIAN_POINT ( 'NONE',  ( 6.966220764712121927, 6.002124920821316323, 2.420000000000000373 ) ) ;
#127534 = CARTESIAN_POINT ( 'NONE',  ( 5.031484404002889654, 6.003058238492422483, 1.082531754730549078 ) ) ;
#127535 = CARTESIAN_POINT ( 'NONE',  ( 3.285556943749998737, -2.705208332855374209, -1.896917185911906500 ) ) ;
#127536 = CARTESIAN_POINT ( 'NONE',  ( -0.6823417656249969321, 5.467708333674756283, -1.181850606188749264 ) ) ;
#127537 = CARTESIAN_POINT ( 'NONE',  ( 4.699289266375740404, -0.5861454505808120219, 2.111544493182772708 ) ) ;
#127538 = CARTESIAN_POINT ( 'NONE',  ( 2.408827471728996361, -1.163269702728772392, -1.646838680093346996 ) ) ;
#127539 = CARTESIAN_POINT ( 'NONE',  ( 1.874305484616908934, -0.09156810461483089192, -1.839108553062768214 ) ) ;
#127540 = CARTESIAN_POINT ( 'NONE',  ( 5.933664784275179294, 10.07435934829639912, -0.7998128361456291469 ) ) ;
#127541 = PRESENTATION_STYLE_ASSIGNMENT (( #112334 ) ) ;
#127542 = CARTESIAN_POINT ( 'NONE',  ( 6.704125975539116489, -1.825092170400946845, 0.04854515157103055090 ) ) ;
#127543 = CARTESIAN_POINT ( 'NONE',  ( 0.1066027571702803795, -0.1042336552941041522, 2.296444677329109840 ) ) ;
#127544 = CARTESIAN_POINT ( 'NONE',  ( -6.015013705957189316, 10.16926642359206134, 0.7998128361456481317 ) ) ;
#127546 = CARTESIAN_POINT ( 'NONE',  ( -4.294900800479008574, 8.232744377192641849, 0.000000000000000000 ) ) ;
#127545 = CARTESIAN_POINT ( 'NONE',  ( 5.225545412997908201, -2.150153479602398221, 0.7043797957921889008 ) ) ;
#127547 = CARTESIAN_POINT ( 'NONE',  ( 0.3640743269037312602, 2.082829956593022835, -0.3111531555848711106 ) ) ;
#127548 = CARTESIAN_POINT ( 'NONE',  ( -6.237633190739009237, 9.434933268240943249, 1.199719254218452047 ) ) ;
#127549 = CARTESIAN_POINT ( 'NONE',  ( 8.263858322729371153, 9.599921783727809910, -1.199719254218446718 ) ) ;
#127550 = CARTESIAN_POINT ( 'NONE',  ( 5.953438849732186178, 8.999410187112612647, -1.082531754730548412 ) ) ;
#127551 = DIRECTION ( 'NONE',  ( 0.9120491373041518246, 0.000000000000000000, 0.4100809324301146752 ) ) ;
#127553 = EDGE_CURVE ( 'NONE', #121557, #41100, #157968, .T. ) ;
#127552 = CARTESIAN_POINT ( 'NONE',  ( -8.389798128758148010, 8.682519326506312751, 0.7998128361456462443 ) ) ;
#127554 = UNCERTAINTY_MEASURE_WITH_UNIT (LENGTH_MEASURE( 1.000000000000000082E-05 ), #74308, 'distance_accuracy_value', 'NONE');
#127555 = DIRECTION ( 'NONE',  ( 0.000000000000000000, 0.000000000000000000, -1.000000000000000000 ) ) ;
#127556 = CARTESIAN_POINT ( 'NONE',  ( 7.415946836550722843, 8.714654733139752807, 1.082531754730558626 ) ) ;
#127557 = CARTESIAN_POINT ( 'NONE',  ( 4.044190953901719787, 7.767772900817621284, 0.4663397696828552874 ) ) ;
#127558 = CARTESIAN_POINT ( 'NONE',  ( -7.687109909268394325, 11.91211929421440097, 0.000000000000000000 ) ) ;
#127560 = CARTESIAN_POINT ( 'NONE',  ( 3.393049125975013069, -2.141818966976690497, -0.5891788363768469816 ) ) ;
#127559 = CARTESIAN_POINT ( 'NONE',  ( 1.793382672576701919, -0.1090974814243403090, -2.117938670719583527 ) ) ;
#127561 = CARTESIAN_POINT ( 'NONE',  ( -0.4000000000000513700, 3.949999999999967315, 0.8338124244295243015 ) ) ;
#127562 = CARTESIAN_POINT ( 'NONE',  ( -4.613517410400161722, 8.604463755433990002, -0.7998128361456362523 ) ) ;
#127563 = CARTESIAN_POINT ( 'NONE',  ( 5.769158057814842699, 6.689438141327490150, 1.199719254218462483 ) ) ;
#127564 = CARTESIAN_POINT ( 'NONE',  ( 3.982823771651412770, 1.862158852298421152, 0.6176278068941787325 ) ) ;
#127565 = CARTESIAN_POINT ( 'NONE',  ( 10.06423010004587759, 10.63602329300870153, 0.000000000000000000 ) ) ;
#127566 = CARTESIAN_POINT ( 'NONE',  ( -5.660981573724272131, 6.153771497223376130, 0.8018600159674215133 ) ) ;
#127567 = CARTESIAN_POINT ( 'NONE',  ( 2.333974999846879061, 5.874721266463329705, -0.7998128361456291469 ) ) ;
#127568 = CARTESIAN_POINT ( 'NONE',  ( -3.689227196694341515, 7.318199139536432973, -0.7216878364870458196 ) ) ;
#127570 = ORIENTED_EDGE ( 'NONE', *, *, #76439, .T. ) ;
#127569 = CARTESIAN_POINT ( 'NONE',  ( -7.890482213473404727, 8.307910125248191946, 0.7216878364870578100 ) ) ;
#127572 = CARTESIAN_POINT ( 'NONE',  ( 3.111701630267147412, 1.674174984267240429, 1.301503359413098249 ) ) ;
#127571 = AXIS2_PLACEMENT_3D ( 'NONE', #90916, #174305, #109354 ) ;
#127573 = CARTESIAN_POINT ( 'NONE',  ( -4.285259070371116863, 7.157163461145040095, 1.199719254218452935 ) ) ;
#127574 = CARTESIAN_POINT ( 'NONE',  ( 4.346650381253648554, 0.5737703434565506466, 2.084106190491950006 ) ) ;
#127575 = CARTESIAN_POINT ( 'NONE',  ( 4.352959896991869471, 0.3989296284454147412, -1.797357466088687961 ) ) ;
#127576 = CARTESIAN_POINT ( 'NONE',  ( -4.245236785304952853, 7.324258608653995140, 0.8904289178662868620 ) ) ;
#127577 = CARTESIAN_POINT ( 'NONE',  ( -1.364683531250014514, -0.4489583329919089039, -0.7879004041258359514 ) ) ;
#127578 = CARTESIAN_POINT ( 'NONE',  ( 5.788919933143140462, 1.322006966288125085, 1.131936178618123456 ) ) ;
#127579 = CARTESIAN_POINT ( 'NONE',  ( -10.91944002402978775, -9.900000000000005684, 0.1105873483556694958 ) ) ;
#127580 = CARTESIAN_POINT ( 'NONE',  ( 4.867013957625893283, 4.780530493426062399, 1.040834085586084257E-14 ) ) ;
#127581 = CARTESIAN_POINT ( 'NONE',  ( -0.7499999999999972244, 3.639583334016149863, -1.299038105676652011 ) ) ;
#127582 = CARTESIAN_POINT ( 'NONE',  ( 3.151412294154242844, -1.766339975446712174, -1.245920677233211871 ) ) ;
#127583 = CARTESIAN_POINT ( 'NONE',  ( 5.307970166423544356, -1.730600239375930549, 1.034008556546859969 ) ) ;
#127584 = CARTESIAN_POINT ( 'NONE',  ( -10.12757755928392456, 10.91785469536048758, 0.7216878364870438212 ) ) ;
#127585 = VECTOR ( 'NONE', #83073, 1000.000000000000000 ) ;
#127586 = CARTESIAN_POINT ( 'NONE',  ( 2.782270202741622178, -1.112240752214749273, 1.853481441253836071 ) ) ;
#127587 = EDGE_CURVE ( 'NONE', #77611, #155158, #163296, .T. ) ;
#127589 = CARTESIAN_POINT ( 'NONE',  ( 3.374254075663080332, -1.176934739253515438, 1.581319453489488325 ) ) ;
#127588 = B_SPLINE_CURVE_WITH_KNOTS ( 'NONE', 1,
 ( #115081, #95603 ),
 .UNSPECIFIED., .F., .F.,
 ( 2, 2 ),
 ( 0.7585745852332145267, 1.000000000000000000 ),
 .UNSPECIFIED. ) ;
#127590 = CARTESIAN_POINT ( 'NONE',  ( 4.845229750085990439, 0.6055439843271113176, -1.845326283916528753 ) ) ;
#127593 = ORIENTED_EDGE ( 'NONE', *, *, #95578, .T. ) ;
#127592 =( NAMED_UNIT ( * ) SI_UNIT ( $, .STERADIAN. ) SOLID_ANGLE_UNIT ( ) );
#127591 = CARTESIAN_POINT ( 'NONE',  ( -8.798878505144649864, 11.28844422746735532, -1.443375672974058777 ) ) ;
#127594 = CARTESIAN_POINT ( 'NONE',  ( -6.577640801285370209, 7.702944352034914566, -1.199719254218452047 ) ) ;
#127595 = FACE_OUTER_BOUND ( 'NONE', #190694, .T. ) ;
#127597 = VERTEX_POINT ( 'NONE', #150650 ) ;
#127596 = CARTESIAN_POINT ( 'NONE',  ( -3.494969737272722643, 7.299491470118629088, -0.7998128361456481317 ) ) ;
#127598 = CARTESIAN_POINT ( 'NONE',  ( -7.659993601596710278, 10.92011438762942355, -1.082531754730543083 ) ) ;
#127599 = CARTESIAN_POINT ( 'NONE',  ( 1.747397587315655088, -1.864034986486883039, 1.180896971623420999 ) ) ;
#127600 = CARTESIAN_POINT ( 'NONE',  ( 3.285556943750000070, -1.334374999522040861, 0.000000000000000000 ) ) ;
#127601 = CARTESIAN_POINT ( 'NONE',  ( 6.139501739389007007, 1.813922436357641388, -0.7475906808915923074 ) ) ;
#127602 = CARTESIAN_POINT ( 'NONE',  ( -0.6823417656250212460, 4.863541667008086655, 1.181850606188767472 ) ) ;
#127603 = CARTESIAN_POINT ( 'NONE',  ( -1.500000000000011324, 4.410416667349484676, -0.8660254037844313801 ) ) ;
#127604 = CARTESIAN_POINT ( 'NONE',  ( 5.763841807162588537, 6.241519824923047466, -1.009562751112670576 ) ) ;
#127606 = CARTESIAN_POINT ( 'NONE',  ( 6.721333373144884327, -0.1645177889858795151, 2.170883633896856679 ) ) ;
#127605 = CARTESIAN_POINT ( 'NONE',  ( 0.07479286986305369589, 0.004866263145587855152, -1.855573292446037970 ) ) ;
#127607 = CARTESIAN_POINT ( 'NONE',  ( 5.841722611436678925, 1.839261846420519708, 0.08593139445873397564 ) ) ;
#127608 = EDGE_LOOP ( 'NONE', ( #122105, #86592, #158759, #155646 ) ) ;
#127609 = CARTESIAN_POINT ( 'NONE',  ( 0.6124999999999741762, 2.729166667349444797, -1.060881119635955327 ) ) ;
#127610 = CARTESIAN_POINT ( 'NONE',  ( -7.670162217029145246, 9.971608557999250166, 1.599625672291295375 ) ) ;
#127611 = DIRECTION ( 'NONE',  ( 0.000000000000000000, -1.000000000000000000, 0.000000000000000000 ) ) ;
#127612 = CARTESIAN_POINT ( 'NONE',  ( 6.170199167347634628, 2.114832956739281400, -0.1575216572810705096 ) ) ;
#127613 = CARTESIAN_POINT ( 'NONE',  ( 11.48899393572690997, 7.332171132234710065, 3.320533030897445670 ) ) ;
#127614 = CARTESIAN_POINT ( 'NONE',  ( 5.823390672269506574, 6.752709524857930745, -1.199719254218446718 ) ) ;
#127615 = CARTESIAN_POINT ( 'NONE',  ( 6.098915436037096960, 1.687290577560787375, -1.182889608693861394 ) ) ;
#127616 =( GEOMETRIC_REPRESENTATION_CONTEXT ( 3 ) GLOBAL_UNCERTAINTY_ASSIGNED_CONTEXT ( ( #84021 ) ) GLOBAL_UNIT_ASSIGNED_CONTEXT ( ( #70164, #51822, #132032 ) ) REPRESENTATION_CONTEXT ( 'NONE', 'WORKASPACE' ) );
#127618 = CARTESIAN_POINT ( 'NONE',  ( 4.054132754448328768, -1.361571661076573792, 1.239656203754435193 ) ) ;
#127617 = CARTESIAN_POINT ( 'NONE',  ( 2.259996020855909116, -1.860750554326926487, 0.04185779618384557338 ) ) ;
#127619 = CARTESIAN_POINT ( 'NONE',  ( 5.459129407796876166, 9.520734742405036144, 1.040834085586084257E-14 ) ) ;
#127620 = CARTESIAN_POINT ( 'NONE',  ( -9.438511317522861432, 14.67479611868992606, -7.309645042966809392 ) ) ;
#127621 = CARTESIAN_POINT ( 'NONE',  ( -5.607179047703544583, 8.699403434699558346, 1.199719254218454489 ) ) ;
#127623 = VERTEX_POINT ( 'NONE', #69352 ) ;
#127622 = CARTESIAN_POINT ( 'NONE',  ( -10.09384670630917746, -7.616807780223579627, 1.138412281109779656E-15 ) ) ;
#127624 = CARTESIAN_POINT ( 'NONE',  ( 3.088704478669739295, -2.174299887604825177, -0.3769171259565203269 ) ) ;
#127625 = CARTESIAN_POINT ( 'NONE',  ( 5.782586711780850486, -2.205454299129143703, -0.5038293679325082097 ) ) ;
#127626 = CARTESIAN_POINT ( 'NONE',  ( -6.738039156311804945, 6.963393225226301553, 1.040834085586084257E-14 ) ) ;
#127627 = CARTESIAN_POINT ( 'NONE',  ( 5.396671993488243224, -1.769204348786549641, -0.3888369506312178703 ) ) ;
#127628 = CARTESIAN_POINT ( 'NONE',  ( 6.473869786608328347, -0.8128310455158479497, 1.733272608194774689 ) ) ;
#127629 = CARTESIAN_POINT ( 'NONE',  ( -2.428612866367529932E-14, 2.800000000000024691, 0.7750000000000117906 ) ) ;
#127630 = CARTESIAN_POINT ( 'NONE',  ( 6.174654088403855212, -1.776896415251895789, -0.5849557326117056366 ) ) ;
#127631 = CARTESIAN_POINT ( 'NONE',  ( 5.549440478958018730, -1.726947976793649975, 0.8215754744917985741 ) ) ;
#127632 = CARTESIAN_POINT ( 'NONE',  ( 4.528060117284232966, 6.305822774963486310, 1.443375672974062551 ) ) ;
#127633 = CARTESIAN_POINT ( 'NONE',  ( 0.9888773766892227091, 1.651582696977689890, -0.8784067438419729257 ) ) ;
#127634 = CARTESIAN_POINT ( 'NONE',  ( 1.534389036647098692, 0.6371565916030231813, 1.913260934284975345 ) ) ;
#127636 = CARTESIAN_POINT ( 'NONE',  ( 3.967482597722607363, 0.2578578757282763978, -2.090148584218749939 ) ) ;
#127635 = CARTESIAN_POINT ( 'NONE',  ( -9.612894607289142357, 11.17379744904754801, -1.199719254218441611 ) ) ;
#127637 = CARTESIAN_POINT ( 'NONE',  ( 7.086107841436786181, 11.41887624831828418, 1.040834085586084257E-14 ) ) ;
#127639 = CARTESIAN_POINT ( 'NONE',  ( -10.00321840878439339, 10.56484298653695397, 1.040834085586084257E-14 ) ) ;
#127638 = CARTESIAN_POINT ( 'NONE',  ( -1.402160292154681736E-14, -0.4124999999999747202, -1.732050807568870754 ) ) ;
#127640 = CARTESIAN_POINT ( 'NONE',  ( 11.44779964734710909, 10.10189529870395830, 3.599999963171363060 ) ) ;
#127641 = CARTESIAN_POINT ( 'NONE',  ( 2.865494903669623117, -1.653614387114977990, -1.159512146270498478 ) ) ;
#127642 = B_SPLINE_CURVE_WITH_KNOTS ( 'NONE', 3,
 ( #168275, #70743, #104354, #102210, #4670, #37206 ),
 .UNSPECIFIED., .F., .F.,
 ( 4, 2, 4 ),
 ( 0.000000000000000000, 0.0003778774010236168619, 0.0007557548020472337237 ),
 .UNSPECIFIED. ) ;
#127643 = CARTESIAN_POINT ( 'NONE',  ( 0.6823417656249899377, 3.676041667008085767, -1.181850606188754593 ) ) ;
#127644 = CARTESIAN_POINT ( 'NONE',  ( 3.816783937446950770, 4.411668334231586996, 1.199719254218464037 ) ) ;
#127645 = CARTESIAN_POINT ( 'NONE',  ( 3.268983376858981327, -1.995845357749256976, -0.8305886511386084692 ) ) ;
#127646 = CARTESIAN_POINT ( 'NONE',  ( -1.981037863234370811, 3.482875600935725569, 0.4617754461038545699 ) ) ;
#127647 = CARTESIAN_POINT ( 'NONE',  ( -1.201851678989727383E-14, 4.587500000000025224, -1.732050807568863648 ) ) ;
#127649 = LINE ( 'NONE', #178448, #162464 ) ;
#127648 = CARTESIAN_POINT ( 'NONE',  ( 7.343676480457483002, 8.596652644402405841, -1.199719254218452047 ) ) ;
#127650 = CARTESIAN_POINT ( 'NONE',  ( 7.063434842595398777, 11.18449838309590483, -0.7216878364870267237 ) ) ;
#127652 = CARTESIAN_POINT ( 'NONE',  ( 7.471610726854514439, 15.41851326508443165, -9.339756462365158995 ) ) ;
#127651 = CARTESIAN_POINT ( 'NONE',  ( 0.4851436980863755299, 2.077851564382672933, 0.6296362999115376891 ) ) ;
#127653 = CARTESIAN_POINT ( 'NONE',  ( -6.236387472606153892, 8.298871356172400127, -1.443375672974059665 ) ) ;
#127654 = CARTESIAN_POINT ( 'NONE',  ( -0.6823417656250212460, 1.551041667008083769, 1.181850606188755259 ) ) ;
#127655 = CARTESIAN_POINT ( 'NONE',  ( 2.015410700679621137, -2.124826835150806392, 0.5361769018528695918 ) ) ;
#127656 = CARTESIAN_POINT ( 'NONE',  ( -0.007601003541780289308, -8.259585062615352413, 10.93184718803891187 ) ) ;
#127657 = CARTESIAN_POINT ( 'NONE',  ( 2.079355054740182229, -0.1115493103639639688, -2.259872350005930119 ) ) ;
#127658 = CARTESIAN_POINT ( 'NONE',  ( -7.100719765255177229, 9.307259030929609267, -1.599625672291263179 ) ) ;
#127659 = CARTESIAN_POINT ( 'NONE',  ( 4.610564714392807240, 1.931124171932835809, 0.5807562064495259690 ) ) ;
#127661 = AXIS2_PLACEMENT_3D ( 'NONE', #180004, #44686, #159477 ) ;
#127660 = CARTESIAN_POINT ( 'NONE',  ( -1.364683531250010295, 5.301041667008085767, -0.7879004041258300672 ) ) ;
#127662 = CARTESIAN_POINT ( 'NONE',  ( 6.017777097630443883, 7.067734144800174256, 1.048426327298467742 ) ) ;
#127663 = CARTESIAN_POINT ( 'NONE',  ( 0.7500000000000006661, 11.91666666666666607, -1.299038105676657340 ) ) ;
#127664 = CARTESIAN_POINT ( 'NONE',  ( 6.373741612200162443, 8.529394195690610303, 1.443375672974065660 ) ) ;
#127665 = CARTESIAN_POINT ( 'NONE',  ( 4.745210919507984570, -1.367539302148174318, -1.123239564495488674 ) ) ;
#127666 = CARTESIAN_POINT ( 'NONE',  ( 7.964525173024008531, 11.37936423758166526, 1.199719254218460707 ) ) ;
#127667 = CARTESIAN_POINT ( 'NONE',  ( 1.132014994273435216, -1.335988328115779167, -1.627952913800976731 ) ) ;
#127668 = CARTESIAN_POINT ( 'NONE',  ( 1.364683531250000303, 9.755208333674735499, -0.7879004041258355073 ) ) ;
#127669 = COLOUR_RGB ( '', 0.66274510, 0.83137255, 0.94901961) ;
#127670 = CARTESIAN_POINT ( 'NONE',  ( -6.134138155540168391, 6.121192367743780949, 0.000000000000000000 ) ) ;
#127671 = CARTESIAN_POINT ( 'NONE',  ( 6.380482474105581225, -0.5405081658083621399, -1.942537888137134461 ) ) ;
#127672 = ORIENTED_EDGE ( 'NONE', *, *, #156042, .F. ) ;
#127673 = ADVANCED_FACE ( 'NONE', ( #170072 ), #81695, .F. ) ;
#127674 = CARTESIAN_POINT ( 'NONE',  ( 9.480175724453529185, 12.08329098332774265, 1.599625672291279388 ) ) ;
#127675 = CARTESIAN_POINT ( 'NONE',  ( 4.205816867194319464, -1.865656749788859647, 0.1373567816406878750 ) ) ;
#127676 = CARTESIAN_POINT ( 'NONE',  ( 2.993098612437726125, 0.2488643248897918769, 2.055149816265568585 ) ) ;
#127677 = CARTESIAN_POINT ( 'NONE',  ( -5.844973620822877969, 7.912498205750389424, 1.443375672974058777 ) ) ;
#127678 = CARTESIAN_POINT ( 'NONE',  ( -0.4153311931459208184, 3.850000000000006306, -0.4999999999999961142 ) ) ;
#127679 = CARTESIAN_POINT ( 'NONE',  ( 9.589694723567584234, 10.08239868711733855, -0.7998128361456281477 ) ) ;
#127680 = CARTESIAN_POINT ( 'NONE',  ( -8.859363311525973117, 12.42334206583395328, -1.199719254218446718 ) ) ;
#127681 = CARTESIAN_POINT ( 'NONE',  ( -5.646002790254049941, 6.144272845372873881, 0.7680594912782515715 ) ) ;
#127682 = CARTESIAN_POINT ( 'NONE',  ( 6.420800710400103917, 2.015122584031241004, 0.7829223626853940576 ) ) ;
#127683 = CARTESIAN_POINT ( 'NONE',  ( -1.364683531250014514, -1.011458332991911568, -0.7879004041258359514 ) ) ;
#127684 = EDGE_CURVE ( 'NONE', #154122, #191521, #98761, .T. ) ;
#127685 = CARTESIAN_POINT ( 'NONE',  ( 3.490630252122446375, 1.913478943654752129, 0.4322817992908413176 ) ) ;
#127686 = CARTESIAN_POINT ( 'NONE',  ( 1.370470000664014254, -0.4925687793003556969, 1.954872606163795989 ) ) ;
#127687 = CARTESIAN_POINT ( 'NONE',  ( -4.981695098378565945, 4.776675467721892332, -0.7998128361456362523 ) ) ;
#127689 = CARTESIAN_POINT ( 'NONE',  ( -11.48243876534946217, 9.799999999999982947, 3.199999999999997957 ) ) ;
#127688 = CARTESIAN_POINT ( 'NONE',  ( 8.945682426918439845, 9.331051007693339727, 1.040834085586084257E-14 ) ) ;
#127690 = CARTESIAN_POINT ( 'NONE',  ( 1.528351178377739927, 1.801267752838480840, 0.5040548479407629401 ) ) ;
#127691 = CARTESIAN_POINT ( 'NONE',  ( 1.364683531249990311, 3.384375000341416140, 1.214306433183764966E-14 ) ) ;
#127692 = CARTESIAN_POINT ( 'NONE',  ( 3.568611400213494989, 0.7284950617309441379, 1.876934371664749301 ) ) ;
#127694 = CARTESIAN_POINT ( 'NONE',  ( 2.724332569758937339, 2.101576450279537767, 0.2563457491038360070 ) ) ;
#127693 = CARTESIAN_POINT ( 'NONE',  ( -6.887178846062128379, 7.137389529935019183, -0.7216878364870278340 ) ) ;
#127695 = CARTESIAN_POINT ( 'NONE',  ( 0.000000000000000000, 2.000000000000001776, 0.000000000000000000 ) ) ;
#127696 = CARTESIAN_POINT ( 'NONE',  ( 4.158688916442685013, -0.6465363538536235133, -1.966910096795893681 ) ) ;
#127697 = CARTESIAN_POINT ( 'NONE',  ( 6.156284269057003655, 9.340026192945279249, -1.199719254218452047 ) ) ;
#127699 = CARTESIAN_POINT ( 'NONE',  ( 11.89317557362561217, 13.76275843837575152, 1.599935658895948576 ) ) ;
#127698 = CARTESIAN_POINT ( 'NONE',  ( 0.1872078708128835645, 1.551958633911882934, 1.401156373025253421 ) ) ;
#127701 = ORIENTED_EDGE ( 'NONE', *, *, #44659, .F. ) ;
#127700 = CARTESIAN_POINT ( 'NONE',  ( 5.245057492501287832, -1.564903486862476489, 0.9398553879134128319 ) ) ;
#127702 = CARTESIAN_POINT ( 'NONE',  ( 7.079328764629950754, 11.41096732537697633, 0.7998128361456462443 ) ) ;
#127703 = CARTESIAN_POINT ( 'NONE',  ( -4.858757509019071996, 5.629766575900002401, 7.500000000000000000 ) ) ;
#127704 = CARTESIAN_POINT ( 'NONE',  ( 10.20276969027985992, 13.21904656514576004, -7.144040684766732596 ) ) ;
#127705 = CARTESIAN_POINT ( 'NONE',  ( 6.018643902988223715, 1.486383190695803158, -1.631276885294789203 ) ) ;
#127706 = CARTESIAN_POINT ( 'NONE',  ( -0.6823417656250039265, 11.38020833367473017, -1.181850606188755259 ) ) ;
#127707 = CARTESIAN_POINT ( 'NONE',  ( 5.637344576021464881, -0.04253375892994575719, 1.911971901805488816 ) ) ;
#127708 = CARTESIAN_POINT ( 'NONE',  ( -8.188234707649510113, 11.64035869464474082, -1.199719254218446718 ) ) ;
#127709 = CIRCLE ( 'NONE', #124161, 0.07999999999999998779 ) ;
#127710 = CARTESIAN_POINT ( 'NONE',  ( 5.472687561410540802, 9.536552588287639409, 0.7998128361456462443 ) ) ;
#127711 = CARTESIAN_POINT ( 'NONE',  ( -0.6801582343750420812, 2.713541667008087632, 1.178068619123787908 ) ) ;
#127712 = CARTESIAN_POINT ( 'NONE',  ( 3.673896439178923057, 5.309298483840612093, 1.443375672974066548 ) ) ;
#127713 = EDGE_CURVE ( 'NONE', #1871, #33092, #41172, .T. ) ;
#127714 = SURFACE_SIDE_STYLE ('',( #129834 ) ) ;
#127715 = CARTESIAN_POINT ( 'NONE',  ( 5.522248639467795428, 5.337044922334209573, -0.7998128361456231517 ) ) ;
#127716 = ORIENTED_EDGE ( 'NONE', *, *, #4614, .T. ) ;
#127717 = CARTESIAN_POINT ( 'NONE',  ( -6.717278222822391953, -7.246166700180828535, 6.830415307812263137 ) ) ;
#127718 = CARTESIAN_POINT ( 'NONE',  ( -0.02319159430947542386, 0.2540490248266329965, -1.846305437520213477 ) ) ;
#127719 = CARTESIAN_POINT ( 'NONE',  ( 4.844006021832467646, 8.873367135438366304, 0.000000000000000000 ) ) ;
#127720 = CARTESIAN_POINT ( 'NONE',  ( -0.3870072406890526229, 1.529612873802630002, 11.82510647457161923 ) ) ;
#127721 = CIRCLE ( 'NONE', #172164, 0.07999999999999975187 ) ;
#127722 = CARTESIAN_POINT ( 'NONE',  ( -6.220586654761008027, 6.942393398233093649, 0.8502372543972673835 ) ) ;
#127723 = CARTESIAN_POINT ( 'NONE',  ( -6.914295153289458540, 7.169025221700239925, 0.7216878364870317197 ) ) ;
#127724 = CARTESIAN_POINT ( 'NONE',  ( 4.708759422647839976, 4.387974169377582001, -0.7998128361456211532 ) ) ;
#127725 = CARTESIAN_POINT ( 'NONE',  ( 2.641402650619076198, 1.802640082279869382, -0.7936183362749064107 ) ) ;
#127726 = EDGE_CURVE ( 'NONE', #148041, #4447, #154549, .T. ) ;
#127727 = CARTESIAN_POINT ( 'NONE',  ( 3.778922869151004171, 1.701937167235707982, -1.081084515101193633 ) ) ;
#127728 = CARTESIAN_POINT ( 'NONE',  ( -5.845536785786364931, 9.971543350059432598, 0.000000000000000000 ) ) ;
#127729 = CARTESIAN_POINT ( 'NONE',  ( 6.229045230835819069, 6.231917288922055320, -0.7998128361456481317 ) ) ;
#127730 = CARTESIAN_POINT ( 'NONE',  ( 6.727182134110236689, 0.5535242275785922095, 2.340336476220133743 ) ) ;
#127731 = CARTESIAN_POINT ( 'NONE',  ( 3.521585679250069045, -1.305302140894725627, -1.760141160621036649 ) ) ;
#127732 = DIRECTION ( 'NONE',  ( -5.578564026256490882E-16, -1.000000000000000000, -9.066213480720158442E-32 ) ) ;
#127733 = CARTESIAN_POINT ( 'NONE',  ( 2.502848596126582059, 1.548454276800725449, -1.145803370841493418 ) ) ;
#127734 = CARTESIAN_POINT ( 'NONE',  ( -7.811469059767924605, 12.26513100303794168, -0.7998128361456281477 ) ) ;
#127735 = EDGE_CURVE ( 'NONE', #87955, #166237, #64559, .T. ) ;
#127736 = CARTESIAN_POINT ( 'NONE',  ( -0.1296875068447882473, 5.724785194352729256, -2.420566058096422779 ) ) ;
#127737 = CARTESIAN_POINT ( 'NONE',  ( 0.2333540202161349941, 2.877056899079268870, -2.534299598574590640 ) ) ;
#127738 = LINE ( 'NONE', #212061, #51663 ) ;
#127739 = CARTESIAN_POINT ( 'NONE',  ( 8.446893396513862839, 9.813462703143045474, -1.199719254218445830 ) ) ;
#127740 = CARTESIAN_POINT ( 'NONE',  ( 6.148786358997489820, 7.132337826040578754, -1.199719254218446718 ) ) ;
#127741 = CARTESIAN_POINT ( 'NONE',  ( 2.703961570921634028, 5.242040035128820108, -1.199719254218446718 ) ) ;
#127742 = CARTESIAN_POINT ( 'NONE',  ( 6.726253606155519371, 7.019919760035800316, -0.7216878364870458196 ) ) ;
#127743 = ORIENTED_EDGE ( 'NONE', *, *, #136398, .F. ) ;
#127745 = CARTESIAN_POINT ( 'NONE',  ( 1.611978021082097978, -0.6760664726842831040, 1.896312242100234524 ) ) ;
#127744 = CARTESIAN_POINT ( 'NONE',  ( 5.267088776126935379, 1.772936381825638952, -0.4966186330585887210 ) ) ;
#127746 = CARTESIAN_POINT ( 'NONE',  ( 4.446792056507931079, 1.496784378905056334, 1.744297655265887537 ) ) ;
#127748 = CARTESIAN_POINT ( 'NONE',  ( 2.412761291957177701, -1.442071615443579091, 1.176286876380010726 ) ) ;
#127747 = CARTESIAN_POINT ( 'NONE',  ( -0.1291982275798392032, 1.351143144720265532, -2.329141727150272789 ) ) ;
#127749 = CARTESIAN_POINT ( 'NONE',  ( -1.642778471874998480, -2.851041666188706802, 2.845375778867863303 ) ) ;
#127750 = CARTESIAN_POINT ( 'NONE',  ( -9.608224290795256195, 15.11803043437814331, -7.189021211466465999 ) ) ;
#127751 = CARTESIAN_POINT ( 'NONE',  ( 5.185773951807310489, 1.841398108398510480, -0.5159224025059682139 ) ) ;
#127753 = B_SPLINE_CURVE_WITH_KNOTS ( 'NONE', 3,
 ( #171545, #208303, #179038, #75126, #159572, #42648, #26357, #145508, #160640, #28507, #92473, #126088, #144438, #30657, #58870, #11170, #193134, #128238, #12240, #158512, #10111, #143363, #61005, #207244, #43712, #63143, #27432, #76184, #45847, #157457, #142292, #161724, #44782, #78314, #174782, #209360, #127162, #59933 ),
 .UNSPECIFIED., .F., .F.,
 ( 4, 2, 2, 2, 2, 2, 2, 2, 2, 2, 2, 2, 2, 2, 2, 2, 2, 2, 4 ),
 ( 1.734723475976806517E-18, 0.001334241201257017244, 0.002668482402514032754, 0.004002723603771048480, 0.005336964805028063773, 0.006004085405656572720, 0.006671206006285081667, 0.008005447207542100430, 0.009339688408799118324, 0.01067392961005613622, 0.01134105021068464170, 0.01200817081131315064, 0.01334241201257016854, 0.01467665321382718990, 0.01601089441508420780, 0.01734513561634122916, 0.01867937681759824706, 0.02001361801885526842, 0.02134785922011228632 ),
 .UNSPECIFIED. ) ;
#127752 = CARTESIAN_POINT ( 'NONE',  ( -6.645467848992654858, 10.90479625713344625, 0.7998128361456481317 ) ) ;
#127754 = CARTESIAN_POINT ( 'NONE',  ( -5.560252395380252288, 7.580323442733986283, 1.443375672974058777 ) ) ;
#127756 = CARTESIAN_POINT ( 'NONE',  ( 3.309304339999539657, -0.3661640501408692794, 1.834289908569000538 ) ) ;
#127755 = CARTESIAN_POINT ( 'NONE',  ( 4.933190498422773018, -1.479524406611672394, -1.477502780037798447 ) ) ;
#127757 = CARTESIAN_POINT ( 'NONE',  ( 7.131225611108096274, 8.382479970123348778, 1.082531754730558626 ) ) ;
#127758 = VERTEX_POINT ( 'NONE', #140821 ) ;
#127759 = AXIS2_PLACEMENT_3D ( 'NONE', #28438, #162721, #175770 ) ;
#127760 = DIRECTION ( 'NONE',  ( 0.000000000000000000, 1.000000000000000000, 0.000000000000000000 ) ) ;
#127761 = CARTESIAN_POINT ( 'NONE',  ( 0.2863826248021899001, -7.730039540835504930, -10.99644352130527025 ) ) ;
#127762 = CARTESIAN_POINT ( 'NONE',  ( 6.621745524129793559, -1.670984818007285266, 0.4274731708342211500 ) ) ;
#127763 = CARTESIAN_POINT ( 'NONE',  ( -7.237355071596549116, 7.338002426484427687, 1.040834085586084257E-14 ) ) ;
#127764 =( BOUNDED_SURFACE ( )  B_SPLINE_SURFACE ( 3, 2, ( 
 ( #104145, #188579, #70533 ),
 ( #122617, #153961, #156096 ),
 ( #54325, #200544, #35927 ),
 ( #7681, #106321, #56456 ) ),
 .UNSPECIFIED., .F., .F., .T. ) 
 B_SPLINE_SURFACE_WITH_KNOTS ( ( 4, 4 ),
 ( 3, 3 ),
 ( 8.673617379884035472E-19, 0.002003486994853858651 ),
 ( 0.000000000000000000, 1.000000000000000000 ),
 .UNSPECIFIED. ) 
 GEOMETRIC_REPRESENTATION_ITEM ( )  RATIONAL_B_SPLINE_SURFACE ( (
 ( 1.000000000000000000, 0.7779734834199515392, 1.000000000000000000),
 ( 1.000000000000000000, 0.7856061901475751563, 1.000000000000000000),
 ( 1.000000000000000000, 0.7951961705782221168, 1.000000000000000000),
 ( 1.000000000000000000, 0.8104931255419017821, 1.000000000000000000) ) ) 
 REPRESENTATION_ITEM ( '' )  SURFACE ( )  );
#127765 = CARTESIAN_POINT ( 'NONE',  ( 1.951430075251599838, -1.585913025431864742, -0.7019457847057923860 ) ) ;
#127766 = DIRECTION ( 'NONE',  ( -0.000000000000000000, -0.000000000000000000, -1.000000000000000000 ) ) ;
#127767 = CYLINDRICAL_SURFACE ( 'NONE', #62039, 1.000000000000000222 ) ;
#127768 = CARTESIAN_POINT ( 'NONE',  ( 5.858309005574939832, -2.171239809575730817, -0.007779773244297875576 ) ) ;
#127769 = CARTESIAN_POINT ( 'NONE',  ( 4.881388680972560401, 1.702354803207173584, -0.6601141376258444771 ) ) ;
#127770 = CARTESIAN_POINT ( 'NONE',  ( 2.606241817087478374, 1.961221450604538008, 0.05310280016677935283 ) ) ;
#127771 = CARTESIAN_POINT ( 'NONE',  ( 0.2634788376212302552, 1.973769265480609381, -0.7665230665306818070 ) ) ;
#127772 = CARTESIAN_POINT ( 'NONE',  ( 9.348761378620915607, 13.52553930298125096, -7.449808453853658641 ) ) ;
#127773 = CARTESIAN_POINT ( 'NONE',  ( 7.960204194457795477E-17, 14.00000000000000533, 0.6500000000000000222 ) ) ;
#127774 = CARTESIAN_POINT ( 'NONE',  ( 7.065770611016287006, 11.39514947949436774, 1.040834085586084257E-14 ) ) ;
#127775 = CARTESIAN_POINT ( 'NONE',  ( 2.824977599723184074, 1.534285384246200090, -1.463936014953904463 ) ) ;
#127776 = CARTESIAN_POINT ( 'NONE',  ( -5.273758566035884776, 5.255065869904374409, 0.000000000000000000 ) ) ;
#127777 = TOROIDAL_SURFACE ( 'NONE', #27334, 2.080000000000000071, 0.08000000000000000167 ) ;
#127778 =( NAMED_UNIT ( * ) PLANE_ANGLE_UNIT ( ) SI_UNIT ( $, .RADIAN. ) );
#127779 = CARTESIAN_POINT ( 'NONE',  ( -5.204229338117261072, 6.461601495962581154, -1.180324454998063377 ) ) ;
#127780 = CARTESIAN_POINT ( 'NONE',  ( 0.7431355771655088205, -0.2497938498803170537, -2.055034051290441255 ) ) ;
#127782 = CARTESIAN_POINT ( 'NONE',  ( -1.500000000000015099, 14.26041666734946212, -0.8660254037844309360 ) ) ;
#127781 = CARTESIAN_POINT ( 'NONE',  ( -10.79203373075640116, 4.452925688118183345, 5.250250085790691301 ) ) ;
#127784 = VERTEX_POINT ( 'NONE', #173300 ) ;
#127783 = CARTESIAN_POINT ( 'NONE',  ( 4.002737143027909283, -2.197200394838841664, -0.3254818186308478523 ) ) ;
#127785 = CARTESIAN_POINT ( 'NONE',  ( 0.9151166212276349299, -1.463470719828030120, -1.772635753884302057 ) ) ;
#127787 = CARTESIAN_POINT ( 'NONE',  ( 5.998899845030374323, 0.3968100507469035643, 2.023884403326465797 ) ) ;
#127786 = CARTESIAN_POINT ( 'NONE',  ( 4.532503425670185493, 4.182342172903648070, 1.214306433183764966E-14 ) ) ;
#127789 = CARTESIAN_POINT ( 'NONE',  ( 1.737500000000001155, -1.633333333333333748, 3.009438278150922130 ) ) ;
#127788 = CARTESIAN_POINT ( 'NONE',  ( 4.746236293235721604, 7.694970221153795364, 1.199719254218451159 ) ) ;
#127790 = CARTESIAN_POINT ( 'NONE',  ( 0.2331563151865486683, 0.005903526429595904942, -1.945944850731482934 ) ) ;
#127791 = CARTESIAN_POINT ( 'NONE',  ( 5.126429434416579056, 0.1410513515392505246, 1.835921608166577013 ) ) ;
#127792 = CARTESIAN_POINT ( 'NONE',  ( 4.867540842506059562, 5.637551390133895168, -1.199719254218452047 ) ) ;
#127793 = CARTESIAN_POINT ( 'NONE',  ( 2.819059531128511598, -0.1711090930666993304, 1.716262065957876004 ) ) ;
#127794 = CARTESIAN_POINT ( 'NONE',  ( 1.675017921984035096, 1.752138005693338441, -0.9981273289914743829 ) ) ;
#127795 = CARTESIAN_POINT ( 'NONE',  ( 2.637635294750583004, 0.7773225462509441019, 2.163377341885423188 ) ) ;
#127796 = CARTESIAN_POINT ( 'NONE',  ( -1.201851678989727383E-14, 3.509375000341421469, -1.575800808251660134 ) ) ;
#127797 = CARTESIAN_POINT ( 'NONE',  ( 2.917521460708580872, -0.2248114924257374192, 2.251233801775154308 ) ) ;
#127798 = CARTESIAN_POINT ( 'NONE',  ( 5.004563900840214963, -0.7087877200973876635, -1.983347251131000855 ) ) ;
#127799 = CARTESIAN_POINT ( 'NONE',  ( -4.990809943606269172, 8.836712344267034780, -0.7216878364870338292 ) ) ;
#127800 = CARTESIAN_POINT ( 'NONE',  ( 3.163107763524728444, 0.2631224511941733790, -1.749944513356870734 ) ) ;
#127801 = ADVANCED_BREP_SHAPE_REPRESENTATION ( '', ( #93359, #200407 ), #124605 ) ;
#127802 = CARTESIAN_POINT ( 'NONE',  ( 4.801558957534076022, 8.753569217098425170, 0.7998128361456462443 ) ) ;
#127804 = CARTESIAN_POINT ( 'NONE',  ( 6.585440809757122871, -0.9837151097084917417, 2.068200907652519405 ) ) ;
#127803 = CARTESIAN_POINT ( 'NONE',  ( 4.299344108864946890, 6.109263775132799168, -1.443375672974068769 ) ) ;
#127805 = CARTESIAN_POINT ( 'NONE',  ( 4.329911453333429527, 1.806054511993939515, 0.3568155486674411958 ) ) ;
#127807 = EDGE_CURVE ( 'NONE', #57442, #201902, #144242, .T. ) ;
#127806 = CARTESIAN_POINT ( 'NONE',  ( -4.303823697334223652, 7.108545849276850959, -1.199719254218452047 ) ) ;
#127808 = CARTESIAN_POINT ( 'NONE',  ( 4.975479186090852046, 6.827811688571220117, 1.443375672974062551 ) ) ;
#127809 = CARTESIAN_POINT ( 'NONE',  ( -1.201851678989727383E-14, 3.837500000000021227, -1.732050807568863648 ) ) ;
#127810 = CARTESIAN_POINT ( 'NONE',  ( 4.470767510317084970, 0.001397387737574890204, -2.191629466793604486 ) ) ;
#127811 = CARTESIAN_POINT ( 'NONE',  ( -5.434120640978981065, 5.234228924097238611, -0.7998128361456221525 ) ) ;
#127812 = CARTESIAN_POINT ( 'NONE',  ( 0.1447443628656777947, 7.100480071729100118, -2.114679381859644547 ) ) ;
#127813 = DIRECTION ( 'NONE',  ( -5.578564026256490882E-16, -1.000000000000000000, -9.066213480720158442E-32 ) ) ;
#127814 = CARTESIAN_POINT ( 'NONE',  ( -1.201851678989727383E-14, 5.196875000341422357, -1.575800808251660134 ) ) ;
#127815 = CARTESIAN_POINT ( 'NONE',  ( 3.422408909100621344, 1.221451249705886477, -1.489789856891531761 ) ) ;
#127816 = CARTESIAN_POINT ( 'NONE',  ( 0.6823417656249969321, 8.776041667008065872, -1.181850606188757036 ) ) ;
#127817 = CARTESIAN_POINT ( 'NONE',  ( -4.500943810056945438, 5.313817868896925312, 1.082531754730560403 ) ) ;
#127818 = CARTESIAN_POINT ( 'NONE',  ( 0.5104038411899833871, -0.7921320118633947693, 2.075572886547627505 ) ) ;
#127819 = ORIENTED_EDGE ( 'NONE', *, *, #63516, .T. ) ;
#127821 = CARTESIAN_POINT ( 'NONE',  ( 4.028709946750490545, 3.988235255965033588, -0.8025987720412866011 ) ) ;
#127820 = CARTESIAN_POINT ( 'NONE',  ( -3.011319516011047082, 6.527306845405913549, 0.7216878364870328300 ) ) ;
#127822 = CARTESIAN_POINT ( 'NONE',  ( 3.842846474469570062, 6.570739089268092137, -1.199719254218452047 ) ) ;
#127823 =( NAMED_UNIT ( * ) PLANE_ANGLE_UNIT ( ) SI_UNIT ( $, .RADIAN. ) );
#127824 = DIRECTION ( 'NONE',  ( 0.000000000000000000, -1.000000000000000000, 0.000000000000000000 ) ) ;
#127825 = VECTOR ( 'NONE', #159110, 1000.000000000000000 ) ;
#127826 = CARTESIAN_POINT ( 'NONE',  ( 0.1021010164683408133, 6.360493866598983637, -3.113991822131907838 ) ) ;
#127827 = CARTESIAN_POINT ( 'NONE',  ( 2.102700294964424454, -0.3804589880251930123, 1.698169956227519872 ) ) ;
#127828 = CARTESIAN_POINT ( 'NONE',  ( 0.000000000000000000, 0.000000000000000000, 0.000000000000000000 ) ) ;
#127829 = CARTESIAN_POINT ( 'NONE',  ( 0.6077679335219284829, 0.6189715888181289705, -1.861716921216026055 ) ) ;
#127830 = CARTESIAN_POINT ( 'NONE',  ( 1.364683531249986537, 0.7177083336747527298, -0.7879004041258239610 ) ) ;
#127831 = CIRCLE ( 'NONE', #20558, 9.523431457505068920 ) ;
#127832 = CARTESIAN_POINT ( 'NONE',  ( 6.121977807712331909, -1.196819783530624015, -1.799967629666970881 ) ) ;
#127833 = CARTESIAN_POINT ( 'NONE',  ( -9.755255220232635693, 11.33988483081495957, -1.199719254218441611 ) ) ;
#127834 = CARTESIAN_POINT ( 'NONE',  ( -5.883875478206491927, 5.966868934103426447, 0.000000000000000000 ) ) ;
#127835 = CARTESIAN_POINT ( 'NONE',  ( 5.260679775997886054, -1.568431141927080219, 1.487858469166832176 ) ) ;
#127837 = EDGE_LOOP ( 'NONE', ( #85470, #102570, #763, #175419, #110081 ) ) ;
#127836 = CARTESIAN_POINT ( 'NONE',  ( -0.2106725631050020975, 5.721452923065615259, -2.597767226077936087 ) ) ;
#127838 = CARTESIAN_POINT ( 'NONE',  ( -1.364683531250010295, 4.030208333674751842, 0.7879004041258379498 ) ) ;
#127839 = CARTESIAN_POINT ( 'NONE',  ( 6.919227946136824237, -0.1375138451006757134, 1.940497564164916922 ) ) ;
#127840 = CARTESIAN_POINT ( 'NONE',  ( 5.835191860132536767, -1.097891704307648597, 1.341895879554096727 ) ) ;
#127842 = CARTESIAN_POINT ( 'NONE',  ( 3.544632465004614374, -1.790652189326558563, 1.263247045326252094 ) ) ;
#127841 = CARTESIAN_POINT ( 'NONE',  ( 1.360316468749980023, 0.01562500034139879812, -2.255140518769849223E-14 ) ) ;
#127843 = CARTESIAN_POINT ( 'NONE',  ( 3.100898361104642120, -0.6683016296473989204, -2.208703637169514788 ) ) ;
#127844 = CARTESIAN_POINT ( 'NONE',  ( 5.571578285044489043, 1.987195396197571462, -0.5455906853745869922 ) ) ;
#127845 = CARTESIAN_POINT ( 'NONE',  ( 1.288897009404812666, 1.470358960358808309, 1.268651691623223110 ) ) ;
#127846 = CARTESIAN_POINT ( 'NONE',  ( -6.575341312503472757, 7.733948288417905381, 1.082531754730549967 ) ) ;
#127848 = EDGE_CURVE ( 'NONE', #151743, #85578, #161522, .T. ) ;
#127847 = CARTESIAN_POINT ( 'NONE',  ( -0.1489494290324539782, -7.995840219786860992, -9.536979704252555479 ) ) ;
#127849 = CARTESIAN_POINT ( 'NONE',  ( -9.386220699155614966, 14.48154074412966175, 7.476614104249496684 ) ) ;
#127850 = CARTESIAN_POINT ( 'NONE',  ( 4.570628194609677841, 0.8141925398062774821, 1.958264201954627026 ) ) ;
#127851 = CARTESIAN_POINT ( 'NONE',  ( 1.668847547943344454E-13, 1.972237431424435750, 11.78526707783969663 ) ) ;
#127852 = CARTESIAN_POINT ( 'NONE',  ( 1.863907939170056149, -0.1017519224979606118, -2.013985838549677609 ) ) ;
#127853 = CARTESIAN_POINT ( 'NONE',  ( -5.327991180046197428, 8.199444895820425572, 1.082531754730548412 ) ) ;
#127854 = CARTESIAN_POINT ( 'NONE',  ( 5.895608061265788180, 1.667329832391790667, 1.445732890734657161 ) ) ;
#127855 = CARTESIAN_POINT ( 'NONE',  ( 1.642778471875000035, -0.3135416661887088785, -2.845375778867859751 ) ) ;
#127856 = CARTESIAN_POINT ( 'NONE',  ( 0.3769810270647707684, 3.049942316455285685, -0.4288785890453113980 ) ) ;
#127857 = CARTESIAN_POINT ( 'NONE',  ( 0.004084906056917469129, 14.55754942065380320, 11.94689476429229202 ) ) ;
#127858 = CARTESIAN_POINT ( 'NONE',  ( -7.099629715411508890, 8.311931418515415615, 1.199719254218452047 ) ) ;
#127860 = CARTESIAN_POINT ( 'NONE',  ( -5.606333003394546211, 5.691104718644762528, 0.3812976639747498453 ) ) ;
#127859 = CARTESIAN_POINT ( 'NONE',  ( -5.337921042252067316, 7.714266718146587820, 1.325459453385816833 ) ) ;
#127861 = CARTESIAN_POINT ( 'NONE',  ( -4.694467135394339685, 8.285658806408200405, 0.6022741701859417596 ) ) ;
#127862 = EDGE_LOOP ( 'NONE', ( #179979, #158784, #97647, #131558 ) ) ;
#127863 = CARTESIAN_POINT ( 'NONE',  ( 4.715729953790866347, -2.021515393979388175, 0.4000037541747498704 ) ) ;
#127864 = DIRECTION ( 'NONE',  ( -0.6507913734559650498, 0.7592566023652995710, 0.000000000000000000 ) ) ;
#127865 = CARTESIAN_POINT ( 'NONE',  ( 7.777967379493318845, -5.907420853759296264, 7.744830294503448620 ) ) ;
#127866 = CARTESIAN_POINT ( 'NONE',  ( -3.958090780185743451, 6.705190779270287393, -1.199719254218452047 ) ) ;
#127867 = CARTESIAN_POINT ( 'NONE',  ( -4.248501033035892327, 6.049946853332221153, -1.599625672291271394 ) ) ;
#127868 = CARTESIAN_POINT ( 'NONE',  ( 4.881513094923572105, 0.1956549798781386795, -2.010156034525738988 ) ) ;
#127869 = CARTESIAN_POINT ( 'NONE',  ( 1.499999999999985123, 0.5458333333333577064, -0.8660254037844253849 ) ) ;
#127871 = CARTESIAN_POINT ( 'NONE',  ( 9.436111725431318931, 10.11114455586577776, -0.7216878364870257245 ) ) ;
#127870 = CARTESIAN_POINT ( 'NONE',  ( -3.305155586681401303, 7.078041627762083898, 0.7998128361456352531 ) ) ;
#127872 = CARTESIAN_POINT ( 'NONE',  ( 5.770966940911189447, 9.884545197705074671, -0.7998128361456291469 ) ) ;
#127873 = CARTESIAN_POINT ( 'NONE',  ( 2.747006664573675039, -1.714185755289293622, 1.143718651939158670 ) ) ;
#127874 = CARTESIAN_POINT ( 'NONE',  ( 2.742814741689561853, 2.006446121045248887, -0.2004354718553730264 ) ) ;
#127875 = VERTEX_POINT ( 'NONE', #125680 ) ;
#127876 = CARTESIAN_POINT ( 'NONE',  ( 6.727182134110222478, 4.688348259194305534, 2.751590707055273199 ) ) ;
#127877 = CARTESIAN_POINT ( 'NONE',  ( 5.379888026524302980, 5.170957540566797128, -0.7998128361456211532 ) ) ;
#127879 = VERTEX_POINT ( 'NONE', #124621 ) ;
#127878 = CARTESIAN_POINT ( 'NONE',  ( -0.5059764118015118717, 7.965522150964809533, -1.935091031283027174 ) ) ;
#127880 = CARTESIAN_POINT ( 'NONE',  ( 2.636092105226188309, 0.1017362925337349233, -2.013677536115268563 ) ) ;
#127881 = CARTESIAN_POINT ( 'NONE',  ( 1.956743257466783570, 0.3155556147324266036, -1.813728304320901596 ) ) ;
#127882 = CARTESIAN_POINT ( 'NONE',  ( 1.313548042387347348, 2.037171730821058624, 1.084164666379479502 ) ) ;
#127883 = CARTESIAN_POINT ( 'NONE',  ( 5.574337433874081427, 6.532423756721743580, -1.199719254218452047 ) ) ;
#127884 = CARTESIAN_POINT ( 'NONE',  ( 2.741676502816026595, -1.599691942034554337, -1.453933697666408120 ) ) ;
#127885 = CARTESIAN_POINT ( 'NONE',  ( 9.043452155515161905, 10.50944792197790889, 1.199719254218453823 ) ) ;
#127886 = CARTESIAN_POINT ( 'NONE',  ( -5.819474248763749635, 7.812472595022922128, -1.599625672291256295 ) ) ;
#127887 = ADVANCED_FACE ( 'NONE', ( #56336 ), #23816, .F. ) ;
#127888 = ORIENTED_EDGE ( 'NONE', *, *, #201067, .T. ) ;
#127889 = CARTESIAN_POINT ( 'NONE',  ( 0.3999999999910882620, 3.122291170403207694, -2.023857702510297507 ) ) ;
#127890 = CARTESIAN_POINT ( 'NONE',  ( 0.7252172114964609007, -1.777616610744123804, 0.5828384007960025759 ) ) ;
#127891 = CARTESIAN_POINT ( 'NONE',  ( 5.225445458360559847, -1.872321802520343414, 0.6175577138636638708 ) ) ;
#127893 = CARTESIAN_POINT ( 'NONE',  ( 9.558135107509954764, 10.25350516829085379, -0.7216878364870257245 ) ) ;
#127892 = CARTESIAN_POINT ( 'NONE',  ( -0.6823417656249969321, 3.217708333674754062, -1.181850606188749264 ) ) ;
#127895 = CARTESIAN_POINT ( 'NONE',  ( 0.5752038918783763943, -2.079344756725898691, -0.7397341299467049547 ) ) ;
#127894 = CARTESIAN_POINT ( 'NONE',  ( -5.364222332501225488, 9.410009821226765325, 0.7998128361456481317 ) ) ;
#127896 = CARTESIAN_POINT ( 'NONE',  ( 6.795378861676105053, -1.851214886592133846, 0.9271815693319698237 ) ) ;
#127897 = CARTESIAN_POINT ( 'NONE',  ( 5.361359679200154105, 8.342337828120466980, 1.199719254218462483 ) ) ;
#127898 = CARTESIAN_POINT ( 'NONE',  ( -6.358937740009323214, 7.377514437221045718, -1.199719254218446718 ) ) ;
#127899 = CARTESIAN_POINT ( 'NONE',  ( 6.539320575229251808, 7.629137130509035636, 2.803262396134009737 ) ) ;
#127900 = CARTESIAN_POINT ( 'NONE',  ( 4.452002833372045387, 1.971050344634683427, -0.04741254548742446229 ) ) ;
#127901 = CARTESIAN_POINT ( 'NONE',  ( 0.03560581989598374242, -0.09759080014098624190, 2.118463022953632091 ) ) ;
#127902 = CARTESIAN_POINT ( 'NONE',  ( -0.7500000000000249800, -0.02708333265051543481, 1.299038105676659116 ) ) ;
#127903 = CARTESIAN_POINT ( 'NONE',  ( 4.600386337014011673, -2.307077041318765342, -0.05981084109947519545 ) ) ;
#127904 = CARTESIAN_POINT ( 'NONE',  ( 2.483324480268500611, -0.004404232681418790429, 2.062741127353195925 ) ) ;
#127905 = CARTESIAN_POINT ( 'NONE',  ( 8.446366511633696561, 8.956441806435218922, 1.040834085586084257E-14 ) ) ;
#127906 = CARTESIAN_POINT ( 'NONE',  ( 3.881377115262159894, 7.750300077773022878, 0.7998128361456271485 ) ) ;
#127907 = CARTESIAN_POINT ( 'NONE',  ( 4.869313445963426190, 5.709895770826003414, 1.199719254218452935 ) ) ;
#127908 = CARTESIAN_POINT ( 'NONE',  ( 1.364683531249988535, 2.176041667008087543, 0.7879004041258500513 ) ) ;
#127909 = CARTESIAN_POINT ( 'NONE',  ( 5.090160327287878594, 4.903218234782778850, -0.7998128361456481317 ) ) ;
#127910 = CARTESIAN_POINT ( 'NONE',  ( 4.799223189113185128, 8.542918120699967588, 1.040834085586084257E-14 ) ) ;
#127911 = CARTESIAN_POINT ( 'NONE',  ( 4.281792510435393773, -2.078899500905183828, 0.6263114880437108400 ) ) ;
#127913 = CARTESIAN_POINT ( 'NONE',  ( 3.843160323004328305, 0.6166970922517557296, -1.735048075492843456 ) ) ;
#127912 = CARTESIAN_POINT ( 'NONE',  ( -3.307826292054310890, 5.842585859829892314, -1.082531754730549967 ) ) ;
#127915 = CARTESIAN_POINT ( 'NONE',  ( -4.792515913634093623E-13, -7.868798029037626485, 9.500000000000001776 ) ) ;
#127914 = CARTESIAN_POINT ( 'NONE',  ( 0.000000000000000000, 12.30000000000000071, 0.000000000000000000 ) ) ;
#127916 = CARTESIAN_POINT ( 'NONE',  ( 5.003566749295822014, -2.181051155298455058, 0.2145382695054529609 ) ) ;
#127917 = FACE_OUTER_BOUND ( 'NONE', #140775, .T. ) ;
#127918 = CARTESIAN_POINT ( 'NONE',  ( 6.385631343721732911, 1.554564302923328700, 1.644106664497286596 ) ) ;
#127919 = ORIENTED_EDGE ( 'NONE', *, *, #171659, .F. ) ;
#127920 = EDGE_CURVE ( 'NONE', #18446, #158767, #123562, .T. ) ;
#127921 = CARTESIAN_POINT ( 'NONE',  ( -4.475961918153980257, 7.265020140467052023, -1.287590260893024086 ) ) ;
#127922 = FACE_OUTER_BOUND ( 'NONE', #166133, .T. ) ;
#127923 = CARTESIAN_POINT ( 'NONE',  ( 4.842126824027952026, 8.201492973507317430, 0.9351865777775794086 ) ) ;
#127924 = AXIS2_PLACEMENT_3D ( 'NONE', #75062, #7906, #88113 ) ;
#127925 = CARTESIAN_POINT ( 'NONE',  ( -5.451787166026575981, 5.533042246551999277, 0.000000000000000000 ) ) ;
#127926 = CARTESIAN_POINT ( 'NONE',  ( 3.607878275012313285, 6.262922849939428716, 1.082531754730549078 ) ) ;
#127927 = CARTESIAN_POINT ( 'NONE',  ( 1.252431388357349684, -1.398210551426328330, 1.084949785890441110 ) ) ;
#127928 = CARTESIAN_POINT ( 'NONE',  ( 4.846344381697188730, 1.033023791896072519, -1.727689222339493069 ) ) ;
#127929 = CARTESIAN_POINT ( 'NONE',  ( 7.481401836642521452, 7.622723652371411696, 1.040834085586084257E-14 ) ) ;
#127930 = CARTESIAN_POINT ( 'NONE',  ( 4.612399560509667928, -0.8980232107528103302, -1.905027153144087437 ) ) ;
#127931 = CARTESIAN_POINT ( 'NONE',  ( 2.020959903547480341, -1.710230010390185296, 0.8631189023672394267 ) ) ;
#127932 = CARTESIAN_POINT ( 'NONE',  ( 2.984766373302843778, 6.633977868828633717, -0.7998128361456291469 ) ) ;
#127934 = EDGE_CURVE ( 'NONE', #212596, #102537, #185428, .T. ) ;
#127933 = CARTESIAN_POINT ( 'NONE',  ( 2.892966452247947906, 0.2382023302623069438, 1.955005545544076240 ) ) ;
#127935 = CARTESIAN_POINT ( 'NONE',  ( 5.853772736177474734, -1.465772220379698343, -1.389892856972896329 ) ) ;
#127936 = CARTESIAN_POINT ( 'NONE',  ( 1.621729638615863944, -1.036547396872866678, -1.557007864774778705 ) ) ;
#127939 = ORIENTED_EDGE ( 'NONE', *, *, #26150, .T. ) ;
#127938 = CARTESIAN_POINT ( 'NONE',  ( 1.423922367354793606, -1.897583212610975734, 0.2371896777705190806 ) ) ;
#127937 = CARTESIAN_POINT ( 'NONE',  ( 5.408750372623219782, 1.302234988713904640, -1.131221429639968745 ) ) ;
#127941 = CARTESIAN_POINT ( 'NONE',  ( 5.205967797967541166, 5.175976640491323444, -0.7216878364870197293 ) ) ;
#127940 = CARTESIAN_POINT ( 'NONE',  ( 0.9618826090718561872, 0.4271145061440981272, -2.164990749644220447 ) ) ;
#127942 = CARTESIAN_POINT ( 'NONE',  ( -1.364683531250014514, 1.801041667008085767, -0.7879004041258289570 ) ) ;
#127944 = AXIS2_PLACEMENT_3D ( 'NONE', #85264, #2920, #135111 ) ;
#127943 = CARTESIAN_POINT ( 'NONE',  ( 9.399880572976245574, 9.860948844760784482, 0.7998128361456462443 ) ) ;
#127945 = CARTESIAN_POINT ( 'NONE',  ( 11.91292854676714974, 11.11481529673021207, 1.446370920797324100 ) ) ;
#127946 = CARTESIAN_POINT ( 'NONE',  ( -4.391951695823077984, 7.211361847513815704, 1.199719254218464037 ) ) ;
#127947 = DIRECTION ( 'NONE',  ( 0.000000000000000000, 0.000000000000000000, -1.000000000000000000 ) ) ;
#127948 = CARTESIAN_POINT ( 'NONE',  ( 1.873570696236816158, -0.2555354716398828274, 2.054483085851127377 ) ) ;
#127949 = CARTESIAN_POINT ( 'NONE',  ( 0.7499999999999885647, 2.066666666666688634, -1.299038105676652899 ) ) ;
#127950 = CARTESIAN_POINT ( 'NONE',  ( 4.964256800898067645, 8.943383367689749619, 0.7998128361456462443 ) ) ;
#127951 = CARTESIAN_POINT ( 'NONE',  ( -6.204827856548512877, 10.39071626594860476, -0.7998128361456291469 ) ) ;
#127952 = CARTESIAN_POINT ( 'NONE',  ( 5.252858170651868441, 5.093032385374103299, -0.7998128361456481317 ) ) ;
#127953 = CARTESIAN_POINT ( 'NONE',  ( 6.059260758684835046, -1.791542317298041365, 1.134111293253435182 ) ) ;
#127954 = CARTESIAN_POINT ( 'NONE',  ( -0.6823417656250212460, 2.301041667008084435, 1.181850606188767472 ) ) ;
#127955 = VERTEX_POINT ( 'NONE', #108350 ) ;
#127956 = EDGE_CURVE ( 'NONE', #108115, #184329, #110866, .T. ) ;
#127958 = CARTESIAN_POINT ( 'NONE',  ( 4.220665892555866883, 3.818531717603609987, -0.7998128361456211532 ) ) ;
#127957 = CARTESIAN_POINT ( 'NONE',  ( 6.848121815800094936, -0.8396676627679277027, 1.771385694100804375 ) ) ;
#127959 = CARTESIAN_POINT ( 'NONE',  ( 4.833361152654930493, -1.319026006086077230, 1.524810761284051575 ) ) ;
#127960 = CARTESIAN_POINT ( 'NONE',  ( 4.557778266838360182, 1.108094384514320963, 1.562507240529472874 ) ) ;
#127961 =( NAMED_UNIT ( * ) PLANE_ANGLE_UNIT ( ) SI_UNIT ( $, .RADIAN. ) );
#127962 = CARTESIAN_POINT ( 'NONE',  ( 2.454835928891830221, -1.908367152989149718, -1.077367144120815023 ) ) ;
#127963 =( BOUNDED_CURVE ( )  B_SPLINE_CURVE ( 2, ( #24475, #140423, #6085, #76446, #105792, #175040, #72156, #189132, #126354 ),
 .UNSPECIFIED., .F., .T. ) 
 B_SPLINE_CURVE_WITH_KNOTS ( ( 3, 2, 2, 2, 3 ),
 ( 0.9196428571428570953, 0.9226190476190476719, 0.9285714285714286031, 0.9345238095238095344, 0.9375000000000000000 ),
 .UNSPECIFIED. ) 
 CURVE ( )  GEOMETRIC_REPRESENTATION_ITEM ( )  RATIONAL_B_SPLINE_CURVE ( ( 0.9330127018922194093, 0.9330127018922180770, 1.000000000000000000, 0.8660254037844387076, 1.000000000000000000, 0.8660254037844387076, 1.000000000000000000, 0.9330127018922194093, 0.9330127018922194093 ) ) 
 REPRESENTATION_ITEM ( '' )  );
#127964 = CARTESIAN_POINT ( 'NONE',  ( -1.814759087650030356, 3.975067388631713161, 0.4606438099578192280 ) ) ;
#127965 = CARTESIAN_POINT ( 'NONE',  ( -1.500000000000001332, 1.181250000682816603, 0.000000000000000000 ) ) ;
#127966 = CARTESIAN_POINT ( 'NONE',  ( 4.939702229944241907, -1.910329301133410151, 0.6354416197995541582 ) ) ;
#127967 = CARTESIAN_POINT ( 'NONE',  ( -7.691553217654356622, 7.867900263551875994, -0.7998128361456291469 ) ) ;
#127969 = CARTESIAN_POINT ( 'NONE',  ( 6.011343318556897408, -1.993460012771612222, 0.7135861072808927785 ) ) ;
#127968 = CARTESIAN_POINT ( 'NONE',  ( -3.633221978782299910, 5.261844946711204507, -1.443375672974053447 ) ) ;
#127970 = CARTESIAN_POINT ( 'NONE',  ( -8.012344526598182026E-15, 9.859375000341399797, -1.575800808251669460 ) ) ;
#127972 = CARTESIAN_POINT ( 'NONE',  ( -6.149505192250180663, 9.332117270003974951, -1.199719254218452047 ) ) ;
#127971 = CARTESIAN_POINT ( 'NONE',  ( 3.245728744149275702, 2.090933975402937683, -0.002398190518447183318 ) ) ;
#127974 = ORIENTED_EDGE ( 'NONE', *, *, #198453, .T. ) ;
#127973 = CARTESIAN_POINT ( 'NONE',  ( 1.465380626080296400, 1.700101026837578466, -0.2896415544312477830 ) ) ;
#127975 = CARTESIAN_POINT ( 'NONE',  ( 4.834296457332984076, -1.136628438424293508, -1.790084250976264002 ) ) ;
#127976 = CARTESIAN_POINT ( 'NONE',  ( 4.950698647284403009, 8.927565521807144577, 1.040834085586084257E-14 ) ) ;
#127977 = CARTESIAN_POINT ( 'NONE',  ( 10.97030574691034843, 12.29999999999998472, 1.695191245859930307 ) ) ;
#127978 = CARTESIAN_POINT ( 'NONE',  ( 7.722692672890256738, -6.459788825448992355, 7.834474503270634216 ) ) ;
#127979 = CARTESIAN_POINT ( 'NONE',  ( 7.318703993278529829, 7.432909501780090800, 1.040834085586084257E-14 ) ) ;
#127980 = ORIENTED_EDGE ( 'NONE', *, *, #24826, .T. ) ;
#127981 = DIRECTION ( 'NONE',  ( 0.000000000000000000, 1.000000000000000000, 0.000000000000000000 ) ) ;
#127983 = CARTESIAN_POINT ( 'NONE',  ( 1.348006360704995910, 0.8929448326314154416, -1.575985355173844527 ) ) ;
#127982 = CARTESIAN_POINT ( 'NONE',  ( 5.936491157937257235, 8.019268665717216749, 1.599625672291268286 ) ) ;
#127984 = CARTESIAN_POINT ( 'NONE',  ( -7.379715684540041565, 7.504089808251839244, 1.040834085586084257E-14 ) ) ;
#127985 = ORIENTED_EDGE ( 'NONE', *, *, #84476, .T. ) ;
#127986 = CARTESIAN_POINT ( 'NONE',  ( 4.539282502477016479, 4.190251095844947926, 0.7998128361456341429 ) ) ;
#127987 = CARTESIAN_POINT ( 'NONE',  ( 5.037736595929563244, 8.035053907629919223, -1.199719254218452047 ) ) ;
#127988 = CARTESIAN_POINT ( 'NONE',  ( 3.158660791640830467, 0.4427227019567353539, 1.756387338163778233 ) ) ;
#127989 = CARTESIAN_POINT ( 'NONE',  ( 0.4153311931458965045, 3.850000000000006306, -0.4999999999999987232 ) ) ;
#127990 = CARTESIAN_POINT ( 'NONE',  ( 4.413087178904756769, 7.101426714207548230, 1.094556639780567053 ) ) ;
#127991 = VECTOR ( 'NONE', #182433, 1000.000000000000114 ) ;
#127992 = CARTESIAN_POINT ( 'NONE',  ( 4.246440214068532448, -1.840602306905499086, -0.2743259802632999622 ) ) ;
#127993 = CARTESIAN_POINT ( 'NONE',  ( 1.423292265346193464, -1.388624197914482883, -1.319832876491247697 ) ) ;
#127994 = CARTESIAN_POINT ( 'NONE',  ( 6.422877973628248860, 1.797746274024723201, 0.6925914001822802701 ) ) ;
#127995 = CARTESIAN_POINT ( 'NONE',  ( 0.7500000000000006661, 11.66666666666666607, -1.299038105676657340 ) ) ;
#127996 = CARTESIAN_POINT ( 'NONE',  ( 1.249999999999964695, 8.500000000000000000, -9.921567416492218072 ) ) ;
#127997 = CARTESIAN_POINT ( 'NONE',  ( 0.3282377607281167786, 1.488835450998188259, -1.225000000000016298 ) ) ;
#127998 = CARTESIAN_POINT ( 'NONE',  ( -3.958617665510283601, 4.681104033592509595, -1.082531754730549967 ) ) ;
#127999 = CARTESIAN_POINT ( 'NONE',  ( 6.643132081016105417, 10.69414516125339887, 0.7216878364870438212 ) ) ;
#128000 = CARTESIAN_POINT ( 'NONE',  ( 6.121921657745279077, 1.940899573806122325, -0.3330216297181831653 ) ) ;
#128001 = EDGE_CURVE ( 'NONE', #29585, #65129, #26520, .T. ) ;
#128002 = CARTESIAN_POINT ( 'NONE',  ( -4.578903193113314174, 6.365139696764064325, 1.599625672291267398 ) ) ;
#128003 = CARTESIAN_POINT ( 'NONE',  ( -11.86145016429273014, 12.69999999999999929, 1.179999999999997051 ) ) ;
#128004 = CARTESIAN_POINT ( 'NONE',  ( -0.02919842301645457147, -0.002306431287177941429, -2.073770398395402115 ) ) ;
#128005 = SURFACE_STYLE_USAGE ( .BOTH. , #80214 ) ;
#128006 = CARTESIAN_POINT ( 'NONE',  ( 5.016589502704805525, 1.328544886203905318, -1.395186341261208884 ) ) ;
#128007 = CARTESIAN_POINT ( 'NONE',  ( -6.368579470117215813, 8.453095353268645695, 1.599625672291283607 ) ) ;
#128008 = ADVANCED_FACE ( 'NONE', ( #171142 ), #24881, .F. ) ;
#128009 = CARTESIAN_POINT ( 'NONE',  ( 1.588595499965880453, -0.2641367610144580991, -1.806243275932853276 ) ) ;
#128010 = CARTESIAN_POINT ( 'NONE',  ( 2.121956728516772639, -2.140194184088719531, 0.5379336890513550795 ) ) ;
#128011 = CARTESIAN_POINT ( 'NONE',  ( 0.1582721923853447621, 1.907395734848855051, 0.1385995803297388196 ) ) ;
#128012 = ORIENTED_EDGE ( 'NONE', *, *, #96950, .F. ) ;
#128013 = CARTESIAN_POINT ( 'NONE',  ( 0.3792734414799744380, -0.1002090192285705339, 1.967142940827655284 ) ) ;
#128014 = CARTESIAN_POINT ( 'NONE',  ( 3.052217916795424202, -1.468930141372110088, 1.270444820450331358 ) ) ;
#128015 = CARTESIAN_POINT ( 'NONE',  ( 0.7552322466577044979, -2.000550463317086525, -0.2495714061315074117 ) ) ;
#128017 = CARTESIAN_POINT ( 'NONE',  ( 5.383604208181901107, -1.767738693978682996, 0.5818682867176503404 ) ) ;
#128016 = CARTESIAN_POINT ( 'NONE',  ( -4.956387674247580755, 7.940146832334256111, 1.199719254218452935 ) ) ;
#128018 = CARTESIAN_POINT ( 'NONE',  ( 4.213551878797002992, 8.137837301896977849, 0.000000000000000000 ) ) ;
#128019 = CARTESIAN_POINT ( 'NONE',  ( -1.225000000000005640, 2.812500000682796486, -1.734723475976807094E-15 ) ) ;
#128020 = CARTESIAN_POINT ( 'NONE',  ( 0.000000000000000000, 9.719999999999982876, 0.000000000000000000 ) ) ;
#128021 = CARTESIAN_POINT ( 'NONE',  ( -5.253948220495577637, 6.088359997788290734, 1.199719254218450271 ) ) ;
#128022 = CARTESIAN_POINT ( 'NONE',  ( -6.050681693448748177, 10.28115541899069463, 0.7998128361456291469 ) ) ;
#128023 = CARTESIAN_POINT ( 'NONE',  ( 1.083813775577105565, -0.9808430935620198188, 1.959877696171570927 ) ) ;
#128024 = CARTESIAN_POINT ( 'NONE',  ( 4.121315508874254796, 5.831287398485176077, -1.443375672974051449 ) ) ;
#128025 = CARTESIAN_POINT ( 'NONE',  ( 11.00029519899100805, -6.134628647623514119, 3.672734859294647059E-15 ) ) ;
#128026 = FACE_OUTER_BOUND ( 'NONE', #169966, .T. ) ;
#128027 = CARTESIAN_POINT ( 'NONE',  ( 2.525780997283606499, -1.050937884436175418, -1.492673824175783093 ) ) ;
#128028 = CARTESIAN_POINT ( 'NONE',  ( -4.308793891044708779, 3.921347715840572956, 1.214306433183764966E-14 ) ) ;
#128029 = CARTESIAN_POINT ( 'NONE',  ( -4.925689880466507908, 4.641059703499347044, -0.7998128361456221525 ) ) ;
#128030 = CARTESIAN_POINT ( 'NONE',  ( -4.620524454801235414, 8.454239455966142458, -0.3877863265914320845 ) ) ;
#128031 = CARTESIAN_POINT ( 'NONE',  ( 6.509000000000010111, 6.037005099786168394, 2.594901386363585694 ) ) ;
#128032 = CARTESIAN_POINT ( 'NONE',  ( 10.22692794340986921, 10.82583744360002243, 0.000000000000000000 ) ) ;
#128033 = CARTESIAN_POINT ( 'NONE',  ( 0.7153026426200872478, -0.2839029868492106701, 1.905349893463634814 ) ) ;
#128034 = CARTESIAN_POINT ( 'NONE',  ( 5.541838416980684023, 1.314774629379747539, 1.456173869884537675 ) ) ;
#128035 = CARTESIAN_POINT ( 'NONE',  ( -7.901704598666176693, 8.113076874732334076, 0.7998128361456602331 ) ) ;
#128036 = CARTESIAN_POINT ( 'NONE',  ( 4.313465427442102929, 8.184126765324453601, 0.7998128361456462443 ) ) ;
#128037 = CARTESIAN_POINT ( 'NONE',  ( 4.704715985517350596, 1.906866092115505840, 1.080010033982371498 ) ) ;
#128038 = CARTESIAN_POINT ( 'NONE',  ( 4.497554271431305040, 6.270232621468402989, -1.599625672291256517 ) ) ;
#128039 = CARTESIAN_POINT ( 'NONE',  ( 4.329010850845236291, -1.929826300244817272, -0.7499136367685385052 ) ) ;
#128041 = CARTESIAN_POINT ( 'NONE',  ( 1.364683531249988757, 1.946875000341415030, 0.000000000000000000 ) ) ;
#128040 = CARTESIAN_POINT ( 'NONE',  ( 8.445188405616965710, 14.00107259802710047, 8.462322735403144947 ) ) ;
#128042 = ORIENTED_EDGE ( 'NONE', *, *, #20908, .T. ) ;
#128043 = CARTESIAN_POINT ( 'NONE',  ( 4.360180292246352174, 0.0003893357360621601550, -2.298851035006874266 ) ) ;
#128045 = ORIENTED_EDGE ( 'NONE', *, *, #167509, .T. ) ;
#128044 = CARTESIAN_POINT ( 'NONE',  ( 6.317736394288122170, 10.31451686007074997, 0.7216878364870438212 ) ) ;
#128047 = DIRECTION ( 'NONE',  ( -5.551115123125766062E-17, 0.000000000000000000, 1.000000000000000000 ) ) ;
#128046 = CARTESIAN_POINT ( 'NONE',  ( 6.726253606155519371, 7.019919760035800316, -0.7216878364870458196 ) ) ;
#128048 = CARTESIAN_POINT ( 'NONE',  ( 6.620655732516647518, 0.007553340620044743381, 1.826407896915738238 ) ) ;
#128049 = FACE_OUTER_BOUND ( 'NONE', #164340, .T. ) ;
#128050 = CARTESIAN_POINT ( 'NONE',  ( 3.451055654028605701, 0.4708835965685866376, -1.883881102318455847 ) ) ;
#128051 = ORIENTED_EDGE ( 'NONE', *, *, #8784, .T. ) ;
#128052 = CARTESIAN_POINT ( 'NONE',  ( 10.53432216769390095, 11.39239007183880581, -0.7216878364870257245 ) ) ;
#128053 = ORIENTED_EDGE ( 'NONE', *, *, #152080, .T. ) ;
#128054 = CARTESIAN_POINT ( 'NONE',  ( 5.502191098127390489, -0.8541586074963626318, 1.711093258865265643 ) ) ;
#128055 = CARTESIAN_POINT ( 'NONE',  ( 6.299779570463345912, -0.5759050694413189175, 1.625906498142214884 ) ) ;
#128056 = CARTESIAN_POINT ( 'NONE',  ( 4.997279897388729353, -0.2910847460899004258, 1.995267753224789997 ) ) ;
#128057 = CARTESIAN_POINT ( 'NONE',  ( 5.355107487717867265, 5.349972945200037522, 1.040834085586084257E-14 ) ) ;
#128058 = CARTESIAN_POINT ( 'NONE',  ( 2.245003380770736801, 0.4850519687749441644, 2.152760086278446394 ) ) ;
#128060 = CARTESIAN_POINT ( 'NONE',  ( 4.000000000000012434, 5.499999999999998224, -1.214306433183764966E-14 ) ) ;
#128059 = CARTESIAN_POINT ( 'NONE',  ( -8.319899820280397762, 12.85830022363583147, -0.7998128361456281477 ) ) ;
#128062 = CARTESIAN_POINT ( 'NONE',  ( 0.2152203129428611750, -1.737008003653650157, 0.3383841826808623443 ) ) ;
#128061 = CARTESIAN_POINT ( 'NONE',  ( 1.746151220907150359, 0.6571888886500141247, 1.984721739902342019 ) ) ;
#128063 = CARTESIAN_POINT ( 'NONE',  ( 5.924453975591452703, -1.462443569488897754, -1.388487997949397368 ) ) ;
#128065 = CARTESIAN_POINT ( 'NONE',  ( 2.607731988003787915, -2.267127051869659571, 0.3377934734241551662 ) ) ;
#128064 = CARTESIAN_POINT ( 'NONE',  ( 6.222266154028957885, 6.224008365980749247, 0.7998128361456352531 ) ) ;
#128066 = CARTESIAN_POINT ( 'NONE',  ( 1.042430265417312985, -1.369658564370433540, -1.073568199598630146 ) ) ;
#128067 = AXIS2_PLACEMENT_3D ( 'NONE', #205036, #55607, #72909 ) ;
#128068 = FACE_OUTER_BOUND ( 'NONE', #207644, .T. ) ;
#128069 = CARTESIAN_POINT ( 'NONE',  ( 0.9656601056488465229, 1.412931828189394556, 1.004572000263863840 ) ) ;
#128070 = CARTESIAN_POINT ( 'NONE',  ( -0.6801582343750282034, 0.4635416670080716450, 1.178068619123793015 ) ) ;
#128071 = CARTESIAN_POINT ( 'NONE',  ( -11.33772463945037146, 12.69999999999998153, 3.599999999999999201 ) ) ;
#128072 = CARTESIAN_POINT ( 'NONE',  ( 0.9421113726552653445, 1.458074577165750396, 1.608915699534870569 ) ) ;
#128073 = CARTESIAN_POINT ( 'NONE',  ( 1.956267901341804283, -1.236798062192035363, 1.592663274815858676 ) ) ;
#128074 = CARTESIAN_POINT ( 'NONE',  ( 4.500000000000003553, -2.561000571632643674E-13, -2.052068128417943171 ) ) ;
#128075 = CARTESIAN_POINT ( 'NONE',  ( -1.500000000000013101, 1.702083334016151417, 0.8660254037844403729 ) ) ;
#128076 = CARTESIAN_POINT ( 'NONE',  ( 6.129514107576198967, -1.813157573415961066, 0.6514091821806231586 ) ) ;
#128077 = CARTESIAN_POINT ( 'NONE',  ( 0.6823417656249934904, 13.19270833367473195, 1.181850606188764807 ) ) ;
#128078 = CARTESIAN_POINT ( 'NONE',  ( 2.883289241188752072, -2.054055030226094480, -0.8463503915563088675 ) ) ;
#128079 = ORIENTED_EDGE ( 'NONE', *, *, #39947, .T. ) ;
#128080 = CARTESIAN_POINT ( 'NONE',  ( -9.578245405452070926, -9.921948021430829101, 0.1647502191513203207 ) ) ;
#128081 = CARTESIAN_POINT ( 'NONE',  ( -1.500000000000015099, -1.079166666666641961, 0.8660254037844403729 ) ) ;
#128082 = CARTESIAN_POINT ( 'NONE',  ( 9.413438726589914651, 9.876766690643398405, 0.000000000000000000 ) ) ;
#128083 = CARTESIAN_POINT ( 'NONE',  ( 5.935049520445493165, -1.266825670006064275, -1.193719461430408968 ) ) ;
#128084 = CARTESIAN_POINT ( 'NONE',  ( 3.947668504265917644, 1.419370528949075005, 1.354593381527373186 ) ) ;
#128086 = CARTESIAN_POINT ( 'NONE',  ( -6.914295153289458540, 7.169025221700239925, 0.7216878364870317197 ) ) ;
#128085 = CARTESIAN_POINT ( 'NONE',  ( 3.440018289565364817, 5.036440642624797626, 1.599625672291267398 ) ) ;
#128087 = CARTESIAN_POINT ( 'NONE',  ( -1.392149563160024472, 4.335119153505146983, -0.1376214334732279998 ) ) ;
#128088 = CARTESIAN_POINT ( 'NONE',  ( 4.710415318105323657, -0.9616676431317521256, -2.047968690232481848 ) ) ;
#128089 = CARTESIAN_POINT ( 'NONE',  ( 1.855998075696059901, -0.6969055236651957586, 1.941492863836144611 ) ) ;
#128090 = CARTESIAN_POINT ( 'NONE',  ( -5.357443255694392725, 9.402100898285455699, 0.000000000000000000 ) ) ;
#128091 = ORIENTED_EDGE ( 'NONE', *, *, #133645, .T. ) ;
#128092 = CARTESIAN_POINT ( 'NONE',  ( 1.499999999999989120, 0.8062500006828163812, 0.000000000000000000 ) ) ;
#128093 = CARTESIAN_POINT ( 'NONE',  ( 3.778450875046265534, -1.801938340082277712, -0.5016190811713144848 ) ) ;
#128094 = CARTESIAN_POINT ( 'NONE',  ( 2.496349097179047405, -1.714988558773246741, 0.2561001183170578677 ) ) ;
#128095 = CARTESIAN_POINT ( 'NONE',  ( 6.603104432341277530, -0.4828188497946246382, 2.145653685147373313 ) ) ;
#128096 = CARTESIAN_POINT ( 'NONE',  ( 0.1302870565101400258, -1.360178740744298675, -1.738515015553928622 ) ) ;
#128097 = CARTESIAN_POINT ( 'NONE',  ( 3.450221060135277629, 2.161883445724331665, 0.001893877739161941697 ) ) ;
#128098 = CARTESIAN_POINT ( 'NONE',  ( 4.329980137697307718, 1.904743498531726198, 0.3774997404530285317 ) ) ;
#128099 = CARTESIAN_POINT ( 'NONE',  ( -4.744990574658554117, 4.638169879964154418, 1.214306433183764966E-14 ) ) ;
#128101 = UNCERTAINTY_MEASURE_WITH_UNIT (LENGTH_MEASURE( 1.000000000000000082E-05 ), #8072, 'distance_accuracy_value', 'NONE');
#128100 = CARTESIAN_POINT ( 'NONE',  ( 6.555916519444559221, 1.865492442988415656, -0.1378669075578625169 ) ) ;
#128102 = CARTESIAN_POINT ( 'NONE',  ( 4.147051400439892177, 7.400425289818373109, 0.7480841269332880739 ) ) ;
#128103 = FACE_OUTER_BOUND ( 'NONE', #100730, .T. ) ;
#128104 = CARTESIAN_POINT ( 'NONE',  ( -0.1049925189658337810, -2.058569791948822392, -0.5088776734372552069 ) ) ;
#128105 = CARTESIAN_POINT ( 'NONE',  ( 0.6801582343750004478, 2.057291667008069425, -1.178068619123876282 ) ) ;
#128106 = CARTESIAN_POINT ( 'NONE',  ( 6.223279759862190730, 1.994869330463379331, 0.2930738960792296233 ) ) ;
#128107 = CARTESIAN_POINT ( 'NONE',  ( -2.779058300676980675, 5.225689869889666106, -1.082531754730543083 ) ) ;
#128108 = CARTESIAN_POINT ( 'NONE',  ( 8.959240580532112475, 9.346868853575953651, -0.7998128361456221525 ) ) ;
#128109 = LINE ( 'NONE', #176762, #91075 ) ;
#128110 = CARTESIAN_POINT ( 'NONE',  ( 2.807047293222181494, 1.542382716246639474, 0.9765254425028799812 ) ) ;
#128111 = CARTESIAN_POINT ( 'NONE',  ( 2.555956245031346885, 0.5892994983645870599, -2.126554282292691500 ) ) ;
#128112 = EDGE_LOOP ( 'NONE', ( #202594, #157792, #159167, #111590 ) ) ;
#128113 = CARTESIAN_POINT ( 'NONE',  ( -5.451787166026575981, 5.533042246551999277, 0.000000000000000000 ) ) ;
#128114 = DIRECTION ( 'NONE',  ( -1.000000000000000000, 0.000000000000000000, 0.000000000000000000 ) ) ;
#128115 = CARTESIAN_POINT ( 'NONE',  ( -8.694856585065634746, 9.038420858865048757, 0.7998128361456462443 ) ) ;
#128116 = CARTESIAN_POINT ( 'NONE',  ( 0.4924518904856821089, -1.118466686806585342, 1.681619975139287515 ) ) ;
#128117 = CARTESIAN_POINT ( 'NONE',  ( 0.6980877996264934771, 1.427081234210248573, 1.568565553304770877 ) ) ;
#128118 = CARTESIAN_POINT ( 'NONE',  ( -5.315678745009726924, 8.359319748223434487, -1.199719254218453823 ) ) ;
#128119 = CARTESIAN_POINT ( 'NONE',  ( 1.481066496106745234, -0.05241980694788496431, 1.860401082089859770 ) ) ;
#128120 = CARTESIAN_POINT ( 'NONE',  ( 5.040934186182656873, 4.775511393501539636, 1.040834085586084257E-14 ) ) ;
#128121 = CARTESIAN_POINT ( 'NONE',  ( 6.438362351209899082, 2.038089008908655853, 0.3048918457534201543 ) ) ;
#128122 = CARTESIAN_POINT ( 'NONE',  ( 6.223279759862189842, 1.994869330463379553, 0.2930738960792296233 ) ) ;
#128123 = ORIENTED_EDGE ( 'NONE', *, *, #16995, .T. ) ;
#128124 = ORIENTED_EDGE ( 'NONE', *, *, #196046, .T. ) ;
#128125 = CARTESIAN_POINT ( 'NONE',  ( -8.611400122974211868, 13.19838391011195888, 1.040834085586084257E-14 ) ) ;
#128126 = CARTESIAN_POINT ( 'NONE',  ( 3.896943178251357054, 1.541351720387572843, -0.9781566455248569270 ) ) ;
#128128 = CARTESIAN_POINT ( 'NONE',  ( -5.594971466091354095, 6.350553869658721595, -1.210626573312810761 ) ) ;
#128127 = CARTESIAN_POINT ( 'NONE',  ( -4.655245641445871385, 6.524482229810530498, 1.599625672291263179 ) ) ;
#128129 = CARTESIAN_POINT ( 'NONE',  ( 5.678247172832384670, 7.430942480705488684, 1.324022058552588366 ) ) ;
#128130 = CARTESIAN_POINT ( 'NONE',  ( 6.731795954091533751, -1.842168972580451314, -0.8196458303668037182 ) ) ;
#128131 = CARTESIAN_POINT ( 'NONE',  ( 6.228435704027582176, 0.1854037366294820077, 1.831779187086844729 ) ) ;
#128132 = CARTESIAN_POINT ( 'NONE',  ( -4.260029445439585061, 7.236136616047151193, -2.420000000000000373 ) ) ;
#128133 = CARTESIAN_POINT ( 'NONE',  ( 4.389522222404328211, 2.062498103173298514, -1.035318202965694434 ) ) ;
#128134 = CARTESIAN_POINT ( 'NONE',  ( 4.746236293235721604, 7.694970221153795364, 1.199719254218451159 ) ) ;
#128135 = CARTESIAN_POINT ( 'NONE',  ( 6.169229141836320096, 0.1658205177522271700, -2.155315574850395155 ) ) ;
#128136 = CARTESIAN_POINT ( 'NONE',  ( 6.470265622219697477, 8.571729197388226140, -1.599625672291262513 ) ) ;
#128137 = CARTESIAN_POINT ( 'NONE',  ( 0.6615421549095920062, 0.9584981283930308349, 1.688995467024148045 ) ) ;
#128138 = EDGE_CURVE ( 'NONE', #102037, #105543, #141889, .T. ) ;
#128139 = ORIENTED_EDGE ( 'NONE', *, *, #186547, .T. ) ;
#128140 = CIRCLE ( 'NONE', #121310, 12.00000000000000178 ) ;
#128141 = EDGE_CURVE ( 'NONE', #110540, #75662, #10760, .T. ) ;
#128142 = CARTESIAN_POINT ( 'NONE',  ( 4.218341386676929261, -1.908100849112413178, -1.281069462185228325 ) ) ;
#128143 = DIRECTION ( 'NONE',  ( 1.000000000000000000, 0.000000000000000000, 0.000000000000000000 ) ) ;
#128144 = CARTESIAN_POINT ( 'NONE',  ( -8.100070429521727178, 8.414780020722290033, 0.7998128361456341429 ) ) ;
#128145 = CARTESIAN_POINT ( 'NONE',  ( 5.137510444216992767, -1.323429205136433140, -1.322332877454430955 ) ) ;
#128146 = ORIENTED_EDGE ( 'NONE', *, *, #176248, .F. ) ;
#128149 = CARTESIAN_POINT ( 'NONE',  ( -4.285259070371116863, 7.157163461145040095, 1.199719254218452935 ) ) ;
#128148 = CARTESIAN_POINT ( 'NONE',  ( 0.7499999999999885647, 0.5979166673494851203, -1.299038105676652899 ) ) ;
#128147 = CARTESIAN_POINT ( 'NONE',  ( 2.109489925670060551, 1.480643174185194200, 1.210387159491378650 ) ) ;
#128150 = CARTESIAN_POINT ( 'NONE',  ( 3.528125218122651230, -1.314342534882004809, -1.772652456903674567 ) ) ;
#128151 = CARTESIAN_POINT ( 'NONE',  ( 6.883263157960407774, 1.288564682660230831, 1.962666442651111565 ) ) ;
#128152 = CARTESIAN_POINT ( 'NONE',  ( 2.703961570921634028, 5.242040035128820108, -1.199719254218446718 ) ) ;
#128153 = CARTESIAN_POINT ( 'NONE',  ( 6.821160681006793070, 7.130644680695653825, 0.7216878364870328300 ) ) ;
#128154 = CARTESIAN_POINT ( 'NONE',  ( -9.646789991323334590, 11.21334206375407305, 1.199719254218462483 ) ) ;
#128155 = CARTESIAN_POINT ( 'NONE',  ( -4.936577328707246082, 8.773440960218172435, 0.000000000000000000 ) ) ;
#128156 = CARTESIAN_POINT ( 'NONE',  ( 1.212115688179933759, -0.8827433895065642799, -1.762721879769993283 ) ) ;
#128157 = CARTESIAN_POINT ( 'NONE',  ( 1.062054608305310177, 0.4471719227481777414, -2.263690193671878514 ) ) ;
#128158 = CARTESIAN_POINT ( 'NONE',  ( 2.312880826517309085, -1.518475810973318074, 1.242258525517292433 ) ) ;
#128159 = CARTESIAN_POINT ( 'NONE',  ( -5.448397627845328550, 7.449826213943242514, 1.599625672291263401 ) ) ;
#128160 = CARTESIAN_POINT ( 'NONE',  ( 5.102416002207363022, 2.056666295747246576, 0.1571963825151497518 ) ) ;
#128161 = CARTESIAN_POINT ( 'NONE',  ( 4.202664430556247055, 6.886563688082179446, 1.082531754730558626 ) ) ;
#128162 = CARTESIAN_POINT ( 'NONE',  ( 5.554000203453580475, 6.508696987897830688, -1.199719254218452047 ) ) ;
#128163 = ORIENTED_EDGE ( 'NONE', *, *, #62788, .T. ) ;
#128164 = CARTESIAN_POINT ( 'NONE',  ( 8.499999999999980460, 6.200000000000038369, 2.873333333333345951 ) ) ;
#128165 = CARTESIAN_POINT ( 'NONE',  ( 0.000000000000000000, 6.999999999999999112, 0.000000000000000000 ) ) ;
#128166 = CARTESIAN_POINT ( 'NONE',  ( 10.39640486358069360, 11.02356051713265650, 0.7998128361456462443 ) ) ;
#128167 = CARTESIAN_POINT ( 'NONE',  ( 1.253040875654364505, -0.5252153140962511069, -2.106489908942406952 ) ) ;
#128168 = CARTESIAN_POINT ( 'NONE',  ( 4.206772801990143584, 8.129928378955675328, 0.7998128361456271485 ) ) ;
#128169 = CARTESIAN_POINT ( 'NONE',  ( 11.07693626658187824, 1.970899860167824924, -4.005980692925287023 ) ) ;
#128170 = CARTESIAN_POINT ( 'NONE',  ( -10.42995565840379335, 1.000000000000000888, 5.797106512947690860 ) ) ;
#128171 = CARTESIAN_POINT ( 'NONE',  ( 2.495189509527053762, 1.443206194050347557, 1.189963633554675937 ) ) ;
#128172 = CARTESIAN_POINT ( 'NONE',  ( 6.889893180375397996, -0.9309023296741396614, 1.948985471107896439 ) ) ;
#128174 = CARTESIAN_POINT ( 'NONE',  ( 6.827182134110195477, 0.006757161851597691914, 1.710856279483467413 ) ) ;
#128173 = CARTESIAN_POINT ( 'NONE',  ( 0.07755575628181492209, 4.082361791518872352, -2.743585103993382734 ) ) ;
#128175 = EDGE_CURVE ( 'NONE', #512, #58907, #170495, .T. ) ;
#128176 = CARTESIAN_POINT ( 'NONE',  ( 1.364683531249986537, -0.8447916663252468261, -0.7879004041258309554 ) ) ;
#128177 = CARTESIAN_POINT ( 'NONE',  ( 2.033716200607054159, -1.854476301366870583, 0.4660679227486629883 ) ) ;
#128178 = AXIS2_PLACEMENT_3D ( 'NONE', #143483, #211619, #158631 ) ;
#128179 = CARTESIAN_POINT ( 'NONE',  ( 4.117836676938036788, -0.9100935957705791335, -1.517748890920249671 ) ) ;
#128180 = CARTESIAN_POINT ( 'NONE',  ( 2.262237773093742188, 1.911903731097279513, 0.04523801603947830152 ) ) ;
#128181 = CARTESIAN_POINT ( 'NONE',  ( -6.013204822860843457, 6.974159367214481264, -1.199719254218446718 ) ) ;
#128183 = CARTESIAN_POINT ( 'NONE',  ( 5.870691181925934643, -0.2860506952705432204, -1.894010149965511758 ) ) ;
#128182 = DIRECTION ( 'NONE',  ( 0.000000000000000000, 0.000000000000000000, -1.000000000000000000 ) ) ;
#128184 = CARTESIAN_POINT ( 'NONE',  ( -1.500000000000001332, -0.5999999999999755529, 0.000000000000000000 ) ) ;
#128185 = CARTESIAN_POINT ( 'NONE',  ( 0.2388460773940295212, -2.007853281042128568, -0.5044432775610437902 ) ) ;
#128186 = CARTESIAN_POINT ( 'NONE',  ( 1.364683531249988757, -0.5531249996585801965, 0.000000000000000000 ) ) ;
#128187 = SURFACE_STYLE_FILL_AREA ( #123131 ) ;
#128188 = CARTESIAN_POINT ( 'NONE',  ( 5.207814216083940018, -1.861544245658670604, 0.1842191830812092979 ) ) ;
#128190 = ORIENTED_EDGE ( 'NONE', *, *, #112880, .T. ) ;
#128189 = CARTESIAN_POINT ( 'NONE',  ( 1.875362892791394787, 1.747422460009705913, -0.5287960245906262458 ) ) ;
#128192 = CARTESIAN_POINT ( 'NONE',  ( 4.920187338115698417, 7.999083482620499730, 0.9937779052983791717 ) ) ;
#128191 = CARTESIAN_POINT ( 'NONE',  ( 4.705825944637973990, -0.5905853116198942487, 2.126329296355852883 ) ) ;
#128193 = CARTESIAN_POINT ( 'NONE',  ( -0.6823417656249969321, 5.780208333674756283, -1.181850606188749264 ) ) ;
#128194 = CARTESIAN_POINT ( 'NONE',  ( 3.297386996040070795, -1.820318649397782318, 0.9700563119749375796 ) ) ;
#128195 = CARTESIAN_POINT ( 'NONE',  ( 6.647575389402066826, 6.649926130590872120, 1.040834085586084257E-14 ) ) ;
#128196 = CARTESIAN_POINT ( 'NONE',  ( -8.701635661872465732, 9.046329781806354831, 1.040834085586084257E-14 ) ) ;
#128197 = LINE ( 'NONE', #30614, #168311 ) ;
#128198 = CARTESIAN_POINT ( 'NONE',  ( 8.204655514564224816, 12.72384853363364066, 1.040834085586084257E-14 ) ) ;
#128199 = CARTESIAN_POINT ( 'NONE',  ( 1.499708767979548218, 3.350898811426534341, -0.07854769233531268269 ) ) ;
#128200 = CARTESIAN_POINT ( 'NONE',  ( 0.000000000000000000, 6.468705557303652931, -4.925226524755051294 ) ) ;
#128201 = CARTESIAN_POINT ( 'NONE',  ( 6.180537922983273091, 8.303989891604203422, -1.599625672291281386 ) ) ;
#128202 = VERTEX_POINT ( 'NONE', #163441 ) ;
#128203 = CARTESIAN_POINT ( 'NONE',  ( 5.090316257491098284, 1.067296284200716983, -1.773933887923849984 ) ) ;
#128204 = CARTESIAN_POINT ( 'NONE',  ( 1.364683531249986981, -1.053124999658580752, 0.000000000000000000 ) ) ;
#128205 = CARTESIAN_POINT ( 'NONE',  ( 2.618638089201937635, 1.414096770131420655, -1.634928933042498533 ) ) ;
#128206 = CARTESIAN_POINT ( 'NONE',  ( -4.940673843451318881, 7.995311821131723562, 1.007273293859496155 ) ) ;
#128207 = CARTESIAN_POINT ( 'NONE',  ( 3.703775025860293724, 1.464345522003915878, 1.391222453660536873 ) ) ;
#128208 = CARTESIAN_POINT ( 'NONE',  ( 6.720655732516672920, 1.239197277384354035, 2.287559680360019332 ) ) ;
#128209 = EDGE_LOOP ( 'NONE', ( #164504, #138179, #150828, #190856 ) ) ;
#128210 = ADVANCED_FACE ( 'NONE', ( #47573 ), #124799, .T. ) ;
#128212 = CARTESIAN_POINT ( 'NONE',  ( 7.836249599018724865, 9.205007956019091608, -1.082531754730537976 ) ) ;
#128211 = CARTESIAN_POINT ( 'NONE',  ( 1.737500000000001155, -1.983333333333333393, 3.009438278150922130 ) ) ;
#128213 = CARTESIAN_POINT ( 'NONE',  ( -3.160459205317013076, 6.701303149596211206, -0.7216878364870458196 ) ) ;
#128214 = CARTESIAN_POINT ( 'NONE',  ( 1.358611653602972646, -1.916354379050893009, -0.6279873632355145174 ) ) ;
#128215 = CARTESIAN_POINT ( 'NONE',  ( 6.075747529084263299, -1.173811750163206158, 1.850510016281024850 ) ) ;
#128216 = CARTESIAN_POINT ( 'NONE',  ( 1.499999999999990896, 4.556250000682819490, 1.214306433183764966E-14 ) ) ;
#128217 = CARTESIAN_POINT ( 'NONE',  ( 4.922078805074791674, -1.902621863305080430, 0.1933406509087298719 ) ) ;
#128218 = CARTESIAN_POINT ( 'NONE',  ( -4.386226389220933441, 5.076017861301227008, -1.199719254218446718 ) ) ;
#128219 = CARTESIAN_POINT ( 'NONE',  ( 7.253248993186735660, 7.564471368247083660, 0.7216878364870317197 ) ) ;
#128221 = CARTESIAN_POINT ( 'NONE',  ( 2.812125237574263803, 1.117814398428567557, -1.678018709429726307 ) ) ;
#128220 = CARTESIAN_POINT ( 'NONE',  ( -8.798878505144648088, 12.24881344176869469, -1.082531754730543083 ) ) ;
#128222 = CARTESIAN_POINT ( 'NONE',  ( -1.402160292154681736E-14, 13.98437500034139624, 1.575800808251682339 ) ) ;
#128223 = CARTESIAN_POINT ( 'NONE',  ( -5.490125858891038213, 5.369844688319787451, -0.7998128361456362523 ) ) ;
#128224 = CARTESIAN_POINT ( 'NONE',  ( 5.139545982361763521, -1.221863454424999329, -1.217595815693907957 ) ) ;
#128225 = CARTESIAN_POINT ( 'NONE',  ( 8.011942431032855083, 8.311964022485323511, 0.7998128361456291469 ) ) ;
#128226 = CARTESIAN_POINT ( 'NONE',  ( 2.846322183865124700, 5.408127416896231665, -1.199719254218446718 ) ) ;
#128227 = CARTESIAN_POINT ( 'NONE',  ( -1.499999999999997780, 4.650000000000022560, 1.214306433183764966E-14 ) ) ;
#128228 = EDGE_CURVE ( 'NONE', #138011, #189127, #4902, .T. ) ;
#128229 = CARTESIAN_POINT ( 'NONE',  ( -2.907411709271221945, 6.510044087496495990, 0.000000000000000000 ) ) ;
#128230 = CARTESIAN_POINT ( 'NONE',  ( 1.288034235163344254, -1.310400469390052836, -1.602789277989056016 ) ) ;
#128231 = DIRECTION ( 'NONE',  ( 0.000000000000000000, -1.000000000000000000, 0.000000000000000000 ) ) ;
#128232 = ORIENTED_EDGE ( 'NONE', *, *, #205195, .T. ) ;
#128233 = CARTESIAN_POINT ( 'NONE',  ( 5.074790875859057415, -1.308146702057958910, 1.253318493144810697 ) ) ;
#128234 = CARTESIAN_POINT ( 'NONE',  ( 4.746236293235721604, 7.694970221153795364, 1.199719254218451159 ) ) ;
#128235 = CYLINDRICAL_SURFACE ( 'NONE', #35670, 0.09999999999999999167 ) ;
#128236 = CARTESIAN_POINT ( 'NONE',  ( 6.094382945298186804, -0.9628849012233617888, 1.534170072110131899 ) ) ;
#128237 = CARTESIAN_POINT ( 'NONE',  ( 6.170369307550823912, 7.331757292631694511, 1.082531754730549967 ) ) ;
#128238 = CARTESIAN_POINT ( 'NONE',  ( 11.97505132285663443, 7.681807955339387206, 0.8856721426690242760 ) ) ;
#128239 = CARTESIAN_POINT ( 'NONE',  ( 3.521585679250069045, -1.305302140894725627, -1.760141160621036649 ) ) ;
#128240 = ORIENTED_EDGE ( 'NONE', *, *, #58178, .T. ) ;
#128242 = CARTESIAN_POINT ( 'NONE',  ( 8.914649696185335870, 10.35917838609310593, -1.199719254218446718 ) ) ;
#128241 = CARTESIAN_POINT ( 'NONE',  ( 0.2210476084268316321, -1.750679471464357650, -0.8856473702157914296 ) ) ;
#128243 = CARTESIAN_POINT ( 'NONE',  ( 4.499565103457034532, -1.877818951341524878, 0.3776799693050793549 ) ) ;
#128244 = CARTESIAN_POINT ( 'NONE',  ( -11.78331023100045627, 9.719999999999982876, 1.799999999999999600 ) ) ;
#128245 = CARTESIAN_POINT ( 'NONE',  ( -6.286530415420750195, 6.898050863092263896, 0.7571273896394186131 ) ) ;
#128246 = FACE_OUTER_BOUND ( 'NONE', #106790, .T. ) ;
#128247 = CARTESIAN_POINT ( 'NONE',  ( 1.364683531249986537, 0.1135416670080857532, 0.7879004041258500513 ) ) ;
#128249 = ORIENTED_EDGE ( 'NONE', *, *, #82633, .F. ) ;
#128248 = CARTESIAN_POINT ( 'NONE',  ( 4.189106276942576201, 7.831115056500907556, 1.040834085586084257E-14 ) ) ;
#128250 = ADVANCED_FACE ( 'NONE', ( #40667 ), #141398, .T. ) ;
#128251 = CARTESIAN_POINT ( 'NONE',  ( -8.839552966430012759, 10.37552855133225904, -1.082531754730543971 ) ) ;
#128252 = CARTESIAN_POINT ( 'NONE',  ( 2.131903390035182255, -1.411712784473453830, -1.637176306262012826 ) ) ;
#128253 = CARTESIAN_POINT ( 'NONE',  ( -4.984557751679625781, 5.844347460828191565, 1.199719254218452935 ) ) ;
#128254 = CARTESIAN_POINT ( 'NONE',  ( 5.713835393516482952, 5.630839145382857680, 0.7998128361456352531 ) ) ;
#128255 = CARTESIAN_POINT ( 'NONE',  ( 1.571042225754931465, 0.1381101175703668971, -1.820421783975199048 ) ) ;
#128256 = CARTESIAN_POINT ( 'NONE',  ( -0.1577409392781377873, -1.310076727147227560, -1.668215054097483385 ) ) ;
#128257 = ADVANCED_FACE ( 'NONE', ( #57962 ), #206300, .T. ) ;
#128258 = CARTESIAN_POINT ( 'NONE',  ( 5.227504313999177477, -1.733024862908550290, 0.5741523302658231298 ) ) ;
#128259 = CARTESIAN_POINT ( 'NONE',  ( 8.414596756380271714, 12.86228968013755747, 8.493303441398989406 ) ) ;
#128260 = CARTESIAN_POINT ( 'NONE',  ( 2.759904966095374501, 0.6844231338998980618, -1.785916880244736715 ) ) ;
#128261 = ORIENTED_EDGE ( 'NONE', *, *, #12966, .F. ) ;
#128262 = CARTESIAN_POINT ( 'NONE',  ( 3.490635713810024132, 1.920951117756137583, 0.4340392168088512692 ) ) ;
#128263 = ORIENTED_EDGE ( 'NONE', *, *, #165616, .F. ) ;
#128264 = CARTESIAN_POINT ( 'NONE',  ( 6.515186996419942034, -1.882659881547473546, 0.4762376372081030262 ) ) ;
#128265 = ORIENTED_EDGE ( 'NONE', *, *, #127295, .T. ) ;
#128266 = CARTESIAN_POINT ( 'NONE',  ( -7.259464905474441565, 7.434073576000447048, -0.7998128361456362523 ) ) ;
#128268 = CARTESIAN_POINT ( 'NONE',  ( 5.783468009189684622, 0.1541500780414573890, -2.115021274163720211 ) ) ;
#128267 = CARTESIAN_POINT ( 'NONE',  ( 6.261886844665240481, 8.398896966899865646, 1.599625672291268286 ) ) ;
#128269 = CARTESIAN_POINT ( 'NONE',  ( 7.661766205054107992, 8.111351125417501251, -0.7216878364870317197 ) ) ;
#128271 = ORIENTED_EDGE ( 'NONE', *, *, #166654, .T. ) ;
#128270 = CARTESIAN_POINT ( 'NONE',  ( 3.984940423737866055, -1.785409543757199291, -0.6854135386504257577 ) ) ;
#128272 = CARTESIAN_POINT ( 'NONE',  ( 4.286934996870309433, 7.472684718058654418, -1.056577385247484457 ) ) ;
#128273 = CARTESIAN_POINT ( 'NONE',  ( -2.103486388414573138, 5.605817886458954291, 1.040834085586084257E-14 ) ) ;
#128274 = CARTESIAN_POINT ( 'NONE',  ( 5.063044020060520900, 4.871582543017558109, 0.7998128361456352531 ) ) ;
#128275 = CIRCLE ( 'NONE', #124853, 11.92000000000000171 ) ;
#128276 = CARTESIAN_POINT ( 'NONE',  ( 4.846344381697188730, 1.033023791896072519, -1.727689222339493069 ) ) ;
#128277 = CARTESIAN_POINT ( 'NONE',  ( 0.09623479069433779620, -9.919835240146305466, 9.499512666137798433 ) ) ;
#128278 = CARTESIAN_POINT ( 'NONE',  ( 5.584540971669589737, -1.782103179330214449, -0.3958202769075992444 ) ) ;
#128279 = CARTESIAN_POINT ( 'NONE',  ( 0.3618904354094238940, -0.5536326762660361833, 1.994880328902041589 ) ) ;
#128280 = CARTESIAN_POINT ( 'NONE',  ( -8.676855123066030018, 9.225345186439589895, -0.7216878364870267237 ) ) ;
#128281 = CARTESIAN_POINT ( 'NONE',  ( -5.527359202251545867, 7.456348097644321271, -1.248928334283349040 ) ) ;
#128282 = CARTESIAN_POINT ( 'NONE',  ( 0.6124999999999898304, 1.916666666666677621, -1.060881119635962211 ) ) ;
#128283 = CARTESIAN_POINT ( 'NONE',  ( 6.666881909320486521, -1.711340306973156977, -0.7558587634414122292 ) ) ;
#128284 = CARTESIAN_POINT ( 'NONE',  ( 6.262976894508937242, 9.394224579314053969, -1.199719254218440723 ) ) ;
#128285 = CARTESIAN_POINT ( 'NONE',  ( -4.192495815123837843, 5.914331089109674977, -1.599625672291256517 ) ) ;
#128286 = CARTESIAN_POINT ( 'NONE',  ( 4.701980345841006326, 4.380065246436280368, 0.7998128361456341429 ) ) ;
#128287 = CARTESIAN_POINT ( 'NONE',  ( -1.364683531250014514, 11.15104166700806232, -0.7879004041258335089 ) ) ;
#128288 = CARTESIAN_POINT ( 'NONE',  ( -4.680589345215810049, 6.483773540883647435, -1.599625672291256295 ) ) ;
#128290 = CARTESIAN_POINT ( 'NONE',  ( -5.935437387732586778, 10.14670372898850381, -0.7998128361456362523 ) ) ;
#128289 = FILL_AREA_STYLE_COLOUR ( '', #41627 ) ;
#128291 = CARTESIAN_POINT ( 'NONE',  ( 3.392920078539514162, -0.7062313252990999324, -1.584032799413936710 ) ) ;
#128292 = CARTESIAN_POINT ( 'NONE',  ( -6.091691091241777656, 6.001394449403842479, 0.7998128361456341429 ) ) ;
#128293 = CARTESIAN_POINT ( 'NONE',  ( 1.182579820358391931, 1.236233925375467058, -1.660450453320160058 ) ) ;
#128294 = CARTESIAN_POINT ( 'NONE',  ( 1.986098615764248398, -2.116669865667855088, 0.05555418577087371801 ) ) ;
#128295 = CARTESIAN_POINT ( 'NONE',  ( 3.669453130792974971, 7.432779085900453886, 1.040834085586084257E-14 ) ) ;
#128296 = CARTESIAN_POINT ( 'NONE',  ( 7.065770611016287006, 11.39514947949436774, 1.040834085586084257E-14 ) ) ;
#128297 = CARTESIAN_POINT ( 'NONE',  ( -0.1004607481840987110, 6.432248552227529004, 3.209664736303321497 ) ) ;
#128298 = CARTESIAN_POINT ( 'NONE',  ( 1.076931260867712625, 1.817606662292377218, 0.7587987759381797925 ) ) ;
#128299 = CARTESIAN_POINT ( 'NONE',  ( 4.369547513234953939, 7.382648021784232739, 1.157447143386416188 ) ) ;
#128300 = CARTESIAN_POINT ( 'NONE',  ( 4.473827502829567315, 7.202920605734387749, -1.082531754730548412 ) ) ;
#128302 = CARTESIAN_POINT ( 'NONE',  ( 1.214306433183764966E-14, 2.428612866367529932E-14, 1.500000000000001332 ) ) ;
#128301 = CARTESIAN_POINT ( 'NONE',  ( 0.000000000000000000, -1.137499999999999067, -4.012584370867899430 ) ) ;
#128303 = CARTESIAN_POINT ( 'NONE',  ( 2.027642443044708198, -1.499220162234589093, -1.734095823995058794 ) ) ;
#128304 = CARTESIAN_POINT ( 'NONE',  ( 0.9085097582094739943, 1.384192474337717194, -1.190531929384466503 ) ) ;
#128305 = CARTESIAN_POINT ( 'NONE',  ( 3.006014587165442453, -0.7710369221427433306, 1.750240277048662030 ) ) ;
#128306 = CARTESIAN_POINT ( 'NONE',  ( 5.668190738965027897, 8.770583741171307679, -1.199719254218452047 ) ) ;
#128307 = CARTESIAN_POINT ( 'NONE',  ( 7.768458830506048685, 8.165549511786275971, -0.7216878364870267237 ) ) ;
#128308 = CARTESIAN_POINT ( 'NONE',  ( -7.700141177557535244, 11.07091624287075859, -1.199719254218446718 ) ) ;
#128309 = CARTESIAN_POINT ( 'NONE',  ( 2.144791297303435762, 1.953827510466410455, 0.4849535144586021307 ) ) ;
#128310 = CARTESIAN_POINT ( 'NONE',  ( 1.657006586592904673, 1.606862555911577006, -1.125131163738995577 ) ) ;
#128311 = CARTESIAN_POINT ( 'NONE',  ( -8.134002093194872884, 11.57708731111429401, 1.199719254218453823 ) ) ;
#128312 = CARTESIAN_POINT ( 'NONE',  ( -8.525379664894808585, 8.840697785332414682, -0.7998128361456291469 ) ) ;
#128313 = CARTESIAN_POINT ( 'NONE',  ( -3.890826896997543471, 7.483122446565097619, 0.7216878364870037421 ) ) ;
#128315 = CARTESIAN_POINT ( 'NONE',  ( 3.520126680498508520, 1.123421168108656776, -1.367553765667248955 ) ) ;
#128314 = CARTESIAN_POINT ( 'NONE',  ( 5.296857843117306786, 1.708683220140273740, 1.204356289764816568 ) ) ;
#128316 = CARTESIAN_POINT ( 'NONE',  ( -1.878313713275644226, 13.99999999999692513, 12.68000002627077905 ) ) ;
#128318 = CARTESIAN_POINT ( 'NONE',  ( 6.369073578265099123, 2.195482680428318290, -0.6590174882785122534 ) ) ;
#128317 = DIRECTION ( 'NONE',  ( 0.000000000000000000, 1.000000000000000000, 0.000000000000000000 ) ) ;
#128319 = CARTESIAN_POINT ( 'NONE',  ( 4.857210178628561970, 1.720700030253617951, -0.2597475362437673407 ) ) ;
#128320 = CARTESIAN_POINT ( 'NONE',  ( 10.24048609702354717, 10.84165528948263457, -0.7998128361456281477 ) ) ;
#128321 = CARTESIAN_POINT ( 'NONE',  ( 8.064677165291193717, -5.223431457505076203, -7.446209719563348983 ) ) ;
#128322 = CARTESIAN_POINT ( 'NONE',  ( 4.903498277369322977, 0.2971982615034232111, 1.707963748468165122 ) ) ;
#128323 = AXIS2_PLACEMENT_3D ( 'NONE', #109147, #10490, #106998 ) ;
#128324 = CARTESIAN_POINT ( 'NONE',  ( 5.160662515399747186, -0.7266353732918430230, -2.046117350891932141 ) ) ;
#128325 = CARTESIAN_POINT ( 'NONE',  ( 2.523789150438203510, 6.096171108819874007, 0.7998128361456462443 ) ) ;
#128326 = CARTESIAN_POINT ( 'NONE',  ( -0.2349522205629230309, -0.1529240981989663239, -2.083514258294770105 ) ) ;
#128327 = CARTESIAN_POINT ( 'NONE',  ( 4.843750000000003553, 1.895863743164186710, 0.7852924748297296365 ) ) ;
#128328 = CARTESIAN_POINT ( 'NONE',  ( 1.499999999999989120, 5.327083334016152527, -0.8660254037844323793 ) ) ;
#128329 = CARTESIAN_POINT ( 'NONE',  ( 3.100521554045695627, -0.5575540177290801980, -1.843951249938739378 ) ) ;
#128330 = CARTESIAN_POINT ( 'NONE',  ( 1.499999999999993117, 9.635416667349465669, 0.8660254037844409281 ) ) ;
#128331 = CARTESIAN_POINT ( 'NONE',  ( 0.4170203200158085211, -0.7540967040414385814, -2.089506846138278195 ) ) ;
#128332 = VERTEX_POINT ( 'NONE', #18006 ) ;
#128333 = CARTESIAN_POINT ( 'NONE',  ( 6.883263157960408662, 2.979503955789930547, 2.299731230128279513 ) ) ;
#128334 = CARTESIAN_POINT ( 'NONE',  ( -1.500000000000013101, 2.879166666666688634, -0.8660254037844313801 ) ) ;
#128335 = CARTESIAN_POINT ( 'NONE',  ( 5.311043488251262268, 7.219303374425030562, -1.599625672291256295 ) ) ;
#128336 = CARTESIAN_POINT ( 'NONE',  ( 2.157158246434082827, 0.4899616716134093108, 2.166440146811992040 ) ) ;
#128337 = CARTESIAN_POINT ( 'NONE',  ( -0.02900071798687918478, 7.629137130509076492, -2.773797386654376584 ) ) ;
#128338 = CARTESIAN_POINT ( 'NONE',  ( 7.998947442382716488, 9.394822106610419610, -1.082531754730543083 ) ) ;
#128339 = CARTESIAN_POINT ( 'NONE',  ( -10.42585693878457853, 11.26584730477792284, -0.7216878364870267237 ) ) ;
#128340 = CARTESIAN_POINT ( 'NONE',  ( 7.349928672384119288, 8.707909884937221179, 1.082531754730549967 ) ) ;
#128341 = CARTESIAN_POINT ( 'NONE',  ( 1.020157974382044364, -1.821741137083273010, 0.8647263380179845971 ) ) ;
#128343 = CARTESIAN_POINT ( 'NONE',  ( 5.758276963478038191, -2.062851381910678850, -0.003602753815758196875 ) ) ;
#128342 = CARTESIAN_POINT ( 'NONE',  ( 8.809047120577066181, 11.30030761213851953, 1.599625672291281386 ) ) ;
#128344 = CARTESIAN_POINT ( 'NONE',  ( -11.89942855770814134, 13.88000000000000078, 0.6999999999999992895 ) ) ;
#128345 = CARTESIAN_POINT ( 'NONE',  ( -2.916975605234527702, 6.554888639415577423, 1.040834085586084257E-14 ) ) ;
#128346 = CARTESIAN_POINT ( 'NONE',  ( -1.364683531250000748, 1.259375000341421469, 0.000000000000000000 ) ) ;
#128347 = CARTESIAN_POINT ( 'NONE',  ( 6.784453417974287248, -1.834524189944960693, -0.3643881242741816573 ) ) ;
#128348 = CARTESIAN_POINT ( 'NONE',  ( 6.223290642006293893, 1.716731611696775683, 0.2442158411369663995 ) ) ;
#128349 = CARTESIAN_POINT ( 'NONE',  ( 5.811982450300033243, 1.162468279597946630, -1.295502344845029574 ) ) ;
#128350 = CARTESIAN_POINT ( 'NONE',  ( 3.105313311461850745, -0.4450742334846323756, 2.248595817482400783 ) ) ;
#128351 = CARTESIAN_POINT ( 'NONE',  ( -1.364683531250014514, -0.7614583329919104582, -0.7879004041258359514 ) ) ;
#128352 = CARTESIAN_POINT ( 'NONE',  ( 1.130510352786683326, -1.665311210022573540, 0.7854980884962547982 ) ) ;
#128353 = FACE_BOUND ( 'NONE', #171776, .T. ) ;
#128354 = CARTESIAN_POINT ( 'NONE',  ( 2.449991753796490368, 1.825138167369045661, 0.04731899098397300552 ) ) ;
#128355 = CARTESIAN_POINT ( 'NONE',  ( 2.813125141109920069, 1.117832431973438734, -1.678005364621336426 ) ) ;
#128356 = CARTESIAN_POINT ( 'NONE',  ( 1.412352946837617473, 1.469754387505791460, -1.625674263109680329 ) ) ;
#128357 = CARTESIAN_POINT ( 'NONE',  ( 8.806171940766564177, 13.38206018750110182, -7.684638306840279043 ) ) ;
#128358 = CARTESIAN_POINT ( 'NONE',  ( 4.629967194361879201, -1.293677666091449296, -1.661686202823991820 ) ) ;
#128359 = CARTESIAN_POINT ( 'NONE',  ( -7.877450944739929461, 9.149113176073413456, 1.199719254218462483 ) ) ;
#128360 = CARTESIAN_POINT ( 'NONE',  ( 7.740615115470229846, 13.97676715014342008, 10.04400721814316810 ) ) ;
#128361 =( BOUNDED_SURFACE ( )  B_SPLINE_SURFACE ( 1, 2, ( 
 ( #15241, #95484, #196154, #81328, #111768, #62940, #162592, #113908, #77052, #145310, #93343, #129108, #97600, #64014, #126973, #79195, #65056, #160448, #177775, #14166, #131212, #210246, #159379, #163659, #13117, #47794, #194002, #176700, #195082, #45651, #46720, #112833, #130162, #44587, #30460, #197200, #178849, #29390, #94409, #48839, #110700, #180953, #114953, #28313, #12055, #10978, #144253, #133310, #32576, #164709, #200383, #52031, #36826, #34696, #199315, #166847, #41, #16297, #35765, #152721, #82382, #202511, #50961, #20570, #4303, #116019, #151672, #150608, #119218, #148473, #67175, #3243, #54161, #184141, #185201, #118157, #17364, #66105, #83448, #117085, #183084, #136489, #69309, #100765, #132247, #101840, #167908, #102907, #2168, #201442, #134379, #168966, #135421, #19506, #68245, #120300, #198255, #18443, #85582, #98652, #49895, #53083, #84520, #86653, #70374, #182005, #33636, #99709, #165781, #149528, #1114, #157009, #6447, #58427, #170028, #140780, #108312, #204644, #55228, #56295, #40051, #158076, #123523, #7518, #154865, #188414, #103985, #205725, #174332, #141853, #139702, #124580, #74677, #9664, #90943, #206795, #87722, #187349, #8595 ),
 ( #21614, #72525, #190541, #207858, #189487, #42197, #57360, #171102, #153795, #22693, #138621, #122455, #75740, #25908, #106160, #71447, #41130, #107242, #92018, #89881, #59484, #73600, #186273, #37909, #173263, #155933, #5365, #137559, #172186, #24844, #203577, #121374, #38978, #23776, #105064, #88806, #60548, #125641, #45390, #161260, #109382, #179646, #96279, #160189, #212110, #175389, #79995, #47528, #143987, #208914, #209978, #193744, #97340, #62672, #12847, #94150, #127789, #43264, #145043, #113641, #81069, #78921, #63747, #13913, #163398, #30189, #146099, #26975, #126706, #162329, #14972, #129906, #195890, #93080, #111506, #31266, #192667, #61619, #128831, #147155, #28057, #191602, #213180, #177512, #159122, #11790, #44321, #211046, #77864, #29124, #194813, #10723, #76792, #46449, #178581, #95211, #112570, #110443, #142914, #176445, #152473, #168716, #148216, #98389, #35507, #117902, #165515, #64809, #196946, #18179, #84266, #69057, #66912, #17107, #199054, #32321, #48586, #67980, #184946, #114702, #20320, #83185, #52831, #36573, #214218, #50700, #116824, #149268, #101584, #151416, #49631, #150351, #847, #1921, #82123, #130956, #133052, #182826, #65847 ) ),
 .UNSPECIFIED., .F., .F., .T. ) 
 B_SPLINE_SURFACE_WITH_KNOTS ( ( 2, 2 ),
 ( 3, 2, 2, 2, 2, 2, 2, 2, 2, 2, 2, 2, 2, 2, 2, 2, 2, 2, 2, 2, 2, 2, 2, 2, 2, 2, 2, 2, 2, 2, 2, 2, 2, 2, 2, 2, 2, 2, 2, 2, 2, 2, 2, 2, 2, 2, 2, 2, 2, 2, 2, 2, 2, 2, 2, 2, 2, 2, 2, 2, 2, 2, 2, 2, 2, 2, 2, 2, 2, 3 ),
 ( 0.000000000000000000, 1.000000000000000000 ),
 ( 0.000000000000000000, 0.01388888888888888812, 0.02777777777777777624, 0.04166666666666666435, 0.05555555555555555247, 0.06944444444444444753, 0.08333333333333332871, 0.09722222222222222376, 0.1111111111111111049, 0.1250000000000000000, 0.1388888888888888951, 0.1527777777777777901, 0.1666666666666666574, 0.1805555555555555525, 0.1944444444444444475, 0.2083333333333333426, 0.2222222222222222099, 0.2361111111111111049, 0.2500000000000000000, 0.2638888888888888951, 0.2777777777777777901, 0.2916666666666666852, 0.3055555555555555802, 0.3194444444444444198, 0.3333333333333333148, 0.3472222222222222099, 0.3611111111111111049, 0.3750000000000000000, 0.3888888888888888951, 0.4027777777777777901, 0.4166666666666666852, 0.4305555555555555802, 0.4444444444444444198, 0.4583333333333333148, 0.4722222222222222099, 0.4861111111111111049, 0.5000000000000000000, 0.5138888888888888395, 0.5277777777777777901, 0.5416666666666666297, 0.5555555555555555802, 0.5694444444444444198, 0.5833333333333333703, 0.5972222222222222099, 0.6111111111111111605, 0.6250000000000000000, 0.6388888888888888395, 0.6527777777777777901, 0.6666666666666666297, 0.6805555555555555802, 0.6944444444444444198, 0.7083333333333333703, 0.7222222222222222099, 0.7361111111111111605, 0.7500000000000000000, 0.7638888888888888395, 0.7777777777777777901, 0.7916666666666666297, 0.8055555555555555802, 0.8194444444444444198, 0.8333333333333333703, 0.8472222222222222099, 0.8611111111111111605, 0.8750000000000000000, 0.8888888888888888395, 0.9027777777777777901, 0.9166666666666666297, 0.9305555555555555802, 0.9444444444444444198, 0.9523586252412667985 ),
 .UNSPECIFIED. ) 
 GEOMETRIC_REPRESENTATION_ITEM ( )  RATIONAL_B_SPLINE_SURFACE ( (
 ( 1.000000000000000000, 0.8660254037844387076, 1.000000000000000000, 0.8660254037844387076, 1.000000000000000000, 0.8660254037844387076, 1.000000000000000000, 0.8660254037844387076, 1.000000000000000000, 0.8660254037844387076, 1.000000000000000000, 0.8660254037844387076, 1.000000000000000000, 0.8660254037844387076, 1.000000000000000000, 0.8660254037844387076, 1.000000000000000000, 0.8660254037844387076, 1.000000000000000000, 0.8660254037844387076, 1.000000000000000000, 0.8660254037844387076, 1.000000000000000000, 0.8660254037844387076, 1.000000000000000000, 0.8660254037844387076, 1.000000000000000000, 0.8660254037844387076, 1.000000000000000000, 0.8660254037844387076, 1.000000000000000000, 0.8660254037844387076, 1.000000000000000000, 0.8660254037844387076, 1.000000000000000000, 0.8660254037844387076, 1.000000000000000000, 0.8660254037844387076, 1.000000000000000000, 0.8660254037844387076, 1.000000000000000000, 0.8660254037844387076, 1.000000000000000000, 0.8660254037844387076, 1.000000000000000000, 0.8660254037844387076, 1.000000000000000000, 0.8660254037844387076, 1.000000000000000000, 0.8660254037844387076, 1.000000000000000000, 0.8660254037844387076, 1.000000000000000000, 0.8660254037844387076, 1.000000000000000000, 0.8660254037844387076, 1.000000000000000000, 0.8660254037844387076, 1.000000000000000000, 0.8660254037844387076, 1.000000000000000000, 0.8660254037844387076, 1.000000000000000000, 0.8660254037844387076, 1.000000000000000000, 0.8660254037844387076, 1.000000000000000000, 0.8660254037844387076, 1.000000000000000000, 0.8660254037844387076, 1.000000000000000000, 0.8660254037844387076, 1.000000000000000000, 0.8660254037844387076, 1.000000000000000000, 0.8660254037844387076, 1.000000000000000000, 0.8660254037844387076, 1.000000000000000000, 0.8660254037844387076, 1.000000000000000000, 0.8660254037844387076, 1.000000000000000000, 0.8660254037844387076, 1.000000000000000000, 0.8660254037844387076, 1.000000000000000000, 0.8660254037844387076, 1.000000000000000000, 0.8660254037844387076, 1.000000000000000000, 0.8660254037844387076, 1.000000000000000000, 0.8660254037844387076, 1.000000000000000000, 0.8660254037844387076, 1.000000000000000000, 0.8660254037844387076, 1.000000000000000000, 0.8660254037844387076, 1.000000000000000000, 0.8660254037844387076, 1.000000000000000000, 0.8660254037844387076, 1.000000000000000000, 0.8660254037844387076, 1.000000000000000000, 0.8660254037844387076, 1.000000000000000000, 0.8660254037844387076, 1.000000000000000000, 0.8660254037844387076, 1.000000000000000000, 0.8660254037844387076, 1.000000000000000000, 0.8660254037844387076, 1.000000000000000000, 0.8660254037844387076, 1.000000000000000000, 0.8660254037844387076, 1.000000000000000000, 0.8660254037844387076, 1.000000000000000000, 0.8660254037844387076, 1.000000000000000000, 0.8660254037844387076, 1.000000000000000000, 0.8660254037844387076, 1.000000000000000000, 0.8660254037844387076, 1.000000000000000000, 0.8660254037844387076, 1.000000000000000000, 0.8660254037844387076, 1.000000000000000000, 0.8660254037844387076, 1.000000000000000000, 0.9236584592825519691, 0.9343189473637074638),
 ( 1.000000000000000000, 0.8660254037844387076, 1.000000000000000000, 0.8660254037844387076, 1.000000000000000000, 0.8660254037844387076, 1.000000000000000000, 0.8660254037844387076, 1.000000000000000000, 0.8660254037844387076, 1.000000000000000000, 0.8660254037844387076, 1.000000000000000000, 0.8660254037844387076, 1.000000000000000000, 0.8660254037844387076, 1.000000000000000000, 0.8660254037844387076, 1.000000000000000000, 0.8660254037844387076, 1.000000000000000000, 0.8660254037844387076, 1.000000000000000000, 0.8660254037844387076, 1.000000000000000000, 0.8660254037844387076, 1.000000000000000000, 0.8660254037844387076, 1.000000000000000000, 0.8660254037844387076, 1.000000000000000000, 0.8660254037844387076, 1.000000000000000000, 0.8660254037844387076, 1.000000000000000000, 0.8660254037844387076, 1.000000000000000000, 0.8660254037844387076, 1.000000000000000000, 0.8660254037844387076, 1.000000000000000000, 0.8660254037844387076, 1.000000000000000000, 0.8660254037844387076, 1.000000000000000000, 0.8660254037844387076, 1.000000000000000000, 0.8660254037844387076, 1.000000000000000000, 0.8660254037844387076, 1.000000000000000000, 0.8660254037844387076, 1.000000000000000000, 0.8660254037844387076, 1.000000000000000000, 0.8660254037844387076, 1.000000000000000000, 0.8660254037844387076, 1.000000000000000000, 0.8660254037844387076, 1.000000000000000000, 0.8660254037844387076, 1.000000000000000000, 0.8660254037844387076, 1.000000000000000000, 0.8660254037844387076, 1.000000000000000000, 0.8660254037844387076, 1.000000000000000000, 0.8660254037844387076, 1.000000000000000000, 0.8660254037844387076, 1.000000000000000000, 0.8660254037844387076, 1.000000000000000000, 0.8660254037844387076, 1.000000000000000000, 0.8660254037844387076, 1.000000000000000000, 0.8660254037844387076, 1.000000000000000000, 0.8660254037844387076, 1.000000000000000000, 0.8660254037844387076, 1.000000000000000000, 0.8660254037844387076, 1.000000000000000000, 0.8660254037844387076, 1.000000000000000000, 0.8660254037844387076, 1.000000000000000000, 0.8660254037844387076, 1.000000000000000000, 0.8660254037844387076, 1.000000000000000000, 0.8660254037844387076, 1.000000000000000000, 0.8660254037844387076, 1.000000000000000000, 0.8660254037844387076, 1.000000000000000000, 0.8660254037844387076, 1.000000000000000000, 0.8660254037844387076, 1.000000000000000000, 0.8660254037844387076, 1.000000000000000000, 0.8660254037844387076, 1.000000000000000000, 0.8660254037844387076, 1.000000000000000000, 0.8660254037844387076, 1.000000000000000000, 0.8660254037844387076, 1.000000000000000000, 0.8660254037844387076, 1.000000000000000000, 0.8660254037844387076, 1.000000000000000000, 0.8660254037844387076, 1.000000000000000000, 0.8660254037844387076, 1.000000000000000000, 0.8660254037844387076, 1.000000000000000000, 0.8660254037844387076, 1.000000000000000000, 0.8660254037844387076, 1.000000000000000000, 0.8660254037844387076, 1.000000000000000000, 0.8660254037844387076, 1.000000000000000000, 0.8660254037844387076, 1.000000000000000000, 0.8660254037844387076, 1.000000000000000000, 0.9236584592825519691, 0.9343189473637074638) ) ) 
 REPRESENTATION_ITEM ( '' )  SURFACE ( )  );
#128362 = CARTESIAN_POINT ( 'NONE',  ( 1.117730493923989599, 0.4056601665377962407, -2.030061024271647252 ) ) ;
#128363 = CARTESIAN_POINT ( 'NONE',  ( 5.412729640353754590, 7.337937218544611895, 1.599625672291267398 ) ) ;
#128364 = CARTESIAN_POINT ( 'NONE',  ( -4.757329562667670667E-14, -0.8906249996585621220, -1.570758158831818241 ) ) ;
#128365 = CARTESIAN_POINT ( 'NONE',  ( 4.160867320283115234, 0.5667376361006767338, 2.043264482828925033 ) ) ;
#128366 = CARTESIAN_POINT ( 'NONE',  ( 0.2406815423939384080, 0.3279693432677989184, 1.898232506199586167 ) ) ;
#128367 = ORIENTED_EDGE ( 'NONE', *, *, #119057, .T. ) ;
#128368 = CARTESIAN_POINT ( 'NONE',  ( -5.981082042284069367, 7.006959133200059142, 1.199719254218452935 ) ) ;
#128369 = CARTESIAN_POINT ( 'NONE',  ( 10.72180055030867329, 11.40318881831530540, 0.7998128361456341429 ) ) ;
#128370 = CARTESIAN_POINT ( 'NONE',  ( 4.855228407025239612, 8.678533884922511987, 0.000000000000000000 ) ) ;
#128371 = CARTESIAN_POINT ( 'NONE',  ( 3.475000000000000533, -1.152083332377417557, -2.006292185433951047 ) ) ;
#128372 = CARTESIAN_POINT ( 'NONE',  ( -3.906720819032141190, 7.709591388846142479, -0.7998128361456281477 ) ) ;
#128373 = CARTESIAN_POINT ( 'NONE',  ( 6.398696098476772676, -2.079943653215409416, -0.4123558718646391785 ) ) ;
#128374 = CARTESIAN_POINT ( 'NONE',  ( 1.202331507228219243, -2.106147100265920002, -0.0002331622408376087278 ) ) ;
#128375 = CARTESIAN_POINT ( 'NONE',  ( -3.969505113751027547, 7.853116076009993840, 1.214306433183764966E-14 ) ) ;
#128376 = CARTESIAN_POINT ( 'NONE',  ( 10.07778825365955733, 10.65184113889131012, -0.7998128361456281477 ) ) ;
#128377 = CARTESIAN_POINT ( 'NONE',  ( 5.102340918953698790, 1.855823733615385551, 0.1392438295388219172 ) ) ;
#128378 = CARTESIAN_POINT ( 'NONE',  ( 7.079328764629950754, 11.41096732537697633, 0.7998128361456462443 ) ) ;
#128379 =( BOUNDED_SURFACE ( )  B_SPLINE_SURFACE ( 1, 2, ( 
 ( #59609, #125765, #95344, #176568, #124701, #28178, #160314, #123646, #190660, #161394, #42321, #11918, #191727, #26032, #107364, #173385, #24968, #92144, #158198, #27101, #47657, #50823, #145170, #130030, #64930, #974, #146224, #163519, #67040, #79053, #214337, #182949, #149392, #81195, #181869, #196021, #164576, #98514, #148337, #82246, #32445, #49758, #194942, #16161, #65967, #212242, #199177, #132116, #113768, #178707, #166712, #34564, #162457, #112697, #115884, #198126, #179771, #211175, #62801, #33505, #133177, #116950, #46578, #48706, #31388, #15106, #165642, #99578, #100635, #17230, #147273, #83305, #128962, #30322, #14033, #96407, #197069, #80119, #63876, #97463, #213305, #131080, #114820, #180818, #37775, #3104, #68105, #69175, #104927, #101703, #138490, #185067, #87596, #18302, #122323, #84388, #36693, #102778, #168835, #120164, #88674, #55096, #153667, #136357, #106029, #134241, #20438, #54027, #52949, #86521, #184011, #200248, #103849, #135295, #150475, #201309, #152586, #186140, #2035, #72390, #70242, #21486, #202377, #119087, #51900, #169897, #121245, #118022, #19371, #203442, #4173, #204511, #35625, #5235, #71311, #154733, #85451, #137423, #6316, #167774, #187215, #188280, #56160, #38844, #170969, #22568, #39921, #151536, #26848, #175263, #125511, #142783, #73465, #109255, #158999, #24710, #77737, #10592, #140650, #57230, #45259, #61489, #40995, #205593, #208788, #76668, #58295, #172051, #89752, #191474, #27926, #160059, #139566, #141723, #206663, #42066, #44193, #60419, #193618, #126579, #108180, #43142, #11663, #143858, #107106, #192539, #75613, #110313, #7385, #124451, #123391, #92952, #25779, #207732, #176320, #156876, #189355, #8463, #94020, #173129, #209851, #190410, #127654, #23644, #155802, #90812, #174206, #91891, #157947, #59355, #74550, #9538, #147029, #113511, #115622, #161131, #63625, #179520, #96151, #79863, #144915, #95083, #163265, #30062, #111379, #162202, #195760, #31138, #12719, #214087, #97213, #65715, #13789, #114574, #32188, #148082, #145972, #128711, #211984, #129779, #131863, #80937, #194682, #14847, #213051, #28996, #210922, #197870, #46324, #178453, #78792, #47399, #98264, #112440, #49502, #64680, #130826, #177382, #62548, #196818, #48460, #180566, #164322, #15912, #81995, #127279, #159686, #208415, #178082, #206289, #92586, #126204, #125140, #108873, #41694, #140269, #175952, #207364, #90430, #58984, #10225, #192166, #74177, #144552, #142407, #210560, #141349, #193250, #44897, #12350, #174897, #173830, #26476, #158628, #62195, #27548, #91510, #43827, #109943, #156499, #107805, #194318, #157570, #93643, #60049, #191098, #57913, #11287, #111004, #124078, #9163, #61118, #42766, #128351, #8089, #76299, #77366, #78430, #75239, #143480, #45959, #190042, #209476, #112080, #160755, #177008, #28625, #94713, #25407, #49150, #98963, #32886, #197507, #341, #145620, #181259, #16609 ),
 ( #165014, #29699, #195396, #129413, #33945, #95781, #162899, #17672, #212683, #66414, #13426, #82690, #148772, #132559, #47026, #80570, #113141, #179148, #161838, #63252, #130468, #100020, #147715, #115267, #198559, #31834, #131503, #50207, #14481, #97909, #30772, #116325, #182316, #79502, #96851, #133627, #146669, #166084, #81630, #64324, #211616, #83758, #149850, #196458, #48101, #1419, #114213, #67482, #180211, #163969, #15545, #199629, #213733, #65356, #51275, #117399, #104294, #72836, #39283, #185518, #71755, #85904, #54472, #202823, #38221, #186594, #136798, #154108, #84832, #120616, #170342, #36071, #89123, #21927, #151978, #68558, #56608, #138940, #52339, #2482, #5677, #88036, #69622, #183396, #101073, #137871, #105378, #171417, #150921, #153037, #3552, #53395, #55536, #203891, #204960, #121690, #119532, #187657, #23005, #155177, #118467, #6761, #86968, #35001, #18747, #135732, #134685, #167160, #37142, #4611, #200688, #168219, #184453, #19819, #102153, #201754, #103224, #169283, #20869, #70685, #24026, #158326, #142098, #92281, #73862, #189734, #204898, #41386, #121631, #104238, #172439, #188675, #105318, #57616, #7771, #106416, #22950, #74931, #170284, #173524, #190792, #141041, #138880, #156195, #90128, #58679, #59740, #208111, #89064, #5619, #187600, #137813, #139956, #155122, #124827, #205981, #108561, #107497, #39227, #40308, #123774, #75993, #25098, #171356, #91199, #157259, #21872, #55477, #125898, #6704, #8851, #207048, #56551, #154052, #42454, #174589, #71701, #72781, #26164, #122712, #191857, #87978, #9919, #203832, #179898, #110694, #128041, #31521, #43518, #178843, #147402, #113903, #45645, #146355, #160441, #129102, #62934, #112827, #46714, #211309, #14161, #159374, #195074, #30454, #176694, #163654, #96540, #12047, #143175, #131207, #213428, #126967, #77046, #80256, #162587, #144247, #109641, #175644, #212367, #97595, #15236, #10973, #13111, #78117, #193996, #130157, #64009, #65051, #196149, #111762, #47789, #81323, #27230, #192925, #93338, #161526, #209168, #60806, #210239, #44581, #28307, #177768, #79188, #94403, #61876, #29384, #95478, #145303, #66100, #102901, #149523, #50956, #82377, #200377, #52025, #1109, #67170, #133305, #84513, #53076, #19500, #118151, #100760, #70368, #98647, #199310, #18438, #17359, #117080, #148468, #32570, #68239, #99704, #197195, #165776, #183079, #150602, #180948, #36820, #34691, #168960, #33631, #85576, #151665, #119211, #166842, #48834, #83443, #2162, #134373, #164704, #20564, #184135, #86647, #35759, #3237, #69302, #185195, #101833, #132242, #167902, #135415, #152715, #201436, #198250, #4297, #114948, #16292, #36, #49889, #116014, #182000, #188406, #171093, #186267, #89874, #24837, #37902, #137552, #107235, #105057, #108305, #202505, #187342, #122448, #58420, #203570, #6440, #124573, #136482, #57353, #25900, #206788, #138614, #90936, #38971, #7511 ) ),
 .UNSPECIFIED., .F., .F., .F. ) 
 B_SPLINE_SURFACE_WITH_KNOTS ( ( 2, 2 ),
 ( 3, 2, 2, 2, 2, 2, 2, 2, 2, 2, 2, 2, 2, 2, 2, 2, 2, 2, 2, 2, 2, 2, 2, 2, 2, 2, 2, 2, 2, 2, 2, 2, 2, 2, 2, 2, 2, 2, 2, 2, 2, 2, 2, 2, 2, 2, 2, 2, 2, 2, 2, 2, 2, 2, 2, 2, 2, 2, 2, 2, 2, 2, 2, 2, 2, 2, 2, 2, 2, 2, 2, 2, 2, 2, 2, 2, 2, 2, 2, 2, 2, 2, 2, 2, 2, 2, 2, 2, 2, 2, 2, 2, 2, 2, 2, 2, 2, 2, 2, 2, 2, 2, 2, 2, 2, 2, 2, 2, 2, 2, 2, 2, 2, 2, 2, 2, 2, 2, 2, 2, 2, 2, 2, 2, 2, 2, 2, 2, 2, 2, 2, 2, 2, 2, 2, 2, 2, 2, 2, 2, 2, 2, 2, 2, 2, 2, 2, 2, 2, 2, 2, 2, 2, 2, 2, 2, 2, 2, 2, 2, 2, 2, 2, 2, 2, 2, 2, 2, 3 ),
 ( 0.000000000000000000, 1.000000000000000000 ),
 ( 0.000000000000000000, 0.005952380952380952051, 0.01190476190476190410, 0.01785714285714285615, 0.02380952380952380820, 0.02976190476190476025, 0.03571428571428571230, 0.04166666666666666435, 0.04761904761904761640, 0.05357142857142856845, 0.05952380952380952051, 0.06547619047619047949, 0.07142857142857142461, 0.07738095238095238360, 0.08333333333333332871, 0.08928571428571428770, 0.09523809523809523281, 0.1011904761904761918, 0.1071428571428571369, 0.1130952380952380959, 0.1190476190476190410, 0.1250000000000000000, 0.1309523809523809590, 0.1369047619047619180, 0.1428571428571428492, 0.1488095238095238082, 0.1547619047619047672, 0.1607142857142857262, 0.1666666666666666574, 0.1726190476190476164, 0.1785714285714285754, 0.1845238095238095344, 0.1904761904761904656, 0.1964285714285714246, 0.2023809523809523836, 0.2083333333333333426, 0.2142857142857142738, 0.2202380952380952328, 0.2261904761904761918, 0.2321428571428571508, 0.2380952380952380820, 0.2440476190476190410, 0.2500000000000000000, 0.2559523809523809312, 0.2619047619047619180, 0.2678571428571428492, 0.2738095238095238360, 0.2797619047619047672, 0.2857142857142856984, 0.2916666666666666852, 0.2976190476190476164, 0.3035714285714285476, 0.3095238095238095344, 0.3154761904761904656, 0.3214285714285714524, 0.3273809523809523836, 0.3333333333333333148, 0.3392857142857143016, 0.3452380952380952328, 0.3511904761904761640, 0.3571428571428571508, 0.3630952380952380820, 0.3690476190476190688, 0.3750000000000000000, 0.3809523809523809312, 0.3869047619047619180, 0.3928571428571428492, 0.3988095238095238360, 0.4047619047619047672, 0.4107142857142856984, 0.4166666666666666852, 0.4226190476190476164, 0.4285714285714285476, 0.4345238095238095344, 0.4404761904761904656, 0.4464285714285714524, 0.4523809523809523836, 0.4583333333333333148, 0.4642857142857143016, 0.4702380952380952328, 0.4761904761904761640, 0.4821428571428571508, 0.4880952380952380820, 0.4940476190476190688, 0.5000000000000000000, 0.5059523809523809312, 0.5119047619047618625, 0.5178571428571429047, 0.5238095238095238360, 0.5297619047619047672, 0.5357142857142856984, 0.5416666666666666297, 0.5476190476190476719, 0.5535714285714286031, 0.5595238095238095344, 0.5654761904761904656, 0.5714285714285713969, 0.5773809523809523281, 0.5833333333333333703, 0.5892857142857143016, 0.5952380952380952328, 0.6011904761904761640, 0.6071428571428570953, 0.6130952380952381375, 0.6190476190476190688, 0.6250000000000000000, 0.6309523809523809312, 0.6369047619047618625, 0.6428571428571429047, 0.6488095238095238360, 0.6547619047619047672, 0.6607142857142856984, 0.6666666666666666297, 0.6726190476190476719, 0.6785714285714286031, 0.6845238095238095344, 0.6904761904761904656, 0.6964285714285713969, 0.7023809523809523281, 0.7083333333333333703, 0.7142857142857143016, 0.7202380952380952328, 0.7261904761904761640, 0.7321428571428570953, 0.7380952380952381375, 0.7440476190476190688, 0.7500000000000000000, 0.7559523809523809312, 0.7619047619047618625, 0.7678571428571429047, 0.7738095238095238360, 0.7797619047619047672, 0.7857142857142856984, 0.7916666666666666297, 0.7976190476190476719, 0.8035714285714286031, 0.8095238095238095344, 0.8154761904761904656, 0.8214285714285713969, 0.8273809523809523281, 0.8333333333333333703, 0.8392857142857143016, 0.8452380952380952328, 0.8511904761904761640, 0.8571428571428570953, 0.8630952380952381375, 0.8690476190476190688, 0.8750000000000000000, 0.8809523809523809312, 0.8869047619047618625, 0.8928571428571429047, 0.8988095238095238360, 0.9047619047619047672, 0.9107142857142856984, 0.9166666666666666297, 0.9226190476190476719, 0.9285714285714286031, 0.9345238095238095344, 0.9404761904761904656, 0.9464285714285713969, 0.9523809523809523281, 0.9583333333333333703, 0.9642857142857143016, 0.9702380952380952328, 0.9761904761904761640, 0.9821428571428570953, 0.9880952380952381375, 0.9940476190476190688, 1.000000000000000000 ),
 .UNSPECIFIED. ) 
 GEOMETRIC_REPRESENTATION_ITEM ( )  RATIONAL_B_SPLINE_SURFACE ( (
 ( 1.000000000000000000, 0.8660254037844387076, 1.000000000000000000, 0.8660254037844387076, 1.000000000000000000, 0.8660254037844387076, 1.000000000000000000, 0.8660254037844387076, 1.000000000000000000, 0.8660254037844387076, 1.000000000000000000, 0.8660254037844387076, 1.000000000000000000, 0.8660254037844387076, 1.000000000000000000, 0.8660254037844387076, 1.000000000000000000, 0.8660254037844387076, 1.000000000000000000, 0.8660254037844387076, 1.000000000000000000, 0.8660254037844387076, 1.000000000000000000, 0.8660254037844387076, 1.000000000000000000, 0.8660254037844387076, 1.000000000000000000, 0.8660254037844387076, 1.000000000000000000, 0.8660254037844387076, 1.000000000000000000, 0.8660254037844387076, 1.000000000000000000, 0.8660254037844387076, 1.000000000000000000, 0.8660254037844387076, 1.000000000000000000, 0.8660254037844387076, 1.000000000000000000, 0.8660254037844387076, 1.000000000000000000, 0.8660254037844387076, 1.000000000000000000, 0.8660254037844387076, 1.000000000000000000, 0.8660254037844387076, 1.000000000000000000, 0.8660254037844387076, 1.000000000000000000, 0.8660254037844387076, 1.000000000000000000, 0.8660254037844387076, 1.000000000000000000, 0.8660254037844387076, 1.000000000000000000, 0.8660254037844387076, 1.000000000000000000, 0.8660254037844387076, 1.000000000000000000, 0.8660254037844387076, 1.000000000000000000, 0.8660254037844387076, 1.000000000000000000, 0.8660254037844387076, 1.000000000000000000, 0.8660254037844387076, 1.000000000000000000, 0.8660254037844387076, 1.000000000000000000, 0.8660254037844387076, 1.000000000000000000, 0.8660254037844387076, 1.000000000000000000, 0.8660254037844387076, 1.000000000000000000, 0.8660254037844387076, 1.000000000000000000, 0.8660254037844387076, 1.000000000000000000, 0.8660254037844387076, 1.000000000000000000, 0.8660254037844387076, 1.000000000000000000, 0.8660254037844387076, 1.000000000000000000, 0.8660254037844387076, 1.000000000000000000, 0.8660254037844387076, 1.000000000000000000, 0.8660254037844387076, 1.000000000000000000, 0.8660254037844387076, 1.000000000000000000, 0.8660254037844387076, 1.000000000000000000, 0.8660254037844387076, 1.000000000000000000, 0.8660254037844387076, 1.000000000000000000, 0.8660254037844387076, 1.000000000000000000, 0.8660254037844387076, 1.000000000000000000, 0.8660254037844387076, 1.000000000000000000, 0.8660254037844387076, 1.000000000000000000, 0.8660254037844387076, 1.000000000000000000, 0.8660254037844387076, 1.000000000000000000, 0.8660254037844387076, 1.000000000000000000, 0.8660254037844387076, 1.000000000000000000, 0.8660254037844387076, 1.000000000000000000, 0.8660254037844387076, 1.000000000000000000, 0.8660254037844387076, 1.000000000000000000, 0.8660254037844387076, 1.000000000000000000, 0.8660254037844387076, 1.000000000000000000, 0.8660254037844387076, 1.000000000000000000, 0.8660254037844387076, 1.000000000000000000, 0.8660254037844387076, 1.000000000000000000, 0.8660254037844387076, 1.000000000000000000, 0.8660254037844387076, 1.000000000000000000, 0.8660254037844387076, 1.000000000000000000, 0.8660254037844387076, 1.000000000000000000, 0.8660254037844387076, 1.000000000000000000, 0.8660254037844387076, 1.000000000000000000, 0.8660254037844387076, 1.000000000000000000, 0.8660254037844387076, 1.000000000000000000, 0.8660254037844387076, 1.000000000000000000, 0.8660254037844387076, 1.000000000000000000, 0.8660254037844387076, 1.000000000000000000, 0.8660254037844387076, 1.000000000000000000, 0.8660254037844387076, 1.000000000000000000, 0.8660254037844387076, 1.000000000000000000, 0.8660254037844387076, 1.000000000000000000, 0.8660254037844387076, 1.000000000000000000, 0.8660254037844387076, 1.000000000000000000, 0.8660254037844387076, 1.000000000000000000, 0.8660254037844387076, 1.000000000000000000, 0.8660254037844387076, 1.000000000000000000, 0.8660254037844387076, 1.000000000000000000, 0.8660254037844387076, 1.000000000000000000, 0.8660254037844387076, 1.000000000000000000, 0.8660254037844387076, 1.000000000000000000, 0.8660254037844387076, 1.000000000000000000, 0.8660254037844387076, 1.000000000000000000, 0.8660254037844387076, 1.000000000000000000, 0.8660254037844387076, 1.000000000000000000, 0.8660254037844387076, 1.000000000000000000, 0.8660254037844387076, 1.000000000000000000, 0.8660254037844387076, 1.000000000000000000, 0.8660254037844387076, 1.000000000000000000, 0.8660254037844387076, 1.000000000000000000, 0.8660254037844387076, 1.000000000000000000, 0.8660254037844387076, 1.000000000000000000, 0.8660254037844387076, 1.000000000000000000, 0.8660254037844387076, 1.000000000000000000, 0.8660254037844387076, 1.000000000000000000, 0.8660254037844387076, 1.000000000000000000, 0.8660254037844387076, 1.000000000000000000, 0.8660254037844387076, 1.000000000000000000, 0.8660254037844387076, 1.000000000000000000, 0.8660254037844387076, 1.000000000000000000, 0.8660254037844387076, 1.000000000000000000, 0.8660254037844387076, 1.000000000000000000, 0.8660254037844387076, 1.000000000000000000, 0.8660254037844387076, 1.000000000000000000, 0.8660254037844387076, 1.000000000000000000, 0.8660254037844387076, 1.000000000000000000, 0.8660254037844387076, 1.000000000000000000, 0.8660254037844387076, 1.000000000000000000, 0.8660254037844387076, 1.000000000000000000, 0.8660254037844387076, 1.000000000000000000, 0.8660254037844387076, 1.000000000000000000, 0.8660254037844387076, 1.000000000000000000, 0.8660254037844387076, 1.000000000000000000, 0.8660254037844387076, 1.000000000000000000, 0.8660254037844387076, 1.000000000000000000, 0.8660254037844387076, 1.000000000000000000, 0.8660254037844387076, 1.000000000000000000, 0.8660254037844387076, 1.000000000000000000, 0.8660254037844387076, 1.000000000000000000, 0.8660254037844387076, 1.000000000000000000, 0.8660254037844387076, 1.000000000000000000, 0.8660254037844387076, 1.000000000000000000, 0.8660254037844387076, 1.000000000000000000, 0.8660254037844387076, 1.000000000000000000, 0.8660254037844387076, 1.000000000000000000, 0.8660254037844387076, 1.000000000000000000, 0.8660254037844387076, 1.000000000000000000, 0.8660254037844387076, 1.000000000000000000, 0.8660254037844387076, 1.000000000000000000, 0.8660254037844387076, 1.000000000000000000, 0.8660254037844387076, 1.000000000000000000, 0.8660254037844387076, 1.000000000000000000, 0.8660254037844387076, 1.000000000000000000, 0.8660254037844387076, 1.000000000000000000, 0.8660254037844387076, 1.000000000000000000, 0.8660254037844387076, 1.000000000000000000, 0.8660254037844387076, 1.000000000000000000, 0.8660254037844387076, 1.000000000000000000, 0.8660254037844387076, 1.000000000000000000, 0.8660254037844387076, 1.000000000000000000, 0.8660254037844387076, 1.000000000000000000, 0.8660254037844387076, 1.000000000000000000, 0.8660254037844387076, 1.000000000000000000, 0.8660254037844387076, 1.000000000000000000, 0.8660254037844387076, 1.000000000000000000, 0.8660254037844387076, 1.000000000000000000, 0.8660254037844387076, 1.000000000000000000, 0.8660254037844387076, 1.000000000000000000, 0.8660254037844387076, 1.000000000000000000, 0.8660254037844387076, 1.000000000000000000, 0.8660254037844387076, 1.000000000000000000, 0.8660254037844387076, 1.000000000000000000, 0.8660254037844387076, 1.000000000000000000, 0.8660254037844387076, 1.000000000000000000, 0.8660254037844387076, 1.000000000000000000, 0.8660254037844387076, 1.000000000000000000, 0.8660254037844387076, 1.000000000000000000, 0.8660254037844387076, 1.000000000000000000, 0.8660254037844387076, 1.000000000000000000, 0.8660254037844387076, 1.000000000000000000),
 ( 1.000000000000000000, 0.8660254037844387076, 1.000000000000000000, 0.8660254037844387076, 1.000000000000000000, 0.8660254037844387076, 1.000000000000000000, 0.8660254037844387076, 1.000000000000000000, 0.8660254037844387076, 1.000000000000000000, 0.8660254037844387076, 1.000000000000000000, 0.8660254037844387076, 1.000000000000000000, 0.8660254037844387076, 1.000000000000000000, 0.8660254037844387076, 1.000000000000000000, 0.8660254037844387076, 1.000000000000000000, 0.8660254037844387076, 1.000000000000000000, 0.8660254037844387076, 1.000000000000000000, 0.8660254037844387076, 1.000000000000000000, 0.8660254037844387076, 1.000000000000000000, 0.8660254037844387076, 1.000000000000000000, 0.8660254037844387076, 1.000000000000000000, 0.8660254037844387076, 1.000000000000000000, 0.8660254037844387076, 1.000000000000000000, 0.8660254037844387076, 1.000000000000000000, 0.8660254037844387076, 1.000000000000000000, 0.8660254037844387076, 1.000000000000000000, 0.8660254037844387076, 1.000000000000000000, 0.8660254037844387076, 1.000000000000000000, 0.8660254037844387076, 1.000000000000000000, 0.8660254037844387076, 1.000000000000000000, 0.8660254037844387076, 1.000000000000000000, 0.8660254037844387076, 1.000000000000000000, 0.8660254037844387076, 1.000000000000000000, 0.8660254037844387076, 1.000000000000000000, 0.8660254037844387076, 1.000000000000000000, 0.8660254037844387076, 1.000000000000000000, 0.8660254037844387076, 1.000000000000000000, 0.8660254037844387076, 1.000000000000000000, 0.8660254037844387076, 1.000000000000000000, 0.8660254037844387076, 1.000000000000000000, 0.8660254037844387076, 1.000000000000000000, 0.8660254037844387076, 1.000000000000000000, 0.8660254037844387076, 1.000000000000000000, 0.8660254037844387076, 1.000000000000000000, 0.8660254037844387076, 1.000000000000000000, 0.8660254037844387076, 1.000000000000000000, 0.8660254037844387076, 1.000000000000000000, 0.8660254037844387076, 1.000000000000000000, 0.8660254037844387076, 1.000000000000000000, 0.8660254037844387076, 1.000000000000000000, 0.8660254037844387076, 1.000000000000000000, 0.8660254037844387076, 1.000000000000000000, 0.8660254037844387076, 1.000000000000000000, 0.8660254037844387076, 1.000000000000000000, 0.8660254037844387076, 1.000000000000000000, 0.8660254037844387076, 1.000000000000000000, 0.8660254037844387076, 1.000000000000000000, 0.8660254037844387076, 1.000000000000000000, 0.8660254037844387076, 1.000000000000000000, 0.8660254037844387076, 1.000000000000000000, 0.8660254037844387076, 1.000000000000000000, 0.8660254037844387076, 1.000000000000000000, 0.8660254037844387076, 1.000000000000000000, 0.8660254037844387076, 1.000000000000000000, 0.8660254037844387076, 1.000000000000000000, 0.8660254037844387076, 1.000000000000000000, 0.8660254037844387076, 1.000000000000000000, 0.8660254037844387076, 1.000000000000000000, 0.8660254037844387076, 1.000000000000000000, 0.8660254037844387076, 1.000000000000000000, 0.8660254037844387076, 1.000000000000000000, 0.8660254037844387076, 1.000000000000000000, 0.8660254037844387076, 1.000000000000000000, 0.8660254037844387076, 1.000000000000000000, 0.8660254037844387076, 1.000000000000000000, 0.8660254037844387076, 1.000000000000000000, 0.8660254037844387076, 1.000000000000000000, 0.8660254037844387076, 1.000000000000000000, 0.8660254037844387076, 1.000000000000000000, 0.8660254037844387076, 1.000000000000000000, 0.8660254037844387076, 1.000000000000000000, 0.8660254037844387076, 1.000000000000000000, 0.8660254037844387076, 1.000000000000000000, 0.8660254037844387076, 1.000000000000000000, 0.8660254037844387076, 1.000000000000000000, 0.8660254037844387076, 1.000000000000000000, 0.8660254037844387076, 1.000000000000000000, 0.8660254037844387076, 1.000000000000000000, 0.8660254037844387076, 1.000000000000000000, 0.8660254037844387076, 1.000000000000000000, 0.8660254037844387076, 1.000000000000000000, 0.8660254037844387076, 1.000000000000000000, 0.8660254037844387076, 1.000000000000000000, 0.8660254037844387076, 1.000000000000000000, 0.8660254037844387076, 1.000000000000000000, 0.8660254037844387076, 1.000000000000000000, 0.8660254037844387076, 1.000000000000000000, 0.8660254037844387076, 1.000000000000000000, 0.8660254037844387076, 1.000000000000000000, 0.8660254037844387076, 1.000000000000000000, 0.8660254037844387076, 1.000000000000000000, 0.8660254037844387076, 1.000000000000000000, 0.8660254037844387076, 1.000000000000000000, 0.8660254037844387076, 1.000000000000000000, 0.8660254037844387076, 1.000000000000000000, 0.8660254037844387076, 1.000000000000000000, 0.8660254037844387076, 1.000000000000000000, 0.8660254037844387076, 1.000000000000000000, 0.8660254037844387076, 1.000000000000000000, 0.8660254037844387076, 1.000000000000000000, 0.8660254037844387076, 1.000000000000000000, 0.8660254037844387076, 1.000000000000000000, 0.8660254037844387076, 1.000000000000000000, 0.8660254037844387076, 1.000000000000000000, 0.8660254037844387076, 1.000000000000000000, 0.8660254037844387076, 1.000000000000000000, 0.8660254037844387076, 1.000000000000000000, 0.8660254037844387076, 1.000000000000000000, 0.8660254037844387076, 1.000000000000000000, 0.8660254037844387076, 1.000000000000000000, 0.8660254037844387076, 1.000000000000000000, 0.8660254037844387076, 1.000000000000000000, 0.8660254037844387076, 1.000000000000000000, 0.8660254037844387076, 1.000000000000000000, 0.8660254037844387076, 1.000000000000000000, 0.8660254037844387076, 1.000000000000000000, 0.8660254037844387076, 1.000000000000000000, 0.8660254037844387076, 1.000000000000000000, 0.8660254037844387076, 1.000000000000000000, 0.8660254037844387076, 1.000000000000000000, 0.8660254037844387076, 1.000000000000000000, 0.8660254037844387076, 1.000000000000000000, 0.8660254037844387076, 1.000000000000000000, 0.8660254037844387076, 1.000000000000000000, 0.8660254037844387076, 1.000000000000000000, 0.8660254037844387076, 1.000000000000000000, 0.8660254037844387076, 1.000000000000000000, 0.8660254037844387076, 1.000000000000000000, 0.8660254037844387076, 1.000000000000000000, 0.8660254037844387076, 1.000000000000000000, 0.8660254037844387076, 1.000000000000000000, 0.8660254037844387076, 1.000000000000000000, 0.8660254037844387076, 1.000000000000000000, 0.8660254037844387076, 1.000000000000000000, 0.8660254037844387076, 1.000000000000000000, 0.8660254037844387076, 1.000000000000000000, 0.8660254037844387076, 1.000000000000000000, 0.8660254037844387076, 1.000000000000000000, 0.8660254037844387076, 1.000000000000000000, 0.8660254037844387076, 1.000000000000000000, 0.8660254037844387076, 1.000000000000000000, 0.8660254037844387076, 1.000000000000000000, 0.8660254037844387076, 1.000000000000000000, 0.8660254037844387076, 1.000000000000000000, 0.8660254037844387076, 1.000000000000000000, 0.8660254037844387076, 1.000000000000000000, 0.8660254037844387076, 1.000000000000000000, 0.8660254037844387076, 1.000000000000000000, 0.8660254037844387076, 1.000000000000000000, 0.8660254037844387076, 1.000000000000000000, 0.8660254037844387076, 1.000000000000000000, 0.8660254037844387076, 1.000000000000000000, 0.8660254037844387076, 1.000000000000000000, 0.8660254037844387076, 1.000000000000000000, 0.8660254037844387076, 1.000000000000000000, 0.8660254037844387076, 1.000000000000000000, 0.8660254037844387076, 1.000000000000000000, 0.8660254037844387076, 1.000000000000000000, 0.8660254037844387076, 1.000000000000000000, 0.8660254037844387076, 1.000000000000000000, 0.8660254037844387076, 1.000000000000000000, 0.8660254037844387076, 1.000000000000000000, 0.8660254037844387076, 1.000000000000000000) ) ) 
 REPRESENTATION_ITEM ( '' )  SURFACE ( )  );
#128380 = CARTESIAN_POINT ( 'NONE',  ( -10.41468459643390254, 5.042717479376880974, -5.872073626459179962 ) ) ;
#128381 = CARTESIAN_POINT ( 'NONE',  ( -7.919371124158132602, 8.411890197705517380, -0.7216878364870338292 ) ) ;
#128382 = CARTESIAN_POINT ( 'NONE',  ( -8.175203439360366531, 12.48156174598837787, 1.040834085586084257E-14 ) ) ;
#128384 = CARTESIAN_POINT ( 'NONE',  ( 2.119516022818414669, 0.3384452847540948550, -1.932298432780136244 ) ) ;
#128383 = CARTESIAN_POINT ( 'NONE',  ( -7.206322340863467346, 8.366129804884193888, 1.199719254218450271 ) ) ;
#128386 = CARTESIAN_POINT ( 'NONE',  ( 0.6730137850648570952, -2.035850703004048246, -0.7271551459356735414 ) ) ;
#128385 = B_SPLINE_CURVE_WITH_KNOTS ( 'NONE', 3,
 ( #192274, #142514, #74290, #73195, #206404, #90552, #10331, #77474, #91630, #41811 ),
 .UNSPECIFIED., .F., .F.,
 ( 4, 1, 1, 1, 1, 1, 1, 4 ),
 ( 0.000000000000000000, 0.09272347919791326665, 0.1850049962306132278, 0.2567072177207115891, 0.3610482009861257779, 0.5209239196176974618, 0.7336689415868371533, 1.000000000000000000 ),
 .UNSPECIFIED. ) ;
#128388 = CARTESIAN_POINT ( 'NONE',  ( -6.082092046053040768, 6.030765914320626919, 0.4329532585971782033 ) ) ;
#128387 = CARTESIAN_POINT ( 'NONE',  ( -6.394605727500880299, 7.489403432619674561, -1.199719254218452047 ) ) ;
#128389 = CARTESIAN_POINT ( 'NONE',  ( -0.6823417656250246877, -0.1989583329919109023, 1.181850606188755259 ) ) ;
#128390 = CARTESIAN_POINT ( 'NONE',  ( 3.022450238936627009, 1.725798670860735351, -0.1664453034943418896 ) ) ;
#128391 = CARTESIAN_POINT ( 'NONE',  ( 1.833560160614732704, 1.721085009045751901, 0.2571270737643116533 ) ) ;
#128392 = CARTESIAN_POINT ( 'NONE',  ( 7.809133291791403586, 8.213003049952529722, -0.7216878364870257245 ) ) ;
#128393 = CARTESIAN_POINT ( 'NONE',  ( -11.77619280525687451, 4.711391180887883223, -4.977117663154129623 ) ) ;
#128394 = EDGE_CURVE ( 'NONE', #162142, #68781, #111835, .T. ) ;
#128395 = CARTESIAN_POINT ( 'NONE',  ( 1.212267286723569981, -1.587592435625035270, -1.242539042498117086 ) ) ;
#128396 = CARTESIAN_POINT ( 'NONE',  ( 6.925078400183548588, 2.417948008941684268, 2.525058136801380027 ) ) ;
#128397 = CARTESIAN_POINT ( 'NONE',  ( -3.284818356260900796, 7.054314858938165678, 0.7998128361456352531 ) ) ;
#128398 = CARTESIAN_POINT ( 'NONE',  ( 1.024223545076022424, 1.176019522272594875, -1.582147633265261977 ) ) ;
#128400 = CARTESIAN_POINT ( 'NONE',  ( -6.807602527837528505, 7.114826835331461652, 0.7216878364870317197 ) ) ;
#128399 = CARTESIAN_POINT ( 'NONE',  ( 5.449440537890920311, -1.726199344983204265, 0.8234401749890255529 ) ) ;
#128401 = CARTESIAN_POINT ( 'NONE',  ( -5.912764388891193157, 9.912325863766124456, 0.000000000000000000 ) ) ;
#128402 = CARTESIAN_POINT ( 'NONE',  ( 7.876360894896227371, 8.153785563659219804, -0.7998128361456341429 ) ) ;
#128403 = CARTESIAN_POINT ( 'NONE',  ( -5.596483547390937119, 9.751257581923240991, 0.000000000000000000 ) ) ;
#128404 = CARTESIAN_POINT ( 'NONE',  ( 1.735027068915934167, 1.885295237280168790, 0.7248928932378613244 ) ) ;
#128405 =( NAMED_UNIT ( * ) SI_UNIT ( $, .STERADIAN. ) SOLID_ANGLE_UNIT ( ) );
#128406 = CARTESIAN_POINT ( 'NONE',  ( 4.471882758057180496, 2.239461445850467580, -0.5561450820626266944 ) ) ;
#128407 = CARTESIAN_POINT ( 'NONE',  ( 5.898874287966751950, 0.3812104124719677412, 1.924297140916144233 ) ) ;
#128408 = EDGE_CURVE ( 'NONE', #101488, #137788, #15851, .T. ) ;
#128409 = CARTESIAN_POINT ( 'NONE',  ( 1.797631089865757259, -1.417250949620936895, -1.356651810197152086 ) ) ;
#128410 = CARTESIAN_POINT ( 'NONE',  ( 8.723781775389312543, 12.26516360700784958, -1.199719254218446718 ) ) ;
#128411 = CARTESIAN_POINT ( 'NONE',  ( -9.585855168520197367, 15.23438424536737656, 7.219146574778744885 ) ) ;
#128412 = ORIENTED_EDGE ( 'NONE', *, *, #111969, .F. ) ;
#128413 = CARTESIAN_POINT ( 'NONE',  ( 1.780608593570524034, -0.5699985197749558585, -2.039088110117696750 ) ) ;
#128415 = CARTESIAN_POINT ( 'NONE',  ( -7.344766530301162000, 9.591980256816594164, 1.599625672291295375 ) ) ;
#128414 = CARTESIAN_POINT ( 'NONE',  ( -5.298539104842322267, 5.076050465271134016, 0.7998128361456341429 ) ) ;
#128416 = CARTESIAN_POINT ( 'NONE',  ( 0.9020086522944226193, 1.395640307904035593, -1.200911154268270664 ) ) ;
#128417 = EDGE_LOOP ( 'NONE', ( #120116, #212261, #190614, #29841 ) ) ;
#128418 = CARTESIAN_POINT ( 'NONE',  ( 11.08203335251971744, 9.254633050982178588, 4.606539154764891286 ) ) ;
#128419 = CARTESIAN_POINT ( 'NONE',  ( 3.428091063814618700, -2.088597262255381448, 0.3661859999234198249 ) ) ;
#128420 = CARTESIAN_POINT ( 'NONE',  ( -1.500000000000013101, 3.910416667349482012, -0.8660254037844313801 ) ) ;
#128421 = CARTESIAN_POINT ( 'NONE',  ( 9.399880572976245574, 9.860948844760784482, 0.7998128361456462443 ) ) ;
#128422 = CARTESIAN_POINT ( 'NONE',  ( -1.225000000000050271, 2.583333334016200133, 0.7072540797572757221 ) ) ;
#128423 = CARTESIAN_POINT ( 'NONE',  ( 3.321608758505911307, -1.986990267296639745, 0.5463351552400242950 ) ) ;
#128425 = CARTESIAN_POINT ( 'NONE',  ( 0.6437974683802077935, 0.5340323341261629109, 1.762076181610471526 ) ) ;
#128424 = CARTESIAN_POINT ( 'NONE',  ( -6.991200766141138168, 11.30815132714001159, 0.7998128361456481317 ) ) ;
#128426 = CARTESIAN_POINT ( 'NONE',  ( -0.6823417656249969321, 3.967708333674754950, -1.181850606188749264 ) ) ;
#128427 = CARTESIAN_POINT ( 'NONE',  ( -3.474999999999997868, -2.770833333333333037, 2.006292185433951047 ) ) ;
#128428 = CARTESIAN_POINT ( 'NONE',  ( 1.494964465105833584, 4.335022008103392110, -0.1399972980471321238 ) ) ;
#128429 =( BOUNDED_CURVE ( )  B_SPLINE_CURVE ( 2, ( #125457, #191419, #43086, #175211, #77682, #193568, #144866, #13739, #30013 ),
 .UNSPECIFIED., .F., .T. ) 
 B_SPLINE_CURVE_WITH_KNOTS ( ( 3, 2, 2, 2, 3 ),
 ( 0.9196428571428570953, 0.9226190476190476719, 0.9285714285714286031, 0.9345238095238095344, 0.9375000000000000000 ),
 .UNSPECIFIED. ) 
 CURVE ( )  GEOMETRIC_REPRESENTATION_ITEM ( )  RATIONAL_B_SPLINE_CURVE ( ( 0.9330127018922194093, 0.9330127018922180770, 1.000000000000000000, 0.8660254037844387076, 1.000000000000000000, 0.8660254037844387076, 1.000000000000000000, 0.9330127018922194093, 0.9330127018922194093 ) ) 
 REPRESENTATION_ITEM ( '' )  );
#128430 = CARTESIAN_POINT ( 'NONE',  ( -5.111060722227552588, 6.025620933095978238, 1.082531754730546636 ) ) ;
#128431 = CARTESIAN_POINT ( 'NONE',  ( 2.689068300184436655, -0.3842959826076980390, -2.229375072012912629 ) ) ;
#128432 = CARTESIAN_POINT ( 'NONE',  ( -9.680158490477310806, 10.39586578175276266, 0.7216878364870438212 ) ) ;
#128433 = CARTESIAN_POINT ( 'NONE',  ( 2.478518767674630308, -1.246658584539367176, 1.314663817856591699 ) ) ;
#128434 = CARTESIAN_POINT ( 'NONE',  ( 3.503066848181853654, -0.1354201214893405170, 1.910964455010273344 ) ) ;
#128435 = CARTESIAN_POINT ( 'NONE',  ( 4.264170421968140445, -2.065031762457261610, 0.1491743435546449281 ) ) ;
#128436 = CARTESIAN_POINT ( 'NONE',  ( 0.6823417656249882723, 2.238541667008084435, -1.181850606188749264 ) ) ;
#128437 = CIRCLE ( 'NONE', #159574, 11.99999999999999112 ) ;
#128438 = CARTESIAN_POINT ( 'NONE',  ( 1.938291742056476030, 1.949724373066508143, 0.2912656003557292927 ) ) ;
#128439 = CARTESIAN_POINT ( 'NONE',  ( 0.4637318561061140043, 1.905900585730261110, -0.2794304195078872732 ) ) ;
#128440 = CARTESIAN_POINT ( 'NONE',  ( 2.641296366799699147, -1.384790685969448099, -1.257831364775918503 ) ) ;
#128442 = CARTESIAN_POINT ( 'NONE',  ( 4.868750418105482147, 8.172599172502351905, -0.9747704861028365642 ) ) ;
#128441 = CARTESIAN_POINT ( 'NONE',  ( 0.9971819109757291688, -0.5654680449962052879, -2.237236815885994989 ) ) ;
#128443 = CARTESIAN_POINT ( 'NONE',  ( 2.857670863715315424, -0.5868061553097079219, 1.766171933019081042 ) ) ;
#128444 = CARTESIAN_POINT ( 'NONE',  ( -1.364683531250012516, 3.530208333674758059, 0.7879004041258379498 ) ) ;
#128445 = CARTESIAN_POINT ( 'NONE',  ( 6.812941044521420686, -1.596950470092706853, 1.305146078352089845 ) ) ;
#128446 = CARTESIAN_POINT ( 'NONE',  ( -4.466521540698216164, 7.298359999868178960, -1.199719254218452047 ) ) ;
#128447 = CARTESIAN_POINT ( 'NONE',  ( -1.412038856124949504, 3.476454961006842037, -0.5099368981155086855 ) ) ;
#128448 = CARTESIAN_POINT ( 'NONE',  ( 6.827182134110199030, -0.004087946457608306570, 2.088967824442849341 ) ) ;
#128449 = CARTESIAN_POINT ( 'NONE',  ( -1.201851678989727383E-14, 3.759375000341422801, -1.575800808251660134 ) ) ;
#128450 = CARTESIAN_POINT ( 'NONE',  ( 6.134075720976177593, 1.071308383804179476, -1.877395391766012445 ) ) ;
#128451 = CARTESIAN_POINT ( 'NONE',  ( 0.03542360567958083295, -0.09470281839311225913, 2.017672626582614814 ) ) ;
#128452 = CARTESIAN_POINT ( 'NONE',  ( 0.6823417656249882723, -0.1572916663252488245, 1.181850606188755259 ) ) ;
#128453 = CARTESIAN_POINT ( 'NONE',  ( -5.775410249741523394, 5.840326167560965231, 0.7216878364870317197 ) ) ;
#128454 = EDGE_CURVE ( 'NONE', #88263, #114098, #187809, .T. ) ;
#128457 = CARTESIAN_POINT ( 'NONE',  ( 5.856759171423504107, 5.935233242856626568, -0.7216878364870257245 ) ) ;
#128456 = CARTESIAN_POINT ( 'NONE',  ( 6.825078400183554272, 2.980425674467934272, 2.309322343017068402 ) ) ;
#128455 = CARTESIAN_POINT ( 'NONE',  ( 4.688087255275310561, 8.691461907788344377, -0.7998128361456381397 ) ) ;
#128458 = CARTESIAN_POINT ( 'NONE',  ( -4.817943484809863008, 6.714296380401858499, 1.599625672291263179 ) ) ;
#128459 = CARTESIAN_POINT ( 'NONE',  ( 5.155482549980198392, 1.942097955248718533, -0.5424665614216088727 ) ) ;
#128460 = CARTESIAN_POINT ( 'NONE',  ( -8.525379664894808585, 8.840697785332414682, -0.7998128361456291469 ) ) ;
#128462 = CARTESIAN_POINT ( 'NONE',  ( -5.750066545527201534, 9.722511713174800008, 0.000000000000000000 ) ) ;
#128461 = CARTESIAN_POINT ( 'NONE',  ( -10.14113571334194930, 10.93367254176152059, -0.7216878364870267237 ) ) ;
#128463 = CARTESIAN_POINT ( 'NONE',  ( 1.364683531249990311, 4.634375000341417916, 1.214306433183764966E-14 ) ) ;
#128465 = CARTESIAN_POINT ( 'NONE',  ( 1.364683531250000748, 8.755208333674731946, -0.7879004041258355073 ) ) ;
#128464 = CARTESIAN_POINT ( 'NONE',  ( 5.928642344448160628, 2.082074431819755045, 0.5810635428650026135 ) ) ;
#128466 = CARTESIAN_POINT ( 'NONE',  ( 11.33772463945036790, 10.90000000000000036, -3.600000000000002309 ) ) ;
#128467 = CARTESIAN_POINT ( 'NONE',  ( -11.86286653539476177, 7.770451347058147995, 1.827103009650931753 ) ) ;
#128469 = CARTESIAN_POINT ( 'NONE',  ( 6.345327396762703742, 0.3419173589993273477, -1.987050850726256979 ) ) ;
#128468 = CARTESIAN_POINT ( 'NONE',  ( -6.873620692004104527, 7.121571683533994168, 0.7216878364870317197 ) ) ;
#128470 = CARTESIAN_POINT ( 'NONE',  ( -1.364683531250014514, -0.4489583329919089039, -0.7879004041258359514 ) ) ;
#128471 = DIRECTION ( 'NONE',  ( 0.000000000000000000, 1.000000000000000000, 0.000000000000000000 ) ) ;
#128472 = CARTESIAN_POINT ( 'NONE',  ( 1.769703478646069028, 0.8846387809394311574, 1.480598516496567152 ) ) ;
#128473 = CARTESIAN_POINT ( 'NONE',  ( 7.693325821111733021, 7.940244644243982464, -0.7998128361456341429 ) ) ;
#128474 = CARTESIAN_POINT ( 'NONE',  ( 4.369470645354133431, 8.319742529546998000, 0.7998128361456271485 ) ) ;
#128475 = CARTESIAN_POINT ( 'NONE',  ( -11.06911165594924462, 7.103609171308002956, -4.638933421456848727 ) ) ;
#128476 = CARTESIAN_POINT ( 'NONE',  ( 6.309813054293936574, -1.856383540575656799, 0.2289572138471432372 ) ) ;
#128477 = CARTESIAN_POINT ( 'NONE',  ( 4.637309883081485395, 8.320457421531981979, 0.4059539251603030974 ) ) ;
#128478 = CARTESIAN_POINT ( 'NONE',  ( 1.067042177248921364, -1.585704042599777264, 1.240073755948613243 ) ) ;
#128479 = CARTESIAN_POINT ( 'NONE',  ( 3.522699392456357881, 1.401646575410384843, -1.704459333586107794 ) ) ;
#128480 = CARTESIAN_POINT ( 'NONE',  ( 5.946172770594575496, -0.9833217254726284162, 1.935730195829394429 ) ) ;
#128481 = ORIENTED_EDGE ( 'NONE', *, *, #21723, .F. ) ;
#128482 = CARTESIAN_POINT ( 'NONE',  ( -1.500000000000001332, -0.3499999999999753308, 0.000000000000000000 ) ) ;
#128484 = CARTESIAN_POINT ( 'NONE',  ( 9.585251414737269826, 11.24551007435741568, -1.082531754730537088 ) ) ;
#128483 = AXIS2_PLACEMENT_3D ( 'NONE', #59875, #93472, #191988 ) ;
#128486 = CARTESIAN_POINT ( 'NONE',  ( 2.935172905452135161, -1.650095542580119812, -1.158671029019647358 ) ) ;
#128485 = CARTESIAN_POINT ( 'NONE',  ( 2.789816089392273213, 2.012775272720100705, -0.6673941125509493810 ) ) ;
#128488 = ORIENTED_EDGE ( 'NONE', *, *, #103113, .F. ) ;
#128487 = CARTESIAN_POINT ( 'NONE',  ( 2.689504281738527514, 1.718874962283756691, -0.5722189708131807384 ) ) ;
#128489 = CARTESIAN_POINT ( 'NONE',  ( 5.742760583840166966, 8.857581893525663830, 1.199719254218452047 ) ) ;
#128490 = ORIENTED_EDGE ( 'NONE', *, *, #105724, .T. ) ;
#128491 = CARTESIAN_POINT ( 'NONE',  ( 0.08069323953814251660, -0.1329233695197447052, -1.840450602299897431 ) ) ;
#128492 = CARTESIAN_POINT ( 'NONE',  ( 5.289652487626049115, 9.323011668872403845, 0.7998128361456462443 ) ) ;
#128494 = CARTESIAN_POINT ( 'NONE',  ( 1.217839795352684273, 0.9409426854420616104, -1.668592810110066438 ) ) ;
#128493 = CARTESIAN_POINT ( 'NONE',  ( -5.251085567194491155, 5.020688004682002159, -0.7998128361456221525 ) ) ;
#128495 = CARTESIAN_POINT ( 'NONE',  ( -2.659371061294795613, 0.4155010417826092151, -0.1333820918543257572 ) ) ;
#128496 = CARTESIAN_POINT ( 'NONE',  ( 1.499999999999822586, 7.360382131182487520, 4.205521753552998732 ) ) ;
#128497 = CARTESIAN_POINT ( 'NONE',  ( -1.402160292154681736E-14, 2.259375000341416140, -1.575800808251660134 ) ) ;
#128498 = DIRECTION ( 'NONE',  ( 0.000000000000000000, 0.000000000000000000, 1.000000000000000000 ) ) ;
#128499 = CARTESIAN_POINT ( 'NONE',  ( -7.960608749518247151, 12.43912730774665576, 0.000000000000000000 ) ) ;
#128500 = EDGE_CURVE ( 'NONE', #53115, #39641, #118791, .T. ) ;
#128501 = CARTESIAN_POINT ( 'NONE',  ( 4.909125497034264818, 1.879091090907711425, 1.068517025386829467 ) ) ;
#128502 = CARTESIAN_POINT ( 'NONE',  ( -5.695833931516914639, 6.778132687258748845, 1.082531754730549078 ) ) ;
#128503 = CARTESIAN_POINT ( 'NONE',  ( -7.584860592202423035, 7.813701877183096833, -0.7998128361456362523 ) ) ;
#128504 = CARTESIAN_POINT ( 'NONE',  ( 3.392942708002244068, -2.044739723715986113, -0.5619712599038150236 ) ) ;
#128506 = CARTESIAN_POINT ( 'NONE',  ( -11.33523815116046229, 5.279172990141937305, 5.677742996778201601 ) ) ;
#128505 = CARTESIAN_POINT ( 'NONE',  ( -0.1296875068448125057, 2.889142263448498227, -2.315371602238533555 ) ) ;
#128507 = CARTESIAN_POINT ( 'NONE',  ( 4.675049781410951510, 0.003005680196035282782, -1.971530341645504780 ) ) ;
#128508 = ORIENTED_EDGE ( 'NONE', *, *, #200438, .T. ) ;
#128510 = EDGE_CURVE ( 'NONE', #123166, #211245, #44267, .T. ) ;
#128509 = PRESENTATION_STYLE_ASSIGNMENT (( #213893 ) ) ;
#128511 = CARTESIAN_POINT ( 'NONE',  ( 0.8364851226981102617, -1.151554295457988930, 1.720357586142134076 ) ) ;
#128512 = CARTESIAN_POINT ( 'NONE',  ( 2.800647771853786772, 1.640754720439155268, 1.038516083699735582 ) ) ;
#128513 = ORIENTED_EDGE ( 'NONE', *, *, #200040, .T. ) ;
#128514 = CARTESIAN_POINT ( 'NONE',  ( -4.442231607132987925, 5.211633625523774960, -1.199719254218453823 ) ) ;
#128515 = CARTESIAN_POINT ( 'NONE',  ( 6.550524494058025837, 7.671308660269694712, -1.199719254218452047 ) ) ;
#128517 = CARTESIAN_POINT ( 'NONE',  ( 6.440286661691305703, 7.472421512516709718, 1.199719254218462483 ) ) ;
#128516 = CARTESIAN_POINT ( 'NONE',  ( 2.976600611693449139, -0.1542612496043833104, -2.085005227243463821 ) ) ;
#128518 = CARTESIAN_POINT ( 'NONE',  ( 3.377389663135653031, 6.954388683717978026, -0.7216878364870338292 ) ) ;
#128520 = ORIENTED_EDGE ( 'NONE', *, *, #103265, .F. ) ;
#128519 = CARTESIAN_POINT ( 'NONE',  ( 0.8557779741884026237, 0.7350315055517571139, -1.655818919202347361 ) ) ;
#128521 = CARTESIAN_POINT ( 'NONE',  ( 4.196070124731249074, -0.8457972711899945928, 2.038567251995755836 ) ) ;
#128522 = CARTESIAN_POINT ( 'NONE',  ( 2.678998284833411070, -2.111460168698295004, -0.6414983429729387288 ) ) ;
#128523 = CARTESIAN_POINT ( 'NONE',  ( 6.747154001095143627, 11.02343010125301959, -0.7998128361456291469 ) ) ;
#128524 = CYLINDRICAL_SURFACE ( 'NONE', #51312, 1.250000000000000000 ) ;
#128525 = CARTESIAN_POINT ( 'NONE',  ( 2.297387027313551044, 1.747684631587187454, -0.7765785915121098393 ) ) ;
#128526 = CARTESIAN_POINT ( 'NONE',  ( 11.52483635780546933, 13.87999991357535201, -3.345866325258015639 ) ) ;
#128527 = CARTESIAN_POINT ( 'NONE',  ( 4.316890830952234914, -1.536253448065309613, 1.388129241271539138 ) ) ;
#128529 = CARTESIAN_POINT ( 'NONE',  ( 2.922914210685311431, 2.035003303901411265, 0.7295308445595325431 ) ) ;
#128528 = CARTESIAN_POINT ( 'NONE',  ( -4.302014814237876017, 3.913438792899272212, 0.7998128361456341429 ) ) ;
#128530 = CARTESIAN_POINT ( 'NONE',  ( 4.441096743985088580, -1.694418930461354611, -1.389946530008886905 ) ) ;
#128531 = DIRECTION ( 'NONE',  ( -3.347138415753903010E-16, -0.6000000000000018652, 0.7999999999999984901 ) ) ;
#128532 = DIRECTION ( 'NONE',  ( 1.224646799147353207E-16, 1.000000000000000000, -0.000000000000000000 ) ) ;
#128533 = CARTESIAN_POINT ( 'NONE',  ( -0.1447443628656817916, 7.100480071729094789, 2.114679381859663199 ) ) ;
#128534 = CARTESIAN_POINT ( 'NONE',  ( 6.574778147984297938, 6.635272358928617997, -0.7998128361456481317 ) ) ;
#128535 = CARTESIAN_POINT ( 'NONE',  ( 1.642778471875001811, -2.880208332855377584, 2.845375778867859751 ) ) ;
#128536 = CARTESIAN_POINT ( 'NONE',  ( -4.305596300791617814, 7.180890229968955651, 1.199719254218452935 ) ) ;
#128537 = CARTESIAN_POINT ( 'NONE',  ( 0.3170300144729014669, 1.034162889623980286, -1.730867746391979933 ) ) ;
#128539 = EDGE_CURVE ( 'NONE', #135745, #63949, #152834, .T. ) ;
#128538 = CIRCLE ( 'NONE', #156144, 0.07999999999999977962 ) ;
#128540 = CARTESIAN_POINT ( 'NONE',  ( -9.164948653158003111, 9.794787638213568570, -0.7216878364870267237 ) ) ;
#128541 = CARTESIAN_POINT ( 'NONE',  ( 4.979381509686323426, -0.1069728651886258930, 2.067640925720988232 ) ) ;
#128542 = CARTESIAN_POINT ( 'NONE',  ( 2.947785801820240970, 0.6929415146892035082, -1.797737524126517217 ) ) ;
#128543 = CARTESIAN_POINT ( 'NONE',  ( 6.099228927766127129, -0.2589519472634767006, 2.101251757753983984 ) ) ;
#128544 = CARTESIAN_POINT ( 'NONE',  ( 3.825371897350130723, 7.614684313550482031, 0.7998128361456321445 ) ) ;
#128545 = CARTESIAN_POINT ( 'NONE',  ( -1.001543065824772872E-14, 5.571875000341416140, 1.575800808251672791 ) ) ;
#128546 = CARTESIAN_POINT ( 'NONE',  ( 3.485164662121999601, 0.04367138265829079852, 1.969119211374547707 ) ) ;
#128547 = CARTESIAN_POINT ( 'NONE',  ( 6.228533256425053288, 0.2185279184554402288, 2.281841813635554495 ) ) ;
#128548 = CARTESIAN_POINT ( 'NONE',  ( 4.424309136736732206, 1.121156565774838354, -1.440799707636587712 ) ) ;
#128549 = PRODUCT_DEFINITION_SHAPE ( 'NONE', 'NONE',  #103356 ) ;
#128550 = CARTESIAN_POINT ( 'NONE',  ( 6.034787771858531435, 10.05468647722803865, 0.000000000000000000 ) ) ;
#128551 = CARTESIAN_POINT ( 'NONE',  ( 4.324687812634897988, 4.147816657603229373, 0.7216878364870317197 ) ) ;
#128552 = CARTESIAN_POINT ( 'NONE',  ( -6.038177310039794854, 8.137902509836795417, -1.599625672291271394 ) ) ;
#128553 = CARTESIAN_POINT ( 'NONE',  ( 4.505052181490820651, 8.477920988373101707, -0.7998128361456381397 ) ) ;
#128554 = EDGE_LOOP ( 'NONE', ( #91829, #187394, #116021, #177469 ) ) ;
#128556 = CARTESIAN_POINT ( 'NONE',  ( 5.519794446587845016, -0.4848760706452569513, 1.953846845731139759 ) ) ;
#128555 = CARTESIAN_POINT ( 'NONE',  ( 1.979791773625012352, -1.805961398883266344, -0.3578489297004632808 ) ) ;
#128557 = CARTESIAN_POINT ( 'NONE',  ( 0.3339538366646053191, -1.498446967350696379, 1.742810101306817794 ) ) ;
#128558 = CARTESIAN_POINT ( 'NONE',  ( 6.034033239799157400, 1.165729394902741189, 1.577711426528668692 ) ) ;
#128559 = CARTESIAN_POINT ( 'NONE',  ( -5.018489415352746619, 9.006654751220198207, 0.7998128361456481317 ) ) ;
#128560 = DIRECTION ( 'NONE',  ( -1.000000000000000000, 7.771561172376094797E-16, -3.330669073875481454E-16 ) ) ;
#128561 = CARTESIAN_POINT ( 'NONE',  ( -3.750802052474980108, 7.527686161196117887, 1.040834085586084257E-14 ) ) ;
#128562 = DIRECTION ( 'NONE',  ( 6.217248937900876626E-15, 0.000000000000000000, 1.000000000000000000 ) ) ;
#128563 = CARTESIAN_POINT ( 'NONE',  ( -4.339491684825780737, 7.220434844675483355, -1.199719254218455378 ) ) ;
#128565 = CARTESIAN_POINT ( 'NONE',  ( 0.1275333129481092398, -1.147091320445620566, -1.478225367208672703 ) ) ;
#128564 = CARTESIAN_POINT ( 'NONE',  ( 2.050439074220523406, -1.614099552242785895, 1.328842424969446823 ) ) ;
#128566 = CARTESIAN_POINT ( 'NONE',  ( -0.003079562120915812617, 7.078201604703583172, 2.121336893758693609 ) ) ;
#128567 = CARTESIAN_POINT ( 'NONE',  ( 1.364683531249988535, 3.467708333674749621, -0.7879004041258239610 ) ) ;
#128568 = CARTESIAN_POINT ( 'NONE',  ( 1.294060738426667134, 1.423250580516822072, -1.001416416642088469 ) ) ;
#128569 = AXIS2_PLACEMENT_3D ( 'NONE', #90320, #74064, #39425 ) ;
#128570 = CARTESIAN_POINT ( 'NONE',  ( 7.070740804726770357, 8.207951346058097286, 1.199719254218462483 ) ) ;
#128572 = CARTESIAN_POINT ( 'NONE',  ( 1.547033095191288954, 8.694673270357780481, 2.507079848779477871 ) ) ;
#128571 = FILL_AREA_STYLE ('',( #208640 ) ) ;
#128573 = CARTESIAN_POINT ( 'NONE',  ( 2.209205535023693212, -0.3792257637574465434, 1.682495413129220907 ) ) ;
#128574 = CARTESIAN_POINT ( 'NONE',  ( 1.435386855117400717, -1.590506285900999295, -1.507976327226906443 ) ) ;
#128575 = CARTESIAN_POINT ( 'NONE',  ( 4.494872972331320327, -0.4818267175418550208, -2.153482813429814069 ) ) ;
#128576 = CARTESIAN_POINT ( 'NONE',  ( -10.83049189199067719, 4.361170120774730208, -4.636001201543571426 ) ) ;
#128577 = CARTESIAN_POINT ( 'NONE',  ( 0.8663802385432646247, -2.160743160283730813, 0.2111063225179575509 ) ) ;
#128578 = CARTESIAN_POINT ( 'NONE',  ( 0.06470675514189982991, -1.629034059718449834, -0.8243793580787887043 ) ) ;
#128579 = CARTESIAN_POINT ( 'NONE',  ( 3.221969581791602977, 0.9480887764680032692, -1.893252576601434756 ) ) ;
#128580 = CARTESIAN_POINT ( 'NONE',  ( 6.539320575229234933, 1.301352213286063320, 1.914891792149053140 ) ) ;
#128581 = ORIENTED_EDGE ( 'NONE', *, *, #55578, .F. ) ;
#128583 = CARTESIAN_POINT ( 'NONE',  ( 0.6823417656249864960, -0.5114583329919111243, -1.181850606188749264 ) ) ;
#128582 = CARTESIAN_POINT ( 'NONE',  ( 4.036908492867667064, -1.994400080153370558, 1.130107982421886481 ) ) ;
#128584 = CARTESIAN_POINT ( 'NONE',  ( 3.708318708537623021, 4.285125567170706695, -1.199719254218446718 ) ) ;
#128585 = CARTESIAN_POINT ( 'NONE',  ( 3.357615597678655917, 7.068968630600412695, 0.7998128361456321445 ) ) ;
#128586 = VECTOR ( 'NONE', #9568, 1000.000000000000000 ) ;
#128587 = CARTESIAN_POINT ( 'NONE',  ( 5.742908703533418091, 2.140221812536883927, 0.5945068574613203705 ) ) ;
#128588 = CARTESIAN_POINT ( 'NONE',  ( -5.721177635286839092, 9.618531641235897212, 0.7216878364870458196 ) ) ;
#128589 = CARTESIAN_POINT ( 'NONE',  ( 5.070386261830877928, 5.978167395966564435, -1.082531754730548412 ) ) ;
#128590 = CARTESIAN_POINT ( 'NONE',  ( -8.473482818416682605, 8.988077497682020578, -0.7216878364870267237 ) ) ;
#128591 = CARTESIAN_POINT ( 'NONE',  ( 5.912764389335563919, 6.070849007079172743, -0.7216878364870458196 ) ) ;
#128592 = ORIENTED_EDGE ( 'NONE', *, *, #41997, .T. ) ;
#128593 = CARTESIAN_POINT ( 'NONE',  ( 4.289685514112329123, 1.556909497225898109, -1.281360267751927129 ) ) ;
#128595 = CARTESIAN_POINT ( 'NONE',  ( 1.903259321421392425, -1.744647275545135212, 1.099889041785537813 ) ) ;
#128594 = CARTESIAN_POINT ( 'NONE',  ( 5.636439174979242850, 7.598931675607687453, -1.599625672291262513 ) ) ;
#128596 = LINE ( 'NONE', #164205, #116474 ) ;
#128597 = CARTESIAN_POINT ( 'NONE',  ( 4.163762572728282763, 6.911454530608037494, -1.082531754730548412 ) ) ;
#128598 = CARTESIAN_POINT ( 'NONE',  ( -9.605391220871888791, -6.900199406649615952, 0.04765083308772638526 ) ) ;
#128599 = CARTESIAN_POINT ( 'NONE',  ( 1.364683531249992088, 5.384375000341417916, 1.214306433183764966E-14 ) ) ;
#128600 = CARTESIAN_POINT ( 'NONE',  ( 4.839868765920234850, 2.185429510258177110, 0.1630863781024796955 ) ) ;
#128601 = CARTESIAN_POINT ( 'NONE',  ( 2.760388869050140137, 1.913803604375517109, -0.6351994527180188088 ) ) ;
#128602 = CARTESIAN_POINT ( 'NONE',  ( 1.839159199666509981, 0.7036077657225293658, -1.701706503975081830 ) ) ;
#128603 = CARTESIAN_POINT ( 'NONE',  ( 8.932124273304774320, 9.315233161810734686, 0.7998128361456462443 ) ) ;
#128604 = SURFACE_STYLE_FILL_AREA ( #129669 ) ;
#128605 = CARTESIAN_POINT ( 'NONE',  ( 5.666980381186065507, -1.651371415153819688, -0.7785968546244539379 ) ) ;
#128606 = CARTESIAN_POINT ( 'NONE',  ( 6.346327303948391396, 0.3419391630616851474, -1.987045965717588958 ) ) ;
#128607 = CARTESIAN_POINT ( 'NONE',  ( -6.353967546298838087, 10.56471257065732416, 0.000000000000000000 ) ) ;
#128609 = CARTESIAN_POINT ( 'NONE',  ( -5.607179047703544583, 8.699403434699558346, 1.199719254218454489 ) ) ;
#128608 = CARTESIAN_POINT ( 'NONE',  ( 6.104402428500737443, -0.8075561382203682026, -2.113670588390024196 ) ) ;
#128610 = CARTESIAN_POINT ( 'NONE',  ( 0.5750072486576313091, -1.983761410860336527, -0.7076436626956124076 ) ) ;
#128611 = CARTESIAN_POINT ( 'NONE',  ( -8.100070429521727178, 8.414780020722290033, 0.7998128361456341429 ) ) ;
#128612 = CARTESIAN_POINT ( 'NONE',  ( 8.239604668803105270, 10.63595808506888396, -1.599625672291268286 ) ) ;
#128613 = CARTESIAN_POINT ( 'NONE',  ( -0.6801582343750108839, 2.880208333674722176, -1.178068619123848526 ) ) ;
#128614 = DIRECTION ( 'NONE',  ( 0.7399106458895119420, -0.4377907168496474322, -0.5107558363245954247 ) ) ;
#128615 = CARTESIAN_POINT ( 'NONE',  ( -7.283754839039664475, 9.520799950344851936, -1.599625672291263179 ) ) ;
#128616 = B_SPLINE_CURVE_WITH_KNOTS ( 'NONE', 3,
 ( #156548, #105683, #70984, #136027, #137097, #186887 ),
 .UNSPECIFIED., .F., .F.,
 ( 4, 2, 4 ),
 ( 0.0006258038130483376113, 0.0009388807108837884767, 0.001251957608719239451 ),
 .UNSPECIFIED. ) ;
#128617 = CARTESIAN_POINT ( 'NONE',  ( 11.04536101718726293, 10.90000000000000036, 1.099999999999996758 ) ) ;
#128618 = CARTESIAN_POINT ( 'NONE',  ( 3.065552130021340194, 6.590578228417936835, 0.000000000000000000 ) ) ;
#128619 = CARTESIAN_POINT ( 'NONE',  ( 5.112599315731837457, 6.496590726105775815, -1.208607640439966158 ) ) ;
#128620 = CARTESIAN_POINT ( 'NONE',  ( -9.164948653157999559, 10.75515685251491504, -1.082531754730539753 ) ) ;
#128622 = CARTESIAN_POINT ( 'NONE',  ( 2.742673093864269163, 1.230450920196803022, -1.849320754654346866 ) ) ;
#128621 = CARTESIAN_POINT ( 'NONE',  ( 1.846092968827160119, -1.388944967848893430, -1.602481653760478020 ) ) ;
#128623 = CARTESIAN_POINT ( 'NONE',  ( -5.608756857104943094, 5.628625835799693888, 0.4592586763518708426 ) ) ;
#128624 = CARTESIAN_POINT ( 'NONE',  ( -4.288121723672178476, 8.224835454251337552, -0.7998128361456362523 ) ) ;
#128625 = CARTESIAN_POINT ( 'NONE',  ( 4.638861114170084399, 8.563755066507100722, 0.7998128361456462443 ) ) ;
#128626 = CARTESIAN_POINT ( 'NONE',  ( 3.648837080137564470, -0.3802854374791163616, -1.924481129451253603 ) ) ;
#128627 = CARTESIAN_POINT ( 'NONE',  ( 6.484877546038077867, 6.460111979999551224, 1.040834085586084257E-14 ) ) ;
#128628 = CARTESIAN_POINT ( 'NONE',  ( -4.235850332497944848, 7.335353122692886529, 0.8760575672057471230 ) ) ;
#128629 = CARTESIAN_POINT ( 'NONE',  ( 4.684505768721569652, 5.424010470718658716, -1.199719254218452047 ) ) ;
#128630 = CARTESIAN_POINT ( 'NONE',  ( -5.492461627311929995, 5.580495784718250363, 0.000000000000000000 ) ) ;
#128631 = CARTESIAN_POINT ( 'NONE',  ( -6.399085315970142851, 8.488685506763726352, -1.443375672974059665 ) ) ;
#128632 = COLOUR_RGB ( '', 0.66274510, 0.83137255, 0.94901961) ;
#128633 = CARTESIAN_POINT ( 'NONE',  ( 2.777707764728345907, 0.3069055913166895966, -2.098134212408508059 ) ) ;
#128634 = CARTESIAN_POINT ( 'NONE',  ( -6.296835998904160014, 6.311006518335105397, 0.000000000000000000 ) ) ;
#128635 = CARTESIAN_POINT ( 'NONE',  ( 4.399409362686744096, 1.734418756986338295, 1.290045131933370781 ) ) ;
#128636 = CARTESIAN_POINT ( 'NONE',  ( 3.333393596924072444, 0.8250370302015205271, -1.646115572170883334 ) ) ;
#128637 = TOROIDAL_SURFACE ( 'NONE', #476, 3.971937515251341644, 0.08000000000000000167 ) ;
#128638 = CARTESIAN_POINT ( 'NONE',  ( -4.698067037153471404, 6.865000302791745668, 1.228424997642649563 ) ) ;
#128639 = CARTESIAN_POINT ( 'NONE',  ( -0.6823417656250246877, -0.1364583329919108468, 1.181850606188755259 ) ) ;
#128640 = CARTESIAN_POINT ( 'NONE',  ( 6.246048974015395494, 0.5531718476652900396, 1.650163303580793217 ) ) ;
#128641 = CARTESIAN_POINT ( 'NONE',  ( -11.33772463945037146, 19.00000000000000000, 3.679999999999999272 ) ) ;
#128642 = CARTESIAN_POINT ( 'NONE',  ( 5.341549334104194635, 6.294524313618772737, 1.082531754730558626 ) ) ;
#128643 = EDGE_CURVE ( 'NONE', #51477, #164408, #177465, .T. ) ;
#128645 = CARTESIAN_POINT ( 'NONE',  ( 2.975616057669258741, 2.053088362031017855, -0.6768339029224537118 ) ) ;
#128644 = PRODUCT_DEFINITION ( 'UNKNOWN', '', #173395, #184634 ) ;
#128646 = CARTESIAN_POINT ( 'NONE',  ( 4.253279712585047001, -1.993766238088546361, -0.2985801555873274227 ) ) ;
#128647 = CARTESIAN_POINT ( 'NONE',  ( -9.503902493055310430, 11.15060299906175167, 1.082531754730558626 ) ) ;
#128648 = CARTESIAN_POINT ( 'NONE',  ( 2.711983997553393699, -2.138339778157403615, 0.3160903847422363300 ) ) ;
#128649 = CARTESIAN_POINT ( 'NONE',  ( 2.776590643643538581, -1.885432240069355503, -0.5755950866291289492 ) ) ;
#128650 = CARTESIAN_POINT ( 'NONE',  ( 6.509000000000010999, 0.004788705324892603143, 2.000274819378269786 ) ) ;
#128651 = CARTESIAN_POINT ( 'NONE',  ( 4.458499667006603495, -1.736235857128598070, -0.8702183630341918663 ) ) ;
#128654 = VERTEX_POINT ( 'NONE', #67808 ) ;
#128653 = CARTESIAN_POINT ( 'NONE',  ( 8.029456579251872839, -5.199789852012450808, -7.518896314322964791 ) ) ;
#128652 = CARTESIAN_POINT ( 'NONE',  ( -9.503902493055310430, 11.15060299906175167, 1.082531754730558626 ) ) ;
#128655 = CARTESIAN_POINT ( 'NONE',  ( -6.084577077482911101, 10.32070003369722144, 0.000000000000000000 ) ) ;
#128656 = LINE ( 'NONE', #210866, #43762 ) ;
#128658 = VERTEX_POINT ( 'NONE', #199963 ) ;
#128657 = CARTESIAN_POINT ( 'NONE',  ( -6.005335696210345020, 5.970922831858983315, 0.7998128361456281477 ) ) ;
#128659 = CARTESIAN_POINT ( 'NONE',  ( -8.093854517234044366, 11.42628545587295186, 1.082531754730549967 ) ) ;
#128660 = CARTESIAN_POINT ( 'NONE',  ( 0.9388347430083656686, 2.174419798330699649, 0.3756190385216377492 ) ) ;
#128661 = CARTESIAN_POINT ( 'NONE',  ( 1.642778471875001811, -1.042708332855375009, 2.845375778867859751 ) ) ;
#128662 = CARTESIAN_POINT ( 'NONE',  ( 5.893401036868160858, -1.775023410133094615, 0.8355650083611900758 ) ) ;
#128663 = CARTESIAN_POINT ( 'NONE',  ( 1.364683531249990311, 5.196875000341417916, 1.214306433183764966E-14 ) ) ;
#128664 = CARTESIAN_POINT ( 'NONE',  ( -1.500000000000011324, 4.660416667349484676, -0.8660254037844313801 ) ) ;
#128665 = CARTESIAN_POINT ( 'NONE',  ( 5.089368577813358385, 6.729159871965151751, -1.415889853396500975 ) ) ;
#128666 = CARTESIAN_POINT ( 'NONE',  ( 0.07499057489264347731, 7.629137130509110243, -2.555503484197537922 ) ) ;
#128667 = CARTESIAN_POINT ( 'NONE',  ( 5.947170714876300224, 0.5300644225827764178, -1.763184533696081857 ) ) ;
#128668 = VERTEX_POINT ( 'NONE', #35334 ) ;
#128669 = CARTESIAN_POINT ( 'NONE',  ( -1.360316468750002894, -0.6302083329919370147, -0.7853790794158941324 ) ) ;
#128670 = CARTESIAN_POINT ( 'NONE',  ( -6.659026002606323047, 10.92061410301605662, 0.000000000000000000 ) ) ;
#128671 = CARTESIAN_POINT ( 'NONE',  ( 0.000000000000000000, 15.00041888085534758, 0.000000000000000000 ) ) ;
#128672 = CARTESIAN_POINT ( 'NONE',  ( 6.328397690248316110, -1.000878058022572903, -1.869571840794107986 ) ) ;
#128673 = CARTESIAN_POINT ( 'NONE',  ( 9.070174955424544549, 12.14068019893067429, 7.786856565648018424 ) ) ;
#128674 = CARTESIAN_POINT ( 'NONE',  ( 5.124091990960999432, 8.065525525174782828, -1.199719254218452047 ) ) ;
#128675 = CARTESIAN_POINT ( 'NONE',  ( 0.07516593201271813685, 0.0004601587237540622779, -2.044269526395313452 ) ) ;
#128678 = CARTESIAN_POINT ( 'NONE',  ( 3.140019216317342376, 0.4501627324021878485, 1.785233193441162491 ) ) ;
#128677 = CARTESIAN_POINT ( 'NONE',  ( 1.662329954472214322, -0.6657413170317361129, -1.738099805993092106 ) ) ;
#128676 = CARTESIAN_POINT ( 'NONE',  ( 0.000000000000000000, 15.50000000000019362, 0.000000000000000000 ) ) ;
#128679 = CARTESIAN_POINT ( 'NONE',  ( 7.096803341749390981, 10.36702210109460154, -1.199719254218441611 ) ) ;
#128680 = FACE_OUTER_BOUND ( 'NONE', #93349, .T. ) ;
#128681 = CARTESIAN_POINT ( 'NONE',  ( -7.117104292530948229, 7.267986194233038155, -0.7998128361456362523 ) ) ;
#128682 = CARTESIAN_POINT ( 'NONE',  ( -6.776370306708066948, -7.161464053357560644, -6.781144757626046626 ) ) ;
#128683 = CARTESIAN_POINT ( 'NONE',  ( 3.334799921508072806, 2.153101868192684343, 0.4835390122766567433 ) ) ;
#128684 = CARTESIAN_POINT ( 'NONE',  ( 5.747450795320371064, -1.778423256021565813, -1.398359773074304480 ) ) ;
#128685 = CARTESIAN_POINT ( 'NONE',  ( -5.395781948558855845, 9.238903340053241209, 0.7216878364870458196 ) ) ;
#128686 = CARTESIAN_POINT ( 'NONE',  ( 5.554893708145399067, 0.3617622393776204204, 1.774916939089685730 ) ) ;
#128687 = CARTESIAN_POINT ( 'NONE',  ( 5.946487413881851758, -1.349596479577100272, 1.359900094196204279 ) ) ;
#128688 = DIRECTION ( 'NONE',  ( 1.000000000000000000, -8.673617379884035472E-16, 0.000000000000000000 ) ) ;
#128689 = CARTESIAN_POINT ( 'NONE',  ( 5.981297838379462384, 1.727768277425823396, -0.7175292643646775659 ) ) ;
#128690 = CARTESIAN_POINT ( 'NONE',  ( 5.517805331081858888, 5.539787095791365523, 1.040834085586084257E-14 ) ) ;
#128691 = AXIS2_PLACEMENT_3D ( 'NONE', #186294, #99729, #149548 ) ;
#128692 = CARTESIAN_POINT ( 'NONE',  ( 6.086734230332795370, -0.2636980280019511902, -1.749942407053702409 ) ) ;
#128693 = CARTESIAN_POINT ( 'NONE',  ( 0.9894706735516716201, -0.4852629857438545691, 1.957171443305204761 ) ) ;
#128695 = CARTESIAN_POINT ( 'NONE',  ( 3.352270206574393008, 2.106257355090755290, -0.0002192025019883553090 ) ) ;
#128694 = CARTESIAN_POINT ( 'NONE',  ( -10.00321840878439339, 10.56484298653695397, 1.040834085586084257E-14 ) ) ;
#128696 = CARTESIAN_POINT ( 'NONE',  ( 8.718056468787178659, 10.12981962079525289, 1.199719254218462483 ) ) ;
#128698 = CARTESIAN_POINT ( 'NONE',  ( -8.666686507633592385, 11.13422023037111330, 1.599625672291269396 ) ) ;
#128697 = CARTESIAN_POINT ( 'NONE',  ( 1.499999999999985123, -0.2041666666666457353, -0.8660254037844323793 ) ) ;
#128699 = DIRECTION ( 'NONE',  ( 0.000000000000000000, -0.000000000000000000, 1.000000000000000000 ) ) ;
#128700 = CARTESIAN_POINT ( 'NONE',  ( 3.023699206349286239, -0.3898671064326043045, 1.981619672226095918 ) ) ;
#128701 = CARTESIAN_POINT ( 'NONE',  ( -1.364683531250012516, 3.738541667008087099, -0.7879004041258300672 ) ) ;
#128702 = CARTESIAN_POINT ( 'NONE',  ( 3.009020027229115879, 5.597941567487558778, -1.199719254218446718 ) ) ;
#128703 = CARTESIAN_POINT ( 'NONE',  ( 3.427187520701843404, 0.04928524951339217919, 2.161187641841005647 ) ) ;
#128704 = CARTESIAN_POINT ( 'NONE',  ( 7.472478939787284169, 8.746922180287201698, 1.199719254218452935 ) ) ;
#128706 =( NAMED_UNIT ( * ) PLANE_ANGLE_UNIT ( ) SI_UNIT ( $, .RADIAN. ) );
#128705 = CARTESIAN_POINT ( 'NONE',  ( 5.982890925380405456, 10.20206618957764100, 0.000000000000000000 ) ) ;
#128707 = CARTESIAN_POINT ( 'NONE',  ( 9.042925270190625753, 11.57316545335434199, 1.443375672974076540 ) ) ;
#128709 = CARTESIAN_POINT ( 'NONE',  ( 6.928203230275522984, 15.46908218388476008, -9.797958971132700867 ) ) ;
#128708 = CARTESIAN_POINT ( 'NONE',  ( 1.012457490462664644, 2.168662962709181574, -0.1065306264821704596 ) ) ;
#128710 = CARTESIAN_POINT ( 'NONE',  ( -5.856759171423528088, 8.816340885760650892, 1.082531754730548412 ) ) ;
#128711 = CARTESIAN_POINT ( 'NONE',  ( -1.201851678989727383E-14, 0.8218750003414171390, 1.575800808251672791 ) ) ;
#128712 = CARTESIAN_POINT ( 'NONE',  ( 2.525153347276567484, -2.043736813514348771, 0.7916865192442237298 ) ) ;
#128713 = CARTESIAN_POINT ( 'NONE',  ( 0.4680205011783269420, 8.035366863023833517, 1.945178226287680223 ) ) ;
#128714 = CARTESIAN_POINT ( 'NONE',  ( 2.817521562391828827, -0.2228243041610066255, 2.251526839675880520 ) ) ;
#128715 = CARTESIAN_POINT ( 'NONE',  ( -6.808165692356648258, 11.09461040772476714, 0.7998128361456481317 ) ) ;
#128716 = CARTESIAN_POINT ( 'NONE',  ( -3.429849674132948500, 5.024577257953626308, -1.443375672974051449 ) ) ;
#128717 = CARTESIAN_POINT ( 'NONE',  ( 0.6823417656249917140, 3.905208333674754950, 1.181850606188765695 ) ) ;
#128718 = CARTESIAN_POINT ( 'NONE',  ( 5.355423173304108886, 7.585870477640591858, 1.239999553246450725 ) ) ;
#128719 = PRESENTATION_LAYER_ASSIGNMENT (  '', '', ( #145980 ) ) ;
#128720 = CARTESIAN_POINT ( 'NONE',  ( -1.500000000000008216, 11.99999999999999645, 3.469446951953614189E-15 ) ) ;
#128721 = CARTESIAN_POINT ( 'NONE',  ( 6.211043768836173484, 8.339580045099285854, 1.443375672974065660 ) ) ;
#128722 = CARTESIAN_POINT ( 'NONE',  ( 3.795971232924668648, -1.767634583600716569, -0.08911788016389800282 ) ) ;
#128723 = CARTESIAN_POINT ( 'NONE',  ( 8.062294901620731480, 12.55776115186623620, 1.040834085586084257E-14 ) ) ;
#128724 = CARTESIAN_POINT ( 'NONE',  ( 6.821333372217227797, -0.1664864972488830641, 2.170661319153658564 ) ) ;
#128725 = CARTESIAN_POINT ( 'NONE',  ( 0.6823417656249969321, 9.776041667008065872, -1.181850606188757036 ) ) ;
#128726 = CARTESIAN_POINT ( 'NONE',  ( -4.634908411025374875, 6.500755460986618495, 1.599625672291263179 ) ) ;
#128727 = DIRECTION ( 'NONE',  ( 0.000000000000000000, 1.000000000000000000, 0.000000000000000000 ) ) ;
#128728 = ORIENTED_EDGE ( 'NONE', *, *, #35454, .T. ) ;
#128729 = COLOUR_RGB ( '', 0.66274510, 0.83137255, 0.94901961) ;
#128730 = CARTESIAN_POINT ( 'NONE',  ( 3.854256360616271415, 0.6726810918341770140, 1.745705178215435582 ) ) ;
#128731 = CARTESIAN_POINT ( 'NONE',  ( 3.643477671580112709, 1.873648065284461817, -0.8808079623299628347 ) ) ;
#128732 = CARTESIAN_POINT ( 'NONE',  ( -6.739811759324840779, 7.035737605399991601, -0.7216878364870338292 ) ) ;
#128733 = CARTESIAN_POINT ( 'NONE',  ( -9.949604414185204249, 5.483733089116166859, -6.039292150722699759 ) ) ;
#128734 =( BOUNDED_SURFACE ( )  B_SPLINE_SURFACE ( 1, 2, ( 
 ( #37430, #198053, #81116, #83233, #203106, #17159, #15025, #149318, #96326, #147202, #213227, #103508, #64859, #212161, #137081, #131004, #69903, #80043, #136013, #53686, #119817, #54751, #120901, #169567, #196996, #16087, #82171, #148265, #49682, #115809, #181797, #33430, #124117, #104584, #190080, #157607, #40658, #126242, #170629, #141390, #22215, #9203, #73115, #155455, #5970, #56887, #24360, #172788, #92622, #76337, #26514, #8128, #41732, #139216, #107841, #55817, #38506, #106759, #123062, #39568, #205246, #158664, #105670, #89406, #121974, #173869, #142444, #207400, #75275, #189016, #90471, #156538, #208452, #187938, #74214, #191137, #154392, #171697, #72040, #140309, #23296, #59019, #206327, #42802, #125175, #88328, #108911, #60084, #174933, #204162, #57952, #138153, #7038, #25443, #91550, #10262, #78467, #63290, #209514, #192203, #45997, #62229, #193287, #144586, #97946, #44932, #28664, #61155, #129450, #15576, #146703, #162935, #12388, #29734, #112116, #81663, #127317, #210600, #130504, #93683, #111040, #11324, #95816, #177047, #212719, #13462, #196491, #64358, #109981, #14516, #213767, #48133, #143519, #178119, #27585, #94749, #179183, #147749, #114246, #80610, #79538, #65388, #30806, #161875, #180243, #194354, #31867, #164000, #128387, #145656, #195433, #43865, #211652, #47062, #113179, #96886, #175991, #159725, #77402, #160797, #132587, #53424, #197537, #37177, #16641, #167187, #66445, #69653, #119561, #49182, #2512, #3578, #35027, #116356, #118497, #20897, #134710, #198589, #200717, #131535, #82725, #148802, #135761, #371, #181291, #185548, #165049, #102181, #115301, #52368, #184479, #152006, #103252, #153066, #36096, #50236, #32918, #182346, #17699, #201784, #101100, #68585, #150948, #168248, #98994, #19847, #85934, #133656, #4643, #33975, #169313, #100050, #86993, #166114, #83786, #149881, #1446, #117428, #51303, #67511, #199657, #183426, #18774, #84860, #72864, #173617, #58765, #89153, #188760, #73952, #25189, #155206, #40400, #206069, #106502, #24113, #90216, #104324, #54500, #71785, #207141 ),
 ( #190881, #123860, #39315, #170372, #158406, #174678, #154140, #21959, #41474, #189825, #171448, #70713, #202852, #156280, #8940, #124919, #5708, #137900, #105410, #6787, #157351, #107584, #42546, #120644, #26251, #23037, #108650, #92369, #203919, #91293, #172529, #75020, #186623, #138970, #141131, #136826, #7864, #38250, #140044, #55567, #88067, #121721, #187686, #204993, #56637, #122801, #57703, #109722, #13208, #79282, #28399, #94494, #160532, #111858, #80345, #46807, #145400, #128127, #97686, #125982, #12137, #45739, #10005, #76081, #211400, #78210, #144334, #161616, #159464, #142182, #210334, #177863, #208197, #64104, #195173, #44670, #96626, #59830, #178933, #146446, #61972, #93425, #194090, #29475, #196237, #63029, #95566, #193018, #129196, #191940, #175729, #113993, #77142, #112921, #30548, #110782, #43605, #162681, #14254, #27323, #11063, #212459, #47880, #130246, #179988, #31611, #143263, #209253, #60897, #127056, #176784, #16387, #69399, #2258, #132334, #48925, #36915, #53177, #32658, #197285, #134466, #68334, #49980, #163744, #81413, #117172, #101928, #3329, #98737, #164795, #198340, #33720, #35850, #200469, #135506, #147495, #119305, #116098, #151760, #201529, #82467, #52116, #67260, #167994, #213516, #182090, #118244, #185291, #100852, #19600, #183174, #148556, #65139, #122, #85672, #66190, #15323, #99798, #17449, #115045, #166938, #18530, #165863, #83533, #149615, #51048, #131295, #184226, #84607, #133398, #181043, #1197, #199402, #34778, #150696, #190623, #106247, #105149, #171189, #40134, #37997, #102998, #22779, #138712, #86741, #157093, #73689, #137645, #189571, #152811, #57446, #24929, #121465, #186362, #187435, #88896, #74764, #172271, #204729, #71535, #154950, #20651, #54250, #206879, #170116, #23858, #6535, #203665, #4389, #56379, #205814, #70460, #104069, #139787, #140867, #41217, #123607, #136577, #72613, #91033, #21702, #39063, #8682, #169054, #89965, #58511, #173347, #122542, #107323, #5455, #188503, #156017, #124666, #7605, #202597, #55315, #120387, #87814, #153886, #110530, #126798 ) ),
 .UNSPECIFIED., .F., .F., .F. ) 
 B_SPLINE_SURFACE_WITH_KNOTS ( ( 2, 2 ),
 ( 3, 2, 2, 2, 2, 2, 2, 2, 2, 2, 2, 2, 2, 2, 2, 2, 2, 2, 2, 2, 2, 2, 2, 2, 2, 2, 2, 2, 2, 2, 2, 2, 2, 2, 2, 2, 2, 2, 2, 2, 2, 2, 2, 2, 2, 2, 2, 2, 2, 2, 2, 2, 2, 2, 2, 2, 2, 2, 2, 2, 2, 2, 2, 2, 2, 2, 2, 2, 2, 2, 2, 2, 2, 2, 2, 2, 2, 2, 2, 2, 2, 2, 2, 2, 2, 2, 2, 2, 2, 2, 2, 2, 2, 2, 2, 2, 2, 2, 2, 2, 2, 2, 2, 2, 2, 2, 2, 2, 2, 2, 2, 2, 2, 2, 2, 2, 2, 2, 2, 2, 3 ),
 ( 0.000000000000000000, 1.000000000000000000 ),
 ( 0.000000000000000000, 0.008333333333333333218, 0.01666666666666666644, 0.02500000000000000139, 0.03333333333333333287, 0.04166666666666666435, 0.05000000000000000278, 0.05833333333333333426, 0.06666666666666666574, 0.07499999999999999722, 0.08333333333333332871, 0.09166666666666666019, 0.1000000000000000056, 0.1083333333333333370, 0.1166666666666666685, 0.1250000000000000000, 0.1333333333333333315, 0.1416666666666666630, 0.1499999999999999944, 0.1583333333333333259, 0.1666666666666666574, 0.1749999999999999889, 0.1833333333333333204, 0.1916666666666666796, 0.2000000000000000111, 0.2083333333333333426, 0.2166666666666666741, 0.2250000000000000056, 0.2333333333333333370, 0.2416666666666666685, 0.2500000000000000000, 0.2583333333333333592, 0.2666666666666666630, 0.2750000000000000222, 0.2833333333333333259, 0.2916666666666666852, 0.2999999999999999889, 0.3083333333333333481, 0.3166666666666666519, 0.3250000000000000111, 0.3333333333333333148, 0.3416666666666666741, 0.3499999999999999778, 0.3583333333333333370, 0.3666666666666666408, 0.3750000000000000000, 0.3833333333333333592, 0.3916666666666666630, 0.4000000000000000222, 0.4083333333333333259, 0.4166666666666666852, 0.4249999999999999889, 0.4333333333333333481, 0.4416666666666666519, 0.4500000000000000111, 0.4583333333333333148, 0.4666666666666666741, 0.4749999999999999778, 0.4833333333333333370, 0.4916666666666666408, 0.5000000000000000000, 0.5083333333333333037, 0.5166666666666667185, 0.5250000000000000222, 0.5333333333333333259, 0.5416666666666666297, 0.5500000000000000444, 0.5583333333333333481, 0.5666666666666666519, 0.5749999999999999556, 0.5833333333333333703, 0.5916666666666666741, 0.5999999999999999778, 0.6083333333333332815, 0.6166666666666666963, 0.6250000000000000000, 0.6333333333333333037, 0.6416666666666667185, 0.6500000000000000222, 0.6583333333333333259, 0.6666666666666666297, 0.6750000000000000444, 0.6833333333333333481, 0.6916666666666666519, 0.6999999999999999556, 0.7083333333333333703, 0.7166666666666666741, 0.7249999999999999778, 0.7333333333333332815, 0.7416666666666666963, 0.7500000000000000000, 0.7583333333333333037, 0.7666666666666667185, 0.7750000000000000222, 0.7833333333333333259, 0.7916666666666666297, 0.8000000000000000444, 0.8083333333333333481, 0.8166666666666666519, 0.8249999999999999556, 0.8333333333333333703, 0.8416666666666666741, 0.8499999999999999778, 0.8583333333333332815, 0.8666666666666666963, 0.8750000000000000000, 0.8833333333333333037, 0.8916666666666667185, 0.9000000000000000222, 0.9083333333333333259, 0.9166666666666666297, 0.9250000000000000444, 0.9333333333333333481, 0.9416666666666666519, 0.9499999999999999556, 0.9583333333333333703, 0.9666666666666666741, 0.9749999999999999778, 0.9833333333333332815, 0.9916666666666666963, 1.000000000000000000 ),
 .UNSPECIFIED. ) 
 GEOMETRIC_REPRESENTATION_ITEM ( )  RATIONAL_B_SPLINE_SURFACE ( (
 ( 1.000000000000000000, 0.8660254037844387076, 1.000000000000000000, 0.8660254037844387076, 1.000000000000000000, 0.8660254037844387076, 1.000000000000000000, 0.8660254037844387076, 1.000000000000000000, 0.8660254037844387076, 1.000000000000000000, 0.8660254037844387076, 1.000000000000000000, 0.8660254037844387076, 1.000000000000000000, 0.8660254037844387076, 1.000000000000000000, 0.8660254037844387076, 1.000000000000000000, 0.8660254037844387076, 1.000000000000000000, 0.8660254037844387076, 1.000000000000000000, 0.8660254037844387076, 1.000000000000000000, 0.8660254037844387076, 1.000000000000000000, 0.8660254037844387076, 1.000000000000000000, 0.8660254037844387076, 1.000000000000000000, 0.8660254037844387076, 1.000000000000000000, 0.8660254037844387076, 1.000000000000000000, 0.8660254037844387076, 1.000000000000000000, 0.8660254037844387076, 1.000000000000000000, 0.8660254037844387076, 1.000000000000000000, 0.8660254037844387076, 1.000000000000000000, 0.8660254037844387076, 1.000000000000000000, 0.8660254037844387076, 1.000000000000000000, 0.8660254037844387076, 1.000000000000000000, 0.8660254037844387076, 1.000000000000000000, 0.8660254037844387076, 1.000000000000000000, 0.8660254037844387076, 1.000000000000000000, 0.8660254037844387076, 1.000000000000000000, 0.8660254037844387076, 1.000000000000000000, 0.8660254037844387076, 1.000000000000000000, 0.8660254037844387076, 1.000000000000000000, 0.8660254037844387076, 1.000000000000000000, 0.8660254037844387076, 1.000000000000000000, 0.8660254037844387076, 1.000000000000000000, 0.8660254037844387076, 1.000000000000000000, 0.8660254037844387076, 1.000000000000000000, 0.8660254037844387076, 1.000000000000000000, 0.8660254037844387076, 1.000000000000000000, 0.8660254037844387076, 1.000000000000000000, 0.8660254037844387076, 1.000000000000000000, 0.8660254037844387076, 1.000000000000000000, 0.8660254037844387076, 1.000000000000000000, 0.8660254037844387076, 1.000000000000000000, 0.8660254037844387076, 1.000000000000000000, 0.8660254037844387076, 1.000000000000000000, 0.8660254037844387076, 1.000000000000000000, 0.8660254037844387076, 1.000000000000000000, 0.8660254037844387076, 1.000000000000000000, 0.8660254037844387076, 1.000000000000000000, 0.8660254037844387076, 1.000000000000000000, 0.8660254037844387076, 1.000000000000000000, 0.8660254037844387076, 1.000000000000000000, 0.8660254037844387076, 1.000000000000000000, 0.8660254037844387076, 1.000000000000000000, 0.8660254037844387076, 1.000000000000000000, 0.8660254037844387076, 1.000000000000000000, 0.8660254037844387076, 1.000000000000000000, 0.8660254037844387076, 1.000000000000000000, 0.8660254037844387076, 1.000000000000000000, 0.8660254037844387076, 1.000000000000000000, 0.8660254037844387076, 1.000000000000000000, 0.8660254037844387076, 1.000000000000000000, 0.8660254037844387076, 1.000000000000000000, 0.8660254037844387076, 1.000000000000000000, 0.8660254037844387076, 1.000000000000000000, 0.8660254037844387076, 1.000000000000000000, 0.8660254037844387076, 1.000000000000000000, 0.8660254037844387076, 1.000000000000000000, 0.8660254037844387076, 1.000000000000000000, 0.8660254037844387076, 1.000000000000000000, 0.8660254037844387076, 1.000000000000000000, 0.8660254037844387076, 1.000000000000000000, 0.8660254037844387076, 1.000000000000000000, 0.8660254037844387076, 1.000000000000000000, 0.8660254037844387076, 1.000000000000000000, 0.8660254037844387076, 1.000000000000000000, 0.8660254037844387076, 1.000000000000000000, 0.8660254037844387076, 1.000000000000000000, 0.8660254037844387076, 1.000000000000000000, 0.8660254037844387076, 1.000000000000000000, 0.8660254037844387076, 1.000000000000000000, 0.8660254037844387076, 1.000000000000000000, 0.8660254037844387076, 1.000000000000000000, 0.8660254037844387076, 1.000000000000000000, 0.8660254037844387076, 1.000000000000000000, 0.8660254037844387076, 1.000000000000000000, 0.8660254037844387076, 1.000000000000000000, 0.8660254037844387076, 1.000000000000000000, 0.8660254037844387076, 1.000000000000000000, 0.8660254037844387076, 1.000000000000000000, 0.8660254037844387076, 1.000000000000000000, 0.8660254037844387076, 1.000000000000000000, 0.8660254037844387076, 1.000000000000000000, 0.8660254037844387076, 1.000000000000000000, 0.8660254037844387076, 1.000000000000000000, 0.8660254037844387076, 1.000000000000000000, 0.8660254037844387076, 1.000000000000000000, 0.8660254037844387076, 1.000000000000000000, 0.8660254037844387076, 1.000000000000000000, 0.8660254037844387076, 1.000000000000000000, 0.8660254037844387076, 1.000000000000000000, 0.8660254037844387076, 1.000000000000000000, 0.8660254037844387076, 1.000000000000000000, 0.8660254037844387076, 1.000000000000000000, 0.8660254037844387076, 1.000000000000000000, 0.8660254037844387076, 1.000000000000000000, 0.8660254037844387076, 1.000000000000000000, 0.8660254037844387076, 1.000000000000000000, 0.8660254037844387076, 1.000000000000000000, 0.8660254037844387076, 1.000000000000000000, 0.8660254037844387076, 1.000000000000000000, 0.8660254037844387076, 1.000000000000000000, 0.8660254037844387076, 1.000000000000000000, 0.8660254037844387076, 1.000000000000000000, 0.8660254037844387076, 1.000000000000000000, 0.8660254037844387076, 1.000000000000000000, 0.8660254037844387076, 1.000000000000000000, 0.8660254037844387076, 1.000000000000000000, 0.8660254037844387076, 1.000000000000000000, 0.8660254037844387076, 1.000000000000000000),
 ( 1.000000000000000000, 0.8660254037844387076, 1.000000000000000000, 0.8660254037844387076, 1.000000000000000000, 0.8660254037844387076, 1.000000000000000000, 0.8660254037844387076, 1.000000000000000000, 0.8660254037844387076, 1.000000000000000000, 0.8660254037844387076, 1.000000000000000000, 0.8660254037844387076, 1.000000000000000000, 0.8660254037844387076, 1.000000000000000000, 0.8660254037844387076, 1.000000000000000000, 0.8660254037844387076, 1.000000000000000000, 0.8660254037844387076, 1.000000000000000000, 0.8660254037844387076, 1.000000000000000000, 0.8660254037844387076, 1.000000000000000000, 0.8660254037844387076, 1.000000000000000000, 0.8660254037844387076, 1.000000000000000000, 0.8660254037844387076, 1.000000000000000000, 0.8660254037844387076, 1.000000000000000000, 0.8660254037844387076, 1.000000000000000000, 0.8660254037844387076, 1.000000000000000000, 0.8660254037844387076, 1.000000000000000000, 0.8660254037844387076, 1.000000000000000000, 0.8660254037844387076, 1.000000000000000000, 0.8660254037844387076, 1.000000000000000000, 0.8660254037844387076, 1.000000000000000000, 0.8660254037844387076, 1.000000000000000000, 0.8660254037844387076, 1.000000000000000000, 0.8660254037844387076, 1.000000000000000000, 0.8660254037844387076, 1.000000000000000000, 0.8660254037844387076, 1.000000000000000000, 0.8660254037844387076, 1.000000000000000000, 0.8660254037844387076, 1.000000000000000000, 0.8660254037844387076, 1.000000000000000000, 0.8660254037844387076, 1.000000000000000000, 0.8660254037844387076, 1.000000000000000000, 0.8660254037844387076, 1.000000000000000000, 0.8660254037844387076, 1.000000000000000000, 0.8660254037844387076, 1.000000000000000000, 0.8660254037844387076, 1.000000000000000000, 0.8660254037844387076, 1.000000000000000000, 0.8660254037844387076, 1.000000000000000000, 0.8660254037844387076, 1.000000000000000000, 0.8660254037844387076, 1.000000000000000000, 0.8660254037844387076, 1.000000000000000000, 0.8660254037844387076, 1.000000000000000000, 0.8660254037844387076, 1.000000000000000000, 0.8660254037844387076, 1.000000000000000000, 0.8660254037844387076, 1.000000000000000000, 0.8660254037844387076, 1.000000000000000000, 0.8660254037844387076, 1.000000000000000000, 0.8660254037844387076, 1.000000000000000000, 0.8660254037844387076, 1.000000000000000000, 0.8660254037844387076, 1.000000000000000000, 0.8660254037844387076, 1.000000000000000000, 0.8660254037844387076, 1.000000000000000000, 0.8660254037844387076, 1.000000000000000000, 0.8660254037844387076, 1.000000000000000000, 0.8660254037844387076, 1.000000000000000000, 0.8660254037844387076, 1.000000000000000000, 0.8660254037844387076, 1.000000000000000000, 0.8660254037844387076, 1.000000000000000000, 0.8660254037844387076, 1.000000000000000000, 0.8660254037844387076, 1.000000000000000000, 0.8660254037844387076, 1.000000000000000000, 0.8660254037844387076, 1.000000000000000000, 0.8660254037844387076, 1.000000000000000000, 0.8660254037844387076, 1.000000000000000000, 0.8660254037844387076, 1.000000000000000000, 0.8660254037844387076, 1.000000000000000000, 0.8660254037844387076, 1.000000000000000000, 0.8660254037844387076, 1.000000000000000000, 0.8660254037844387076, 1.000000000000000000, 0.8660254037844387076, 1.000000000000000000, 0.8660254037844387076, 1.000000000000000000, 0.8660254037844387076, 1.000000000000000000, 0.8660254037844387076, 1.000000000000000000, 0.8660254037844387076, 1.000000000000000000, 0.8660254037844387076, 1.000000000000000000, 0.8660254037844387076, 1.000000000000000000, 0.8660254037844387076, 1.000000000000000000, 0.8660254037844387076, 1.000000000000000000, 0.8660254037844387076, 1.000000000000000000, 0.8660254037844387076, 1.000000000000000000, 0.8660254037844387076, 1.000000000000000000, 0.8660254037844387076, 1.000000000000000000, 0.8660254037844387076, 1.000000000000000000, 0.8660254037844387076, 1.000000000000000000, 0.8660254037844387076, 1.000000000000000000, 0.8660254037844387076, 1.000000000000000000, 0.8660254037844387076, 1.000000000000000000, 0.8660254037844387076, 1.000000000000000000, 0.8660254037844387076, 1.000000000000000000, 0.8660254037844387076, 1.000000000000000000, 0.8660254037844387076, 1.000000000000000000, 0.8660254037844387076, 1.000000000000000000, 0.8660254037844387076, 1.000000000000000000, 0.8660254037844387076, 1.000000000000000000, 0.8660254037844387076, 1.000000000000000000, 0.8660254037844387076, 1.000000000000000000, 0.8660254037844387076, 1.000000000000000000, 0.8660254037844387076, 1.000000000000000000, 0.8660254037844387076, 1.000000000000000000, 0.8660254037844387076, 1.000000000000000000, 0.8660254037844387076, 1.000000000000000000, 0.8660254037844387076, 1.000000000000000000, 0.8660254037844387076, 1.000000000000000000, 0.8660254037844387076, 1.000000000000000000, 0.8660254037844387076, 1.000000000000000000, 0.8660254037844387076, 1.000000000000000000, 0.8660254037844387076, 1.000000000000000000, 0.8660254037844387076, 1.000000000000000000, 0.8660254037844387076, 1.000000000000000000, 0.8660254037844387076, 1.000000000000000000, 0.8660254037844387076, 1.000000000000000000, 0.8660254037844387076, 1.000000000000000000, 0.8660254037844387076, 1.000000000000000000, 0.8660254037844387076, 1.000000000000000000, 0.8660254037844387076, 1.000000000000000000, 0.8660254037844387076, 1.000000000000000000, 0.8660254037844387076, 1.000000000000000000, 0.8660254037844387076, 1.000000000000000000) ) ) 
 REPRESENTATION_ITEM ( '' )  SURFACE ( )  );
#128735 = CARTESIAN_POINT ( 'NONE',  ( 5.998930166150279852, 1.769978137569449883, -1.240765152474863298 ) ) ;
#128736 = CARTESIAN_POINT ( 'NONE',  ( -1.001543065824772872E-14, 5.634375000341415252, 1.575800808251672791 ) ) ;
#128737 = CARTESIAN_POINT ( 'NONE',  ( 2.998438581075290710, 1.946722116546204306, 0.2428724957088539971 ) ) ;
#128738 = CARTESIAN_POINT ( 'NONE',  ( 0.5618747747782488755, 1.677749815653075460, -1.117659098820653174 ) ) ;
#128739 = CARTESIAN_POINT ( 'NONE',  ( 7.654042494670951690E-16, 3.799999999999998046, -6.249999999999995559 ) ) ;
#128741 = CARTESIAN_POINT ( 'NONE',  ( -11.94654170777226376, 13.65174326158935969, -1.134972293687621647 ) ) ;
#128740 = CARTESIAN_POINT ( 'NONE',  ( 7.584896871841365851, 10.93646455286856956, -1.199719254218446718 ) ) ;
#128742 = CARTESIAN_POINT ( 'NONE',  ( 0.6845637836509765872, -0.2226890396202323152, -1.857165095135074218 ) ) ;
#128743 = CARTESIAN_POINT ( 'NONE',  ( -1.201851678989727383E-14, 4.196875000341417028, -1.575800808251660134 ) ) ;
#128744 = CARTESIAN_POINT ( 'NONE',  ( 2.636979257498579088, 1.897111442976556317, 0.6741904779793208569 ) ) ;
#128746 = CARTESIAN_POINT ( 'NONE',  ( 1.775175926465226039, 1.840253878465339055, -1.046873989079605050 ) ) ;
#128745 = CARTESIAN_POINT ( 'NONE',  ( -7.049876689426106680, 9.247942109129029475, -1.443375672974059665 ) ) ;
#128748 = ADVANCED_FACE ( 'NONE', ( #51612 ), #19081, .F. ) ;
#128747 = CARTESIAN_POINT ( 'NONE',  ( 10.38156701084615108, 9.116244165890112328, -6.071958079708653422 ) ) ;
#128749 = CARTESIAN_POINT ( 'NONE',  ( 3.859880467719906783, -0.6038372105774907350, 1.980330894321411517 ) ) ;
#128750 = CARTESIAN_POINT ( 'NONE',  ( 3.464990776744291345, 6.200183785247111778, 1.199719254218452047 ) ) ;
#128752 = CARTESIAN_POINT ( 'NONE',  ( 4.715538499454675403, 4.395883092318884522, 1.214306433183764966E-14 ) ) ;
#128751 = CARTESIAN_POINT ( 'NONE',  ( 5.384749270845579083, 1.844215719714219492, -0.9846981469126301345 ) ) ;
#128754 = VERTEX_POINT ( 'NONE', #56933 ) ;
#128753 = CARTESIAN_POINT ( 'NONE',  ( 5.543921259432438298, 0.7380120197021734496, -1.669944898041133552 ) ) ;
#128755 = CARTESIAN_POINT ( 'NONE',  ( 9.134442807305049428, 11.67993591332117376, 1.599625672291281386 ) ) ;
#128756 = CARTESIAN_POINT ( 'NONE',  ( 5.690973801507735352, 5.856266416820083975, -2.499999999999995115 ) ) ;
#128757 = CARTESIAN_POINT ( 'NONE',  ( 11.96247689755394639, 8.209949295921704859, 0.8094914028917779003 ) ) ;
#128758 = CARTESIAN_POINT ( 'NONE',  ( 6.651417122894856426, -1.768357563224710605, -1.319949637914811458 ) ) ;
#128759 = CARTESIAN_POINT ( 'NONE',  ( -1.364683531250000748, 10.92187500034139802, 0.000000000000000000 ) ) ;
#128760 = CARTESIAN_POINT ( 'NONE',  ( 5.162724115531083235, 0.5589384127702141658, 1.828758346017298919 ) ) ;
#128761 = CARTESIAN_POINT ( 'NONE',  ( -10.62011439820619429, 11.28455497419572318, -0.7998128361456221525 ) ) ;
#128762 = TOROIDAL_SURFACE ( 'NONE', #35280, 3.970406073902761790, 0.08000000000000000167 ) ;
#128763 = CARTESIAN_POINT ( 'NONE',  ( 7.091078035147269532, 8.231678114882006625, 1.199719254218462483 ) ) ;
#128764 = CARTESIAN_POINT ( 'NONE',  ( -1.360316468750007779, 2.171875000341411344, -4.336808689942017736E-14 ) ) ;
#128765 = CARTESIAN_POINT ( 'NONE',  ( 3.497113557321089861, 6.167384019261527683, -1.199719254218446718 ) ) ;
#128766 = EDGE_LOOP ( 'NONE', ( #15776, #192144 ) ) ;
#128767 = CARTESIAN_POINT ( 'NONE',  ( -7.262327558775498737, 8.501745569106741840, 1.199719254218452047 ) ) ;
#128768 = CARTESIAN_POINT ( 'NONE',  ( 4.657402308249613654, 0.4116239899518738810, -1.824517662812553009 ) ) ;
#128769 = CARTESIAN_POINT ( 'NONE',  ( -11.04536101718726293, 13.40000000000000036, 1.099999999999996758 ) ) ;
#128770 = CARTESIAN_POINT ( 'NONE',  ( 5.020262018810099924, 9.078999131912302900, 0.7998128361456331437 ) ) ;
#128771 = FACE_OUTER_BOUND ( 'NONE', #49129, .T. ) ;
#128772 = CARTESIAN_POINT ( 'NONE',  ( -6.232040409365024125, 6.934648621905299848, 0.8351839086257698552 ) ) ;
#128773 = EDGE_CURVE ( 'NONE', #67360, #94475, #15252, .T. ) ;
#128774 = CARTESIAN_POINT ( 'NONE',  ( -6.900736999675794792, 7.153207375817628666, 1.040834085586084257E-14 ) ) ;
#128775 = CARTESIAN_POINT ( 'NONE',  ( 5.345992642490140057, 5.131412925860272090, 1.040834085586084257E-14 ) ) ;
#128776 = CARTESIAN_POINT ( 'NONE',  ( 0.9363041846261275225, -1.098647377812447923, 1.634312829373037568 ) ) ;
#128777 = CARTESIAN_POINT ( 'NONE',  ( 2.917592388753763810, -1.356314522985989646, -1.492243612603139979 ) ) ;
#128778 = CARTESIAN_POINT ( 'NONE',  ( -6.008234629150358330, 10.16135750065076060, 0.000000000000000000 ) ) ;
#128779 = CARTESIAN_POINT ( 'NONE',  ( 6.052789233858158369, 6.026285292448116948, 0.000000000000000000 ) ) ;
#128780 = CARTESIAN_POINT ( 'NONE',  ( 3.134921595499224445, -1.932508288125428741, 1.033376004005027715 ) ) ;
#128781 = CARTESIAN_POINT ( 'NONE',  ( -8.890396042259075315, 11.39521468743417998, -1.599625672291263179 ) ) ;
#128782 = CARTESIAN_POINT ( 'NONE',  ( 6.825078400183556937, 1.282741234726336943, 1.971047034039685952 ) ) ;
#128783 = CARTESIAN_POINT ( 'NONE',  ( 0.2329586101569866563, 2.046406029004425253, -2.262590835625963415 ) ) ;
#128784 = CARTESIAN_POINT ( 'NONE',  ( 5.085717018901939390, 5.105960408239938353, 0.000000000000000000 ) ) ;
#128785 = CARTESIAN_POINT ( 'NONE',  ( 6.774270308322468459, 11.05506579301824743, 0.7998128361456462443 ) ) ;
#128786 = CARTESIAN_POINT ( 'NONE',  ( 6.536439455564168277, 6.798469917679251573, 0.7216878364870328300 ) ) ;
#128787 = ORIENTED_EDGE ( 'NONE', *, *, #208559, .F. ) ;
#128789 = CARTESIAN_POINT ( 'NONE',  ( 1.981109662258444537, -1.841391200710382980, -0.8139001868950055396 ) ) ;
#128788 = CARTESIAN_POINT ( 'NONE',  ( 4.985823801847525161, -1.827980399782932697, -0.2200341325891697619 ) ) ;
#128790 = CARTESIAN_POINT ( 'NONE',  ( 3.778943494763619793, -2.265100756353163103, 0.3889815702934427688 ) ) ;
#128792 = CARTESIAN_POINT ( 'NONE',  ( 1.955673630663162132, -0.6329532555123269510, 1.750116298748620958 ) ) ;
#128791 = CARTESIAN_POINT ( 'NONE',  ( -0.02880301295726198432, 7.629137130509075604, -2.873797191217826619 ) ) ;
#128793 = CARTESIAN_POINT ( 'NONE',  ( 1.001543065824772753E-15, -1.421874999522042327, 3.793834371823811669 ) ) ;
#128794 = CARTESIAN_POINT ( 'NONE',  ( 5.308822938259078583, -0.4706598425541131947, -1.853433239416848455 ) ) ;
#128795 = CARTESIAN_POINT ( 'NONE',  ( -7.344766530301162000, 9.591980256816594164, 1.599625672291295375 ) ) ;
#128796 = CARTESIAN_POINT ( 'NONE',  ( -4.990809943606273613, 7.876343129965691858, -1.082531754730549967 ) ) ;
#128798 = CARTESIAN_POINT ( 'NONE',  ( 3.344469905398727239, 0.4532862802011444758, 1.814783984445811127 ) ) ;
#128797 = CARTESIAN_POINT ( 'NONE',  ( 4.317973780707057507, 1.284968578774790426, -1.649195526182813509 ) ) ;
#128799 = CARTESIAN_POINT ( 'NONE',  ( 5.341549334104176872, 9.175631956522799726, 0.7216878364870438212 ) ) ;
#128800 = CARTESIAN_POINT ( 'NONE',  ( 5.970224376651540155, -1.750504005202535796, -0.5711807346103907612 ) ) ;
#128801 = VECTOR ( 'NONE', #200298, 1000.000000000000000 ) ;
#128802 = CARTESIAN_POINT ( 'NONE',  ( 2.510230996824538430, 6.080353262937265413, 0.000000000000000000 ) ) ;
#128803 = CARTESIAN_POINT ( 'NONE',  ( -1.938011383317839176E-15, -8.407420853759283830, -11.00029519899099917 ) ) ;
#128804 = CARTESIAN_POINT ( 'NONE',  ( 5.285687151129126349, 1.162661966624499277, 1.274325963116212934 ) ) ;
#128805 = CARTESIAN_POINT ( 'NONE',  ( -5.982172092127739482, 8.002286745614243912, -1.599625672291263179 ) ) ;
#128806 = FACE_OUTER_BOUND ( 'NONE', #191684, .T. ) ;
#128807 = CARTESIAN_POINT ( 'NONE',  ( -1.499999999999997780, 7.388542872122518368, -4.154462424328208670 ) ) ;
#128808 = CARTESIAN_POINT ( 'NONE',  ( 6.227749967195368441, 0.7672974224810541477, -1.865044430435198741 ) ) ;
#128809 = FILL_AREA_STYLE ('',( #61597 ) ) ;
#128810 = CARTESIAN_POINT ( 'NONE',  ( 4.891568528303794849, -1.987603774517988642, 0.8738605845971869623 ) ) ;
#128811 = CARTESIAN_POINT ( 'NONE',  ( 4.740742070742828496, 0.3150700179065483719, 1.798135100120237251 ) ) ;
#128812 = CARTESIAN_POINT ( 'NONE',  ( 1.621847549879054107, 1.933622029546874010, -0.3300716771732490895 ) ) ;
#128813 = CARTESIAN_POINT ( 'NONE',  ( 0.4744016597374626221, -2.101792896462660210, -0.2546084012580717704 ) ) ;
#128814 = CARTESIAN_POINT ( 'NONE',  ( 1.364683531249988535, 4.426041667008082214, 0.7879004041258500513 ) ) ;
#128815 = CARTESIAN_POINT ( 'NONE',  ( 3.999405481576134846, 7.808394548344907093, -0.08844146109573064463 ) ) ;
#128816 = CARTESIAN_POINT ( 'NONE',  ( 8.925345196497941558, 9.307324238869423283, 1.040834085586084257E-14 ) ) ;
#128817 = CARTESIAN_POINT ( 'NONE',  ( 2.860144583491229131, 0.7611018733697445526, -1.979373954265637892 ) ) ;
#128818 = CARTESIAN_POINT ( 'NONE',  ( -2.955314298098991266, 6.391691081183366485, 0.7216878364870317197 ) ) ;
#128819 = CARTESIAN_POINT ( 'NONE',  ( 5.112833325684902341, 7.058334528089427629, -1.443375672974078316 ) ) ;
#128820 = AXIS2_PLACEMENT_3D ( 'NONE', #61175, #193305, #194372 ) ;
#128821 = CARTESIAN_POINT ( 'NONE',  ( -3.755245360860919757, 7.324943987738961049, -0.7216878364870257245 ) ) ;
#128822 = CARTESIAN_POINT ( 'NONE',  ( 0.4442981077158770775, -0.9790059121952739973, 1.824179074426744762 ) ) ;
#128824 = CARTESIAN_POINT ( 'NONE',  ( -6.009258394948636914E-15, 13.71875000068279782, -1.732050807568875195 ) ) ;
#128823 = CARTESIAN_POINT ( 'NONE',  ( 6.983263157960330147, 7.052490050591996962, 2.551961896892048109 ) ) ;
#128826 = VERTEX_POINT ( 'NONE', #174972 ) ;
#128825 = CARTESIAN_POINT ( 'NONE',  ( 2.456000923045877027, -1.648014358291004733, -1.489564561520567487 ) ) ;
#128827 = CARTESIAN_POINT ( 'NONE',  ( 0.9502802867703894485, -2.080962668894706269, -0.9767702978288366200 ) ) ;
#128829 = CARTESIAN_POINT ( 'NONE',  ( 5.823111402427982419, -1.862227451873458728, -0.8870778100700682511 ) ) ;
#128828 = CARTESIAN_POINT ( 'NONE',  ( 2.672928840188529609, 6.270167413528593414, 0.000000000000000000 ) ) ;
#128831 = CARTESIAN_POINT ( 'NONE',  ( 3.475000000000000533, -2.274999999999999467, 0.000000000000000000 ) ) ;
#128830 = CARTESIAN_POINT ( 'NONE',  ( 6.052789233858158369, 6.026285292448116948, 0.000000000000000000 ) ) ;
#128832 = CARTESIAN_POINT ( 'NONE',  ( 6.387826650694035990, 7.481494509678370264, -1.199719254218452047 ) ) ;
#128833 = CARTESIAN_POINT ( 'NONE',  ( 0.1333542156527660338, 0.2446709926765543996, -2.080993637364982884 ) ) ;
#128834 = CARTESIAN_POINT ( 'NONE',  ( 5.267088776126935379, 1.772936381825638952, -0.4966186330585887210 ) ) ;
#128835 = CARTESIAN_POINT ( 'NONE',  ( 4.650610384687404952, 5.384465856012134566, 1.199719254218462483 ) ) ;
#128836 =( LENGTH_UNIT ( ) NAMED_UNIT ( * ) SI_UNIT ( .MILLI., .METRE. ) );
#128837 = CARTESIAN_POINT ( 'NONE',  ( 2.010387792931751516, 1.280683741330263858, -1.155484876777863379 ) ) ;
#128838 = CARTESIAN_POINT ( 'NONE',  ( 0.9367328597341374463, -1.586666764284098807, 1.244388658875786424 ) ) ;
#128839 = CARTESIAN_POINT ( 'NONE',  ( 2.338912275282720277, 0.6088908215152682990, -2.216548965993940801 ) ) ;
#128840 = CARTESIAN_POINT ( 'NONE',  ( -1.364683531250010295, 4.342708333674753618, 0.7879004041258379498 ) ) ;
#128841 = CARTESIAN_POINT ( 'NONE',  ( 2.302381833152538082, -2.261912932826372735, 0.05377845686085034466 ) ) ;
#128842 = CARTESIAN_POINT ( 'NONE',  ( 3.615936863914733124, -2.074906038012876763, 0.3600020511305370707 ) ) ;
#128843 = CARTESIAN_POINT ( 'NONE',  ( -4.659162064951642535, 5.464719159645540003, 1.199719254218452935 ) ) ;
#128844 = CARTESIAN_POINT ( 'NONE',  ( 2.706023412207391843, -0.6731984680253579878, -1.636901589742848051 ) ) ;
#128845 = CARTESIAN_POINT ( 'NONE',  ( 5.229694566569264680, 7.124396299129368337, 1.599625672291267398 ) ) ;
#128847 = CARTESIAN_POINT ( 'NONE',  ( 5.196947908113320302, 1.872795242347685463, 1.321741379092307600 ) ) ;
#128846 = CARTESIAN_POINT ( 'NONE',  ( 3.716343503477301802, 7.349834830783237294, -1.734723475976807094E-15 ) ) ;
#128848 = CARTESIAN_POINT ( 'NONE',  ( 4.206863059814883066, -0.3125640686512491384, 1.814249101404527220 ) ) ;
#128849 = CARTESIAN_POINT ( 'NONE',  ( -3.737243898861318137, 7.511868315313511069, 0.7998128361456341429 ) ) ;
#128850 = CARTESIAN_POINT ( 'NONE',  ( 5.626270559546814098, 7.587068290936515247, 1.443375672974062551 ) ) ;
#128851 = CARTESIAN_POINT ( 'NONE',  ( -0.7499999999999972244, 3.858333333333359594, -1.299038105676652011 ) ) ;
#128852 = AXIS2_PLACEMENT_3D ( 'NONE', #166434, #18025, #63608 ) ;
#128853 = CARTESIAN_POINT ( 'NONE',  ( 2.531617689938488791, -0.2033970545941807817, 2.110794199748195599 ) ) ;
#128854 = CARTESIAN_POINT ( 'NONE',  ( 4.769572470968366673, 1.260305947291120221, 1.792593939366843303 ) ) ;
#128855 = CARTESIAN_POINT ( 'NONE',  ( -3.588104209110990706, 7.337872010604796991, 1.040834085586084257E-14 ) ) ;
#128856 = CARTESIAN_POINT ( 'NONE',  ( 0.08369048095983153135, 7.010987279216816859, -1.999726996211172336 ) ) ;
#128857 = CARTESIAN_POINT ( 'NONE',  ( 5.009736938882257462, 7.905775019223336919, -1.089308093605208194 ) ) ;
#128858 = CARTESIAN_POINT ( 'NONE',  ( 1.364683531249988535, 4.405208333674754506, -0.7879004041258300672 ) ) ;
#128859 = CARTESIAN_POINT ( 'NONE',  ( 2.736843622788497132, 0.2362483484473417716, 1.911901653511848931 ) ) ;
#128860 = CARTESIAN_POINT ( 'NONE',  ( 0.6823417656249934904, 9.442708333674735499, 1.181850606188764807 ) ) ;
#128861 = CARTESIAN_POINT ( 'NONE',  ( -2.806174608348664723, 6.217694776474651519, 1.040834085586084257E-14 ) ) ;
#128862 = CARTESIAN_POINT ( 'NONE',  ( 6.117454236943913770, 1.763945953808215394, 1.176740244630887222 ) ) ;
#128863 = CARTESIAN_POINT ( 'NONE',  ( -6.346625304972878467, 7.537389289624049304, 1.082531754730548412 ) ) ;
#128864 = ORIENTED_EDGE ( 'NONE', *, *, #57277, .F. ) ;
#128866 = SURFACE_STYLE_FILL_AREA ( #193776 ) ;
#128865 = CARTESIAN_POINT ( 'NONE',  ( -5.316205630334268406, 6.335233002545657577, -1.082531754730549967 ) ) ;
#128867 = CARTESIAN_POINT ( 'NONE',  ( 3.005103603723342953, 6.657704637652544832, -0.7998128361456291469 ) ) ;
#128868 = CARTESIAN_POINT ( 'NONE',  ( 7.725699985795379199, -5.832912386296868590, -7.725699985795413838 ) ) ;
#128869 = CARTESIAN_POINT ( 'NONE',  ( 0.4019237886466884846, 11.20758545099816317, -1.499999999999994449 ) ) ;
#128870 = CARTESIAN_POINT ( 'NONE',  ( 0.08888683327021046354, 6.492044364012832247, -3.106763327641855810 ) ) ;
#128871 = CARTESIAN_POINT ( 'NONE',  ( -1.001543065824772872E-14, 4.384375000341417916, 1.575800808251672791 ) ) ;
#128872 = CARTESIAN_POINT ( 'NONE',  ( 2.032363155619838935, -1.554395792557780487, 0.7831100076771575491 ) ) ;
#128873 = DIRECTION ( 'NONE',  ( 0.000000000000000000, 1.000000000000000000, 0.000000000000000000 ) ) ;
#128874 = CARTESIAN_POINT ( 'NONE',  ( 0.6253529088778921885, 0.1960189665039281104, -1.952063659030292220 ) ) ;
#128875 = CARTESIAN_POINT ( 'NONE',  ( -0.6823417656250003738, 0.2802083336747515641, -1.181850606188749264 ) ) ;
#128876 = CARTESIAN_POINT ( 'NONE',  ( 2.295757763869426871, 5.519548059767960702, 0.4031905389056070765 ) ) ;
#128877 = EDGE_CURVE ( 'NONE', #40383, #190182, #72634, .T. ) ;
#128878 = CARTESIAN_POINT ( 'NONE',  ( 6.631704542599726082, -1.407888343591977121, -1.640466528430361670 ) ) ;
#128879 = CARTESIAN_POINT ( 'NONE',  ( -9.134442807305063639, 11.67993591332117376, 1.599625672291281386 ) ) ;
#128880 = CARTESIAN_POINT ( 'NONE',  ( -5.192409643909507544, 9.001635651295671892, 0.7216878364870458196 ) ) ;
#128881 = CARTESIAN_POINT ( 'NONE',  ( 5.366167234668930419, 1.061923416652654550, 1.882811416686725359 ) ) ;
#128883 = ORIENTED_EDGE ( 'NONE', *, *, #187231, .T. ) ;
#128882 = LINE ( 'NONE', #43309, #4904 ) ;
#128884 = CARTESIAN_POINT ( 'NONE',  ( -0.6823417656250212460, 3.801041667008085767, 1.181850606188767472 ) ) ;
#128885 = CARTESIAN_POINT ( 'NONE',  ( 0.5615140978009087736, 1.851110617189118734, -0.2680550677405246773 ) ) ;
#128886 = CARTESIAN_POINT ( 'NONE',  ( 6.555961055344926791, 1.506409351870329649, -0.8582156258899288348 ) ) ;
#128888 = CARTESIAN_POINT ( 'NONE',  ( 3.105210138592546798, -0.4252477525170209605, 2.149737936336936883 ) ) ;
#128887 = CARTESIAN_POINT ( 'NONE',  ( -5.157946788997579689E-14, 1.203125000341463746, 1.570758158831762286 ) ) ;
#128889 = CARTESIAN_POINT ( 'NONE',  ( 3.557953228543974777, 0.5631008447647236625, -2.237707790512387440 ) ) ;
#128890 = CARTESIAN_POINT ( 'NONE',  ( 5.677046966798700467, -0.04615325445976201785, -2.060428132270344381 ) ) ;
#128891 = CARTESIAN_POINT ( 'NONE',  ( 1.710778446297245958, -0.2380136870633246249, 1.927241887951787858 ) ) ;
#128892 = CARTESIAN_POINT ( 'NONE',  ( -6.900736999231456004, 8.113576589600553390, 1.082531754730549967 ) ) ;
#128893 = CARTESIAN_POINT ( 'NONE',  ( -0.2943368945748598420, -8.203192640252309431, -9.495705940876561613 ) ) ;
#128894 = CARTESIAN_POINT ( 'NONE',  ( 4.553055379497691568, 0.3652949536288411791, 2.088752307168060707 ) ) ;
#128895 = DIRECTION ( 'NONE',  ( -0.000000000000000000, 1.000000000000000000, -0.000000000000000000 ) ) ;
#128896 = CARTESIAN_POINT ( 'NONE',  ( 2.145157927413956944, 0.8647252629472859109, 1.821741647932619390 ) ) ;
#128897 = CARTESIAN_POINT ( 'NONE',  ( -5.626270559546828309, 7.587068290936515247, 1.443375672974064550 ) ) ;
#128898 = CARTESIAN_POINT ( 'NONE',  ( 4.102700518754747172, -0.6894086160392081108, -2.096397988278507096 ) ) ;
#128899 = DIRECTION ( 'NONE',  ( 1.016547956922408957E-15, 1.000000000000000000, -4.622230424712075819E-32 ) ) ;
#128900 = CARTESIAN_POINT ( 'NONE',  ( -3.343839487215291673, -3.074644732671757641, 0.8435610638829383889 ) ) ;
#128901 = DIRECTION ( 'NONE',  ( 0.000000000000000000, 1.000000000000000000, 0.000000000000000000 ) ) ;
#128902 = CARTESIAN_POINT ( 'NONE',  ( -6.237633190739009237, 9.434933268240943249, 1.199719254218452047 ) ) ;
#128904 = DIRECTION ( 'NONE',  ( 0.000000000000000000, 1.000000000000000000, 0.000000000000000000 ) ) ;
#128903 = CARTESIAN_POINT ( 'NONE',  ( -4.599258460307840579, 8.480642220064158465, 0.2485357878534207865 ) ) ;
#128905 = CARTESIAN_POINT ( 'NONE',  ( 1.594690046439222630, 8.741643652401167586, -2.463706593913769893 ) ) ;
#128906 = EDGE_LOOP ( 'NONE', ( #165784, #72537, #208188, #10904 ) ) ;
#128907 = CARTESIAN_POINT ( 'NONE',  ( 4.100502863055309533, -0.6448639507273239424, -1.957478828838697504 ) ) ;
#128908 = CARTESIAN_POINT ( 'NONE',  ( -7.553300976144787349, 8.945177572657957654, -1.082531754730549967 ) ) ;
#128909 = CARTESIAN_POINT ( 'NONE',  ( 0.1254057754173175943, 7.054063922337675763, -3.955400951015573874 ) ) ;
#128910 = CARTESIAN_POINT ( 'NONE',  ( -4.717347382551060342, 7.590990148696470818, 1.199719254218464037 ) ) ;
#128911 = CARTESIAN_POINT ( 'NONE',  ( -4.417564364067771088, 7.323841156470280112, 1.242459261498860323 ) ) ;
#128912 = CARTESIAN_POINT ( 'NONE',  ( 2.912765130361310018, -0.5885411476599323732, -1.932001019476004888 ) ) ;
#128913 = CARTESIAN_POINT ( 'NONE',  ( 1.499999999999989120, 1.275000000000019229, 0.000000000000000000 ) ) ;
#128915 = CARTESIAN_POINT ( 'NONE',  ( 8.920901888111989919, 11.43080484092926241, 1.443375672974076540 ) ) ;
#128914 = CARTESIAN_POINT ( 'NONE',  ( -5.652823702255029836, 5.559658838911111900, -0.7998128361456362523 ) ) ;
#128916 = CARTESIAN_POINT ( 'NONE',  ( 7.467843683028853263, 7.606905806488803101, 0.7998128361456341429 ) ) ;
#128917 = CARTESIAN_POINT ( 'NONE',  ( 2.922786580453646366, 1.940006684909411971, 0.6957959148722169251 ) ) ;
#128918 = CARTESIAN_POINT ( 'NONE',  ( 3.235000160576475992, 2.016597019841442240, -0.002811030766311505089 ) ) ;
#128919 = DIRECTION ( 'NONE',  ( 3.330669073875478989E-16, -3.540251991789410786E-16, -1.000000000000000000 ) ) ;
#128920 = CARTESIAN_POINT ( 'NONE',  ( 4.547870462380197765, 7.393267075163835855, 1.199719254218462483 ) ) ;
#128921 = CARTESIAN_POINT ( 'NONE',  ( 3.239470508323912146, 0.4852670486454255250, -1.957170429962351577 ) ) ;
#128922 = VECTOR ( 'NONE', #21689, 1000.000000000000000 ) ;
#128924 = ORIENTED_EDGE ( 'NONE', *, *, #141157, .F. ) ;
#128923 = CARTESIAN_POINT ( 'NONE',  ( -0.1332994001262414741, 7.096108761198731685, -2.115961662170576574 ) ) ;
#128925 = CARTESIAN_POINT ( 'NONE',  ( 3.022814370378481552, 2.006652721595225675, -0.1948103792988181704 ) ) ;
#128926 = CARTESIAN_POINT ( 'NONE',  ( 1.745803608711377075, 0.5764907460206626366, 1.748616612666432868 ) ) ;
#128927 = AXIS2_PLACEMENT_3D ( 'NONE', #42964, #175088, #26676 ) ;
#128928 = EDGE_CURVE ( 'NONE', #96195, #76877, #97863, .T. ) ;
#128929 = CARTESIAN_POINT ( 'NONE',  ( 6.498651167236064730, -0.5841124237929047336, -2.128106146270396071 ) ) ;
#128930 = CARTESIAN_POINT ( 'NONE',  ( 3.874598038455354665, 7.742391154831717692, -0.7998128361456362523 ) ) ;
#128931 = CARTESIAN_POINT ( 'NONE',  ( 2.161604200734370096, 0.3718190433680613749, -2.129227089361292791 ) ) ;
#128932 = CARTESIAN_POINT ( 'NONE',  ( -2.657034918598338180, 6.043698471765932112, -0.7216878364870267237 ) ) ;
#128933 = CARTESIAN_POINT ( 'NONE',  ( 4.997310516409209313, -0.3076690597460414733, 2.094731796426703152 ) ) ;
#128934 = DIRECTION ( 'NONE',  ( -1.276756478318932585E-15, 1.000000000000000000, -1.665334536937738262E-16 ) ) ;
#128935 = CARTESIAN_POINT ( 'NONE',  ( 1.586564105604048480, -0.2713065988851799393, -1.850747533123621391 ) ) ;
#128936 =( BOUNDED_CURVE ( )  B_SPLINE_CURVE ( 2, ( #56821, #75211, #143450, #60021, #174868 ),
 .UNSPECIFIED., .F., .T. ) 
 B_SPLINE_CURVE_WITH_KNOTS ( ( 3, 2, 3 ),
 ( 0.000000000000000000, 0.01041666666666666609, 0.01562500000000013531 ),
 .UNSPECIFIED. ) 
 CURVE ( )  GEOMETRIC_REPRESENTATION_ITEM ( )  RATIONAL_B_SPLINE_CURVE ( ( 1.000000000000000000, 0.8660254037844387076, 1.000000000000000000, 0.9330127018922176330, 0.9330127018922194093 ) ) 
 REPRESENTATION_ITEM ( '' )  );
#128937 = CARTESIAN_POINT ( 'NONE',  ( 4.909034519618480807, 1.714790629392642707, 0.9726076082038226378 ) ) ;
#128940 = ADVANCED_FACE ( 'NONE', ( #153368 ), #49, .T. ) ;
#128939 = CARTESIAN_POINT ( 'NONE',  ( 8.717529583462649612, 10.23316793787035195, 1.082531754730558626 ) ) ;
#128938 = CARTESIAN_POINT ( 'NONE',  ( -0.6823417656250003738, 2.967708333674754062, -1.181850606188749264 ) ) ;
#128942 = CARTESIAN_POINT ( 'NONE',  ( 5.795568699328918605, 1.593732954614892616, 1.376895199011922477 ) ) ;
#128941 = CARTESIAN_POINT ( 'NONE',  ( -6.256197817702116026, 9.386315656372753224, -1.199719254218440723 ) ) ;
#128943 = CARTESIAN_POINT ( 'NONE',  ( 5.045036709957831711, 4.903268083610561767, 0.3063280728123271568 ) ) ;
#128944 = CARTESIAN_POINT ( 'NONE',  ( 4.957477724091233995, 8.935474444748447098, -0.7998128361456281477 ) ) ;
#128945 = CARTESIAN_POINT ( 'NONE',  ( -5.201524489137236529, 9.220195670635433771, 0.7998128361456481317 ) ) ;
#128946 = CARTESIAN_POINT ( 'NONE',  ( 6.639320575229230137, 7.629137130509035636, 2.603262396134010892 ) ) ;
#128947 = CARTESIAN_POINT ( 'NONE',  ( 5.541858398712612654, 0.7996551022716179569, -1.802186847774432943 ) ) ;
#128948 = CARTESIAN_POINT ( 'NONE',  ( -0.1049925189658337810, -2.058569791948822392, -0.5088776734372552069 ) ) ;
#128949 = CARTESIAN_POINT ( 'NONE',  ( -0.7500000000000006661, 0.3895833340161539149, -1.299038105676652011 ) ) ;
#128950 = CARTESIAN_POINT ( 'NONE',  ( 4.617980755673473325, -2.263821322725892315, 0.4470779566097658475 ) ) ;
#128951 = CARTESIAN_POINT ( 'NONE',  ( 2.377848133335142222, -2.001750602163259174, 0.4968105773679451498 ) ) ;
#128952 = CARTESIAN_POINT ( 'NONE',  ( 7.782016984564060103, 9.141736572488651902, 1.082531754730558626 ) ) ;
#128953 = CARTESIAN_POINT ( 'NONE',  ( 6.201928923608456046, 6.200281597156833691, 0.7998128361456352531 ) ) ;
#128954 = CARTESIAN_POINT ( 'NONE',  ( 5.194709132691408549, 6.089524072008651423, 1.199719254218452935 ) ) ;
#128955 = CARTESIAN_POINT ( 'NONE',  ( -1.364683531250014514, 1.801041667008085767, -0.7879004041258289570 ) ) ;
#128956 = CARTESIAN_POINT ( 'NONE',  ( 3.902768115887398803, 5.646591783325653147, -1.599625672291269396 ) ) ;
#128957 = CARTESIAN_POINT ( 'NONE',  ( 4.975479186090847605, 7.788180902872553268, 1.082531754730558626 ) ) ;
#128958 = CARTESIAN_POINT ( 'NONE',  ( 4.299414767360295819, -1.890980460948383790, 1.066717558251949471 ) ) ;
#128959 = CARTESIAN_POINT ( 'NONE',  ( -3.137887434649874407, -0.8887487162373172156, -0.9976822016299863316 ) ) ;
#128961 = CARTESIAN_POINT ( 'NONE',  ( 3.579498943475650563, -0.9044721095569520086, 1.603693017070174864 ) ) ;
#128960 = CARTESIAN_POINT ( 'NONE',  ( -4.446711195602255806, 5.250546485366484717, -1.082531754730544860 ) ) ;
#128963 = CARTESIAN_POINT ( 'NONE',  ( -0.05425791151749961849, -7.744511198441866640, 9.500000000000131450 ) ) ;
#128962 = CARTESIAN_POINT ( 'NONE',  ( -1.364683531249997417, 4.259375000341424133, 1.214306433183764966E-14 ) ) ;
#128964 = CARTESIAN_POINT ( 'NONE',  ( 5.530878137806295669, -1.981686641427220286, 0.9361944923952856268 ) ) ;
#128965 = CARTESIAN_POINT ( 'NONE',  ( 1.500000000000065503, 6.071532165918824830E-15, 10.99818166789400742 ) ) ;
#128966 = CARTESIAN_POINT ( 'NONE',  ( 6.526273518496622295, 1.309208030111205900, -1.845092234498114658 ) ) ;
#128967 = EDGE_LOOP ( 'NONE', ( #61000, #111316, #20756, #43601 ) ) ;
#128968 = CARTESIAN_POINT ( 'NONE',  ( -5.140457058134151325, 6.683247392444177315, -1.432107399977754270 ) ) ;
#128969 = CARTESIAN_POINT ( 'NONE',  ( 4.628438946891473726, 8.448539137754004003, 0.3726521946380862427 ) ) ;
#128970 = PRODUCT_DEFINITION ( 'UNKNOWN', '', #125065, #35183 ) ;
#128971 = CARTESIAN_POINT ( 'NONE',  ( -5.980555156959541208, 7.110307450275150210, 1.082531754730549078 ) ) ;
#128972 = CARTESIAN_POINT ( 'NONE',  ( -0.04570195657714287013, 1.813436143228260855, 11.99992749206847975 ) ) ;
#128973 = CARTESIAN_POINT ( 'NONE',  ( 0.5843626980001519478, -0.2102794380555508547, -1.757238120818458649 ) ) ;
#128974 = CARTESIAN_POINT ( 'NONE',  ( 4.758451920691616266, 2.007841679651333422, 0.1459793341078066131 ) ) ;
#128975 = CARTESIAN_POINT ( 'NONE',  ( 6.979750152936881058, 7.037463354714830643, 0.7998128361456341429 ) ) ;
#128976 = CARTESIAN_POINT ( 'NONE',  ( 4.155375932019107488, -1.749630165425161143, -1.171798067238625229 ) ) ;
#128977 = CARTESIAN_POINT ( 'NONE',  ( 1.599098272587581748, -0.2325377738172547115, 1.901345697680896007 ) ) ;
#128978 = CARTESIAN_POINT ( 'NONE',  ( 2.510230996824538430, 6.080353262937265413, 0.000000000000000000 ) ) ;
#128979 = CARTESIAN_POINT ( 'NONE',  ( 3.666418788940009943, -0.7958718277518551654, -1.801768233320384605 ) ) ;
#128980 = CARTESIAN_POINT ( 'NONE',  ( 5.537369811128121988, -0.04535447194144863470, 2.019437878860441238 ) ) ;
#128981 = CARTESIAN_POINT ( 'NONE',  ( 2.131529507118444133, -1.219933349377068099, -1.418231869465089057 ) ) ;
#128982 = CARTESIAN_POINT ( 'NONE',  ( 1.943732651021431224, 1.350599318427040840, 1.423195245143428433 ) ) ;
#128985 = VERTEX_POINT ( 'NONE', #104629 ) ;
#128984 = CARTESIAN_POINT ( 'NONE',  ( 0.9317291061951762376, -1.865162313430932750, 0.4216105838140621342 ) ) ;
#128983 = CARTESIAN_POINT ( 'NONE',  ( 4.055083665587292607, -1.435586732866575010, -0.9558459365816800446 ) ) ;
#128987 = CARTESIAN_POINT ( 'NONE',  ( 5.178851490740196795, 7.065079377328788546, 1.443375672974062551 ) ) ;
#128986 = CARTESIAN_POINT ( 'NONE',  ( 0.8915962724085277902, 1.944627461026976034, -1.043433064090833140 ) ) ;
#128988 = CARTESIAN_POINT ( 'NONE',  ( -1.364683531250000748, 1.571875000341421691, 0.000000000000000000 ) ) ;
#128989 = CARTESIAN_POINT ( 'NONE',  ( 8.239604668803105270, 10.63595808506888396, -1.599625672291268286 ) ) ;
#128990 = CARTESIAN_POINT ( 'NONE',  ( 6.772336237553374438, -1.148929780121176414, 1.476827877338216632 ) ) ;
#128991 = CARTESIAN_POINT ( 'NONE',  ( -8.748013565000578140, 3.829536045110815579, -7.724821879577381090 ) ) ;
#128992 = CARTESIAN_POINT ( 'NONE',  ( -5.607123201593087636, 5.580137643357920396, -0.3617017252367187852 ) ) ;
#128993 = AXIS2_PLACEMENT_3D ( 'NONE', #187257, #38884, #58332 ) ;
#128994 = CARTESIAN_POINT ( 'NONE',  ( 6.842638490404138629, -2.029097751484234546, -0.4099019697717393163 ) ) ;
#128995 = AXIS2_PLACEMENT_3D ( 'NONE', #9651, #90932, #41119 ) ;
#128996 = CARTESIAN_POINT ( 'NONE',  ( 0.3970419974134197783, 0.3524218036512065111, 2.039982198586967943 ) ) ;
#128997 = CARTESIAN_POINT ( 'NONE',  ( 0.7499999999999885647, 1.566666666666688412, -1.299038105676652899 ) ) ;
#128998 = CARTESIAN_POINT ( 'NONE',  ( 4.774442650306744085, 8.721933525333202653, -0.7998128361456281477 ) ) ;
#128999 = CARTESIAN_POINT ( 'NONE',  ( -6.855619230004478482, 11.14997286831390788, -0.7998128361456291469 ) ) ;
#129000 = CARTESIAN_POINT ( 'NONE',  ( 5.017399365509065845, 8.011327138806002779, -1.199719254218450271 ) ) ;
#129001 = CARTESIAN_POINT ( 'NONE',  ( 5.988958055669808545, -2.013456733998910231, -0.6654305520411086805 ) ) ;
#129002 = CARTESIAN_POINT ( 'NONE',  ( 3.413620815590684199, 7.204584394822967752, 0.7998128361456281477 ) ) ;
#129003 = CARTESIAN_POINT ( 'NONE',  ( 1.364683531249988535, 2.863541667008082658, 0.7879004041258500513 ) ) ;
#129004 = ORIENTED_EDGE ( 'NONE', *, *, #60154, .T. ) ;
#129005 = CARTESIAN_POINT ( 'NONE',  ( 1.499999999999989120, 3.504166666666683749, 0.8660254037844524744 ) ) ;
#129007 = CARTESIAN_POINT ( 'NONE',  ( 3.602716132929354664, 5.226254793216122074, 1.599625672291267398 ) ) ;
#129006 = CARTESIAN_POINT ( 'NONE',  ( 6.373494408814909917, -0.2414686440028299685, 1.946897059556201848 ) ) ;
#129008 = CARTESIAN_POINT ( 'NONE',  ( 3.848982377512806696, -0.9961485462514391154, 1.752762419822328610 ) ) ;
#129009 = CARTESIAN_POINT ( 'NONE',  ( 3.327253086410830729, -1.454009962414861912, -1.247479002808443704 ) ) ;
#129010 = AXIS2_PLACEMENT_3D ( 'NONE', #32599, #164730, #16319 ) ;
#129011 = CARTESIAN_POINT ( 'NONE',  ( 1.593588134247824639, -0.7342643958434189599, 2.065040727587868830 ) ) ;
#129012 = DIRECTION ( 'NONE',  ( -0.6929666359396602360, 0.000000000000000000, 0.7209696536432518288 ) ) ;
#129013 = CARTESIAN_POINT ( 'NONE',  ( 1.499999999999987121, 0.2854166673494805684, 0.8660254037844524744 ) ) ;
#129014 = CARTESIAN_POINT ( 'NONE',  ( 5.572526294291941795, 0.8198877612898677336, 1.838878804361820274 ) ) ;
#129015 = CARTESIAN_POINT ( 'NONE',  ( -5.533699252672048985, 9.607732894759390518, -0.7998128361456231517 ) ) ;
#129017 = CARTESIAN_POINT ( 'NONE',  ( 6.134383104757832328, 0.6643169034818379171, 2.010352329694592655 ) ) ;
#129016 = CARTESIAN_POINT ( 'NONE',  ( -4.284013352238265959, 5.060732334775157604, -1.082531754730544860 ) ) ;
#129019 = EDGE_CURVE ( 'NONE', #183021, #146105, #170676, .T. ) ;
#129018 =( LENGTH_UNIT ( ) NAMED_UNIT ( * ) SI_UNIT ( .MILLI., .METRE. ) );
#129021 = CARTESIAN_POINT ( 'NONE',  ( -5.921879234118920365, 10.13088588310589699, 0.000000000000000000 ) ) ;
#129020 = CARTESIAN_POINT ( 'NONE',  ( 3.017214641935324071, -2.014214092474704731, 0.5601794093188486867 ) ) ;
#129023 = VERTEX_POINT ( 'NONE', #110020 ) ;
#129022 = CARTESIAN_POINT ( 'NONE',  ( 1.606044756371062920, -0.6162743471601249690, -1.611104689205801188 ) ) ;
#129024 = CARTESIAN_POINT ( 'NONE',  ( 5.150683391976684788, 2.089615912265533559, 0.3601871064465370087 ) ) ;
#129025 = CARTESIAN_POINT ( 'NONE',  ( 6.796715079152391148, 6.823922435299587974, 0.7998128361456341429 ) ) ;
#129026 = VECTOR ( 'NONE', #150837, 1000.000000000000000 ) ;
#129027 = CARTESIAN_POINT ( 'NONE',  ( -1.453605123272271094, 13.24045051524828942, -0.3701785320580647798 ) ) ;
#129028 = CARTESIAN_POINT ( 'NONE',  ( 1.224999999999982991, 0.8749999999999937828, -4.163336342344337027E-14 ) ) ;
#129029 = CARTESIAN_POINT ( 'NONE',  ( 6.717748655458900764, -7.473374494057228645, -6.717748655460318297 ) ) ;
#129030 = CARTESIAN_POINT ( 'NONE',  ( 6.144869935491714230, 8.192100896205568361, -1.599625672291262513 ) ) ;
#129031 = ORIENTED_EDGE ( 'NONE', *, *, #151935, .T. ) ;
#129033 =( BOUNDED_CURVE ( )  B_SPLINE_CURVE ( 2, ( #160906, #12503, #129555, #144697, #81779, #163048, #15693 ),
 .UNSPECIFIED., .F., .T. ) 
 B_SPLINE_CURVE_WITH_KNOTS ( ( 3, 2, 2, 3 ),
 ( 0.3392857142857143571, 0.3452380952380953438, 0.3511904761904763861, 0.3571428571428574283 ),
 .UNSPECIFIED. ) 
 CURVE ( )  GEOMETRIC_REPRESENTATION_ITEM ( )  RATIONAL_B_SPLINE_CURVE ( ( 0.9999999999999987788, 0.8660254037844399289, 1.000000000000000000, 0.8660254037844387076, 1.000000000000000000, 0.8660254037844324904, 1.000000000000006217 ) ) 
 REPRESENTATION_ITEM ( '' )  );
#129032 = CARTESIAN_POINT ( 'NONE',  ( -11.84668729410359411, 13.50620512324532818, -1.400000000000001688 ) ) ;
#129035 = CARTESIAN_POINT ( 'NONE',  ( 2.015983567491559381, -1.811083833189537806, 0.04518873659950343319 ) ) ;
#129034 = CARTESIAN_POINT ( 'NONE',  ( 6.703580607314123085, 6.785541894813420072, 0.000000000000000000 ) ) ;
#129036 = CARTESIAN_POINT ( 'NONE',  ( -6.184490626128011925, 10.36698949712469364, -0.7998128361456291469 ) ) ;
#129037 = EDGE_LOOP ( 'NONE', ( #108599, #31969 ) ) ;
#129038 = CARTESIAN_POINT ( 'NONE',  ( 4.376584659113025744, 4.000436945253625254, 0.7998128361456341429 ) ) ;
#129039 = EDGE_LOOP ( 'NONE', ( #59751, #163222, #134046, #995, #148660, #145517, #41016, #184332, #17992 ) ) ;
#129040 = CARTESIAN_POINT ( 'NONE',  ( 5.550083779947807550, 7.568460058062819407, -1.599625672291283607 ) ) ;
#129041 = CARTESIAN_POINT ( 'NONE',  ( 2.824650661615616620, 1.310593810787925362, -1.250744805450889618 ) ) ;
#129042 = CARTESIAN_POINT ( 'NONE',  ( 0.4153311931458965600, 3.780177299622912823, -0.4999999999999988343 ) ) ;
#129043 = FILL_AREA_STYLE ('',( #115953 ) ) ;
#129044 = CARTESIAN_POINT ( 'NONE',  ( 8.563946585326370098, 13.14302144952281814, 0.7998128361456462443 ) ) ;
#129045 = CARTESIAN_POINT ( 'NONE',  ( 4.677432586336220055, 6.849818891840005364, 1.226792522213099979 ) ) ;
#129046 = ORIENTED_EDGE ( 'NONE', *, *, #128138, .T. ) ;
#129047 = CARTESIAN_POINT ( 'NONE',  ( 4.228838981530287811, -1.735973604985484142, -0.6712095357626171044 ) ) ;
#129048 = EDGE_CURVE ( 'NONE', #138779, #128826, #192244, .T. ) ;
#129049 = CARTESIAN_POINT ( 'NONE',  ( 1.862754361789496160, -0.09592165986596230820, -1.913344494172765753 ) ) ;
#129050 = CARTESIAN_POINT ( 'NONE',  ( 0.2877648253245302379, -0.8656086203641421006, 1.607325130595547602 ) ) ;
#129051 = CARTESIAN_POINT ( 'NONE',  ( 1.499999999999996891, 11.64583333333333748, -0.8660254037844378194 ) ) ;
#129052 = CARTESIAN_POINT ( 'NONE',  ( -0.3642516066350167114, 3.313053037719472016, 1.968202613562980430 ) ) ;
#129053 = CARTESIAN_POINT ( 'NONE',  ( 4.597294405107005488, 8.370805622008914426, 0.1071034531749150143 ) ) ;
#129054 = FILL_AREA_STYLE ('',( #212320 ) ) ;
#129055 = CARTESIAN_POINT ( 'NONE',  ( -2.331639231870358930, 5.664070170583284103, -0.7216878364870267237 ) ) ;
#129056 = CARTESIAN_POINT ( 'NONE',  ( 7.076992996653421741, 10.23994701519558781, -1.082531754730537976 ) ) ;
#129057 = CARTESIAN_POINT ( 'NONE',  ( 4.557443512217212778, 1.579177641033597368, 1.176567834677658908 ) ) ;
#129058 = CARTESIAN_POINT ( 'NONE',  ( -4.554649539187067830, 7.401175998105142817, 1.199719254218464037 ) ) ;
#129060 = CARTESIAN_POINT ( 'NONE',  ( -0.1399997263889594112, -0.002789056014654289761, -2.000146600338557956 ) ) ;
#129059 = B_SPLINE_CURVE_WITH_KNOTS ( 'NONE', 3,
 ( #23018, #203903, #54483, #41456, #40381, #187667, #7845, #55549 ),
 .UNSPECIFIED., .F., .F.,
 ( 4, 2, 2, 4 ),
 ( 2.544396950891272413E-07, 0.0002984430161323578892, 0.0005966315925696265331, 0.001193008745444163604 ),
 .UNSPECIFIED. ) ;
#129061 = CARTESIAN_POINT ( 'NONE',  ( 0.09384556119819162379, -2.090229486699231032, -0.04899896570133810414 ) ) ;
#129062 = CARTESIAN_POINT ( 'NONE',  ( 0.000000000000000000, 0.9200000000000041478, 6.329999999999995630 ) ) ;
#129063 = CARTESIAN_POINT ( 'NONE',  ( 5.280268953417031952, -1.070192140894361099, 1.601580209743416860 ) ) ;
#129064 = CARTESIAN_POINT ( 'NONE',  ( -7.854251061018346469, 8.057714414143200443, -0.7998128361456291469 ) ) ;
#129065 = ADVANCED_FACE ( 'NONE', ( #92661 ), #193327, .T. ) ;
#129066 = CARTESIAN_POINT ( 'NONE',  ( 1.676486011727536418, -1.732352342712149440, -0.5761224636358779350 ) ) ;
#129067 = CARTESIAN_POINT ( 'NONE',  ( 2.297764732281985633, 1.706874461811638044, 1.398895601573101111 ) ) ;
#129068 = CARTESIAN_POINT ( 'NONE',  ( -6.205606397109380445, 6.952550393956807184, 0.8692890898145851919 ) ) ;
#129069 = CARTESIAN_POINT ( 'NONE',  ( -0.03509584499547176162, -1.534781374734139670, 1.140672443274578729 ) ) ;
#129070 = ORIENTED_EDGE ( 'NONE', *, *, #14168, .T. ) ;
#129071 = EDGE_LOOP ( 'NONE', ( #172940, #119000, #17552, #137753 ) ) ;
#129072 = CARTESIAN_POINT ( 'NONE',  ( 0.1507525579465497367, -0.4251589684514142653, -1.929747299214799483 ) ) ;
#129073 = CARTESIAN_POINT ( 'NONE',  ( 1.733828471206948496, 1.921180395534723528, 0.2831599317468564969 ) ) ;
#129074 = CARTESIAN_POINT ( 'NONE',  ( 1.141953626738337890, -0.04666616626641807014, -2.015725262716171695 ) ) ;
#129076 = CARTESIAN_POINT ( 'NONE',  ( 5.787920722453932854, -1.179413039982403433, -1.439513333959110852 ) ) ;
#129075 = CARTESIAN_POINT ( 'NONE',  ( -4.782994330570982555, 8.802186828966616972, 0.000000000000000000 ) ) ;
#129077 = CARTESIAN_POINT ( 'NONE',  ( 5.631432701629774051, 7.663367133358481631, 1.599625672291269396 ) ) ;
#129078 = CARTESIAN_POINT ( 'NONE',  ( 1.499999999999963141, 6.999999999999999112, -9.886859966642596476 ) ) ;
#129079 = FACE_OUTER_BOUND ( 'NONE', #198257, .T. ) ;
#129080 = CARTESIAN_POINT ( 'NONE',  ( -4.554649539187067830, 7.401175998105142817, 1.199719254218464037 ) ) ;
#129081 = CARTESIAN_POINT ( 'NONE',  ( -5.264308783856126439, 9.363720357799287797, -0.7998128361456362523 ) ) ;
#129082 = CARTESIAN_POINT ( 'NONE',  ( 1.909981697816802049, -1.036543071415759298, -1.930953618257096993 ) ) ;
#129083 = CARTESIAN_POINT ( 'NONE',  ( 4.256897045010922476, 5.029096643009940415, -1.082531754730548412 ) ) ;
#129084 = DIRECTION ( 'NONE',  ( -0.000000000000000000, -1.000000000000000000, -0.000000000000000000 ) ) ;
#129085 = DIRECTION ( 'NONE',  ( 1.276756478318909314E-15, -1.000000000000000000, 0.000000000000000000 ) ) ;
#129086 = CARTESIAN_POINT ( 'NONE',  ( 1.506192966688112422, -0.6554880476431452774, -1.704135612709246184 ) ) ;
#129087 = CARTESIAN_POINT ( 'NONE',  ( -3.216308754939891212, 4.775446185561722956, -1.599625672291262513 ) ) ;
#129088 = CARTESIAN_POINT ( 'NONE',  ( -2.930533758848195447, 6.570706485298192234, -0.7998128361456281477 ) ) ;
#129089 = CARTESIAN_POINT ( 'NONE',  ( -6.358822508390924888, 6.928531665952419871, -0.8607971499900844981 ) ) ;
#129090 = CARTESIAN_POINT ( 'NONE',  ( 6.609000000000053276, 6.037706995087852135, 2.494900065673964829 ) ) ;
#129091 = CARTESIAN_POINT ( 'NONE',  ( 8.432281472695482449, 11.92507992053172572, 1.199719254218450271 ) ) ;
#129092 = CIRCLE ( 'NONE', #35591, 0.07999999999999998779 ) ;
#129093 = CARTESIAN_POINT ( 'NONE',  ( 1.523919215901398783, -1.069746099203742418, -1.602010878309991559 ) ) ;
#129094 = CARTESIAN_POINT ( 'NONE',  ( 3.959774770350584561, -0.5736532364168048792, 1.875976257969473648 ) ) ;
#129095 = CARTESIAN_POINT ( 'NONE',  ( -6.503107236049161521, 10.73870887536603291, 0.7998128361456481317 ) ) ;
#129096 = CARTESIAN_POINT ( 'NONE',  ( 6.647575389402066826, 6.649926130590872120, 1.040834085586084257E-14 ) ) ;
#129097 = ADVANCED_FACE ( 'NONE', ( #63334 ), #87378, .T. ) ;
#129098 = CARTESIAN_POINT ( 'NONE',  ( 4.792620198997869174, 1.822056328612733145, -1.217503271791681163 ) ) ;
#129099 = CARTESIAN_POINT ( 'NONE',  ( 3.822509244049070887, 6.547012320444182798, -1.199719254218452047 ) ) ;
#129100 = CARTESIAN_POINT ( 'NONE',  ( 3.731357587288412159, 0.05568397596692271218, -2.069689236595618542 ) ) ;
#129102 = CARTESIAN_POINT ( 'NONE',  ( -1.402160292154681736E-14, 1.759375000341421469, -1.575800808251659024 ) ) ;
#129101 = DIRECTION ( 'NONE',  ( 0.000000000000000000, 0.000000000000000000, 1.000000000000000000 ) ) ;
#129103 = ORIENTED_EDGE ( 'NONE', *, *, #11410, .F. ) ;
#129104 = CARTESIAN_POINT ( 'NONE',  ( 3.868082235913085309, -0.2263641512248204812, -2.287543476887623051 ) ) ;
#129106 = ORIENTED_EDGE ( 'NONE', *, *, #88854, .T. ) ;
#129105 = CARTESIAN_POINT ( 'NONE',  ( 6.290620087060792009, 10.28288116830553101, -0.7216878364870267237 ) ) ;
#129108 = CARTESIAN_POINT ( 'NONE',  ( -3.285556943749998737, -0.4302083328553760744, 1.896917185911908499 ) ) ;
#129107 = CARTESIAN_POINT ( 'NONE',  ( 5.966997003790217136, 8.054858819212300958, -1.443375672974078761 ) ) ;
#129109 = CARTESIAN_POINT ( 'NONE',  ( 6.620655732516613767, 2.976578140159558128, 2.379908536877679559 ) ) ;
#129110 = CARTESIAN_POINT ( 'NONE',  ( -9.703135535010517287, 4.518467101586145063, -7.062303484189693670 ) ) ;
#129111 = CARTESIAN_POINT ( 'NONE',  ( 3.960829289611409898, 0.2367351755836170912, -1.927401316828970979 ) ) ;
#129112 = VERTEX_POINT ( 'NONE', #117476 ) ;
#129113 = FACE_OUTER_BOUND ( 'NONE', #161465, .T. ) ;
#129114 = CARTESIAN_POINT ( 'NONE',  ( 5.185773951807310489, 1.841398108398510480, -0.5159224025059682139 ) ) ;
#129115 = FILL_AREA_STYLE ('',( #164715 ) ) ;
#129116 = CARTESIAN_POINT ( 'NONE',  ( 6.686556848510641693, -1.692700875910668312, -0.3300756604382968362 ) ) ;
#129117 = CARTESIAN_POINT ( 'NONE',  ( 4.188685576152741064, 1.555700494002542067, -1.282988152656767911 ) ) ;
#129118 = CARTESIAN_POINT ( 'NONE',  ( -2.030969412801321816, 8.463209591663684250, 2.499999999999998668 ) ) ;
#129119 = CARTESIAN_POINT ( 'NONE',  ( 0.9618826090718561872, 0.4271145061440981272, -2.164990749644220447 ) ) ;
#129121 = CARTESIAN_POINT ( 'NONE',  ( -5.316205630334268406, 6.335233002545657577, -1.082531754730549967 ) ) ;
#129120 = CARTESIAN_POINT ( 'NONE',  ( -3.838381494955496187, 7.492212646896947881, -0.0007785181141982987826 ) ) ;
#129123 = CARTESIAN_POINT ( 'NONE',  ( 0.2855648877363594629, -0.8402267237041045611, 1.557686187855854554 ) ) ;
#129122 = CARTESIAN_POINT ( 'NONE',  ( 0.04111360010001801485, -1.617408405202691135, -1.324400026677017728 ) ) ;
#129124 = CARTESIAN_POINT ( 'NONE',  ( 6.029922689959810178, -1.701949372586025744, 1.081063231324945528 ) ) ;
#129126 = CARTESIAN_POINT ( 'NONE',  ( 3.275583346405244622, 1.454120551940318418, 1.771997285204220507 ) ) ;
#129125 = CARTESIAN_POINT ( 'NONE',  ( 4.386945222473598527, 7.275797305264619652, -1.199719254218452047 ) ) ;
#129127 = CARTESIAN_POINT ( 'NONE',  ( 1.499541640181512481, -0.6240335575410212998, -1.624780663456944385 ) ) ;
#129128 = VECTOR ( 'NONE', #101187, 1000.000000000000000 ) ;
#129129 = LINE ( 'NONE', #196174, #193992 ) ;
#129130 = CARTESIAN_POINT ( 'NONE',  ( 1.282125424323858898, -1.693001012030776353, 0.3732380902255887367 ) ) ;
#129131 = CARTESIAN_POINT ( 'NONE',  ( 1.360316468749963592, 1.317708333674712184, -0.7853790794158981292 ) ) ;
#129132 = CARTESIAN_POINT ( 'NONE',  ( -11.94650005372637835, 13.65102700337638275, -1.135399707157295435 ) ) ;
#129133 = CARTESIAN_POINT ( 'NONE',  ( 1.557326333469456481, 1.775469013113859074, -1.249449068179921518 ) ) ;
#129134 = CARTESIAN_POINT ( 'NONE',  ( 2.360564879530482330, -1.931125380751706810, -0.5807522007576990664 ) ) ;
#129135 = CARTESIAN_POINT ( 'NONE',  ( 5.437500000000002665, 1.451031289060892737, -1.451031289061332608 ) ) ;
#129136 = CARTESIAN_POINT ( 'NONE',  ( 0.7499999999999885647, 2.097916667349486453, -1.299038105676652899 ) ) ;
#129137 = CARTESIAN_POINT ( 'NONE',  ( 0.2176306489089273599, -1.889907718300526174, 0.3723054783561028369 ) ) ;
#129138 = CARTESIAN_POINT ( 'NONE',  ( 1.364683531249996529, 12.96354166700806410, 0.7879004041258405033 ) ) ;
#129139 = CARTESIAN_POINT ( 'NONE',  ( 3.199698422319953384, 2.006668028495290024, -0.9531968752462171013 ) ) ;
#129140 = ORIENTED_EDGE ( 'NONE', *, *, #109079, .F. ) ;
#129141 = CARTESIAN_POINT ( 'NONE',  ( 5.764827401431699805, 7.068052664419874453, 2.440105445505980519 ) ) ;
#129142 = CARTESIAN_POINT ( 'NONE',  ( 1.499999999999987566, -0.9749999999999827693, 0.000000000000000000 ) ) ;
#129143 = CARTESIAN_POINT ( 'NONE',  ( 7.239163954692881653, 10.53310948286200599, -1.199719254218441611 ) ) ;
#129144 = CARTESIAN_POINT ( 'NONE',  ( 6.983858524370772258, 9.241197259889668558, 1.443375672974063439 ) ) ;
#129145 = EDGE_CURVE ( 'NONE', #4671, #80885, #111452, .T. ) ;
#129146 = CARTESIAN_POINT ( 'NONE',  ( 5.214300491592821274, 1.611006010870178251, 0.6591642633846701571 ) ) ;
#129147 = CARTESIAN_POINT ( 'NONE',  ( 3.631260574587381829, 0.05062604155347744800, -1.961386756325018021 ) ) ;
#129149 = CARTESIAN_POINT ( 'NONE',  ( -4.907688418466881863, 8.669460888279271416, 0.7216878364870458196 ) ) ;
#129148 = CARTESIAN_POINT ( 'NONE',  ( 10.56143847536557878, 11.42402576412244386, 0.000000000000000000 ) ) ;
#129150 = CARTESIAN_POINT ( 'NONE',  ( -1.430949710260812413, 4.025263519208086116, 0.4689103363401336266 ) ) ;
#129151 = CARTESIAN_POINT ( 'NONE',  ( 4.833442251172010984, -2.071103420340114187, 0.9108926349224757413 ) ) ;
#129152 = AXIS2_PLACEMENT_3D ( 'NONE', #179635, #46438, #48575 ) ;
#129153 = CARTESIAN_POINT ( 'NONE',  ( 1.645062733043511027, -0.3006328960593112054, -2.040525779345269797 ) ) ;
#129154 = CARTESIAN_POINT ( 'NONE',  ( -5.831978632172702071, 9.955725504176825780, 0.7998128361456481317 ) ) ;
#129155 = CARTESIAN_POINT ( 'NONE',  ( 2.835161494786802461, 0.2760463380651246856, 2.245541603805699005 ) ) ;
#129156 = ORIENTED_EDGE ( 'NONE', *, *, #131609, .F. ) ;
#129157 = CARTESIAN_POINT ( 'NONE',  ( 1.499999999999987121, 1.535416667349486453, 0.8660254037844524744 ) ) ;
#129158 = CARTESIAN_POINT ( 'NONE',  ( 3.215925951850879816, -0.9189154559356220719, -1.629173103855706906 ) ) ;
#129159 = CARTESIAN_POINT ( 'NONE',  ( 2.056849044198369114, -1.066344721839644460, 1.367450411802049182 ) ) ;
#129160 = CARTESIAN_POINT ( 'NONE',  ( 6.023007056224171762, -2.064090639567913499, 0.7368321019862942300 ) ) ;
#129161 = CARTESIAN_POINT ( 'NONE',  ( 6.229535257468108433, -2.175718461381468405, 0.7693011637898824473 ) ) ;
#129162 = CARTESIAN_POINT ( 'NONE',  ( 4.452137864729129646, 2.161286467946467837, -0.05003489268536746859 ) ) ;
#129163 = CARTESIAN_POINT ( 'NONE',  ( 4.734287085814634644, 0.3336016870040105498, 1.912933106389144822 ) ) ;
#129164 = CARTESIAN_POINT ( 'NONE',  ( -3.511198595814942980, 5.119484333249288532, 1.443375672974064550 ) ) ;
#129165 = ADVANCED_FACE ( 'NONE', ( #1492 ), #197585, .F. ) ;
#129167 = ORIENTED_EDGE ( 'NONE', *, *, #41782, .T. ) ;
#129166 = CARTESIAN_POINT ( 'NONE',  ( 6.819622122755134797, -1.814287395386984691, 0.4549875680220638596 ) ) ;
#129168 = CARTESIAN_POINT ( 'NONE',  ( 4.139348914150634329, 7.410017372392475821, 0.7316189255667099323 ) ) ;
#129169 = CARTESIAN_POINT ( 'NONE',  ( -0.1341500063891595818, -0.1486117279969369209, -1.983907055413631992 ) ) ;
#129170 = DIRECTION ( 'NONE',  ( -1.000000000000000000, 0.000000000000000000, 0.000000000000000000 ) ) ;
#129171 = CARTESIAN_POINT ( 'NONE',  ( -3.160134022698144918, 2.806877976488492354, -2.466440901443690326 ) ) ;
#129173 = CARTESIAN_POINT ( 'NONE',  ( 5.889296118903345700, -0.7283762112263308941, -1.880435897373772258 ) ) ;
#129172 = COLOUR_RGB ( '', 0.31764706, 0.68627451, 0.89019608) ;
#129174 = CARTESIAN_POINT ( 'NONE',  ( -10.64045162862669081, 11.30828174301964140, -0.7998128361456221525 ) ) ;
#129175 = CARTESIAN_POINT ( 'NONE',  ( 7.609150525767641504, 9.900428251527500834, -1.599625672291262513 ) ) ;
#129176 = CARTESIAN_POINT ( 'NONE',  ( 2.878073747850912412, 6.579779482459851003, -0.7998128361456362523 ) ) ;
#129177 = CARTESIAN_POINT ( 'NONE',  ( 3.545350327189537687, -1.383302465072188792, -1.191577590537174158 ) ) ;
#129178 = CARTESIAN_POINT ( 'NONE',  ( 0.7499999999999920064, 5.233333333333353821, 1.299038105676669330 ) ) ;
#129179 = ORIENTED_EDGE ( 'NONE', *, *, #187231, .F. ) ;
#129180 = CARTESIAN_POINT ( 'NONE',  ( -5.926322542504884439, 6.086666852443364029, -0.7216878364870338292 ) ) ;
#129181 = CARTESIAN_POINT ( 'NONE',  ( 0.000000000000000000, -3.434374999522041616, -3.793834371823813001 ) ) ;
#129182 = CARTESIAN_POINT ( 'NONE',  ( -7.537443334193545397, 10.88110209227943770, -1.199719254218446718 ) ) ;
#129183 = CARTESIAN_POINT ( 'NONE',  ( 0.4397206748869232351, -1.916487937148562137, 0.6377882026268544280 ) ) ;
#129184 = CARTESIAN_POINT ( 'NONE',  ( 1.700013272279196963, 1.464590769506744161, 1.533662747278791816 ) ) ;
#129185 = AXIS2_PLACEMENT_3D ( 'NONE', #88049, #5690, #120628 ) ;
#129186 = CARTESIAN_POINT ( 'NONE',  ( -6.123442655227560927, 7.173046514967467147, 1.199719254218452047 ) ) ;
#129187 = CARTESIAN_POINT ( 'NONE',  ( 1.850234720775156605, -1.851392121210411634, -0.1886080954226591611 ) ) ;
#129188 = CARTESIAN_POINT ( 'NONE',  ( 4.059776932288224671, 6.823824623389866950, 1.199719254218462483 ) ) ;
#129189 = CARTESIAN_POINT ( 'NONE',  ( 6.807514186891733488, -0.4511856701074740683, 2.018123631040650068 ) ) ;
#129190 = CARTESIAN_POINT ( 'NONE',  ( 5.906875006520014182, -1.122496024291631755, -1.674889250513518446 ) ) ;
#129191 = ORIENTED_EDGE ( 'NONE', *, *, #164748, .T. ) ;
#129192 = ORIENTED_EDGE ( 'NONE', *, *, #199481, .T. ) ;
#129193 = ORIENTED_EDGE ( 'NONE', *, *, #48949, .F. ) ;
#129194 = CARTESIAN_POINT ( 'NONE',  ( -8.784793466650835825, 12.33634391347959713, 1.199719254218462483 ) ) ;
#129195 = CARTESIAN_POINT ( 'NONE',  ( 3.738726038629454074, 0.2694068579384528150, 1.805578518607708016 ) ) ;
#129198 = ORIENTED_EDGE ( 'NONE', *, *, #124471, .T. ) ;
#129197 = CARTESIAN_POINT ( 'NONE',  ( 3.475000000000000533, -2.945833333333332416, -2.006292185433951047 ) ) ;
#129196 = CARTESIAN_POINT ( 'NONE',  ( -5.601453741101424022, 6.564059448486966986, -1.199719254218453823 ) ) ;
#129199 = CARTESIAN_POINT ( 'NONE',  ( 6.013528089337225602, 7.174620582783560963, 1.187335689305318853 ) ) ;
#129200 = CARTESIAN_POINT ( 'NONE',  ( 6.679064532090532857, -0.9478974852125362505, -1.779352858464311016 ) ) ;
#129201 = CARTESIAN_POINT ( 'NONE',  ( 5.771403949166884040, 1.100151190403714452, 1.476150860297696932 ) ) ;
#129202 = CARTESIAN_POINT ( 'NONE',  ( -0.02319159430949970999, 4.096340798889516854, -2.366022381217198767 ) ) ;
#129203 = CARTESIAN_POINT ( 'NONE',  ( 2.983396891919448013, -0.1703749763015352803, -2.301462837838092135 ) ) ;
#129204 = CARTESIAN_POINT ( 'NONE',  ( 4.844006021832467646, 8.873367135438366304, 0.000000000000000000 ) ) ;
#129205 = CARTESIAN_POINT ( 'NONE',  ( 5.536455037250767930, 2.128579029500421438, 0.3755436860354774420 ) ) ;
#129206 = CARTESIAN_POINT ( 'NONE',  ( 8.606728586576791074, 8.935604860628076906, 0.7998128361456462443 ) ) ;
#129207 = CARTESIAN_POINT ( 'NONE',  ( 1.681094245561355560, 1.340559147886428271, 1.405378567840375403 ) ) ;
#129208 = CARTESIAN_POINT ( 'NONE',  ( -4.948889764188092677, 5.732458465429559169, 1.199719254218462483 ) ) ;
#129209 = ORIENTED_EDGE ( 'NONE', *, *, #204649, .F. ) ;
#129210 = CARTESIAN_POINT ( 'NONE',  ( 5.009243775243890973, 2.291699508649183592, 0.1762380284849179579 ) ) ;
#129211 = CARTESIAN_POINT ( 'NONE',  ( -4.161989969715274462, 4.726297878971393196, -2.420000000000000373 ) ) ;
#129212 = CARTESIAN_POINT ( 'NONE',  ( -3.709037541790315640, 6.484905011134099340, -1.199719254218450271 ) ) ;
#129213 = CARTESIAN_POINT ( 'NONE',  ( 5.084763247618332649, -0.2297073032716222263, -1.856415652357709778 ) ) ;
#129217 = EDGE_CURVE ( 'NONE', #194084, #94313, #50284, .T. ) ;
#129216 = CARTESIAN_POINT ( 'NONE',  ( -5.472651281771599763, 6.413789912602166687, 1.199719254218452935 ) ) ;
#129215 = CARTESIAN_POINT ( 'NONE',  ( 0.7499999999999885647, 0.8479166673494853423, -1.299038105676652899 ) ) ;
#129214 = CARTESIAN_POINT ( 'NONE',  ( 0.7735182334044669039, 0.3705173918269571431, -1.875978362188877036 ) ) ;
#129218 = CARTESIAN_POINT ( 'NONE',  ( 3.686314334879085663, -1.088174899301070253, 1.919869060924610293 ) ) ;
#129219 = CARTESIAN_POINT ( 'NONE',  ( 6.883263157960402445, 0.5924656843266817852, 1.899575500811432338 ) ) ;
#129220 = CARTESIAN_POINT ( 'NONE',  ( 4.539282502477016479, 4.190251095844947926, 0.7998128361456341429 ) ) ;
#129221 = CARTESIAN_POINT ( 'NONE',  ( 5.465345319640213972, 8.429967735338637524, -1.082531754730548412 ) ) ;
#129222 = CARTESIAN_POINT ( 'NONE',  ( -2.676845263694313637, 5.210404343363602919, -1.199719254218446718 ) ) ;
#129223 = CARTESIAN_POINT ( 'NONE',  ( -6.251718229232856139, 8.387033582228697881, -1.443375672974066548 ) ) ;
#129224 = CARTESIAN_POINT ( 'NONE',  ( 1.757037784194936725, -1.688679813833958709, -1.016973138862599102 ) ) ;
#129225 = EDGE_CURVE ( 'NONE', #62493, #22081, #83831, .T. ) ;
#129226 = CARTESIAN_POINT ( 'NONE',  ( 1.606910496583548786, -0.8321943236449917958, -2.152478949753482862 ) ) ;
#129227 = CARTESIAN_POINT ( 'NONE',  ( 2.119516022818414669, 0.3384452847540948550, -1.932298432780136244 ) ) ;
#129228 = CARTESIAN_POINT ( 'NONE',  ( 5.840703832811390050, -2.011083492259890360, -0.4572853040550031167 ) ) ;
#129229 = CARTESIAN_POINT ( 'NONE',  ( 4.365362273920244007, 6.116008624372160973, 1.443375672974062551 ) ) ;
#129230 = CARTESIAN_POINT ( 'NONE',  ( 4.355912491740495440, 8.303924683664389406, 0.000000000000000000 ) ) ;
#129231 = EDGE_LOOP ( 'NONE', ( #80186, #154470, #198935, #157613 ) ) ;
#129232 =( BOUNDED_SURFACE ( )  B_SPLINE_SURFACE ( 3, 2, ( 
 ( #106907, #172932, #140457 ),
 ( #28802, #162014, #48272 ),
 ( #49324, #212861, #47208 ),
 ( #94886, #13603, #14661 ),
 ( #97025, #132724, #148942 ),
 ( #179330, #163079, #80753 ) ),
 .UNSPECIFIED., .F., .F., .T. ) 
 B_SPLINE_SURFACE_WITH_KNOTS ( ( 4, 2, 4 ),
 ( 3, 3 ),
 ( 0.000000000000000000, 0.0003766405729503176413, 0.0007532811459006352826 ),
 ( 0.000000000000000000, 1.000000000000000000 ),
 .UNSPECIFIED. ) 
 GEOMETRIC_REPRESENTATION_ITEM ( )  RATIONAL_B_SPLINE_SURFACE ( (
 ( 1.000000000000000000, 0.7071067811865551223, 1.000000000000000000),
 ( 1.000000000000000000, 0.7211294902953119257, 1.000000000000000000),
 ( 1.000000000000000000, 0.7311181975231312302, 1.000000000000000000),
 ( 1.000000000000000000, 0.7429553055060466038, 1.000000000000000000),
 ( 1.000000000000000000, 0.7451698531059031128, 1.000000000000000000),
 ( 1.000000000000000000, 0.7452309222763021657, 1.000000000000000000) ) ) 
 REPRESENTATION_ITEM ( '' )  SURFACE ( )  );
#129233 = CARTESIAN_POINT ( 'NONE',  ( 0.4019237886466778820, 10.07366454968462932, 1.500000000000001554 ) ) ;
#129234 = CARTESIAN_POINT ( 'NONE',  ( -1.737499999999997824, -1.341666666666668117, 3.009438278150925683 ) ) ;
#129235 = CARTESIAN_POINT ( 'NONE',  ( 10.24726517383036928, 10.84956421242393887, 0.000000000000000000 ) ) ;
#129236 = CARTESIAN_POINT ( 'NONE',  ( 0.8663802385432646247, -2.160743160283730813, 0.2111063225179575509 ) ) ;
#129238 = CARTESIAN_POINT ( 'NONE',  ( -1.500000000000015099, 12.22916666666666607, -0.8660254037844309360 ) ) ;
#129237 = FACE_OUTER_BOUND ( 'NONE', #162665, .T. ) ;
#129239 = CARTESIAN_POINT ( 'NONE',  ( -1.889151116980601453, 3.755413325228997401, 0.3999999999999940270 ) ) ;
#129240 = CARTESIAN_POINT ( 'NONE',  ( -1.499999999999930278, -6.071532165918824830E-15, 10.99818166789402696 ) ) ;
#129241 = CARTESIAN_POINT ( 'NONE',  ( 2.899504437521780442, -0.5904213222340527478, 1.774967144274109287 ) ) ;
#129242 = CARTESIAN_POINT ( 'NONE',  ( 6.925078400183550364, -0.007619068086212391067, 2.144148427808051594 ) ) ;
#129244 = CARTESIAN_POINT ( 'NONE',  ( 6.827182134110233669, 2.063332311267600971, 2.217821918593851027 ) ) ;
#129243 = CARTESIAN_POINT ( 'NONE',  ( 0.07735805125222078305, -0.0005418671161615954465, -2.088975025666544472 ) ) ;
#129245 = CARTESIAN_POINT ( 'NONE',  ( -1.364683531250000748, -0.9906249996585805295, 0.000000000000000000 ) ) ;
#129246 = CARTESIAN_POINT ( 'NONE',  ( 2.121601645288184290, -0.4173985973947492711, 1.866012167355892926 ) ) ;
#129247 = VECTOR ( 'NONE', #5158, 1000.000000000000000 ) ;
#129248 = CARTESIAN_POINT ( 'NONE',  ( 3.748697311245871688, -1.446992627045262214, 1.018796548582428185 ) ) ;
#129249 = CARTESIAN_POINT ( 'NONE',  ( 1.699719973799845185, 1.319605273547658220, 1.384218846220357291 ) ) ;
#129250 = AXIS2_PLACEMENT_3D ( 'NONE', #189062, #185842, #4938 ) ;
#129251 = CARTESIAN_POINT ( 'NONE',  ( -5.311043488251275591, 7.219303374425030562, -1.599625672291256295 ) ) ;
#129253 = CARTESIAN_POINT ( 'NONE',  ( 5.712480180419416520, 1.847460191615752700, 0.5061846876120765781 ) ) ;
#129252 = SURFACE_SIDE_STYLE ('',( #79334 ) ) ;
#129254 = LINE ( 'NONE', #96689, #70848 ) ;
#129255 = CARTESIAN_POINT ( 'NONE',  ( 0.2564123431100414074, -2.069877475643782994, -0.05227228806716639753 ) ) ;
#129256 = CARTESIAN_POINT ( 'NONE',  ( -1.201851678989727383E-14, 4.587500000000025224, -1.732050807568863648 ) ) ;
#129257 = CARTESIAN_POINT ( 'NONE',  ( 2.250376613284802207, 0.9954810856505689198, -1.872389709364124188 ) ) ;
#129258 = CARTESIAN_POINT ( 'NONE',  ( 4.733189744967194024, -1.710186631362722531, 0.7584244158565585092 ) ) ;
#129260 = VERTEX_POINT ( 'NONE', #167233 ) ;
#129259 = CARTESIAN_POINT ( 'NONE',  ( 1.945663734523142230, 0.6997465788082489757, -1.686465609443507763 ) ) ;
#129262 = CARTESIAN_POINT ( 'NONE',  ( 4.784634885068531851, 8.146353749921887655, 0.8039021629790907841 ) ) ;
#129261 = CARTESIAN_POINT ( 'NONE',  ( 4.916741810085082598, 1.523553907054091328, -1.596827639139485777 ) ) ;
#129263 = CARTESIAN_POINT ( 'NONE',  ( 1.364683531249986537, -0.8864583329919110133, 0.7879004041258500513 ) ) ;
#129264 = CARTESIAN_POINT ( 'NONE',  ( 1.346217686498082378, -0.9293675016086970775, 1.841534056632480265 ) ) ;
#129265 = CARTESIAN_POINT ( 'NONE',  ( 6.205881626753210867, 8.263281202677319470, 1.599625672291281386 ) ) ;
#129266 = CARTESIAN_POINT ( 'NONE',  ( -8.474009703741204547, 9.845098394908269768, -1.199719254218446718 ) ) ;
#129267 = CARTESIAN_POINT ( 'NONE',  ( 0.000000000000000000, 3.499999999999989342, 0.000000000000000000 ) ) ;
#129268 = DIRECTION ( 'NONE',  ( 0.000000000000000000, -1.000000000000000000, 0.000000000000000000 ) ) ;
#129269 = CARTESIAN_POINT ( 'NONE',  ( 0.1753634416057498202, 0.7014533214223102053, -2.226873008360684913 ) ) ;
#129270 = ORIENTED_EDGE ( 'NONE', *, *, #20366, .F. ) ;
#129271 = CARTESIAN_POINT ( 'NONE',  ( 3.842288295254093100, -1.023014542950370975, 1.799900136785845817 ) ) ;
#129272 = CARTESIAN_POINT ( 'NONE',  ( -0.6823417656250246877, -0.8864583329919115684, 1.181850606188755259 ) ) ;
#129273 = CARTESIAN_POINT ( 'NONE',  ( 2.688937055384227115, -0.3666181952855402382, -2.130111032054008646 ) ) ;
#129274 = CARTESIAN_POINT ( 'NONE',  ( -6.152945810502786550, 6.988564382810744213, -0.9301526061148736035 ) ) ;
#129275 = CARTESIAN_POINT ( 'NONE',  ( 1.787766293494430725, 1.931992495155916867, -0.5885693585916639270 ) ) ;
#129276 = CARTESIAN_POINT ( 'NONE',  ( 6.720655732516647163, -0.007268404184145297979, 2.273772995263834140 ) ) ;
#129277 = VERTEX_POINT ( 'NONE', #166156 ) ;
#129279 = CARTESIAN_POINT ( 'NONE',  ( 7.456621297836072415, 9.722477485607340597, 1.443375672974076540 ) ) ;
#129278 = CARTESIAN_POINT ( 'NONE',  ( -1.737499999999997824, -1.341666666666668117, 3.009438278150925683 ) ) ;
#129280 = CARTESIAN_POINT ( 'NONE',  ( -6.583366107887490770, 9.838288338247510367, 1.199719254218452935 ) ) ;
#129281 = CARTESIAN_POINT ( 'NONE',  ( 1.305875433988498813, -1.124247956386617009, -1.673852571057245830 ) ) ;
#129282 = CARTESIAN_POINT ( 'NONE',  ( 5.513277522340928272, -2.138352208816508782, 0.4792397250529822905 ) ) ;
#129283 = CARTESIAN_POINT ( 'NONE',  ( -1.201851678989727383E-14, 4.118750000682818602, -1.732050807568863648 ) ) ;
#129284 = CARTESIAN_POINT ( 'NONE',  ( 4.500206361630255003, -0.8965733778899236395, 1.689174240301967389 ) ) ;
#129285 = CARTESIAN_POINT ( 'NONE',  ( -2.740719608256871442, 6.349256642941639051, 0.7998128361456341429 ) ) ;
#129286 = CARTESIAN_POINT ( 'NONE',  ( 4.799223189113185128, 8.542918120699967588, 1.040834085586084257E-14 ) ) ;
#129288 = CARTESIAN_POINT ( 'NONE',  ( 2.425407844734633223, -1.496065234337567329, -1.352141214786584777 ) ) ;
#129287 = CARTESIAN_POINT ( 'NONE',  ( -8.581948047326017459, 11.99572790764693409, 1.082531754730558626 ) ) ;
#129289 = CARTESIAN_POINT ( 'NONE',  ( -1.364683531250014514, 11.90104166700806587, -0.7879004041258335089 ) ) ;
#129290 = CARTESIAN_POINT ( 'NONE',  ( -5.004894982100124068, 5.868074229652107121, 1.199719254218452935 ) ) ;
#129291 = CARTESIAN_POINT ( 'NONE',  ( 5.579022813628022881, -0.04626586813367798007, -1.724316369773688962 ) ) ;
#129292 = CARTESIAN_POINT ( 'NONE',  ( -0.1394461523061377994, 7.629137130509062281, -2.880276239818948536 ) ) ;
#129293 = CARTESIAN_POINT ( 'NONE',  ( 4.220665892555866883, 3.818531717603609987, -0.7998128361456211532 ) ) ;
#129294 = CARTESIAN_POINT ( 'NONE',  ( 0.7499999999999920064, 4.733333333333352932, 1.299038105676669330 ) ) ;
#129295 = CARTESIAN_POINT ( 'NONE',  ( 5.190073875932979419, 4.949507698210251938, 0.7998128361456341429 ) ) ;
#129296 = CARTESIAN_POINT ( 'NONE',  ( 0.000000000000000000, 1.000000000000000888, 0.000000000000000000 ) ) ;
#129297 = EDGE_LOOP ( 'NONE', ( #55009, #10941 ) ) ;
#129298 = CARTESIAN_POINT ( 'NONE',  ( 0.8310238944931707117, -1.948087850137161459, -0.7009411469260096172 ) ) ;
#129299 = ORIENTED_EDGE ( 'NONE', *, *, #186296, .F. ) ;
#129300 = CARTESIAN_POINT ( 'NONE',  ( 4.582537834466095639, -1.179681096148448738, 1.374793604838970396 ) ) ;
#129301 = CARTESIAN_POINT ( 'NONE',  ( 4.878955176071345434, 6.785476686873604280, -1.599625672291269396 ) ) ;
#129302 = DIRECTION ( 'NONE',  ( 0.000000000000000000, 0.000000000000000000, 1.000000000000000000 ) ) ;
#129303 = CARTESIAN_POINT ( 'NONE',  ( 6.322923312362423331, 1.337123347216003788, -1.222299563558794766 ) ) ;
#129304 = CARTESIAN_POINT ( 'NONE',  ( 6.685579144870162693, 6.972466221869550118, -0.7216878364870458196 ) ) ;
#129305 = CARTESIAN_POINT ( 'NONE',  ( 0.6823417656249899377, 3.238541667008085323, -1.181850606188754593 ) ) ;
#129306 = CARTESIAN_POINT ( 'NONE',  ( 3.011879173929287834, -1.080601074572758558, -1.906429682232862799 ) ) ;
#129307 = ORIENTED_EDGE ( 'NONE', *, *, #157223, .T. ) ;
#129309 = CARTESIAN_POINT ( 'NONE',  ( 9.185812768458653466, 10.67553530374532045, 1.199719254218453823 ) ) ;
#129308 = CARTESIAN_POINT ( 'NONE',  ( 0.1331565106231328843, 0.003911343561965873426, -1.946049565259087455 ) ) ;
#129310 = TOROIDAL_SURFACE ( 'NONE', #125894, 11.92000000000000171, 0.08000000000000000167 ) ;
#129311 = CARTESIAN_POINT ( 'NONE',  ( 5.237857731762096236, 1.913213232725724966, -0.09853679971996709419 ) ) ;
#129312 = AXIS2_PLACEMENT_3D ( 'NONE', #46974, #30718, #212633 ) ;
#129313 = DIRECTION ( 'NONE',  ( 0.000000000000000000, 1.000000000000000000, 0.000000000000000000 ) ) ;
#129314 =( NAMED_UNIT ( * ) SI_UNIT ( $, .STERADIAN. ) SOLID_ANGLE_UNIT ( ) );
#129315 = CARTESIAN_POINT ( 'NONE',  ( -0.6823417656250246877, -0.6989583329919113464, 1.181850606188755259 ) ) ;
#129316 = VECTOR ( 'NONE', #75865, 1000.000000000000000 ) ;
#129317 = CARTESIAN_POINT ( 'NONE',  ( 3.877268743828258479, 7.467304601200877023, 0.7216878364870298324 ) ) ;
#129318 = CARTESIAN_POINT ( 'NONE',  ( -9.517460647113315630, 10.20605163116143821, 0.7216878364870438212 ) ) ;
#129319 = CARTESIAN_POINT ( 'NONE',  ( 1.674925575805393585, -2.052671086741376882, -0.6780288057936025847 ) ) ;
#129320 = CARTESIAN_POINT ( 'NONE',  ( -5.255720823952942489, 6.160704378480398979, -1.199719254218453823 ) ) ;
#129321 = CARTESIAN_POINT ( 'NONE',  ( 4.848976215542928792, 5.686169002002086970, 1.199719254218452047 ) ) ;
#129322 = CARTESIAN_POINT ( 'NONE',  ( 1.623764174509664260, -1.011042645414115260, -1.519837739365454743 ) ) ;
#129323 = CARTESIAN_POINT ( 'NONE',  ( -2.930533758848195447, 6.570706485298192234, -0.7998128361456281477 ) ) ;
#129324 = CARTESIAN_POINT ( 'NONE',  ( 5.086841682847768276, -0.2248377094848166835, -1.811598703993194670 ) ) ;
#129325 = CARTESIAN_POINT ( 'NONE',  ( 9.416996651545288088, 12.55534501603134778, -8.859730546806567020 ) ) ;
#129326 = CARTESIAN_POINT ( 'NONE',  ( 2.900541297466651347, -1.884798985816903860, -0.3226963764228693576 ) ) ;
#129327 = ORIENTED_EDGE ( 'NONE', *, *, #17510, .T. ) ;
#129328 = CARTESIAN_POINT ( 'NONE',  ( 3.473067387030086994, 1.779531822584624834, 0.8443681024216052045 ) ) ;
#129329 = ORIENTED_EDGE ( 'NONE', *, *, #44272, .T. ) ;
#129330 = CARTESIAN_POINT ( 'NONE',  ( 5.231954969198427285, 1.913977456902911767, 0.3281912247276967398 ) ) ;
#129331 = ORIENTED_EDGE ( 'NONE', *, *, #194628, .T. ) ;
#129332 = CARTESIAN_POINT ( 'NONE',  ( -7.584860592202423035, 7.813701877183096833, -0.7998128361456362523 ) ) ;
#129334 = CARTESIAN_POINT ( 'NONE',  ( 5.379186226027963258, -1.918017450862268714, -0.9047448674902383026 ) ) ;
#129333 = CARTESIAN_POINT ( 'NONE',  ( 5.332099551924443404, 9.442809587212341427, 0.000000000000000000 ) ) ;
#129335 = CARTESIAN_POINT ( 'NONE',  ( -3.147653791585730776, 8.919999999999991047, -2.500000000000000444 ) ) ;
#129336 = CARTESIAN_POINT ( 'NONE',  ( 3.193911838225035105, 1.215006091714765368, 1.476655219734591906 ) ) ;
#129337 = CARTESIAN_POINT ( 'NONE',  ( 5.250185332887272516, 6.604911474350376288, -1.376424501724478944 ) ) ;
#129338 = ORIENTED_EDGE ( 'NONE', *, *, #127070, .F. ) ;
#129339 = CARTESIAN_POINT ( 'NONE',  ( 0.2533207856364183552, -1.770817270756098960, 1.316655756711228253 ) ) ;
#129340 = CARTESIAN_POINT ( 'NONE',  ( 4.828775420069912450, 1.386532772215205878, -1.459704157296830784 ) ) ;
#129341 = CARTESIAN_POINT ( 'NONE',  ( -4.229856262585510507, 7.526865594461044751, -1.029777601131131037 ) ) ;
#129342 = CARTESIAN_POINT ( 'NONE',  ( 5.356004772612798170, 1.823420152956479523, -0.09349780940721279243 ) ) ;
#129343 = CARTESIAN_POINT ( 'NONE',  ( 1.258353326579707776, -2.070544811992577561, -0.001879966208345739808 ) ) ;
#129344 = CARTESIAN_POINT ( 'NONE',  ( -7.483737605063437215, 10.71448239167390604, 1.082531754730549967 ) ) ;
#129345 = CARTESIAN_POINT ( 'NONE',  ( -6.596192096975760144, 6.770415987340496322, 0.2575442448356154990 ) ) ;
#129346 = CARTESIAN_POINT ( 'NONE',  ( -0.3282377607281349308, 1.511164550367446235, -1.225000000000023848 ) ) ;
#129347 = CARTESIAN_POINT ( 'NONE',  ( 6.825078400183573812, 0.002648415797040087893, 1.855566311045192540 ) ) ;
#129348 = CARTESIAN_POINT ( 'NONE',  ( 6.636879889089462026, 7.701780277814560982, -1.199719254218446718 ) ) ;
#129349 = CARTESIAN_POINT ( 'NONE',  ( 4.566398809704347528, 4.221886787610169556, -0.7998128361456211532 ) ) ;
#129350 = CARTESIAN_POINT ( 'NONE',  ( 1.364683531249996529, 9.776041667008064096, 0.7879004041258405033 ) ) ;
#129351 = CARTESIAN_POINT ( 'NONE',  ( -3.262708522383007903, 6.958243709422141876, 1.040834085586084257E-14 ) ) ;
#129353 = CARTESIAN_POINT ( 'NONE',  ( -4.624739795592948788, 5.528522862014106920, -1.082531754730549967 ) ) ;
#129352 = CARTESIAN_POINT ( 'NONE',  ( -11.97297122925984958, 11.29874920673088390, -0.8121202983519461016 ) ) ;
#129354 = EDGE_CURVE ( 'NONE', #116379, #172448, #62292, .T. ) ;
#129355 = CARTESIAN_POINT ( 'NONE',  ( -5.066996723205291708, 6.934582148538044777, 1.599625672291267398 ) ) ;
#129356 = CARTESIAN_POINT ( 'NONE',  ( 1.797802452481820135, -1.496673605676283714, -1.430578824989765518 ) ) ;
#129357 = CARTESIAN_POINT ( 'NONE',  ( 2.355205625472241771, 0.1007552864207492405, -2.114937101796029673 ) ) ;
#129358 = CARTESIAN_POINT ( 'NONE',  ( 8.239604668803105270, 10.63595808506888396, -1.599625672291268286 ) ) ;
#129359 = CARTESIAN_POINT ( 'NONE',  ( -5.408618258607211793, 6.146265696677264856, -1.009999807746956524 ) ) ;
#129360 = CARTESIAN_POINT ( 'NONE',  ( 0.7429342955292950190, -0.2353911671746557188, -1.955230025236649682 ) ) ;
#129361 = CARTESIAN_POINT ( 'NONE',  ( 4.058723290341089474, 7.748532961531467755, 0.5319316551511514835 ) ) ;
#129362 = CARTESIAN_POINT ( 'NONE',  ( 5.341549334104194635, 6.294524313618772737, 1.082531754730558626 ) ) ;
#129364 = DIRECTION ( 'NONE',  ( 0.000000000000000000, 1.000000000000000000, 0.000000000000000000 ) ) ;
#129363 = CARTESIAN_POINT ( 'NONE',  ( 3.475000000000000533, -3.325000000000001510, 0.000000000000000000 ) ) ;
#129365 = CARTESIAN_POINT ( 'NONE',  ( 2.677988851928223557, -1.177355775514120850, 1.966668201240986402 ) ) ;
#129366 = CARTESIAN_POINT ( 'NONE',  ( 1.224926655537651676, -0.04696546880481740349, 1.825250005322680780 ) ) ;
#129367 = CARTESIAN_POINT ( 'NONE',  ( 2.004032382285144021, -0.8144628449315849394, 1.730399521388835460 ) ) ;
#129368 = CARTESIAN_POINT ( 'NONE',  ( 5.020262018810099924, 9.078999131912302900, 0.7998128361456331437 ) ) ;
#129369 = CARTESIAN_POINT ( 'NONE',  ( 5.951666246274784910, 9.887435020721849099, 0.7216878364870438212 ) ) ;
#129370 = CARTESIAN_POINT ( 'NONE',  ( 2.039316462420410758, 0.004210374635823382894, 2.013376229890501357 ) ) ;
#129371 = CARTESIAN_POINT ( 'NONE',  ( 2.026150138982992566, 1.004015975608811173, 1.685199498757394831 ) ) ;
#129372 = CARTESIAN_POINT ( 'NONE',  ( -10.13202086811422475, 10.71511252242175161, -0.7998128361456291469 ) ) ;
#129373 = CARTESIAN_POINT ( 'NONE',  ( -6.632963465583701534, 8.761543347979550589, -1.599625672291263179 ) ) ;
#129374 = CARTESIAN_POINT ( 'NONE',  ( -11.55950211276791428, 9.719999999999998863, -3.221476510067114329 ) ) ;
#129376 = CARTESIAN_POINT ( 'NONE',  ( 3.256490041505883504, -1.340903482672378466, 1.155240514129013407 ) ) ;
#129375 = CARTESIAN_POINT ( 'NONE',  ( 5.226549702048478352, 0.1529751191454275516, 2.085101625929087099 ) ) ;
#129377 = CARTESIAN_POINT ( 'NONE',  ( 0.3263184169966897308, 15.00000000000058265, 11.67999999558625213 ) ) ;
#129379 = CARTESIAN_POINT ( 'NONE',  ( 6.228533256425053288, 0.2185279184554402288, 2.281841813635554495 ) ) ;
#129378 = CARTESIAN_POINT ( 'NONE',  ( 1.495221130952435029, 8.717880658893497170, -2.557745341056325117 ) ) ;
#129380 = CARTESIAN_POINT ( 'NONE',  ( 4.558407276396470920, -1.556374654738747587, -0.7788941851257675797 ) ) ;
#129381 = CARTESIAN_POINT ( 'NONE',  ( 9.402743226277308963, 10.92862083786708816, -1.199719254218446718 ) ) ;
#129382 = CARTESIAN_POINT ( 'NONE',  ( -1.201851678989727383E-14, 4.087500000000022560, -1.732050807568863648 ) ) ;
#129383 = CARTESIAN_POINT ( 'NONE',  ( 4.780456778825039166, -1.700172319169111157, 0.3389010404759411621 ) ) ;
#129384 = TOROIDAL_SURFACE ( 'NONE', #201917, 6.500000000000000000, 0.2999999999999999889 ) ;
#129385 = CARTESIAN_POINT ( 'NONE',  ( 4.369693832449129012, -0.3752608539947903665, 2.138364329090262306 ) ) ;
#129386 = CARTESIAN_POINT ( 'NONE',  ( 4.681643115420508039, 4.356338477612361260, 0.7998128361456341429 ) ) ;
#129387 = CARTESIAN_POINT ( 'NONE',  ( 5.841029835422532734, -1.731992920607817288, -1.032484497598872064 ) ) ;
#129388 = CARTESIAN_POINT ( 'NONE',  ( 6.250000000000084377, 2.349784478886278158E-12, 2.052068128417940063 ) ) ;
#129389 = CARTESIAN_POINT ( 'NONE',  ( -1.500000000000011324, 5.410416667349489117, -0.8660254037844313801 ) ) ;
#129390 = CARTESIAN_POINT ( 'NONE',  ( 3.575144680771982220, 0.04857402364528973226, -1.925943534667476476 ) ) ;
#129391 = CARTESIAN_POINT ( 'NONE',  ( -1.402160292154681736E-14, 9.843750000682801371, 1.732050807568881190 ) ) ;
#129392 = CARTESIAN_POINT ( 'NONE',  ( -0.05755013669183139946, -1.372491973113322050, -1.747462644287574030 ) ) ;
#129393 = ORIENTED_EDGE ( 'NONE', *, *, #46380, .T. ) ;
#129394 = CARTESIAN_POINT ( 'NONE',  ( 6.983263157960410972, 2.978556228996271482, 2.299637001123565838 ) ) ;
#129395 = CARTESIAN_POINT ( 'NONE',  ( 1.499999999999989120, 3.254166666666690855, 0.8660254037844524744 ) ) ;
#129396 = CARTESIAN_POINT ( 'NONE',  ( 6.661133543015731462, 6.665743976473484267, -0.7998128361456281477 ) ) ;
#129397 = CARTESIAN_POINT ( 'NONE',  ( 1.577126836321657954, -1.567749618368704967, 1.573888218047289067 ) ) ;
#129398 = CARTESIAN_POINT ( 'NONE',  ( 6.883263157960391787, -0.001104538646235289417, 1.946037152736757925 ) ) ;
#129399 = CARTESIAN_POINT ( 'NONE',  ( 7.375272376154084597, 9.627570410311676596, -1.443375672974057666 ) ) ;
#129400 = CARTESIAN_POINT ( 'NONE',  ( -8.961576348508637935, 12.43862759236002269, -1.082531754730543083 ) ) ;
#129401 = CARTESIAN_POINT ( 'NONE',  ( 2.878073747850912412, 6.579779482459851003, -0.7998128361456362523 ) ) ;
#129402 = CARTESIAN_POINT ( 'NONE',  ( 0.0006249722829775038483, -1.976948959267275541, 0.3961041280396286890 ) ) ;
#129404 = CARTESIAN_POINT ( 'NONE',  ( 5.107907679073590224, 0.6501100083472023394, -1.957599679411163196 ) ) ;
#129403 = CARTESIAN_POINT ( 'NONE',  ( 10.56588178375152864, 11.22128359066528169, -0.7998128361456281477 ) ) ;
#129405 = CARTESIAN_POINT ( 'NONE',  ( -3.928111819657352566, 5.605883094398769195, 1.599625672291267398 ) ) ;
#129406 = DIRECTION ( 'NONE',  ( 0.000000000000000000, -0.000000000000000000, 1.000000000000000000 ) ) ;
#129407 = CARTESIAN_POINT ( 'NONE',  ( -0.6823417656250212460, 0.8010416670080899859, 1.181850606188755259 ) ) ;
#129408 = CARTESIAN_POINT ( 'NONE',  ( 6.608674649642057197, 1.385883050205028333, -1.256505298338560062 ) ) ;
#129409 = CARTESIAN_POINT ( 'NONE',  ( 5.555191991570319843, -1.093772777934084894, 1.345723482730563525 ) ) ;
#129410 = CARTESIAN_POINT ( 'NONE',  ( 5.073663595168481422, -0.9608294848038684277, 1.450969404730037660 ) ) ;
#129411 = CARTESIAN_POINT ( 'NONE',  ( 3.765413976293345844, 5.416068943807445635, 1.599625672291267398 ) ) ;
#129412 = CARTESIAN_POINT ( 'NONE',  ( 2.999882145774832143, -2.289621049425132338, 0.1149546659729560466 ) ) ;
#129413 = CARTESIAN_POINT ( 'NONE',  ( -1.201851678989727383E-14, 5.759375000341417028, -1.575800808251660801 ) ) ;
#129414 = CARTESIAN_POINT ( 'NONE',  ( 1.323879276782027548, 1.773944146221797524, 0.4926282247687193139 ) ) ;
#129415 = EDGE_CURVE ( 'NONE', #120109, #125687, #14798, .T. ) ;
#129416 = CARTESIAN_POINT ( 'NONE',  ( -0.4499999960735147075, 3.999999999999974243, 0.9281957781481157133 ) ) ;
#129417 = CARTESIAN_POINT ( 'NONE',  ( -11.99928154390922330, 8.498563086969809888, 1.147813104201464540 ) ) ;
#129418 = CARTESIAN_POINT ( 'NONE',  ( 2.098414945899258033, -0.4839449910110822373, -1.760204267430766301 ) ) ;
#129419 = CARTESIAN_POINT ( 'NONE',  ( 2.567029916978436077, -1.034165006014248211, 1.730866473406714068 ) ) ;
#129420 = CARTESIAN_POINT ( 'NONE',  ( 1.359612608069910911, 2.158557413232742750, -0.3773744582575569440 ) ) ;
#129421 = CARTESIAN_POINT ( 'NONE',  ( 6.743451144134844810, 14.00000000000000000, -9.536680065235829673 ) ) ;
#129422 = CARTESIAN_POINT ( 'NONE',  ( 4.700279962202062123, -2.105436441984291029, -0.05427613729028049616 ) ) ;
#129423 = CARTESIAN_POINT ( 'NONE',  ( -7.823218330285243383, 9.085841792542966644, -1.199719254218446718 ) ) ;
#129424 = CARTESIAN_POINT ( 'NONE',  ( 8.350859280846282928, 13.12796858787615584, 8.536646826506956387 ) ) ;
#129425 = CARTESIAN_POINT ( 'NONE',  ( 0.9946828900261883710, 2.039433816042154124, 0.3556643922909968891 ) ) ;
#129426 = CARTESIAN_POINT ( 'NONE',  ( 4.333802657862601215, 8.207853534148366492, 0.7998128361456462443 ) ) ;
#129427 = CARTESIAN_POINT ( 'NONE',  ( 1.360316468749959373, -0.4531249996586189654, -4.163336342344337027E-14 ) ) ;
#129428 = CARTESIAN_POINT ( 'NONE',  ( 3.176547234745368264, 0.9552152173708803318, 1.893241096743401464 ) ) ;
#129429 = CARTESIAN_POINT ( 'NONE',  ( 0.2934164811014350893, 1.426665091747752356, 1.294802382297273180 ) ) ;
#129430 = ORIENTED_EDGE ( 'NONE', *, *, #1218, .F. ) ;
#129431 = CARTESIAN_POINT ( 'NONE',  ( -5.306037014901836990, 7.283738832175834510, 1.599625672291263179 ) ) ;
#129432 = B_SPLINE_CURVE_WITH_KNOTS ( 'NONE', 3,
 ( #52097, #150679, #167976, #88878, #18513, #72592 ),
 .UNSPECIFIED., .F., .F.,
 ( 4, 2, 4 ),
 ( 0.000000000000000000, 0.001225895755212361030, 0.002451791510424721626 ),
 .UNSPECIFIED. ) ;
#129433 = CARTESIAN_POINT ( 'NONE',  ( 7.886038904643079661, 12.35212915539230139, -0.7998128361456352531 ) ) ;
#129434 = CARTESIAN_POINT ( 'NONE',  ( 5.329763783503544516, 9.232158490813878515, -0.7216878364870458196 ) ) ;
#129435 = CARTESIAN_POINT ( 'NONE',  ( 1.737499999999999378, -2.522916665710750461, -3.009438278150925683 ) ) ;
#129436 = CARTESIAN_POINT ( 'NONE',  ( -6.091691091241777656, 6.001394449403842479, 0.7998128361456341429 ) ) ;
#129437 = CARTESIAN_POINT ( 'NONE',  ( 6.170199167347634628, 2.114832956739281400, -0.1575216572810705096 ) ) ;
#129438 = CARTESIAN_POINT ( 'NONE',  ( 0.8156195060344322290, -0.3088407994138153700, 2.083069475825300110 ) ) ;
#129439 = CARTESIAN_POINT ( 'NONE',  ( -4.281342646865346602, 8.216926531310035031, 0.7998128361456352531 ) ) ;
#129440 = CARTESIAN_POINT ( 'NONE',  ( 9.589694723567584234, 10.08239868711733855, -0.7998128361456281477 ) ) ;
#129441 = CARTESIAN_POINT ( 'NONE',  ( 5.717585430250381684, 0.3647202891138579539, -1.824662122815931875 ) ) ;
#129442 = CARTESIAN_POINT ( 'NONE',  ( 6.903072767652295383, 11.20533532890304684, 1.040834085586084257E-14 ) ) ;
#129443 = ADVANCED_FACE ( 'NONE', ( #99042 ), #58289, .T. ) ;
#129444 = CARTESIAN_POINT ( 'NONE',  ( -0.5150272702496208055, 4.156437351174604444, 0.3999758201171630390 ) ) ;
#129445 = CARTESIAN_POINT ( 'NONE',  ( -4.496464221587651799, 5.274905009054215554, 1.199719254218452935 ) ) ;
#129446 = CARTESIAN_POINT ( 'NONE',  ( -10.33094986393327197, 11.15512238411806578, 0.7216878364870438212 ) ) ;
#129448 = CARTESIAN_POINT ( 'NONE',  ( 1.926150285298435572, 1.005797860886543660, 1.684270608208485065 ) ) ;
#129447 = CARTESIAN_POINT ( 'NONE',  ( -6.880926654135487652, 7.986501503701545879, 1.199719254218450271 ) ) ;
#129449 = CARTESIAN_POINT ( 'NONE',  ( 0.9717996764858798375, 2.083101276202529384, -0.5774176476955604764 ) ) ;
#129451 = CARTESIAN_POINT ( 'NONE',  ( -5.829309506874599478, 6.192769411583809003, 0.9639237645304669089 ) ) ;
#129450 = CARTESIAN_POINT ( 'NONE',  ( -4.274563570058511175, 8.209017608368725405, 0.000000000000000000 ) ) ;
#129452 = CARTESIAN_POINT ( 'NONE',  ( 1.364683531249986537, 0.6552083336747522857, -0.7879004041258239610 ) ) ;
#129453 = CARTESIAN_POINT ( 'NONE',  ( 3.110371403566422277, 0.6269696901312575843, -1.616694140604297614 ) ) ;
#129454 = CARTESIAN_POINT ( 'NONE',  ( 2.308218407481243961, 1.554217257889878301, 0.7831649204469055547 ) ) ;
#129455 = CARTESIAN_POINT ( 'NONE',  ( 6.914295153289432783, 10.05013286460426691, -1.082531754730537976 ) ) ;
#129456 = CARTESIAN_POINT ( 'NONE',  ( -10.99878419127389684, 6.872217442641685103, 3.961452310287494338 ) ) ;
#129457 = CARTESIAN_POINT ( 'NONE',  ( 1.985689569138231914, 1.418919563317089017, 1.494737215543304965 ) ) ;
#129458 = CARTESIAN_POINT ( 'NONE',  ( 1.405624810022429561, 0.3905361843517705100, 1.977748161624798939 ) ) ;
#129459 = FACE_OUTER_BOUND ( 'NONE', #173428, .T. ) ;
#129460 = CARTESIAN_POINT ( 'NONE',  ( -4.014095998097799267, 6.840806543492835345, -1.199719254218450271 ) ) ;
#129461 = CARTESIAN_POINT ( 'NONE',  ( 1.498834128701274748, 1.612947343535120925, -1.133365233443942355 ) ) ;
#129464 = EDGE_CURVE ( 'NONE', #186824, #190586, #29402, .T. ) ;
#129463 = CARTESIAN_POINT ( 'NONE',  ( -5.858531774880906262, 6.967946837850073294, 1.082531754730549078 ) ) ;
#129462 = CARTESIAN_POINT ( 'NONE',  ( 5.941656858135131891, -1.798430535887390658, 0.6506349336675710804 ) ) ;
#129465 = CARTESIAN_POINT ( 'NONE',  ( -5.424670858799220063, 9.342883411992149334, 0.000000000000000000 ) ) ;
#129466 = CARTESIAN_POINT ( 'NONE',  ( 5.515134625708930649, 9.656350506627580543, 0.000000000000000000 ) ) ;
#129467 = CARTESIAN_POINT ( 'NONE',  ( -6.607619761813764647, 8.802252036906432764, 1.599625672291269396 ) ) ;
#129468 = CARTESIAN_POINT ( 'NONE',  ( 1.295575897195440307, 1.865243415117883385, -0.7750591016795584931 ) ) ;
#129469 = SURFACE_SIDE_STYLE ('',( #26532 ) ) ;
#129470 = EDGE_CURVE ( 'NONE', #63977, #69507, #44386, .T. ) ;
#129471 = CARTESIAN_POINT ( 'NONE',  ( 4.612551310933718618, -0.9822873175598394457, -2.088206479280288796 ) ) ;
#129472 = CARTESIAN_POINT ( 'NONE',  ( 5.934033239752055877, 1.167398200610193282, 1.576599764842034457 ) ) ;
#129473 = CARTESIAN_POINT ( 'NONE',  ( 1.780054392102415672, -1.085390340960286082, -1.633940563308281968 ) ) ;
#129474 = CARTESIAN_POINT ( 'NONE',  ( 10.55910270694468345, 11.21337466772398095, 0.7998128361456462443 ) ) ;
#129475 = CARTESIAN_POINT ( 'NONE',  ( -9.342754679287263997, 14.55305246464195434, 7.460282140107980631 ) ) ;
#129476 = ORIENTED_EDGE ( 'NONE', *, *, #148860, .F. ) ;
#129477 = CARTESIAN_POINT ( 'NONE',  ( 1.147838861943322630, 2.084982156806517661, -0.3680304603586990742 ) ) ;
#129479 = CARTESIAN_POINT ( 'NONE',  ( -8.532158741701643123, 8.848606708273724308, 0.7998128361456462443 ) ) ;
#129478 = CARTESIAN_POINT ( 'NONE',  ( -4.634189577772691138, 4.300976017023221409, 1.214306433183764966E-14 ) ) ;
#129480 = CARTESIAN_POINT ( 'NONE',  ( 0.8316833483592298570, 1.813467871694788069, 0.3170515863319539052 ) ) ;
#129481 = EDGE_LOOP ( 'NONE', ( #196368, #188299, #23427, #77058 ) ) ;
#129482 = CARTESIAN_POINT ( 'NONE',  ( 4.504835797669192843, 0.5730007755406724135, 2.094059341655955198 ) ) ;
#129483 = CARTESIAN_POINT ( 'NONE',  ( 11.51809730133723697, 8.398897926204437425, 3.388883170576209913 ) ) ;
#129484 = CARTESIAN_POINT ( 'NONE',  ( 1.635180430577408028, 1.980530345366804834, 0.7584260845197098311 ) ) ;
#129485 = CARTESIAN_POINT ( 'NONE',  ( 0.7499999999999902300, 3.264583334016149418, 1.299038105676669330 ) ) ;
#129486 = CARTESIAN_POINT ( 'NONE',  ( 9.576136569953906275, 10.06658084123472641, 0.000000000000000000 ) ) ;
#129487 = CARTESIAN_POINT ( 'NONE',  ( 0.000000000000000000, -0.4330127018922214077, 0.000000000000000000 ) ) ;
#129488 = CARTESIAN_POINT ( 'NONE',  ( 3.005207323352117488, 1.739114039596071803, 1.105284290502930089 ) ) ;
#129490 = CARTESIAN_POINT ( 'NONE',  ( 0.8020088176248600931, 1.394402496181508466, -1.202495849378336423 ) ) ;
#129489 = CARTESIAN_POINT ( 'NONE',  ( -8.552495972122143186, 8.872333477097637200, 0.7998128361456462443 ) ) ;
#129491 = CARTESIAN_POINT ( 'NONE',  ( -1.364683531249997417, 4.009375000341424133, 1.214306433183764966E-14 ) ) ;
#129492 = CARTESIAN_POINT ( 'NONE',  ( -0.02264175331117677936, 4.084751018978694859, -2.643765695431527174 ) ) ;
#129493 = CARTESIAN_POINT ( 'NONE',  ( 1.499630086250555383, 4.449194373282669979, 0.09116236908481112344 ) ) ;
#129494 = CARTESIAN_POINT ( 'NONE',  ( 0.2060869173217265982, -0.5842117877600698783, 2.128085570573131413 ) ) ;
#129495 = CARTESIAN_POINT ( 'NONE',  ( 2.126610404160976575, 1.303795175273964269, -1.848758590024823123 ) ) ;
#129496 = CARTESIAN_POINT ( 'NONE',  ( -7.673551755654729689, 11.89630144833179060, 0.7216878364870458196 ) ) ;
#129497 = CARTESIAN_POINT ( 'NONE',  ( 2.619172825086816037, 1.532478635541080214, 0.9657477217557136617 ) ) ;
#129498 = CARTESIAN_POINT ( 'NONE',  ( 1.956118367686721538, -1.175378340988470827, 1.512710158094223933 ) ) ;
#129499 = CARTESIAN_POINT ( 'NONE',  ( 3.367693471486675083, -0.4065805204805824635, 2.029877954327436118 ) ) ;
#129500 = CARTESIAN_POINT ( 'NONE',  ( 1.364683531249988757, 1.696875000341414808, 0.000000000000000000 ) ) ;
#129501 = CARTESIAN_POINT ( 'NONE',  ( 1.428526753364509627, 1.899469058273341338, 0.5276583995704342556 ) ) ;
#129502 = CARTESIAN_POINT ( 'NONE',  ( 0.2176306489089273599, -1.889907718300526174, 0.3723054783561028369 ) ) ;
#129503 = CARTESIAN_POINT ( 'NONE',  ( 2.588565208901713266, -0.3177388942022137397, -1.843305967786903032 ) ) ;
#129505 = CARTESIAN_POINT ( 'NONE',  ( 4.745935331938881951, 8.308991367555595531, -0.7587592799198628057 ) ) ;
#129504 = CARTESIAN_POINT ( 'NONE',  ( 1.120229914364691659, -2.250463172007353130, 0.5101417434775123994 ) ) ;
#129506 = CARTESIAN_POINT ( 'NONE',  ( 2.980726927023560346, 1.751358449955683350, 0.6298351686941299210 ) ) ;
#129507 = CARTESIAN_POINT ( 'NONE',  ( -1.364683531249997417, 2.509375000341422357, 1.214306433183764966E-14 ) ) ;
#129508 = CARTESIAN_POINT ( 'NONE',  ( 5.406706549104464798, 0.5953045380993631230, 1.974924460807401028 ) ) ;
#129509 = CARTESIAN_POINT ( 'NONE',  ( -6.586563698140583512, 6.578745824119123675, 1.040834085586084257E-14 ) ) ;
#129510 = CARTESIAN_POINT ( 'NONE',  ( 7.775764792637399836, 9.030479331953833011, -1.199719254218441611 ) ) ;
#129511 = CARTESIAN_POINT ( 'NONE',  ( -1.272106862006040062, 3.722537557350577675, 0.4878970607599520393 ) ) ;
#129513 = CARTESIAN_POINT ( 'NONE',  ( 6.704139028598911310, -2.105588161048920437, 0.04759252156865538541 ) ) ;
#129512 = VECTOR ( 'NONE', #213017, 1000.000000000000000 ) ;
#129514 = CARTESIAN_POINT ( 'NONE',  ( -0.6823417656250212460, 2.113541667008083991, 1.181850606188767472 ) ) ;
#129515 = CARTESIAN_POINT ( 'NONE',  ( 5.466167184710096549, 1.060119519021487378, 1.883692621652333532 ) ) ;
#129516 = CARTESIAN_POINT ( 'NONE',  ( 0.05299788485858129838, 0.3494575625802974206, 1.989167885679890002 ) ) ;
#129517 = CARTESIAN_POINT ( 'NONE',  ( -0.6823417656250003738, -0.03229166632524871350, -1.181850606188749264 ) ) ;
#129518 = CARTESIAN_POINT ( 'NONE',  ( -5.314433026876900001, 6.262888621853549331, 1.082531754730548412 ) ) ;
#129521 = CARTESIAN_POINT ( 'NONE',  ( 4.853455804012222430, 5.725081861844796727, 1.082531754730560403 ) ) ;
#129520 = CARTESIAN_POINT ( 'NONE',  ( 1.642778471875000035, -0.5760416661887077794, -2.845375778867859751 ) ) ;
#129519 = CARTESIAN_POINT ( 'NONE',  ( 6.170896192875352959, 7.228408975556602556, 1.199719254218453823 ) ) ;
#129522 = CARTESIAN_POINT ( 'NONE',  ( -6.330731382938325602, 6.350551133041632212, 0.7998128361456281477 ) ) ;
#129523 = CARTESIAN_POINT ( 'NONE',  ( 5.260953973667149342, -0.05432152012316109058, -2.015980820358989511 ) ) ;
#129524 = CARTESIAN_POINT ( 'NONE',  ( -8.227100285394159940, 8.492705175914988303, 0.7998128361456602331 ) ) ;
#129526 = CARTESIAN_POINT ( 'NONE',  ( -7.444835747235459600, 8.818634805597074688, 1.082531754730549078 ) ) ;
#129525 = CARTESIAN_POINT ( 'NONE',  ( -2.819205876637805641, 5.376491725131008259, -1.199719254218446718 ) ) ;
#129527 = FACE_OUTER_BOUND ( 'NONE', #50407, .T. ) ;
#129529 = CARTESIAN_POINT ( 'NONE',  ( -1.402160292154681736E-14, 9.671875000341399797, 1.575800808251682339 ) ) ;
#129528 = CARTESIAN_POINT ( 'NONE',  ( 5.911032513020411550, 1.904272706209766630, 1.023102869888978583 ) ) ;
#129530 = DIRECTION ( 'NONE',  ( -0.000000000000000000, -1.000000000000000000, -0.000000000000000000 ) ) ;
#129531 = CARTESIAN_POINT ( 'NONE',  ( -11.82159334412768104, 7.677341743419558107, 2.075736564397430151 ) ) ;
#129533 = CARTESIAN_POINT ( 'NONE',  ( 5.747672784407955149, 1.986098415631059932, -0.3474865836668520336 ) ) ;
#129532 = CARTESIAN_POINT ( 'NONE',  ( -5.056828107772848746, 8.843457192469559303, -0.7216878364870207285 ) ) ;
#129534 = CARTESIAN_POINT ( 'NONE',  ( 1.364683531249986537, -0.5322916663252452718, -0.7879004041258309554 ) ) ;
#129535 = CARTESIAN_POINT ( 'NONE',  ( 2.174029202910219283, -1.062355927555928226, 1.358808029953484597 ) ) ;
#129536 = CARTESIAN_POINT ( 'NONE',  ( 4.037295881819344956, 7.932205305423046582, -0.7998128361456362523 ) ) ;
#129538 = CARTESIAN_POINT ( 'NONE',  ( 7.991605200612358573, 8.288237253661408843, 0.7998128361456281477 ) ) ;
#129537 = CARTESIAN_POINT ( 'NONE',  ( 6.290620087060792009, 10.28288116830553101, -0.7216878364870267237 ) ) ;
#129539 = CARTESIAN_POINT ( 'NONE',  ( -10.50059885609812937, 5.377696206510352184, -5.808392519734754345 ) ) ;
#129540 = CARTESIAN_POINT ( 'NONE',  ( 6.186763334926775215, -0.2743023915687745617, -1.850177433978140051 ) ) ;
#129541 = CARTESIAN_POINT ( 'NONE',  ( 0.7330649400898289203, 1.860844449999502492, 0.7684416140155255759 ) ) ;
#129542 = CARTESIAN_POINT ( 'NONE',  ( 3.012930935654754450, 1.599341701681813444, -1.520756135150652222 ) ) ;
#129543 = CARTESIAN_POINT ( 'NONE',  ( 5.577072259002747501, 2.003115288890752410, 0.8377749483753393900 ) ) ;
#129544 = VERTEX_POINT ( 'NONE', #192943 ) ;
#129545 = CARTESIAN_POINT ( 'NONE',  ( 4.760848217054122422, 5.583353003765119560, -1.199719254218452047 ) ) ;
#129546 = CARTESIAN_POINT ( 'NONE',  ( 8.961576348508637935, 11.47825837805867799, -1.443375672974052559 ) ) ;
#129548 = CARTESIAN_POINT ( 'NONE',  ( 1.827750133516142128, 0.7691037069590834774, -1.864176919362303675 ) ) ;
#129547 = CARTESIAN_POINT ( 'NONE',  ( 3.123802294713691641, -0.4116375371931815796, 2.079978743196985391 ) ) ;
#129550 = ORIENTED_EDGE ( 'NONE', *, *, #114672, .T. ) ;
#129549 = CARTESIAN_POINT ( 'NONE',  ( 2.425776345151516633, -1.791340243523626974, 0.2692766639123735373 ) ) ;
#129551 = CARTESIAN_POINT ( 'NONE',  ( 7.212011367826596242, 7.378711115411311638, 0.000000000000000000 ) ) ;
#129552 = CARTESIAN_POINT ( 'NONE',  ( 5.880485940025228508, 7.883652901494672349, 1.599625672291267398 ) ) ;
#129554 = CARTESIAN_POINT ( 'NONE',  ( 1.323292448300671165, -1.390094005022534773, -1.318457861805687914 ) ) ;
#129553 = CARTESIAN_POINT ( 'NONE',  ( -2.903417451620861289, 6.539070793532962611, 0.7998128361456341429 ) ) ;
#129555 = CARTESIAN_POINT ( 'NONE',  ( 0.7499999999999902300, 3.483333333333352044, 1.299038105676669330 ) ) ;
#129556 = DIRECTION ( 'NONE',  ( 1.776356839400250465E-14, 0.000000000000000000, -1.000000000000000000 ) ) ;
#129557 = CARTESIAN_POINT ( 'NONE',  ( 5.463572716182819811, 8.357623354646536384, 1.082531754730558626 ) ) ;
#129558 = CARTESIAN_POINT ( 'NONE',  ( 0.6823417656249882723, -0.09479166632524876901, 1.181850606188755259 ) ) ;
#129559 = CARTESIAN_POINT ( 'NONE',  ( -9.755255220232635693, 11.33988483081495957, -1.199719254218441611 ) ) ;
#129560 = CARTESIAN_POINT ( 'NONE',  ( 5.524359596833869013, 1.291058806671550485, -1.733668313432787711 ) ) ;
#129561 = CARTESIAN_POINT ( 'NONE',  ( -4.448483799059637533, 7.243629294661272588, 1.082531754730549967 ) ) ;
#129562 = CARTESIAN_POINT ( 'NONE',  ( 4.746763178560250651, 7.591621904078704297, 1.082531754730549078 ) ) ;
#129563 = CARTESIAN_POINT ( 'NONE',  ( 2.320699612028754188, -0.8158636990020677882, -1.957571985684476212 ) ) ;
#129564 = EDGE_CURVE ( 'NONE', #142643, #144530, #118614, .T. ) ;
#129566 = CARTESIAN_POINT ( 'NONE',  ( -11.78041000490145862, 4.728159582424554586, -4.968671142906706528 ) ) ;
#129565 = CARTESIAN_POINT ( 'NONE',  ( 1.500000000000007105, 10.64264068711930733, 1.214306433183764966E-14 ) ) ;
#129567 = CARTESIAN_POINT ( 'NONE',  ( 3.567610853275906546, 1.924076846980572464, -0.4285291244595054727 ) ) ;
#129568 = CARTESIAN_POINT ( 'NONE',  ( 5.888906298306328502, -1.818048641159516476, -0.5935555146628914702 ) ) ;
#129569 = VERTEX_POINT ( 'NONE', #179915 ) ;
#129570 = CARTESIAN_POINT ( 'NONE',  ( 0.5773502691896192918, -2.500000000000002220, 1.000000000000004441 ) ) ;
#129571 = CARTESIAN_POINT ( 'NONE',  ( 0.6782873735513493818, -1.106163567672680204, -1.749894625276714688 ) ) ;
#129572 = CARTESIAN_POINT ( 'NONE',  ( 2.396341059777199689, 1.559625748545325319, -1.156842939599848741 ) ) ;
#129573 = VERTEX_POINT ( 'NONE', #196165 ) ;
#129574 = DIRECTION ( 'NONE',  ( 0.6507913734559641616, -0.7592566023653004592, 0.000000000000000000 ) ) ;
#129576 = CARTESIAN_POINT ( 'NONE',  ( 8.025500584646550806, 8.327781868367935658, 0.000000000000000000 ) ) ;
#129575 = CARTESIAN_POINT ( 'NONE',  ( -7.105881907338169157, 8.423188659050232729, -1.082531754730549967 ) ) ;
#129578 = CARTESIAN_POINT ( 'NONE',  ( 6.979750152936881058, 7.037463354714830643, 0.7998128361456341429 ) ) ;
#129577 = CARTESIAN_POINT ( 'NONE',  ( 2.906283313408718705, 1.513773858955402618, -1.442204806208322809 ) ) ;
#129579 = CARTESIAN_POINT ( 'NONE',  ( 8.039058738260216330, 8.343599714250547805, -0.7998128361456341429 ) ) ;
#129581 = ORIENTED_EDGE ( 'NONE', *, *, #187141, .T. ) ;
#129580 = CARTESIAN_POINT ( 'NONE',  ( 6.059226159983991167, -1.612925389857391645, 1.026989893868179404 ) ) ;
#129582 = CARTESIAN_POINT ( 'NONE',  ( 4.494872972331320327, -0.4818267175418550208, -2.153482813429814069 ) ) ;
#129583 = EDGE_CURVE ( 'NONE', #191009, #173974, #101021, .T. ) ;
#129584 = CARTESIAN_POINT ( 'NONE',  ( 2.872332416675418276, 1.179501869419818494, 1.864919306664609921 ) ) ;
#129585 = CARTESIAN_POINT ( 'NONE',  ( 1.664566505720616929, 0.6010121217654046388, 1.815428919054395518 ) ) ;
#129586 = DIRECTION ( 'NONE',  ( 0.000000000000000000, 0.000000000000000000, -1.000000000000000000 ) ) ;
#129587 = CARTESIAN_POINT ( 'NONE',  ( 8.401248741962376698, 12.95320729893149370, 0.7998128361456462443 ) ) ;
#129588 = CARTESIAN_POINT ( 'NONE',  ( 4.615722581382986967, 0.4567890626981512270, -2.019179087418949692 ) ) ;
#129590 = CARTESIAN_POINT ( 'NONE',  ( 1.534274790466340299, 1.065227450066742687, -1.880959520452238465 ) ) ;
#129589 = CARTESIAN_POINT ( 'NONE',  ( 2.763444990417154240E-17, -6.211932585243244986, 10.91339599544322958 ) ) ;
#129591 = CARTESIAN_POINT ( 'NONE',  ( 4.792620198997869174, 1.822056328612733145, -1.217503271791681163 ) ) ;
#129592 = CARTESIAN_POINT ( 'NONE',  ( -5.864945314351738936, 6.621640825619397042, 0.9118253242758539434 ) ) ;
#129593 = EDGE_CURVE ( 'NONE', #3985, #118628, #13172, .T. ) ;
#129594 = CARTESIAN_POINT ( 'NONE',  ( 0.000000000000000000, -5.166862915010145052, 0.000000000000000000 ) ) ;
#129595 = CARTESIAN_POINT ( 'NONE',  ( -7.095284314752811738, 15.44810195178240342, 9.632597271208634737 ) ) ;
#129596 = CARTESIAN_POINT ( 'NONE',  ( 6.398522151006641678, 6.429640362454684954, 0.000000000000000000 ) ) ;
#129597 = CARTESIAN_POINT ( 'NONE',  ( 1.364683531249996529, 13.77604166700806765, 0.7879004041258405033 ) ) ;
#129598 = CARTESIAN_POINT ( 'NONE',  ( -5.492988512192097161, 6.437516681426083132, 1.199719254218452935 ) ) ;
#129599 = EDGE_CURVE ( 'NONE', #162002, #142064, #146873, .T. ) ;
#129601 = CARTESIAN_POINT ( 'NONE',  ( -0.06968618116158857567, -1.560424145883563929, -1.276814929289785239 ) ) ;
#129600 = AXIS2_PLACEMENT_3D ( 'NONE', #86896, #204883, #19747 ) ;
#129602 = CARTESIAN_POINT ( 'NONE',  ( -7.700668062882059850, 11.92793714009701311, -0.7216878364870267237 ) ) ;
#129603 = CARTESIAN_POINT ( 'NONE',  ( 4.680570891794395116, 1.277791010243028991, -1.628752506732597638 ) ) ;
#129604 = CARTESIAN_POINT ( 'NONE',  ( 3.545458749278436184, -1.459459766114965973, -1.257631776117454914 ) ) ;
#129605 = CARTESIAN_POINT ( 'NONE',  ( 5.958642064211575828, -2.010625215935774257, -0.6636248059145292144 ) ) ;
#129606 = VECTOR ( 'NONE', #188627, 1000.000000000000000 ) ;
#129607 = CARTESIAN_POINT ( 'NONE',  ( 4.364835388595708743, 7.179726155748598515, 1.199719254218462483 ) ) ;
#129608 = CARTESIAN_POINT ( 'NONE',  ( 9.333041836227135235, 4.446947634373625391, 7.472413793103378943 ) ) ;
#129609 = CARTESIAN_POINT ( 'NONE',  ( 4.135575292396717728, 1.855891543885644479, -0.6595280497384666818 ) ) ;
#129610 = CARTESIAN_POINT ( 'NONE',  ( 5.876963737413220201, 2.120050906709324501, -0.8721662429640556491 ) ) ;
#129611 = CARTESIAN_POINT ( 'NONE',  ( 3.527797039230845311, -1.088449851438414218, -1.465592618984489670 ) ) ;
#129612 = CARTESIAN_POINT ( 'NONE',  ( 7.702440666339465558, 8.158804663583751449, -0.7216878364870317197 ) ) ;
#129613 = CARTESIAN_POINT ( 'NONE',  ( 4.243338890952890630, 5.973648010910253880, -1.443375672974051449 ) ) ;
#129614 = CARTESIAN_POINT ( 'NONE',  ( -7.228432174741334038, 8.462200954400218578, -1.199719254218452047 ) ) ;
#129615 = CARTESIAN_POINT ( 'NONE',  ( 5.825163275726873202, 6.825053905550038991, 1.199719254218452047 ) ) ;
#129616 = ORIENTED_EDGE ( 'NONE', *, *, #30361, .T. ) ;
#129618 = CARTESIAN_POINT ( 'NONE',  ( 5.467046525086633579, -1.584481552701553220, 1.241800460852604759 ) ) ;
#129617 = CARTESIAN_POINT ( 'NONE',  ( 1.012948470060770934, -1.796336717620912626, 0.4034172393945419377 ) ) ;
#129619 = AXIS2_PLACEMENT_3D ( 'NONE', #91989, #95181, #161230 ) ;
#129620 = CARTESIAN_POINT ( 'NONE',  ( 5.748750450937779810, 2.265299150918558269, -0.3897391249057541862 ) ) ;
#129621 = CARTESIAN_POINT ( 'NONE',  ( 5.313317156408340125, -1.655227327604656740, -1.052681782574490743 ) ) ;
#129622 = CARTESIAN_POINT ( 'NONE',  ( -7.366157530926372488, 7.488271962369228874, -0.7998128361456291469 ) ) ;
#129623 = CARTESIAN_POINT ( 'NONE',  ( -4.355193658487827690, 6.104145239700998538, -1.599625672291256295 ) ) ;
#129624 = CARTESIAN_POINT ( 'NONE',  ( -7.735357998705607585, -5.759585062615363071, 7.724608556409203075 ) ) ;
#129625 = CARTESIAN_POINT ( 'NONE',  ( -5.309953438407606363, 6.223975762010839574, 1.199719254218452935 ) ) ;
#129627 = CARTESIAN_POINT ( 'NONE',  ( 0.1099206271272800961, -0.7955684105149689600, -1.691499381818922343 ) ) ;
#129626 = CARTESIAN_POINT ( 'NONE',  ( 1.698888801382715252, 1.740066399362389271, 1.158727311120285819 ) ) ;
#129628 = CARTESIAN_POINT ( 'NONE',  ( 5.929623787841700633, 0.9553189508899215809, -1.690649115374833311 ) ) ;
#129629 = CARTESIAN_POINT ( 'NONE',  ( -0.1106727585416019261, 4.087503477334416324, -2.558207815289376796 ) ) ;
#129630 = CARTESIAN_POINT ( 'NONE',  ( 0.4326491639514402077, -1.228936893156933330, -1.232681022120321934 ) ) ;
#129631 = CARTESIAN_POINT ( 'NONE',  ( 5.099838337034727331, 9.101561826515851550, -0.7998128361456281477 ) ) ;
#129633 = CARTESIAN_POINT ( 'NONE',  ( 0.6124999999999949374, 1.645833334016133520, 1.060881119635922243 ) ) ;
#129632 = CARTESIAN_POINT ( 'NONE',  ( -11.86145016429273014, 10.19999999999999929, 1.179999999999997051 ) ) ;
#129634 = CARTESIAN_POINT ( 'NONE',  ( 1.470901328764297800, 0.1297424413324743397, -1.720050270840302487 ) ) ;
#129635 =( BOUNDED_CURVE ( )  B_SPLINE_CURVE ( 2, ( #109287, #91925, #175297, #123430, #189392 ),
 .UNSPECIFIED., .F., .T. ) 
 B_SPLINE_CURVE_WITH_KNOTS ( ( 3, 2, 3 ),
 ( 0.1361778335736238132, 0.1375000000000000111, 0.1392051351651958091 ),
 .UNSPECIFIED. ) 
 CURVE ( )  GEOMETRIC_REPRESENTATION_ITEM ( )  RATIONAL_B_SPLINE_CURVE ( ( 0.9419547032718706969, 0.9574871888551546029, 1.000000000000000000, 0.9451732491399851277, 0.9352202683046937359 ) ) 
 REPRESENTATION_ITEM ( '' )  );
#129636 = CARTESIAN_POINT ( 'NONE',  ( 2.033021410476544943, -1.955939774129427988, 0.9887309579383956049 ) ) ;
#129637 = CARTESIAN_POINT ( 'NONE',  ( 3.809358915828209735, 1.892446193107431451, 1.135094405146239049 ) ) ;
#129638 = CARTESIAN_POINT ( 'NONE',  ( -10.40063108925089885, 3.507138841238251370, -5.415724211249433040 ) ) ;
#129639 = PRESENTATION_STYLE_ASSIGNMENT (( #108039 ) ) ;
#129640 = CARTESIAN_POINT ( 'NONE',  ( 1.692468234204123734, 1.072632775294654062, -1.887553939074837261 ) ) ;
#129641 = CARTESIAN_POINT ( 'NONE',  ( 1.244123718695673952, 3.098244533904601195, -0.7749999999999926947 ) ) ;
#129642 = CARTESIAN_POINT ( 'NONE',  ( 2.061849949441786123, 1.306762352624482038, 1.665877332585569803 ) ) ;
#129643 = MECHANICAL_DESIGN_GEOMETRIC_PRESENTATION_REPRESENTATION (  '', ( #130111 ), #36149 ) ;
#129644 = CARTESIAN_POINT ( 'NONE',  ( -5.233084104750526322, 5.207612331738130429, 0.000000000000000000 ) ) ;
#129645 = ORIENTED_EDGE ( 'NONE', *, *, #95824, .F. ) ;
#129647 = CARTESIAN_POINT ( 'NONE',  ( 1.364683531249986537, -0.2822916663252520997, -0.7879004041258309554 ) ) ;
#129646 = CARTESIAN_POINT ( 'NONE',  ( 2.367065275503206667, 0.1088462660112088087, -2.289894902259086429 ) ) ;
#129648 = FILL_AREA_STYLE_COLOUR ( '', #112563 ) ;
#129649 = CARTESIAN_POINT ( 'NONE',  ( 4.008406971134620633, 7.828225232965717595, 0.7998128361456321445 ) ) ;
#129650 = CARTESIAN_POINT ( 'NONE',  ( 6.287741706623968696, 2.126563164181693555, -0.6417273904879957636 ) ) ;
#129651 = CARTESIAN_POINT ( 'NONE',  ( -5.856759171423528088, 8.816340885760650892, 1.082531754730548412 ) ) ;
#129652 = CARTESIAN_POINT ( 'NONE',  ( 6.019457014787495730, 6.125047393447951016, -0.7216878364870257245 ) ) ;
#129653 = CARTESIAN_POINT ( 'NONE',  ( -8.161645285302366659, 8.624267042381978499, 1.040834085586084257E-14 ) ) ;
#129654 = CARTESIAN_POINT ( 'NONE',  ( 4.746763178560261309, 5.670883475476017566, 1.082531754730549078 ) ) ;
#129655 = CIRCLE ( 'NONE', #108921, 9.499999999999992895 ) ;
#129656 = ORIENTED_EDGE ( 'NONE', *, *, #22175, .F. ) ;
#129657 = CARTESIAN_POINT ( 'NONE',  ( 3.024064729735044921, -1.777011313454954999, 0.9530116517338580451 ) ) ;
#129659 = CARTESIAN_POINT ( 'NONE',  ( 2.184505357994303232, 1.191016756910455943, -1.683754781088636632 ) ) ;
#129658 = CARTESIAN_POINT ( 'NONE',  ( 5.601490020740366838, 9.686822124172440596, 1.040834085586084257E-14 ) ) ;
#129660 = CARTESIAN_POINT ( 'NONE',  ( 0.000000000000000000, 1.000000000000000888, 0.000000000000000000 ) ) ;
#129661 = CARTESIAN_POINT ( 'NONE',  ( 4.217995187182915551, 7.935095128439824563, 0.7216878364870257245 ) ) ;
#129662 = CARTESIAN_POINT ( 'NONE',  ( 1.364683531249988535, 5.405208333674750953, -0.7879004041258300672 ) ) ;
#129663 = CARTESIAN_POINT ( 'NONE',  ( 5.015667846030231303, -1.170523448010954315, -1.852474865436819274 ) ) ;
#129664 = CARTESIAN_POINT ( 'NONE',  ( 2.971327447312217984, -1.987046587055636637, -0.3419355124290662240 ) ) ;
#129665 = CARTESIAN_POINT ( 'NONE',  ( 2.595044651933966495, -0.5755060336137384214, 1.749081985381637061 ) ) ;
#129666 = AXIS2_PLACEMENT_3D ( 'NONE', #94858, #196606, #31981 ) ;
#129667 = EDGE_CURVE ( 'NONE', #29485, #171094, #66474, .T. ) ;
#129668 = CARTESIAN_POINT ( 'NONE',  ( 6.123478934866503742, 10.29580919065294431, 0.7998128361456462443 ) ) ;
#129669 = FILL_AREA_STYLE ('',( #48350 ) ) ;
#129670 = CARTESIAN_POINT ( 'NONE',  ( 5.737271026523679041, -1.649412122839075234, 0.7826820710771440481 ) ) ;
#129671 = CARTESIAN_POINT ( 'NONE',  ( 6.592432824109000222, -0.4393352932590722792, 1.975308225066509049 ) ) ;
#129672 = CARTESIAN_POINT ( 'NONE',  ( -6.690058733339450114, 9.892486724616283311, 1.199719254218452047 ) ) ;
#129674 = CARTESIAN_POINT ( 'NONE',  ( -6.143779885648060102, 7.196773283791382703, 1.199719254218452047 ) ) ;
#129673 = CARTESIAN_POINT ( 'NONE',  ( 5.172873261720807747, -2.128565284095069288, -0.7672878325792488186 ) ) ;
#129675 = CARTESIAN_POINT ( 'NONE',  ( 1.084755975048516285, -2.055113062490296016, -0.4597243831155339300 ) ) ;
#129676 = CARTESIAN_POINT ( 'NONE',  ( -7.286581212701773502, 7.465709267765667789, 0.7998128361456341429 ) ) ;
#129677 = CARTESIAN_POINT ( 'NONE',  ( 7.892817981449907982, 12.36003807833360391, 0.7998128361456462443 ) ) ;
#129678 = DIRECTION ( 'NONE',  ( -1.000000000000000000, 0.000000000000000000, 0.000000000000000000 ) ) ;
#129679 = DIRECTION ( 'NONE',  ( 0.9992388858569857257, 0.000000000000000000, -0.03900831951378930240 ) ) ;
#129680 = CARTESIAN_POINT ( 'NONE',  ( -7.823218330285243383, 9.085841792542966644, -1.199719254218446718 ) ) ;
#129681 = UNCERTAINTY_MEASURE_WITH_UNIT (LENGTH_MEASURE( 1.000000000000000082E-05 ), #107100, 'distance_accuracy_value', 'NONE');
#129682 = CARTESIAN_POINT ( 'NONE',  ( 0.1263921868141488214, 7.050106634747087320, 4.033475512996062662 ) ) ;
#129683 = CARTESIAN_POINT ( 'NONE',  ( 4.882344714252594642, 4.868692719482363707, 0.000000000000000000 ) ) ;
#129684 = CARTESIAN_POINT ( 'NONE',  ( 5.064587263324675348, 6.532718652379178259, -1.222898410871699593 ) ) ;
#129685 = CARTESIAN_POINT ( 'NONE',  ( -8.839552966430002101, 12.29626697993494666, -1.082531754730543971 ) ) ;
#129687 = CARTESIAN_POINT ( 'NONE',  ( 2.848112528106065078, -1.494902295879830589, -1.643281164644925907 ) ) ;
#129686 = CARTESIAN_POINT ( 'NONE',  ( 1.916421503514931679, -2.120014230100770725, 0.05699577502370903326 ) ) ;
#129688 = CARTESIAN_POINT ( 'NONE',  ( 5.575758015699216585, 5.849789923344298259, -0.7899890411014517388 ) ) ;
#129689 = CARTESIAN_POINT ( 'NONE',  ( -5.478376588373717659, 8.549133898814758936, -1.199719254218452047 ) ) ;
#129690 = CARTESIAN_POINT ( 'NONE',  ( 7.298366762858032430, 7.409182732956175244, 1.040834085586084257E-14 ) ) ;
#129691 = CARTESIAN_POINT ( 'NONE',  ( 2.892962425504439050, 0.2373818416543191367, 1.947367909387688112 ) ) ;
#129692 = CARTESIAN_POINT ( 'NONE',  ( 5.555090253297246150, 7.504024600312024340, 1.599625672291267398 ) ) ;
#129693 = CARTESIAN_POINT ( 'NONE',  ( -4.059107376188687333, 7.562469429224047524, 0.4300614504739261879 ) ) ;
#129694 = CARTESIAN_POINT ( 'NONE',  ( 3.846762897975340767, 5.510976019103107859, -1.599625672291256295 ) ) ;
#129695 = CARTESIAN_POINT ( 'NONE',  ( -4.502716413514301408, 7.306900678191715848, -1.082531754730549967 ) ) ;
#129696 = CARTESIAN_POINT ( 'NONE',  ( -5.558479791922849245, 9.428717490644563881, 0.7216878364870458196 ) ) ;
#129697 =( BOUNDED_SURFACE ( )  B_SPLINE_SURFACE ( 1, 2, ( 
 ( #41158, #7546, #106189, #107267, #23803, #24869, #124609, #44349, #157035, #75769, #60577, #8623, #140808, #206820, #6476, #56322, #58454, #76821, #208941, #122482, #126735, #42223, #108340, #25939, #158103, #110471, #159149, #9692, #138651, #141877, #207886, #59509, #28082, #125666, #191628, #109412, #43292, #172214, #10750, #175417, #27001, #188444, #93107, #94178, #72553, #16067, #160217, #147183, #128861, #30221, #95242, #177541, #45418, #130983, #78952, #194843, #111534, #164481, #81094, #179673, #33409, #11818, #63775, #29152, #195922, #178611, #31293, #129934, #127817, #145074, #181776, #15003, #97368, #210008, #163426, #132024, #46476, #196974, #32351, #144015, #47559, #61650, #12876, #77894, #162361, #112600, #113669, #213208, #98416, #48613, #114728, #180726, #115787, #13940, #96305, #198034, #80023, #211077, #82151, #62700, #148243, #146126, #214245, #212139, #161290, #64837, #65876, #49664, #193772, #99487, #50728, #167682, #136267, #19283, #100545, #117932, #135208, #201224, #101615, #52865, #85364, #69087, #66944, #84294, #166618, #118999, #21402, #168747, #34473, #17138, #18210, #182855, #102689, #133084, #200160, #71223, #165545, #153576, #20351, #137338, #187125, #86436, #5146, #152501, #70155, #68011, #134151, #87512, #203355, #83215, #55008, #149297, #116853, #150379, #151446, #3019, #37686, #186051, #4084, #878, #103763, #1950, #51814, #121158, #183926, #199082, #35538, #184977, #36603, #202287, #53939, #120075, #169814, #125419, #188192, #139476, #190321, #24619, #208702, #158911, #90727, #91800, #41980, #174119, #108090, #76580, #105936, #9451, #75522, #7293, #156790, #171960, #141635, #8376, #205505, #74459, #207643, #25692, #59262, #191385, #173037, #142692, #60329, #140564, #206576, #204421, #58204, #89658, #23549, #157858, #154643, #124364, #43051, #109164, #126490, #175176, #38756, #26763, #88586, #104837, #170882, #122232, #92864, #10507, #73371, #22474, #6224, #72294, #138402, #56076, #39827, #155711, #57137, #123305, #189268, #40907, #107013, #28912, #63541, #145893, #46242, #77650, #161043, #128631, #179435, #94997, #211904, #98191, #178372, #214010, #47316, #129696, #27838, #195679, #164239, #12639, #14769, #64604, #176236, #162118, #93934, #45180, #44107, #194598, #78709, #96066, #113429, #130744, #80860, #146950, #212965, #148000, #112359, #144835, #15827, #210843, #177298, #196737, #111293, #48378, #29981, #114490, #62469, #127569, #31056, #13708, #79781, #97132, #192454, #143772, #163184, #180487, #32106, #193538, #81913, #65633, #110228, #159975, #11579, #209767, #61407, #166361, #198838, #184722, #136006, #182598, #202019, #50484, #619, #165295, #34221, #149044, #66687, #35279, #169560, #116605, #200962, #185790, #100294, #150127, #132834, #131781, #115542, #199911, #53678, #119810, #181537, #37423, #1700, #17951, #151192, #84038, #103499, #69894, #51557, #49422, #117683, #67754, #133905, #21142, #183675, #101356, #20092, #167434, #82971, #87245, #19026, #85106, #33165, #99246, #2763, #153311, #4886, #197784, #118738, #68832, #134954, #52609, #36346, #16889, #102424, #168493, #86179, #152249, #3822, #206321, #90463, #158658, #70964, #189009, #170622, #106753, #89399, #156530, #40651, #38498, #204155, #55810, #72033, #172780, #207393, #140303, #5963, #203099, #121964, #154385, #74208, #104576, #171690, #42795, #137074, #125170, #57946, #108904, #54744, #124111, #191129, #190074, #41726, #39561, #105663, #59013, #174927, #120894, #26507, #22208, #88321, #138145, #56880, #123055, #9197, #157602, #107836, #187931, #75269, #23288, #155447, #92616, #7031, #73108, #205239, #24354, #8121, #173861, #25437, #91543, #141383, #96881, #159719, #111034, #161869, #210594, #180240, #130501, #62224, #63284, #13458, #145652, #79534, #48130, #77396, #195428, #47058, #193281, #128382, #143512, #113175, #194349, #177040, #45991, #179179, #211648, #30802, #162931, #144581, #114242, #31864, #112112, #178115, #175985, #29730, #61148, #209508, #129446, #126236, #95812, #14512, #80604, #97940, #146699, #10257, #212715, #60078, #76331, #142437, #93677, #64355, #196488, #44926, #208444, #192196 ),
 ( #109975, #28657, #160790, #43860, #127311, #27578, #11317, #94743, #12382, #78462, #52366, #119557, #17696, #198586, #135758, #116352, #148798, #184476, #16638, #200714, #100047, #36094, #182342, #98991, #2510, #166110, #1443, #101097, #163997, #115296, #83783, #118495, #149876, #165045, #33972, #199655, #51301, #67508, #117426, #133654, #152003, #50232, #82722, #68583, #168245, #368, #19844, #66442, #32914, #197534, #132583, #181287, #183423, #35025, #201780, #167183, #18772, #3575, #84857, #150946, #134708, #15572, #147746, #102178, #85930, #69650, #213764, #53421, #185545, #37174, #81660, #65385, #131531, #49179, #23034, #20894, #171444, #88064, #120641, #91289, #5705, #105407, #206065, #170369, #54497, #41471, #154136, #55563, #86990, #153063, #137897, #8937, #173614, #103249, #90212, #71782, #187683, #38246, #186620, #202849, #73947, #21954, #203916, #104321, #107580, #24110, #122798, #190878, #169310, #6784, #121718, #138967, #39311, #188756, #72860, #70709, #89149, #124914, #172526, #40396, #4638, #106498, #75017, #155203, #140041, #189822, #136822, #204989, #56632, #156277, #7861, #57700, #123856, #25185, #157348, #141127, #207138, #58762, #112918, #145397, #63026, #108646, #174675, #178929, #27320, #30545, #60893, #64101, #11060, #78746, #113464, #99284, #143807, #179469, #66726, #168533, #203143, #199950, #53719, #103539, #659, #201003, #132869, #84080, #83005, #19067, #117721, #134993, #20131, #169599, #119852, #185830, #37461, #186905, #85145, #51597, #54785, #183711, #1736, #21182, #150168, #87285, #167471, #153354, #35318, #166399, #69935, #151232, #68873, #86217, #16925, #182638, #2801, #4924, #52648, #17990, #101397, #118777, #184762, #36389, #102467, #152288, #71001, #3862, #67793, #136047, #137114, #133943, #120932, #202059, #100332, #50520, #38537, #34260, #104614, #149081, #198873, #116643, #25474, #10289, #155487, #189048, #171729, #170662, #154424, #24388, #26541, #92649, #6002, #158691, #40685, #187971, #190107, #23327, #76363, #108938, #90500, #88359, #156564, #7070, #39598, #142470, #73142, #172816, #59044, #89435, #122005, #174959, #139248, #123091, #72073, #138183, #205279, #208478, #60114, #22249, #157633, #56918, #106788, #105701, #8159, #55848, #141418, #74243, #140336, #206355, #204193, #57982, #124145, #41760, #107872, #126273, #42832, #91581, #173898, #192230, #9231, #75303, #43893, #207425, #125202, #191165, #62254, #13490, #96915, #113208, #195461, #127344, #196522, #44960, #210628, #47090, #95847, #65419, #15609, #161903, #162966, #179213, #30838, #14545, #147780, #177074, #80642, #146734, #78496, #79565, #28690, #212752, #145684, #128415, #211682, #64386, #130531, #48165, #114277, #29762, #213796, #131568, #63318, #129479, #61184, #180274, #160824, #94776, #31898, #11350, #97975, #164034, #81697, #197569, #110007, #176020, #27612, #159753, #93712, #77431, #193314, #143548, #209542, #144613, #111068, #12416, #194382, #46025, #112145, #178148, #16673, #100080, #102213, #35060, #136859, #36129, #166142, #200750, #2543, #101131, #148831, #83817, #199691, #168279, #149910, #68618, #169345, #167219, #84891, #82758, #34006, #182376, #150978, #185579, #118526, #1477, #181324, #133686, #51336, #52399, #66476, #184510, #20930, #115333, #103283, #19879, #87026, #49213, #85962, #153098, #152038, #69686, #135790, #201814, #37209, #4673, #32952, #70746, #53458, #99026, #165082, #119596, #88099, #24143, #6818, #7895, #172559, #170402, #121750, #10039, #57735, #73983, #38280, #140077, #174711, #171479, #25221, #75050, #186654, #90245, #104357, #55595, #54531, #56670, #89185, #106533, #206101, #141165, #91324, #157382, #8976, #158438, #122834, #23069, #26286, #155237, #187718, #207173, #72897, #58797, #139002, #124952, #188795, #137927, #41503, #40431, #156311, #123892, #202883, #154172, #189859, #190914, #107616, #203948, #173647, #42579, #108682, #92400, #76113, #120676, #21990, #5739, #209286, #195205, #146479, #193053, #212498, #60933, #11097, #175766, #44707, #159499, #77173, #45775, #180024, #127090, #211434, #196271, #110814, #160565, #143295, #142217, #126015, #210368, #64139 ) ),
 .UNSPECIFIED., .F., .F., .T. ) 
 B_SPLINE_SURFACE_WITH_KNOTS ( ( 2, 2 ),
 ( 3, 2, 2, 2, 2, 2, 2, 2, 2, 2, 2, 2, 2, 2, 2, 2, 2, 2, 2, 2, 2, 2, 2, 2, 2, 2, 2, 2, 2, 2, 2, 2, 2, 2, 2, 2, 2, 2, 2, 2, 2, 2, 2, 2, 2, 2, 2, 2, 2, 2, 2, 2, 2, 2, 2, 2, 2, 2, 2, 2, 2, 2, 2, 2, 2, 2, 2, 2, 2, 2, 2, 2, 2, 2, 2, 2, 2, 2, 2, 2, 2, 2, 2, 2, 2, 2, 2, 2, 2, 2, 2, 2, 2, 2, 2, 2, 2, 2, 2, 2, 2, 2, 2, 2, 2, 2, 2, 2, 2, 2, 2, 2, 2, 2, 2, 2, 2, 2, 2, 2, 2, 2, 2, 2, 2, 2, 2, 2, 2, 2, 2, 2, 2, 2, 2, 2, 2, 2, 2, 2, 2, 2, 2, 2, 2, 2, 2, 2, 2, 2, 2, 2, 2, 2, 2, 2, 2, 2, 2, 2, 2, 2, 2, 2, 2, 2, 2, 2, 2, 2, 2, 2, 2, 2, 2, 2, 2, 2, 2, 2, 2, 2, 2, 2, 2, 2, 2, 2, 2, 2, 2, 2, 2, 2, 2, 2, 2, 2, 2, 2, 2, 2, 2, 2, 2, 2, 2, 2, 2, 2, 2, 2, 2, 2, 2, 2, 2, 2, 2, 2, 2, 2, 2, 2, 2, 2, 2, 2, 2, 2, 2, 2, 2, 2, 2, 2, 2, 2, 2, 2, 3 ),
 ( 0.000000000000000000, 1.000000000000000000 ),
 ( 0.000000000000000000, 0.004166666666666666609, 0.008333333333333333218, 0.01250000000000000069, 0.01666666666666666644, 0.02083333333333333218, 0.02500000000000000139, 0.02916666666666666713, 0.03333333333333333287, 0.03749999999999999861, 0.04166666666666666435, 0.04583333333333333010, 0.05000000000000000278, 0.05416666666666666852, 0.05833333333333333426, 0.06250000000000000000, 0.06666666666666666574, 0.07083333333333333148, 0.07499999999999999722, 0.07916666666666666297, 0.08333333333333332871, 0.08749999999999999445, 0.09166666666666666019, 0.09583333333333333981, 0.1000000000000000056, 0.1041666666666666713, 0.1083333333333333370, 0.1125000000000000028, 0.1166666666666666685, 0.1208333333333333343, 0.1250000000000000000, 0.1291666666666666796, 0.1333333333333333315, 0.1375000000000000111, 0.1416666666666666630, 0.1458333333333333426, 0.1499999999999999944, 0.1541666666666666741, 0.1583333333333333259, 0.1625000000000000056, 0.1666666666666666574, 0.1708333333333333370, 0.1749999999999999889, 0.1791666666666666685, 0.1833333333333333204, 0.1875000000000000000, 0.1916666666666666796, 0.1958333333333333315, 0.2000000000000000111, 0.2041666666666666630, 0.2083333333333333426, 0.2124999999999999944, 0.2166666666666666741, 0.2208333333333333259, 0.2250000000000000056, 0.2291666666666666574, 0.2333333333333333370, 0.2374999999999999889, 0.2416666666666666685, 0.2458333333333333204, 0.2500000000000000000, 0.2541666666666666519, 0.2583333333333333592, 0.2625000000000000111, 0.2666666666666666630, 0.2708333333333333148, 0.2750000000000000222, 0.2791666666666666741, 0.2833333333333333259, 0.2874999999999999778, 0.2916666666666666852, 0.2958333333333333370, 0.2999999999999999889, 0.3041666666666666408, 0.3083333333333333481, 0.3125000000000000000, 0.3166666666666666519, 0.3208333333333333592, 0.3250000000000000111, 0.3291666666666666630, 0.3333333333333333148, 0.3375000000000000222, 0.3416666666666666741, 0.3458333333333333259, 0.3499999999999999778, 0.3541666666666666852, 0.3583333333333333370, 0.3624999999999999889, 0.3666666666666666408, 0.3708333333333333481, 0.3750000000000000000, 0.3791666666666666519, 0.3833333333333333592, 0.3875000000000000111, 0.3916666666666666630, 0.3958333333333333148, 0.4000000000000000222, 0.4041666666666666741, 0.4083333333333333259, 0.4124999999999999778, 0.4166666666666666852, 0.4208333333333333370, 0.4249999999999999889, 0.4291666666666666408, 0.4333333333333333481, 0.4375000000000000000, 0.4416666666666666519, 0.4458333333333333592, 0.4500000000000000111, 0.4541666666666666630, 0.4583333333333333148, 0.4625000000000000222, 0.4666666666666666741, 0.4708333333333333259, 0.4749999999999999778, 0.4791666666666666852, 0.4833333333333333370, 0.4874999999999999889, 0.4916666666666666408, 0.4958333333333333481, 0.5000000000000000000, 0.5041666666666666519, 0.5083333333333333037, 0.5124999999999999556, 0.5166666666666667185, 0.5208333333333333703, 0.5250000000000000222, 0.5291666666666666741, 0.5333333333333333259, 0.5374999999999999778, 0.5416666666666666297, 0.5458333333333332815, 0.5500000000000000444, 0.5541666666666666963, 0.5583333333333333481, 0.5625000000000000000, 0.5666666666666666519, 0.5708333333333333037, 0.5749999999999999556, 0.5791666666666667185, 0.5833333333333333703, 0.5875000000000000222, 0.5916666666666666741, 0.5958333333333333259, 0.5999999999999999778, 0.6041666666666666297, 0.6083333333333332815, 0.6125000000000000444, 0.6166666666666666963, 0.6208333333333333481, 0.6250000000000000000, 0.6291666666666666519, 0.6333333333333333037, 0.6374999999999999556, 0.6416666666666667185, 0.6458333333333333703, 0.6500000000000000222, 0.6541666666666666741, 0.6583333333333333259, 0.6624999999999999778, 0.6666666666666666297, 0.6708333333333332815, 0.6750000000000000444, 0.6791666666666666963, 0.6833333333333333481, 0.6875000000000000000, 0.6916666666666666519, 0.6958333333333333037, 0.6999999999999999556, 0.7041666666666667185, 0.7083333333333333703, 0.7125000000000000222, 0.7166666666666666741, 0.7208333333333333259, 0.7249999999999999778, 0.7291666666666666297, 0.7333333333333332815, 0.7375000000000000444, 0.7416666666666666963, 0.7458333333333333481, 0.7500000000000000000, 0.7541666666666666519, 0.7583333333333333037, 0.7624999999999999556, 0.7666666666666667185, 0.7708333333333333703, 0.7750000000000000222, 0.7791666666666666741, 0.7833333333333333259, 0.7874999999999999778, 0.7916666666666666297, 0.7958333333333332815, 0.8000000000000000444, 0.8041666666666666963, 0.8083333333333333481, 0.8125000000000000000, 0.8166666666666666519, 0.8208333333333333037, 0.8249999999999999556, 0.8291666666666667185, 0.8333333333333333703, 0.8375000000000000222, 0.8416666666666666741, 0.8458333333333333259, 0.8499999999999999778, 0.8541666666666666297, 0.8583333333333332815, 0.8625000000000000444, 0.8666666666666666963, 0.8708333333333333481, 0.8750000000000000000, 0.8791666666666666519, 0.8833333333333333037, 0.8874999999999999556, 0.8916666666666667185, 0.8958333333333333703, 0.9000000000000000222, 0.9041666666666666741, 0.9083333333333333259, 0.9124999999999999778, 0.9166666666666666297, 0.9208333333333332815, 0.9250000000000000444, 0.9291666666666666963, 0.9333333333333333481, 0.9375000000000000000, 0.9416666666666666519, 0.9458333333333333037, 0.9499999999999999556, 0.9541666666666667185, 0.9583333333333333703, 0.9625000000000000222, 0.9666666666666666741, 0.9708333333333333259, 0.9749999999999999778, 0.9791666666666666297, 0.9833333333333332815, 0.9875000000000000444, 0.9916666666666666963, 0.9958333333333333481, 1.000000000000000000 ),
 .UNSPECIFIED. ) 
 GEOMETRIC_REPRESENTATION_ITEM ( )  RATIONAL_B_SPLINE_SURFACE ( (
 ( 1.000000000000000000, 0.8660254037844387076, 1.000000000000000000, 0.8660254037844387076, 1.000000000000000000, 0.8660254037844387076, 1.000000000000000000, 0.8660254037844387076, 1.000000000000000000, 0.8660254037844387076, 1.000000000000000000, 0.8660254037844387076, 1.000000000000000000, 0.8660254037844387076, 1.000000000000000000, 0.8660254037844387076, 1.000000000000000000, 0.8660254037844387076, 1.000000000000000000, 0.8660254037844387076, 1.000000000000000000, 0.8660254037844387076, 1.000000000000000000, 0.8660254037844387076, 1.000000000000000000, 0.8660254037844387076, 1.000000000000000000, 0.8660254037844387076, 1.000000000000000000, 0.8660254037844387076, 1.000000000000000000, 0.8660254037844387076, 1.000000000000000000, 0.8660254037844387076, 1.000000000000000000, 0.8660254037844387076, 1.000000000000000000, 0.8660254037844387076, 1.000000000000000000, 0.8660254037844387076, 1.000000000000000000, 0.8660254037844387076, 1.000000000000000000, 0.8660254037844387076, 1.000000000000000000, 0.8660254037844387076, 1.000000000000000000, 0.8660254037844387076, 1.000000000000000000, 0.8660254037844387076, 1.000000000000000000, 0.8660254037844387076, 1.000000000000000000, 0.8660254037844387076, 1.000000000000000000, 0.8660254037844387076, 1.000000000000000000, 0.8660254037844387076, 1.000000000000000000, 0.8660254037844387076, 1.000000000000000000, 0.8660254037844387076, 1.000000000000000000, 0.8660254037844387076, 1.000000000000000000, 0.8660254037844387076, 1.000000000000000000, 0.8660254037844387076, 1.000000000000000000, 0.8660254037844387076, 1.000000000000000000, 0.8660254037844387076, 1.000000000000000000, 0.8660254037844387076, 1.000000000000000000, 0.8660254037844387076, 1.000000000000000000, 0.8660254037844387076, 1.000000000000000000, 0.8660254037844387076, 1.000000000000000000, 0.8660254037844387076, 1.000000000000000000, 0.8660254037844387076, 1.000000000000000000, 0.8660254037844387076, 1.000000000000000000, 0.8660254037844387076, 1.000000000000000000, 0.8660254037844387076, 1.000000000000000000, 0.8660254037844387076, 1.000000000000000000, 0.8660254037844387076, 1.000000000000000000, 0.8660254037844387076, 1.000000000000000000, 0.8660254037844387076, 1.000000000000000000, 0.8660254037844387076, 1.000000000000000000, 0.8660254037844387076, 1.000000000000000000, 0.8660254037844387076, 1.000000000000000000, 0.8660254037844387076, 1.000000000000000000, 0.8660254037844387076, 1.000000000000000000, 0.8660254037844387076, 1.000000000000000000, 0.8660254037844387076, 1.000000000000000000, 0.8660254037844387076, 1.000000000000000000, 0.8660254037844387076, 1.000000000000000000, 0.8660254037844387076, 1.000000000000000000, 0.8660254037844387076, 1.000000000000000000, 0.8660254037844387076, 1.000000000000000000, 0.8660254037844387076, 1.000000000000000000, 0.8660254037844387076, 1.000000000000000000, 0.8660254037844387076, 1.000000000000000000, 0.8660254037844387076, 1.000000000000000000, 0.8660254037844387076, 1.000000000000000000, 0.8660254037844387076, 1.000000000000000000, 0.8660254037844387076, 1.000000000000000000, 0.8660254037844387076, 1.000000000000000000, 0.8660254037844387076, 1.000000000000000000, 0.8660254037844387076, 1.000000000000000000, 0.8660254037844387076, 1.000000000000000000, 0.8660254037844387076, 1.000000000000000000, 0.8660254037844387076, 1.000000000000000000, 0.8660254037844387076, 1.000000000000000000, 0.8660254037844387076, 1.000000000000000000, 0.8660254037844387076, 1.000000000000000000, 0.8660254037844387076, 1.000000000000000000, 0.8660254037844387076, 1.000000000000000000, 0.8660254037844387076, 1.000000000000000000, 0.8660254037844387076, 1.000000000000000000, 0.8660254037844387076, 1.000000000000000000, 0.8660254037844387076, 1.000000000000000000, 0.8660254037844387076, 1.000000000000000000, 0.8660254037844387076, 1.000000000000000000, 0.8660254037844387076, 1.000000000000000000, 0.8660254037844387076, 1.000000000000000000, 0.8660254037844387076, 1.000000000000000000, 0.8660254037844387076, 1.000000000000000000, 0.8660254037844387076, 1.000000000000000000, 0.8660254037844387076, 1.000000000000000000, 0.8660254037844387076, 1.000000000000000000, 0.8660254037844387076, 1.000000000000000000, 0.8660254037844387076, 1.000000000000000000, 0.8660254037844387076, 1.000000000000000000, 0.8660254037844387076, 1.000000000000000000, 0.8660254037844387076, 1.000000000000000000, 0.8660254037844387076, 1.000000000000000000, 0.8660254037844387076, 1.000000000000000000, 0.8660254037844387076, 1.000000000000000000, 0.8660254037844387076, 1.000000000000000000, 0.8660254037844387076, 1.000000000000000000, 0.8660254037844387076, 1.000000000000000000, 0.8660254037844387076, 1.000000000000000000, 0.8660254037844387076, 1.000000000000000000, 0.8660254037844387076, 1.000000000000000000, 0.8660254037844387076, 1.000000000000000000, 0.8660254037844387076, 1.000000000000000000, 0.8660254037844387076, 1.000000000000000000, 0.8660254037844387076, 1.000000000000000000, 0.8660254037844387076, 1.000000000000000000, 0.8660254037844387076, 1.000000000000000000, 0.8660254037844387076, 1.000000000000000000, 0.8660254037844387076, 1.000000000000000000, 0.8660254037844387076, 1.000000000000000000, 0.8660254037844387076, 1.000000000000000000, 0.8660254037844387076, 1.000000000000000000, 0.8660254037844387076, 1.000000000000000000, 0.8660254037844387076, 1.000000000000000000, 0.8660254037844387076, 1.000000000000000000, 0.8660254037844387076, 1.000000000000000000, 0.8660254037844387076, 1.000000000000000000, 0.8660254037844387076, 1.000000000000000000, 0.8660254037844387076, 1.000000000000000000, 0.8660254037844387076, 1.000000000000000000, 0.8660254037844387076, 1.000000000000000000, 0.8660254037844387076, 1.000000000000000000, 0.8660254037844387076, 1.000000000000000000, 0.8660254037844387076, 1.000000000000000000, 0.8660254037844387076, 1.000000000000000000, 0.8660254037844387076, 1.000000000000000000, 0.8660254037844387076, 1.000000000000000000, 0.8660254037844387076, 1.000000000000000000, 0.8660254037844387076, 1.000000000000000000, 0.8660254037844387076, 1.000000000000000000, 0.8660254037844387076, 1.000000000000000000, 0.8660254037844387076, 1.000000000000000000, 0.8660254037844387076, 1.000000000000000000, 0.8660254037844387076, 1.000000000000000000, 0.8660254037844387076, 1.000000000000000000, 0.8660254037844387076, 1.000000000000000000, 0.8660254037844387076, 1.000000000000000000, 0.8660254037844387076, 1.000000000000000000, 0.8660254037844387076, 1.000000000000000000, 0.8660254037844387076, 1.000000000000000000, 0.8660254037844387076, 1.000000000000000000, 0.8660254037844387076, 1.000000000000000000, 0.8660254037844387076, 1.000000000000000000, 0.8660254037844387076, 1.000000000000000000, 0.8660254037844387076, 1.000000000000000000, 0.8660254037844387076, 1.000000000000000000, 0.8660254037844387076, 1.000000000000000000, 0.8660254037844387076, 1.000000000000000000, 0.8660254037844387076, 1.000000000000000000, 0.8660254037844387076, 1.000000000000000000, 0.8660254037844387076, 1.000000000000000000, 0.8660254037844387076, 1.000000000000000000, 0.8660254037844387076, 1.000000000000000000, 0.8660254037844387076, 1.000000000000000000, 0.8660254037844387076, 1.000000000000000000, 0.8660254037844387076, 1.000000000000000000, 0.8660254037844387076, 1.000000000000000000, 0.8660254037844387076, 1.000000000000000000, 0.8660254037844387076, 1.000000000000000000, 0.8660254037844387076, 1.000000000000000000, 0.8660254037844387076, 1.000000000000000000, 0.8660254037844387076, 1.000000000000000000, 0.8660254037844387076, 1.000000000000000000, 0.8660254037844387076, 1.000000000000000000, 0.8660254037844387076, 1.000000000000000000, 0.8660254037844387076, 1.000000000000000000, 0.8660254037844387076, 1.000000000000000000, 0.8660254037844387076, 1.000000000000000000, 0.8660254037844387076, 1.000000000000000000, 0.8660254037844387076, 1.000000000000000000, 0.8660254037844387076, 1.000000000000000000, 0.8660254037844387076, 1.000000000000000000, 0.8660254037844387076, 1.000000000000000000, 0.8660254037844387076, 1.000000000000000000, 0.8660254037844387076, 1.000000000000000000, 0.8660254037844387076, 1.000000000000000000, 0.8660254037844387076, 1.000000000000000000, 0.8660254037844387076, 1.000000000000000000, 0.8660254037844387076, 1.000000000000000000, 0.8660254037844387076, 1.000000000000000000, 0.8660254037844387076, 1.000000000000000000, 0.8660254037844387076, 1.000000000000000000, 0.8660254037844387076, 1.000000000000000000, 0.8660254037844387076, 1.000000000000000000, 0.8660254037844387076, 1.000000000000000000, 0.8660254037844387076, 1.000000000000000000, 0.8660254037844387076, 1.000000000000000000, 0.8660254037844387076, 1.000000000000000000, 0.8660254037844387076, 1.000000000000000000, 0.8660254037844387076, 1.000000000000000000, 0.8660254037844387076, 1.000000000000000000, 0.8660254037844387076, 1.000000000000000000, 0.8660254037844387076, 1.000000000000000000, 0.8660254037844387076, 1.000000000000000000, 0.8660254037844387076, 1.000000000000000000, 0.8660254037844387076, 1.000000000000000000, 0.8660254037844387076, 1.000000000000000000, 0.8660254037844387076, 1.000000000000000000, 0.8660254037844387076, 1.000000000000000000, 0.8660254037844387076, 1.000000000000000000, 0.8660254037844387076, 1.000000000000000000, 0.8660254037844387076, 1.000000000000000000, 0.8660254037844387076, 1.000000000000000000, 0.8660254037844387076, 1.000000000000000000, 0.8660254037844387076, 1.000000000000000000, 0.8660254037844387076, 1.000000000000000000, 0.8660254037844387076, 1.000000000000000000, 0.8660254037844387076, 1.000000000000000000, 0.8660254037844387076, 1.000000000000000000, 0.8660254037844387076, 1.000000000000000000, 0.8660254037844387076, 1.000000000000000000, 0.8660254037844387076, 1.000000000000000000, 0.8660254037844387076, 1.000000000000000000, 0.8660254037844387076, 1.000000000000000000, 0.8660254037844387076, 1.000000000000000000, 0.8660254037844387076, 1.000000000000000000, 0.8660254037844387076, 1.000000000000000000, 0.8660254037844387076, 1.000000000000000000, 0.8660254037844387076, 1.000000000000000000, 0.8660254037844387076, 1.000000000000000000, 0.8660254037844387076, 1.000000000000000000, 0.8660254037844387076, 1.000000000000000000, 0.8660254037844387076, 1.000000000000000000, 0.8660254037844387076, 1.000000000000000000, 0.8660254037844387076, 1.000000000000000000, 0.8660254037844387076, 1.000000000000000000, 0.8660254037844387076, 1.000000000000000000, 0.8660254037844387076, 1.000000000000000000, 0.8660254037844387076, 1.000000000000000000, 0.8660254037844387076, 1.000000000000000000, 0.8660254037844387076, 1.000000000000000000, 0.8660254037844387076, 1.000000000000000000, 0.8660254037844387076, 1.000000000000000000, 0.8660254037844387076, 1.000000000000000000, 0.8660254037844387076, 1.000000000000000000),
 ( 1.000000000000000000, 0.8660254037844387076, 1.000000000000000000, 0.8660254037844387076, 1.000000000000000000, 0.8660254037844387076, 1.000000000000000000, 0.8660254037844387076, 1.000000000000000000, 0.8660254037844387076, 1.000000000000000000, 0.8660254037844387076, 1.000000000000000000, 0.8660254037844387076, 1.000000000000000000, 0.8660254037844387076, 1.000000000000000000, 0.8660254037844387076, 1.000000000000000000, 0.8660254037844387076, 1.000000000000000000, 0.8660254037844387076, 1.000000000000000000, 0.8660254037844387076, 1.000000000000000000, 0.8660254037844387076, 1.000000000000000000, 0.8660254037844387076, 1.000000000000000000, 0.8660254037844387076, 1.000000000000000000, 0.8660254037844387076, 1.000000000000000000, 0.8660254037844387076, 1.000000000000000000, 0.8660254037844387076, 1.000000000000000000, 0.8660254037844387076, 1.000000000000000000, 0.8660254037844387076, 1.000000000000000000, 0.8660254037844387076, 1.000000000000000000, 0.8660254037844387076, 1.000000000000000000, 0.8660254037844387076, 1.000000000000000000, 0.8660254037844387076, 1.000000000000000000, 0.8660254037844387076, 1.000000000000000000, 0.8660254037844387076, 1.000000000000000000, 0.8660254037844387076, 1.000000000000000000, 0.8660254037844387076, 1.000000000000000000, 0.8660254037844387076, 1.000000000000000000, 0.8660254037844387076, 1.000000000000000000, 0.8660254037844387076, 1.000000000000000000, 0.8660254037844387076, 1.000000000000000000, 0.8660254037844387076, 1.000000000000000000, 0.8660254037844387076, 1.000000000000000000, 0.8660254037844387076, 1.000000000000000000, 0.8660254037844387076, 1.000000000000000000, 0.8660254037844387076, 1.000000000000000000, 0.8660254037844387076, 1.000000000000000000, 0.8660254037844387076, 1.000000000000000000, 0.8660254037844387076, 1.000000000000000000, 0.8660254037844387076, 1.000000000000000000, 0.8660254037844387076, 1.000000000000000000, 0.8660254037844387076, 1.000000000000000000, 0.8660254037844387076, 1.000000000000000000, 0.8660254037844387076, 1.000000000000000000, 0.8660254037844387076, 1.000000000000000000, 0.8660254037844387076, 1.000000000000000000, 0.8660254037844387076, 1.000000000000000000, 0.8660254037844387076, 1.000000000000000000, 0.8660254037844387076, 1.000000000000000000, 0.8660254037844387076, 1.000000000000000000, 0.8660254037844387076, 1.000000000000000000, 0.8660254037844387076, 1.000000000000000000, 0.8660254037844387076, 1.000000000000000000, 0.8660254037844387076, 1.000000000000000000, 0.8660254037844387076, 1.000000000000000000, 0.8660254037844387076, 1.000000000000000000, 0.8660254037844387076, 1.000000000000000000, 0.8660254037844387076, 1.000000000000000000, 0.8660254037844387076, 1.000000000000000000, 0.8660254037844387076, 1.000000000000000000, 0.8660254037844387076, 1.000000000000000000, 0.8660254037844387076, 1.000000000000000000, 0.8660254037844387076, 1.000000000000000000, 0.8660254037844387076, 1.000000000000000000, 0.8660254037844387076, 1.000000000000000000, 0.8660254037844387076, 1.000000000000000000, 0.8660254037844387076, 1.000000000000000000, 0.8660254037844387076, 1.000000000000000000, 0.8660254037844387076, 1.000000000000000000, 0.8660254037844387076, 1.000000000000000000, 0.8660254037844387076, 1.000000000000000000, 0.8660254037844387076, 1.000000000000000000, 0.8660254037844387076, 1.000000000000000000, 0.8660254037844387076, 1.000000000000000000, 0.8660254037844387076, 1.000000000000000000, 0.8660254037844387076, 1.000000000000000000, 0.8660254037844387076, 1.000000000000000000, 0.8660254037844387076, 1.000000000000000000, 0.8660254037844387076, 1.000000000000000000, 0.8660254037844387076, 1.000000000000000000, 0.8660254037844387076, 1.000000000000000000, 0.8660254037844387076, 1.000000000000000000, 0.8660254037844387076, 1.000000000000000000, 0.8660254037844387076, 1.000000000000000000, 0.8660254037844387076, 1.000000000000000000, 0.8660254037844387076, 1.000000000000000000, 0.8660254037844387076, 1.000000000000000000, 0.8660254037844387076, 1.000000000000000000, 0.8660254037844387076, 1.000000000000000000, 0.8660254037844387076, 1.000000000000000000, 0.8660254037844387076, 1.000000000000000000, 0.8660254037844387076, 1.000000000000000000, 0.8660254037844387076, 1.000000000000000000, 0.8660254037844387076, 1.000000000000000000, 0.8660254037844387076, 1.000000000000000000, 0.8660254037844387076, 1.000000000000000000, 0.8660254037844387076, 1.000000000000000000, 0.8660254037844387076, 1.000000000000000000, 0.8660254037844387076, 1.000000000000000000, 0.8660254037844387076, 1.000000000000000000, 0.8660254037844387076, 1.000000000000000000, 0.8660254037844387076, 1.000000000000000000, 0.8660254037844387076, 1.000000000000000000, 0.8660254037844387076, 1.000000000000000000, 0.8660254037844387076, 1.000000000000000000, 0.8660254037844387076, 1.000000000000000000, 0.8660254037844387076, 1.000000000000000000, 0.8660254037844387076, 1.000000000000000000, 0.8660254037844387076, 1.000000000000000000, 0.8660254037844387076, 1.000000000000000000, 0.8660254037844387076, 1.000000000000000000, 0.8660254037844387076, 1.000000000000000000, 0.8660254037844387076, 1.000000000000000000, 0.8660254037844387076, 1.000000000000000000, 0.8660254037844387076, 1.000000000000000000, 0.8660254037844387076, 1.000000000000000000, 0.8660254037844387076, 1.000000000000000000, 0.8660254037844387076, 1.000000000000000000, 0.8660254037844387076, 1.000000000000000000, 0.8660254037844387076, 1.000000000000000000, 0.8660254037844387076, 1.000000000000000000, 0.8660254037844387076, 1.000000000000000000, 0.8660254037844387076, 1.000000000000000000, 0.8660254037844387076, 1.000000000000000000, 0.8660254037844387076, 1.000000000000000000, 0.8660254037844387076, 1.000000000000000000, 0.8660254037844387076, 1.000000000000000000, 0.8660254037844387076, 1.000000000000000000, 0.8660254037844387076, 1.000000000000000000, 0.8660254037844387076, 1.000000000000000000, 0.8660254037844387076, 1.000000000000000000, 0.8660254037844387076, 1.000000000000000000, 0.8660254037844387076, 1.000000000000000000, 0.8660254037844387076, 1.000000000000000000, 0.8660254037844387076, 1.000000000000000000, 0.8660254037844387076, 1.000000000000000000, 0.8660254037844387076, 1.000000000000000000, 0.8660254037844387076, 1.000000000000000000, 0.8660254037844387076, 1.000000000000000000, 0.8660254037844387076, 1.000000000000000000, 0.8660254037844387076, 1.000000000000000000, 0.8660254037844387076, 1.000000000000000000, 0.8660254037844387076, 1.000000000000000000, 0.8660254037844387076, 1.000000000000000000, 0.8660254037844387076, 1.000000000000000000, 0.8660254037844387076, 1.000000000000000000, 0.8660254037844387076, 1.000000000000000000, 0.8660254037844387076, 1.000000000000000000, 0.8660254037844387076, 1.000000000000000000, 0.8660254037844387076, 1.000000000000000000, 0.8660254037844387076, 1.000000000000000000, 0.8660254037844387076, 1.000000000000000000, 0.8660254037844387076, 1.000000000000000000, 0.8660254037844387076, 1.000000000000000000, 0.8660254037844387076, 1.000000000000000000, 0.8660254037844387076, 1.000000000000000000, 0.8660254037844387076, 1.000000000000000000, 0.8660254037844387076, 1.000000000000000000, 0.8660254037844387076, 1.000000000000000000, 0.8660254037844387076, 1.000000000000000000, 0.8660254037844387076, 1.000000000000000000, 0.8660254037844387076, 1.000000000000000000, 0.8660254037844387076, 1.000000000000000000, 0.8660254037844387076, 1.000000000000000000, 0.8660254037844387076, 1.000000000000000000, 0.8660254037844387076, 1.000000000000000000, 0.8660254037844387076, 1.000000000000000000, 0.8660254037844387076, 1.000000000000000000, 0.8660254037844387076, 1.000000000000000000, 0.8660254037844387076, 1.000000000000000000, 0.8660254037844387076, 1.000000000000000000, 0.8660254037844387076, 1.000000000000000000, 0.8660254037844387076, 1.000000000000000000, 0.8660254037844387076, 1.000000000000000000, 0.8660254037844387076, 1.000000000000000000, 0.8660254037844387076, 1.000000000000000000, 0.8660254037844387076, 1.000000000000000000, 0.8660254037844387076, 1.000000000000000000, 0.8660254037844387076, 1.000000000000000000, 0.8660254037844387076, 1.000000000000000000, 0.8660254037844387076, 1.000000000000000000, 0.8660254037844387076, 1.000000000000000000, 0.8660254037844387076, 1.000000000000000000, 0.8660254037844387076, 1.000000000000000000, 0.8660254037844387076, 1.000000000000000000, 0.8660254037844387076, 1.000000000000000000, 0.8660254037844387076, 1.000000000000000000, 0.8660254037844387076, 1.000000000000000000, 0.8660254037844387076, 1.000000000000000000, 0.8660254037844387076, 1.000000000000000000, 0.8660254037844387076, 1.000000000000000000, 0.8660254037844387076, 1.000000000000000000, 0.8660254037844387076, 1.000000000000000000, 0.8660254037844387076, 1.000000000000000000, 0.8660254037844387076, 1.000000000000000000, 0.8660254037844387076, 1.000000000000000000, 0.8660254037844387076, 1.000000000000000000, 0.8660254037844387076, 1.000000000000000000, 0.8660254037844387076, 1.000000000000000000, 0.8660254037844387076, 1.000000000000000000, 0.8660254037844387076, 1.000000000000000000, 0.8660254037844387076, 1.000000000000000000, 0.8660254037844387076, 1.000000000000000000, 0.8660254037844387076, 1.000000000000000000, 0.8660254037844387076, 1.000000000000000000, 0.8660254037844387076, 1.000000000000000000, 0.8660254037844387076, 1.000000000000000000, 0.8660254037844387076, 1.000000000000000000, 0.8660254037844387076, 1.000000000000000000, 0.8660254037844387076, 1.000000000000000000, 0.8660254037844387076, 1.000000000000000000, 0.8660254037844387076, 1.000000000000000000, 0.8660254037844387076, 1.000000000000000000, 0.8660254037844387076, 1.000000000000000000, 0.8660254037844387076, 1.000000000000000000, 0.8660254037844387076, 1.000000000000000000, 0.8660254037844387076, 1.000000000000000000, 0.8660254037844387076, 1.000000000000000000, 0.8660254037844387076, 1.000000000000000000, 0.8660254037844387076, 1.000000000000000000, 0.8660254037844387076, 1.000000000000000000, 0.8660254037844387076, 1.000000000000000000, 0.8660254037844387076, 1.000000000000000000, 0.8660254037844387076, 1.000000000000000000, 0.8660254037844387076, 1.000000000000000000, 0.8660254037844387076, 1.000000000000000000, 0.8660254037844387076, 1.000000000000000000, 0.8660254037844387076, 1.000000000000000000, 0.8660254037844387076, 1.000000000000000000, 0.8660254037844387076, 1.000000000000000000, 0.8660254037844387076, 1.000000000000000000, 0.8660254037844387076, 1.000000000000000000, 0.8660254037844387076, 1.000000000000000000, 0.8660254037844387076, 1.000000000000000000, 0.8660254037844387076, 1.000000000000000000, 0.8660254037844387076, 1.000000000000000000, 0.8660254037844387076, 1.000000000000000000, 0.8660254037844387076, 1.000000000000000000, 0.8660254037844387076, 1.000000000000000000) ) ) 
 REPRESENTATION_ITEM ( '' )  SURFACE ( )  );
#129698 = CARTESIAN_POINT ( 'NONE',  ( 2.601940685209406467, 1.502730264585940168, 1.496503045097858919 ) ) ;
#129699 = CARTESIAN_POINT ( 'NONE',  ( -3.962726036944197894, 7.845207153068690431, -0.7998128361456481317 ) ) ;
#129700 = CARTESIAN_POINT ( 'NONE',  ( 4.100566281481184738, -0.6756360485904688851, -2.053482476349233643 ) ) ;
#129701 = CARTESIAN_POINT ( 'NONE',  ( 2.981803241483144795, -1.814435276338403735, -0.3121031562058202424 ) ) ;
#129702 = CARTESIAN_POINT ( 'NONE',  ( -4.305726085941478765, 7.254707473775878768, 0.9719050602644065950 ) ) ;
#129703 = CARTESIAN_POINT ( 'NONE',  ( 1.364683531249986537, -0.07395833299191513499, 0.7879004041258500513 ) ) ;
#129704 = CARTESIAN_POINT ( 'NONE',  ( 5.542807930227759527, -1.375536301258666105, -1.066015508636003251 ) ) ;
#129705 = CARTESIAN_POINT ( 'NONE',  ( 6.727182134110231360, 6.039168392632435989, 2.405853653942995773 ) ) ;
#129706 = CARTESIAN_POINT ( 'NONE',  ( 5.368665641331531013, 5.365790791082654998, -0.7216878364870207285 ) ) ;
#129707 = CARTESIAN_POINT ( 'NONE',  ( 1.499999999999990896, 3.556250000682818602, 1.214306433183764966E-14 ) ) ;
#129708 = CARTESIAN_POINT ( 'NONE',  ( 2.676834871759771417, -2.068302492614528365, -0.6285112194897370941 ) ) ;
#129709 = CARTESIAN_POINT ( 'NONE',  ( 4.200545946899570282, -1.388273439763810790, -1.462221600879671790 ) ) ;
#129710 = CARTESIAN_POINT ( 'NONE',  ( -9.775065565328612038, 10.50659070241261794, -0.7216878364870267237 ) ) ;
#129711 = CARTESIAN_POINT ( 'NONE',  ( 2.764712544972968811, -1.491509591961351910, 1.564943835847030229 ) ) ;
#129712 = CARTESIAN_POINT ( 'NONE',  ( 3.057844483195955032, 1.962173284599289858, -0.1898399627659839439 ) ) ;
#129713 = CARTESIAN_POINT ( 'NONE',  ( -6.512525376672311239, 6.817996978042812906, 0.6578840964387155932 ) ) ;
#129714 = CARTESIAN_POINT ( 'NONE',  ( 4.968278857500742163, -1.829972417919925265, -0.6506317318197059052 ) ) ;
#129718 = VERTEX_POINT ( 'NONE', #143192 ) ;
#129717 = EDGE_CURVE ( 'NONE', #152917, #1432, #10988, .T. ) ;
#129716 = CARTESIAN_POINT ( 'NONE',  ( 0.000000000000000000, 3.500000000000003109, 0.000000000000000000 ) ) ;
#129715 = CARTESIAN_POINT ( 'NONE',  ( -9.124274191872645545, 9.747334100047323702, -0.7216878364870267237 ) ) ;
#129719 = CARTESIAN_POINT ( 'NONE',  ( -6.851666526859749418, 9.086973262793417661, -1.599625672291271394 ) ) ;
#129720 = CARTESIAN_POINT ( 'NONE',  ( 5.096939404094710468, 4.911127157724081371, 0.000000000000000000 ) ) ;
#129722 = ORIENTED_EDGE ( 'NONE', *, *, #425, .F. ) ;
#129721 = CARTESIAN_POINT ( 'NONE',  ( -6.154475385960665790, 6.144919136567696505, 0.000000000000000000 ) ) ;
#129723 = CARTESIAN_POINT ( 'NONE',  ( -9.015808962963337336, 10.58116054728778366, 1.082531754730558626 ) ) ;
#129724 = CARTESIAN_POINT ( 'NONE',  ( 1.448561363430532989, 2.204290700723564811, 0.1073905156721635390 ) ) ;
#129725 = CARTESIAN_POINT ( 'NONE',  ( 1.642778471875000035, -0.9260416661887073131, -2.845375778867859751 ) ) ;
#129726 = CARTESIAN_POINT ( 'NONE',  ( 4.750807836863311095, -0.4258335417525476729, -1.914832529679215023 ) ) ;
#129727 = CARTESIAN_POINT ( 'NONE',  ( -1.364683531250010295, 5.801041667008088432, -0.7879004041258300672 ) ) ;
#129728 = CARTESIAN_POINT ( 'NONE',  ( -0.7499999999999972244, 4.889583334016150751, -1.299038105676652899 ) ) ;
#129729 = CARTESIAN_POINT ( 'NONE',  ( 5.196774945655527667, 6.645529799594804388, -1.392961322168507765 ) ) ;
#129730 = CARTESIAN_POINT ( 'NONE',  ( 4.543390873910903238, 7.354354215321133204, 1.082531754730548412 ) ) ;
#129731 = CARTESIAN_POINT ( 'NONE',  ( 3.943160212656390051, 0.6185462545997170158, -1.734258544408360248 ) ) ;
#129732 = ORIENTED_EDGE ( 'NONE', *, *, #97488, .F. ) ;
#129733 = CARTESIAN_POINT ( 'NONE',  ( -0.6801582343750213200, -0.4010416663252705516, -1.178068619123886718 ) ) ;
#129734 = EDGE_CURVE ( 'NONE', #1301, #146171, #115224, .T. ) ;
#129735 = CARTESIAN_POINT ( 'NONE',  ( -6.482770005628665011, 10.71498210654212002, 0.7998128361456481317 ) ) ;
#129736 = CARTESIAN_POINT ( 'NONE',  ( -0.9782388782689256379, 3.999999999999989786, 0.3999999999999559464 ) ) ;
#129737 = CARTESIAN_POINT ( 'NONE',  ( 5.924112389714110805, -2.104401743431310923, 0.2612745606217213856 ) ) ;
#129738 = CARTESIAN_POINT ( 'NONE',  ( 8.837199670533893325, 13.05657914357218274, -8.050043542826816889 ) ) ;
#129739 = CARTESIAN_POINT ( 'NONE',  ( 6.647575389402066826, 6.649926130590872120, 1.040834085586084257E-14 ) ) ;
#129740 = CARTESIAN_POINT ( 'NONE',  ( 6.432896526414161542, 0.1972406338010060101, 2.051297006214629182 ) ) ;
#129743 = CARTESIAN_POINT ( 'NONE',  ( 3.983814121021773680, -1.821778379405362136, -0.2661574599523569007 ) ) ;
#129742 = CARTESIAN_POINT ( 'NONE',  ( 2.453354322281832811, 1.436274109216955752, 1.183453651933939588 ) ) ;
#129741 = CARTESIAN_POINT ( 'NONE',  ( 9.348381460497192208, 13.52536904890506797, 7.450314784081282227 ) ) ;
#129744 = CARTESIAN_POINT ( 'NONE',  ( 9.094822116668764167, 9.505047312402055582, 0.7998128361456462443 ) ) ;
#129745 = CARTESIAN_POINT ( 'NONE',  ( -11.40591166468356654, 3.507114751586590362, 3.706005353348402753 ) ) ;
#129746 = CARTESIAN_POINT ( 'NONE',  ( -6.688968683495758683, 8.897159112202094988, -1.599625672291271394 ) ) ;
#129747 = CARTESIAN_POINT ( 'NONE',  ( 5.339274934379806019E-16, -0.5000000000000004441, -3.000000000000010214 ) ) ;
#129748 = CARTESIAN_POINT ( 'NONE',  ( 3.739080281021701868, 0.3231575147602770426, 2.182976880621155136 ) ) ;
#129749 = CARTESIAN_POINT ( 'NONE',  ( 5.712299329104530088, -1.009927678917849736, -2.024548151048012556 ) ) ;
#129750 = CARTESIAN_POINT ( 'NONE',  ( -6.724481002698130538, 7.907944593645035880, -1.082531754730544860 ) ) ;
#129751 = CARTESIAN_POINT ( 'NONE',  ( 5.976795019380008789, -1.274598912183276589, 1.287626877918945922 ) ) ;
#129752 = CARTESIAN_POINT ( 'NONE',  ( 5.753135696777640362, 0.1336808224800915823, -1.911095040969860825 ) ) ;
#129753 = CARTESIAN_POINT ( 'NONE',  ( 7.334597915313080918, 9.580116872663850813, 1.040834085586084257E-14 ) ) ;
#129754 = CARTESIAN_POINT ( 'NONE',  ( 6.561405567229332547, 0.3174558530528898692, -1.843364171016811603 ) ) ;
#129755 = CARTESIAN_POINT ( 'NONE',  ( 5.793359732304666387, -1.682316520808274429, 0.7960761923023454978 ) ) ;
#129756 = CARTESIAN_POINT ( 'NONE',  ( -1.500000000000015099, 12.97916666666666963, -0.8660254037844309360 ) ) ;
#129757 = EDGE_CURVE ( 'NONE', #33851, #81409, #146272, .T. ) ;
#129758 = CARTESIAN_POINT ( 'NONE',  ( 6.819227944281511355, -0.1297537616256147774, 1.740395163524804945 ) ) ;
#129759 = CARTESIAN_POINT ( 'NONE',  ( 1.604704241733472037, 1.883313803065278513, 0.7212895827233902768 ) ) ;
#129761 = CARTESIAN_POINT ( 'NONE',  ( 2.578859754595532294, -2.015555182639038101, -0.6107849380157669428 ) ) ;
#129760 = CARTESIAN_POINT ( 'NONE',  ( -9.840520565420403543, 10.37502883594562597, 1.040834085586084257E-14 ) ) ;
#129762 = VECTOR ( 'NONE', #168923, 1000.000000000000114 ) ;
#129763 = CARTESIAN_POINT ( 'NONE',  ( 9.260382613333817403, 10.76253345609967660, -1.199719254218446718 ) ) ;
#129765 = CARTESIAN_POINT ( 'NONE',  ( -10.16591625214838679, 10.75465713712827487, 1.040834085586084257E-14 ) ) ;
#129764 = CARTESIAN_POINT ( 'NONE',  ( 0.000000000000000000, 0.000000000000000000, 0.000000000000000000 ) ) ;
#129766 =( NAMED_UNIT ( * ) SI_UNIT ( $, .STERADIAN. ) SOLID_ANGLE_UNIT ( ) );
#129767 = CARTESIAN_POINT ( 'NONE',  ( 2.935811755974365500, -1.945362344549756539, 0.5428778075214285570 ) ) ;
#129768 = CARTESIAN_POINT ( 'NONE',  ( 1.364683531249988535, 3.155208333674756283, -0.7879004041258239610 ) ) ;
#129769 = CARTESIAN_POINT ( 'NONE',  ( 2.496672843210871129, 6.064535417054653266, -0.7998128361456291469 ) ) ;
#129770 = CARTESIAN_POINT ( 'NONE',  ( 3.655696586050953378, 0.5291108212043382775, -2.095698868369605616 ) ) ;
#129771 = CARTESIAN_POINT ( 'NONE',  ( 8.025500584646550806, 8.327781868367935658, 0.000000000000000000 ) ) ;
#129773 = CYLINDRICAL_SURFACE ( 'NONE', #200610, 3.475000000000000089 ) ;
#129772 = CARTESIAN_POINT ( 'NONE',  ( 5.885121196783658526, 9.023669275293071834, 1.199719254218452047 ) ) ;
#129774 = CARTESIAN_POINT ( 'NONE',  ( 10.20892648096591770, 11.01276177065614981, -0.7216878364870257245 ) ) ;
#129776 = DIRECTION ( 'NONE',  ( -5.551115123125765446E-17, 0.000000000000000000, 1.000000000000000000 ) ) ;
#129775 = CARTESIAN_POINT ( 'NONE',  ( 0.7136160920222310855, -1.834322530278935215, -1.161324927271490060 ) ) ;
#129777 = AXIS2_PLACEMENT_3D ( 'NONE', #25161, #157322, #9977 ) ;
#129778 = CARTESIAN_POINT ( 'NONE',  ( -5.572037945536512105, 9.444535336527177805, 0.000000000000000000 ) ) ;
#129779 = CARTESIAN_POINT ( 'NONE',  ( -1.364683531250012516, 0.7802083336747528408, 0.7879004041258379498 ) ) ;
#129780 = CARTESIAN_POINT ( 'NONE',  ( 2.120887600855193345, 0.003649250790785373531, 2.191739723551556551 ) ) ;
#129781 = CARTESIAN_POINT ( 'NONE',  ( 0.07021666366551572447, 7.008523639393767546, 2.000250312771564065 ) ) ;
#129782 = CARTESIAN_POINT ( 'NONE',  ( 2.483610925836767791, 2.068663895631245531, -0.9166773448976636152 ) ) ;
#129783 = CARTESIAN_POINT ( 'NONE',  ( -6.347188469492005325, 10.55680364771601809, -0.7998128361456291469 ) ) ;
#129784 = CARTESIAN_POINT ( 'NONE',  ( -2.914639836813632812, 6.344237543017112735, 0.7216878364870317197 ) ) ;
#129785 = CARTESIAN_POINT ( 'NONE',  ( 1.364683531249990311, 3.946875000341417028, 1.214306433183764966E-14 ) ) ;
#129786 = CARTESIAN_POINT ( 'NONE',  ( 5.324837791525375508, 7.612559486139466536, 1.234112182050936646 ) ) ;
#129787 = CARTESIAN_POINT ( 'NONE',  ( 0.7500000000000006661, 11.08333333333333393, 1.299038105676657340 ) ) ;
#129788 = CARTESIAN_POINT ( 'NONE',  ( 6.590672070018850803, 7.822110515511036866, -1.082531754730548412 ) ) ;
#129789 = CARTESIAN_POINT ( 'NONE',  ( 2.987294507434365087, 1.248747198882380394, 1.254300180652974550 ) ) ;
#129790 = EDGE_CURVE ( 'NONE', #188147, #194295, #68256, .T. ) ;
#129791 = CARTESIAN_POINT ( 'NONE',  ( 9.073431116043567002, 11.60875560684942265, -1.599625672291262513 ) ) ;
#129793 = VECTOR ( 'NONE', #84153, 1000.000000000000000 ) ;
#129792 = CARTESIAN_POINT ( 'NONE',  ( 6.756857042228312515, -1.710155547305733492, 1.394389531264042414 ) ) ;
#129794 = CARTESIAN_POINT ( 'NONE',  ( 0.6823417656249934904, 8.942708333674733723, 1.181850606188764807 ) ) ;
#129795 = CARTESIAN_POINT ( 'NONE',  ( -4.122561227007127016, 6.967349310553715647, 1.199719254218452935 ) ) ;
#129796 = CARTESIAN_POINT ( 'NONE',  ( 5.519157712072518152, -1.821736412749059397, 0.8647389720048551665 ) ) ;
#129798 = ORIENTED_EDGE ( 'NONE', *, *, #97607, .T. ) ;
#129797 = CARTESIAN_POINT ( 'NONE',  ( 4.886864132303106345, -1.708302746381512804, -0.6034029335190493892 ) ) ;
#129799 = CARTESIAN_POINT ( 'NONE',  ( 3.520239479114235959, 1.187513476551487424, -1.445374034619355985 ) ) ;
#129800 = CARTESIAN_POINT ( 'NONE',  ( 3.467693386974544545, -0.4085244671708112008, 2.029378838279243258 ) ) ;
#129801 = FACE_OUTER_BOUND ( 'NONE', #103764, .T. ) ;
#129803 = PRESENTATION_LAYER_ASSIGNMENT (  '', '', ( #178280 ) ) ;
#129802 = CARTESIAN_POINT ( 'NONE',  ( -0.4153311931459069406, 3.780155993257306335, -0.4999999999999988343 ) ) ;
#129804 = CARTESIAN_POINT ( 'NONE',  ( -1.580000000000022276, 8.674529973577531194, 2.500000000000011102 ) ) ;
#129805 = CARTESIAN_POINT ( 'NONE',  ( -5.375696267714453747, 6.397419496268610395, 1.092131393413272811 ) ) ;
#129806 = CARTESIAN_POINT ( 'NONE',  ( 0.6823417656249899377, 3.738541667008085767, -1.181850606188754593 ) ) ;
#129807 = CARTESIAN_POINT ( 'NONE',  ( 1.248149539447914513, 0.9399939672071170316, -1.665319807275446928 ) ) ;
#129808 = CARTESIAN_POINT ( 'NONE',  ( 3.191801227909254912, -1.315628469008291557, -1.455533501494077342 ) ) ;
#129809 = CARTESIAN_POINT ( 'NONE',  ( 0.7728142736522191081, -2.006652962095498260, 0.1948079406639269262 ) ) ;
#129810 = CARTESIAN_POINT ( 'NONE',  ( -4.285259070371116863, 7.157163461145040095, 1.199719254218452935 ) ) ;
#129811 = CARTESIAN_POINT ( 'NONE',  ( 9.121938423896107651, 9.536683004167278099, -0.7998128361456221525 ) ) ;
#129812 = CARTESIAN_POINT ( 'NONE',  ( 6.257099195183372764, -1.689481296825417811, -1.015638971094455556 ) ) ;
#129813 = CARTESIAN_POINT ( 'NONE',  ( -1.201851678989727383E-14, 3.821875000341423689, 1.575800808251672791 ) ) ;
#129814 = CARTESIAN_POINT ( 'NONE',  ( 2.092043371607322566, 1.241737408274107501, 1.584530653180368009 ) ) ;
#129816 = CARTESIAN_POINT ( 'NONE',  ( 2.706785462534053277, 1.994624666228937526, 0.7104243659002054123 ) ) ;
#129815 = CARTESIAN_POINT ( 'NONE',  ( -6.507550544879489252, 9.575597488125954015, 1.082531754730548412 ) ) ;
#129817 = CARTESIAN_POINT ( 'NONE',  ( 10.88976023856472075, 8.285890218793616313, -4.933575180849306463 ) ) ;
#129818 = CARTESIAN_POINT ( 'NONE',  ( 3.350112325975619587, -0.8415805752714689003, 1.891790567983504312 ) ) ;
#129819 = CARTESIAN_POINT ( 'NONE',  ( 5.032011289327418702, 5.899709921417326974, 1.199719254218452935 ) ) ;
#129821 = CARTESIAN_POINT ( 'NONE',  ( 3.192055101013606233, 5.811482486902795230, -1.199719254218446718 ) ) ;
#129820 = CARTESIAN_POINT ( 'NONE',  ( 5.876921326125680523, 1.932075295558054240, -0.7991432938223922422 ) ) ;
#129823 = EDGE_LOOP ( 'NONE', ( #86064, #201187, #179949, #173446 ) ) ;
#129822 = CARTESIAN_POINT ( 'NONE',  ( 4.752862199841776381, -1.465721779273346792, 1.088108411805274622 ) ) ;
#129824 = CARTESIAN_POINT ( 'NONE',  ( 8.380911511541880188, 12.92948053010758258, 0.7998128361456462443 ) ) ;
#129825 = CARTESIAN_POINT ( 'NONE',  ( 7.727353211424198065, -6.453073674884657329, -7.679448064523601403 ) ) ;
#129826 = CARTESIAN_POINT ( 'NONE',  ( 10.14644687988836047, 13.59653676117442878, -7.280050914245562055 ) ) ;
#129827 = CARTESIAN_POINT ( 'NONE',  ( -10.37901820579008039, 4.889546506944066451, 5.358714317323078014 ) ) ;
#129828 = CARTESIAN_POINT ( 'NONE',  ( -1.402160292154681736E-14, 10.48437500034139624, 1.575800808251682339 ) ) ;
#129829 = CARTESIAN_POINT ( 'NONE',  ( 5.197880135092803222, 1.287283252470315720, 1.414272151883423589 ) ) ;
#129830 = CARTESIAN_POINT ( 'NONE',  ( -9.622536337397040285, 12.24937836509514710, 1.599625672291281386 ) ) ;
#129831 = CARTESIAN_POINT ( 'NONE',  ( 7.283754839039659146, 9.520799950344851936, -1.599625672291262513 ) ) ;
#129832 = CARTESIAN_POINT ( 'NONE',  ( 1.360316468749997565, 2.067708333674723953, -0.7853790794159001276 ) ) ;
#129833 = CARTESIAN_POINT ( 'NONE',  ( 3.348500752450937590, 5.890039396959305229, 1.082531754730558626 ) ) ;
#129834 = SURFACE_STYLE_FILL_AREA ( #192597 ) ;
#129835 = CARTESIAN_POINT ( 'NONE',  ( 0.3449248370967008537, 0.5783895242766275979, -1.748133987124582012 ) ) ;
#129836 = ORIENTED_EDGE ( 'NONE', *, *, #12907, .F. ) ;
#129837 = EDGE_CURVE ( 'NONE', #5098, #124142, #117806, .T. ) ;
#129838 = CARTESIAN_POINT ( 'NONE',  ( -6.454563648557663846, 9.688018802362710957, -1.199719254218452047 ) ) ;
#129839 = CARTESIAN_POINT ( 'NONE',  ( 4.481629103029507455, 1.220264704679861811, 1.417821649906551906 ) ) ;
#129840 = CARTESIAN_POINT ( 'NONE',  ( -0.02319159430947542733, 0.7471999394491578572, -1.895068635927643630 ) ) ;
#129841 = CARTESIAN_POINT ( 'NONE',  ( 6.180537922983273091, 8.303989891604203422, -1.599625672291281386 ) ) ;
#129842 = FACE_OUTER_BOUND ( 'NONE', #23855, .T. ) ;
#129843 = CARTESIAN_POINT ( 'NONE',  ( -5.568215224448921141, 7.423109701660543180, 1.245465753432648093 ) ) ;
#129844 = CARTESIAN_POINT ( 'NONE',  ( -6.738039156311804945, 6.963393225226301553, 1.040834085586084257E-14 ) ) ;
#129845 = CARTESIAN_POINT ( 'NONE',  ( 3.684065054611349144, 5.321161868511784299, -1.599625672291262513 ) ) ;
#129846 = CARTESIAN_POINT ( 'NONE',  ( 1.270285106180467416, -0.8805531663822261379, -1.761673308874162069 ) ) ;
#129847 = CARTESIAN_POINT ( 'NONE',  ( 2.442982655898734645, -1.755780842375562312, -0.9913809985205720432 ) ) ;
#129848 = CARTESIAN_POINT ( 'NONE',  ( -9.494787648271923786, 9.971673765939062406, 1.040834085586084257E-14 ) ) ;
#129849 = CARTESIAN_POINT ( 'NONE',  ( 4.030516805012513082, 7.924296382481737844, 0.000000000000000000 ) ) ;
#129850 = CARTESIAN_POINT ( 'NONE',  ( 0.000000000000000000, 0.000000000000000000, 0.000000000000000000 ) ) ;
#129851 = CARTESIAN_POINT ( 'NONE',  ( 1.992365796559266267, -0.5863786240636535974, -2.111471653062434672 ) ) ;
#129852 = CARTESIAN_POINT ( 'NONE',  ( 0.05513001983271961781, -8.135652870098732947, 11.00000000000013145 ) ) ;
#129853 = CARTESIAN_POINT ( 'NONE',  ( -8.350932551013499960, 11.83017284523606172, -1.199719254218446718 ) ) ;
#129854 = DIRECTION ( 'NONE',  ( 0.000000000000000000, 1.000000000000000000, 0.000000000000000000 ) ) ;
#129855 = CARTESIAN_POINT ( 'NONE',  ( 3.553645660557675612, 6.199651466408984568, -1.082531754730549967 ) ) ;
#129856 = CARTESIAN_POINT ( 'NONE',  ( 9.257519960032755790, 9.694861462993381807, 0.7998128361456462443 ) ) ;
#129857 = ADVANCED_FACE ( 'NONE', ( #202520 ), #88668, .T. ) ;
#129858 = CARTESIAN_POINT ( 'NONE',  ( 6.647575389402066826, 6.649926130590872120, 1.040834085586084257E-14 ) ) ;
#129859 = CARTESIAN_POINT ( 'NONE',  ( -3.332168893502572171, 7.719402352560116753, -2.450693629706319321 ) ) ;
#129860 = CARTESIAN_POINT ( 'NONE',  ( 7.200788982633824276, 7.573544365927161515, 0.000000000000000000 ) ) ;
#129861 = ORIENTED_EDGE ( 'NONE', *, *, #77449, .F. ) ;
#129863 = CARTESIAN_POINT ( 'NONE',  ( 1.488932678171340118, -1.912290114023627252, -0.6292827167945020950 ) ) ;
#129862 = CARTESIAN_POINT ( 'NONE',  ( 4.739718475747470627, 1.836682745182907972, 0.1304020654292817605 ) ) ;
#129864 = CARTESIAN_POINT ( 'NONE',  ( 3.058317229773829471, 1.972480788633700577, -1.179572646267361025 ) ) ;
#129866 = CARTESIAN_POINT ( 'NONE',  ( 2.184208379282841950, 1.076359544750982389, -1.517863362848305808 ) ) ;
#129865 = CARTESIAN_POINT ( 'NONE',  ( 3.128199800776516160, 2.800000000000115730, -2.480560084996043191 ) ) ;
#129867 = CARTESIAN_POINT ( 'NONE',  ( -3.285556943750000514, -2.238541666188709200, -1.896917185911906500 ) ) ;
#129868 =( LENGTH_UNIT ( ) NAMED_UNIT ( * ) SI_UNIT ( .MILLI., .METRE. ) );
#129869 = CARTESIAN_POINT ( 'NONE',  ( 5.484596585704371918, -1.208295678440996390, 1.482354609825987435 ) ) ;
#129870 = CARTESIAN_POINT ( 'NONE',  ( -9.657485491635913633, 10.16148791653038330, 1.040834085586084257E-14 ) ) ;
#129871 = CIRCLE ( 'NONE', #8721, 0.08000000000000020983 ) ;
#129872 = CARTESIAN_POINT ( 'NONE',  ( -4.651856103264620401, 8.441266197201775512, 0.000000000000000000 ) ) ;
#129874 = CARTESIAN_POINT ( 'NONE',  ( 3.449935675575486638, 1.870836310073907827, 0.001118452434160921221 ) ) ;
#129873 = CARTESIAN_POINT ( 'NONE',  ( 5.319903205935248458, 1.244510898466891780, -1.679860476595731233 ) ) ;
#129875 = CARTESIAN_POINT ( 'NONE',  ( 8.459924665247367415, 8.972259652317825740, -0.7216878364870267237 ) ) ;
#129876 = CARTESIAN_POINT ( 'NONE',  ( 6.233933901472759942, 1.822226914158030286, 0.2631550708301691466 ) ) ;
#129877 = CARTESIAN_POINT ( 'NONE',  ( 2.496672843210871129, 6.064535417054653266, -0.7998128361456291469 ) ) ;
#129878 = PLANE ( 'NONE',  #117171 ) ;
#129879 = CARTESIAN_POINT ( 'NONE',  ( 5.021954727502539129, -0.9268850835505036967, -1.454474922752227339 ) ) ;
#129880 = CARTESIAN_POINT ( 'NONE',  ( -5.768104287610143821, 8.816873204598778102, -1.199719254218440723 ) ) ;
#129881 = CARTESIAN_POINT ( 'NONE',  ( 0.4922575064417636925, -1.726078246012904938, 0.1672019070194027679 ) ) ;
#129882 = DIRECTION ( 'NONE',  ( 5.578564026256490882E-16, 1.000000000000000000, 9.066213480720158442E-32 ) ) ;
#129883 = CARTESIAN_POINT ( 'NONE',  ( 4.000000000000012434, 5.499999999999998224, 0.7500000000000006661 ) ) ;
#129884 = CARTESIAN_POINT ( 'NONE',  ( 5.102462520977921301, 2.164757797245045357, 0.1666947352320021780 ) ) ;
#129885 = CARTESIAN_POINT ( 'NONE',  ( 3.492628380820805400, -0.3572889717703279788, -1.790209119249221548 ) ) ;
#129886 = CARTESIAN_POINT ( 'NONE',  ( 1.305434336737832490, -1.543085766649286317, -1.211208057394968618 ) ) ;
#129887 = CARTESIAN_POINT ( 'NONE',  ( 0.1756132116073009508, 1.572246328413629435, 1.418195661691145304 ) ) ;
#129889 = CARTESIAN_POINT ( 'NONE',  ( -1.364683531250010295, 4.592708333674755394, 0.7879004041258379498 ) ) ;
#129888 = CARTESIAN_POINT ( 'NONE',  ( 0.6918693526153978368, -0.8198495674218098106, 2.140808456117601732 ) ) ;
#129890 = CARTESIAN_POINT ( 'NONE',  ( 2.030969412801347573, 8.463209591663295228, 2.499999999999998668 ) ) ;
#129891 = CARTESIAN_POINT ( 'NONE',  ( 9.240045382913317340, 10.73880668727576015, -1.199719254218446718 ) ) ;
#129892 = CARTESIAN_POINT ( 'NONE',  ( 2.280079029133400326, 2.079044457705871096, -0.4163345062310334632 ) ) ;
#129893 = CARTESIAN_POINT ( 'NONE',  ( -3.294268138440636928, 6.787137228248626641, 1.040834085586084257E-14 ) ) ;
#129894 =( GEOMETRIC_REPRESENTATION_CONTEXT ( 3 ) GLOBAL_UNCERTAINTY_ASSIGNED_CONTEXT ( ( #159448 ) ) GLOBAL_UNIT_ASSIGNED_CONTEXT ( ( #213381, #114541, #160398 ) ) REPRESENTATION_CONTEXT ( 'NONE', 'WORKASPACE' ) );
#129895 = CARTESIAN_POINT ( 'NONE',  ( -5.883875478206491927, 5.966868934103426447, 0.000000000000000000 ) ) ;
#129896 = CARTESIAN_POINT ( 'NONE',  ( 6.977413708759169886, -0.1587332643391472231, 2.136494379638858909 ) ) ;
#129898 = CARTESIAN_POINT ( 'NONE',  ( -1.500000000000015099, 13.51041666734946034, -0.8660254037844309360 ) ) ;
#129897 = CARTESIAN_POINT ( 'NONE',  ( 6.983263157960349687, 0.5706719223780298833, 2.105707282093812083 ) ) ;
#129901 = ORIENTED_EDGE ( 'NONE', *, *, #9913, .F. ) ;
#129900 = CARTESIAN_POINT ( 'NONE',  ( 1.998975601324129769, -2.179183720934555701, -0.4297205562568666148 ) ) ;
#129899 = AXIS2_PLACEMENT_3D ( 'NONE', #111454, #64757, #77811 ) ;
#129902 = CARTESIAN_POINT ( 'NONE',  ( 0.4230186368967851496, -1.631317381931682631, -1.619748931356496113 ) ) ;
#129904 = CARTESIAN_POINT ( 'NONE',  ( 5.787952559958898568, -1.304071791706362449, -1.598039198280821749 ) ) ;
#129903 = CARTESIAN_POINT ( 'NONE',  ( 4.844340958784499662, 4.546152628203684820, 0.7998128361456341429 ) ) ;
#129906 = CARTESIAN_POINT ( 'NONE',  ( -3.474999999999998312, -2.070833333333331971, 2.006292185433951047 ) ) ;
#129905 = CARTESIAN_POINT ( 'NONE',  ( 4.179656494762836516, 8.098292687190454586, -0.7998128361456362523 ) ) ;
#129907 = CARTESIAN_POINT ( 'NONE',  ( 5.468734858265785093, 7.473552982767158070, 1.599625672291269396 ) ) ;
#129908 = CARTESIAN_POINT ( 'NONE',  ( -1.642778471875000035, -3.755208332855374476, -2.845375778867859751 ) ) ;
#129909 = DIRECTION ( 'NONE',  ( -0.000000000000000000, -1.000000000000000000, -0.000000000000000000 ) ) ;
#129910 = CARTESIAN_POINT ( 'NONE',  ( 5.372543328820884589, -0.05112055865702340440, -1.840719716649619198 ) ) ;
#129911 = EDGE_CURVE ( 'NONE', #200201, #72143, #80524, .T. ) ;
#129913 = ORIENTED_EDGE ( 'NONE', *, *, #18291, .T. ) ;
#129912 = CARTESIAN_POINT ( 'NONE',  ( 5.705283713252285338, 5.550585841749444249, -0.7998128361456211532 ) ) ;
#129914 = CARTESIAN_POINT ( 'NONE',  ( 2.238867094643140376, -1.542287835237671212, 0.7722583484809567578 ) ) ;
#129915 = CARTESIAN_POINT ( 'NONE',  ( 1.499232818411553536, -0.2420282084563407654, 2.001858358113464575 ) ) ;
#129916 = CARTESIAN_POINT ( 'NONE',  ( 2.180727191476996563, 1.779927251244978192, 1.454631630963822309 ) ) ;
#129917 = CARTESIAN_POINT ( 'NONE',  ( -1.201851678989727383E-14, 4.509375000341417916, -1.575800808251660134 ) ) ;
#129918 = CARTESIAN_POINT ( 'NONE',  ( 1.950798113461976735, 0.7085273209575352338, 2.148688966898488761 ) ) ;
#129919 = CARTESIAN_POINT ( 'NONE',  ( 4.266313661023513504, 0.9922932564179194337, 1.857654695958657953 ) ) ;
#129920 = CARTESIAN_POINT ( 'NONE',  ( -6.943184063974175757, 9.193743722760251202, -1.443375672974066548 ) ) ;
#129921 = CARTESIAN_POINT ( 'NONE',  ( 2.266550661271060640, -1.615954428537921483, -0.7220204016161780869 ) ) ;
#129922 = CARTESIAN_POINT ( 'NONE',  ( 6.205881626753210867, 8.263281202677319470, 1.599625672291281386 ) ) ;
#129923 = CARTESIAN_POINT ( 'NONE',  ( 5.682275777458854371, 5.801945626556378244, 0.7216878364870328300 ) ) ;
#129924 = CARTESIAN_POINT ( 'NONE',  ( -5.922214171070950606, 5.803671375871217286, -0.7998128361456291469 ) ) ;
#129925 = CARTESIAN_POINT ( 'NONE',  ( 1.499999999999989120, 2.525000000000020339, 1.214306433183764966E-14 ) ) ;
#129926 = CARTESIAN_POINT ( 'NONE',  ( 6.064703480017706205, 0.6958612881963457397, 2.109637055116654558 ) ) ;
#129927 = CARTESIAN_POINT ( 'NONE',  ( 3.275498427308475069, 1.390425696708731396, 1.693851754907250928 ) ) ;
#129928 = CARTESIAN_POINT ( 'NONE',  ( -3.086452525405351643, 6.752611712948207057, 0.7998128361456341429 ) ) ;
#129929 = CARTESIAN_POINT ( 'NONE',  ( 0.4829820140310078780, 7.516281308464741961, -1.942130999994612139 ) ) ;
#129930 = CARTESIAN_POINT ( 'NONE',  ( 6.569000932001921811, -1.639521903533578850, 1.344440124909966450 ) ) ;
#129931 = CARTESIAN_POINT ( 'NONE',  ( 1.364683531249988535, 2.905208333674754506, -0.7879004041258239610 ) ) ;
#129932 = CARTESIAN_POINT ( 'NONE',  ( 0.6823417656249969321, 8.526041667008064096, -1.181850606188757036 ) ) ;
#129934 = CARTESIAN_POINT ( 'NONE',  ( -4.961921032921567054, 4.891255414604337659, 0.7216878364870317197 ) ) ;
#129933 = AXIS2_PLACEMENT_3D ( 'NONE', #133500, #5551, #121563 ) ;
#129935 = CARTESIAN_POINT ( 'NONE',  ( 5.730757696090861941, 1.422813033107739988, -1.572628729999878905 ) ) ;
#129936 = CARTESIAN_POINT ( 'NONE',  ( -4.977251789992602760, 8.820894498384422633, 0.000000000000000000 ) ) ;
#129937 = ORIENTED_EDGE ( 'NONE', *, *, #100401, .F. ) ;
#129938 = CARTESIAN_POINT ( 'NONE',  ( -5.994113311017573054, 6.165756082374834079, 0.7216878364870257245 ) ) ;
#129939 = CARTESIAN_POINT ( 'NONE',  ( 4.496500501226593727, 8.397667684739696270, 0.7998128361456462443 ) ) ;
#129940 = CARTESIAN_POINT ( 'NONE',  ( 6.251489360189885325, 1.835807759842246423, -0.1425652098738516838 ) ) ;
#129941 = DIRECTION ( 'NONE',  ( 0.000000000000000000, 0.000000000000000000, -1.000000000000000000 ) ) ;
#129942 = DIRECTION ( 'NONE',  ( 0.000000000000000000, 0.000000000000000000, 1.000000000000000000 ) ) ;
#129943 = CARTESIAN_POINT ( 'NONE',  ( -1.201851678989727383E-14, 3.634375000341422357, 1.575800808251672791 ) ) ;
#129944 = CARTESIAN_POINT ( 'NONE',  ( 2.296107463031165086, 1.396982486531380463, -1.037807123096459838 ) ) ;
#129945 = CARTESIAN_POINT ( 'NONE',  ( -5.443788192324133135, 7.193024429787462815, -1.249999997929073237 ) ) ;
#129946 = CARTESIAN_POINT ( 'NONE',  ( 1.500000000000001332, 10.90625000068279249, 0.000000000000000000 ) ) ;
#129947 = CARTESIAN_POINT ( 'NONE',  ( 1.364683531249986537, -0.03229166632525094088, -0.7879004041258309554 ) ) ;
#129948 = CARTESIAN_POINT ( 'NONE',  ( -11.94105721237523277, 19.00000000000000000, 1.187919463087248273 ) ) ;
#129949 = CARTESIAN_POINT ( 'NONE',  ( 6.227428301493934448, -2.037140905555033576, 0.7235935974677574212 ) ) ;
#129950 = CARTESIAN_POINT ( 'NONE',  ( -9.996439331977562404, 10.55693406359564790, 0.7998128361456462443 ) ) ;
#129951 = CARTESIAN_POINT ( 'NONE',  ( -7.036318535368094373, 7.311385834125318617, 0.7216878364870317197 ) ) ;
#129952 = AXIS2_PLACEMENT_3D ( 'NONE', #83122, #18112, #84198 ) ;
#129953 = CARTESIAN_POINT ( 'NONE',  ( 5.963787895669664607, 2.130530397400759668, -0.3648857593604309391 ) ) ;
#129955 = EDGE_LOOP ( 'NONE', ( #213576, #66965, #96274, #82546 ) ) ;
#129954 = DIRECTION ( 'NONE',  ( -3.330669073875478989E-16, 3.330669073875478989E-16, 1.000000000000000000 ) ) ;
#129956 = CARTESIAN_POINT ( 'NONE',  ( 1.364683531249988535, 4.905208333674756283, -0.7879004041258300672 ) ) ;
#129957 = CARTESIAN_POINT ( 'NONE',  ( 5.729747329291909885, -1.248464225167019714, -1.525673545143470200 ) ) ;
#129958 = CARTESIAN_POINT ( 'NONE',  ( 5.395702507230883072, 0.1292110896585068891, 1.729053200853872596 ) ) ;
#129960 = CARTESIAN_POINT ( 'NONE',  ( 2.103317784989285677, -0.4765762082987561321, 2.138964651187735821 ) ) ;
#129959 = CARTESIAN_POINT ( 'NONE',  ( 0.6801582343749744686, -0.2760416663252704406, 1.178068619123780802 ) ) ;
#129961 = CARTESIAN_POINT ( 'NONE',  ( 3.487651025411703021, 2.087124329425969371, -0.9845696281253720761 ) ) ;
#129962 = CARTESIAN_POINT ( 'NONE',  ( 6.345006307232072373, -1.743395995315766056, 1.098490678494741912 ) ) ;
#129963 = CARTESIAN_POINT ( 'NONE',  ( 1.745936028080337765, 0.6089015219087092756, 1.844080840262368071 ) ) ;
#129965 = EDGE_CURVE ( 'NONE', #49964, #23806, #66114, .T. ) ;
#129964 = CARTESIAN_POINT ( 'NONE',  ( -5.382223794500827552, 9.223085493652217082, -0.7216878364870207285 ) ) ;
#129966 = CIRCLE ( 'NONE', #98821, 2.650000000000008349 ) ;
#129967 = CARTESIAN_POINT ( 'NONE',  ( -4.950662367645459305, 5.804802846121667415, -1.199719254218453823 ) ) ;
#129968 = CARTESIAN_POINT ( 'NONE',  ( 2.000000000000011990, 2.453105802350476962E-14, 1.500000000000001332 ) ) ;
#129969 = CARTESIAN_POINT ( 'NONE',  ( 3.480829117359967917, -1.421471314662653196, 1.573842340227212366 ) ) ;
#129970 = CARTESIAN_POINT ( 'NONE',  ( -15.75000000000000000, 10.19999999999998153, 1.799999999999999600 ) ) ;
#129971 = CARTESIAN_POINT ( 'NONE',  ( 1.951796282902381163, -1.844710420878793444, -0.8146254186931353169 ) ) ;
#129972 = CARTESIAN_POINT ( 'NONE',  ( -6.412643469139482910, 7.544134137826577380, 1.082531754730549967 ) ) ;
#129973 = CARTESIAN_POINT ( 'NONE',  ( 4.506973327934083784, 1.708129512224244806, -1.397202154207459524 ) ) ;
#129974 = CARTESIAN_POINT ( 'NONE',  ( 3.285556943750000070, -0.3718749995220427262, 0.000000000000000000 ) ) ;
#129975 = CARTESIAN_POINT ( 'NONE',  ( 0.3782569160206594727, 3.049340702855413365, -0.4285286083246188649 ) ) ;
#129976 = CARTESIAN_POINT ( 'NONE',  ( -0.01727558406095473439, -0.1313277740116538805, -1.795991579427682616 ) ) ;
#129977 = CARTESIAN_POINT ( 'NONE',  ( -5.427006627220116286, 9.553534508390610469, -0.7998128361456362523 ) ) ;
#129979 = DIRECTION ( 'NONE',  ( 0.000000000000000000, 0.000000000000000000, 1.000000000000000000 ) ) ;
#129978 = CARTESIAN_POINT ( 'NONE',  ( -4.973494386576447823, 8.059877448926631160, 1.114414082037382236 ) ) ;
#129980 = CARTESIAN_POINT ( 'NONE',  ( 11.01135777277261951, 12.59499145469730763, -1.400000000000001243 ) ) ;
#129981 = VERTEX_POINT ( 'NONE', #18453 ) ;
#129982 = CARTESIAN_POINT ( 'NONE',  ( 4.346593572148568896, 0.5479209435249388083, 1.986652789453833057 ) ) ;
#129983 = CARTESIAN_POINT ( 'NONE',  ( -5.346851039111044201, 6.199209027673978412, 7.500000000000000000 ) ) ;
#129984 = EDGE_CURVE ( 'NONE', #48908, #130487, #204177, .T. ) ;
#129985 = CARTESIAN_POINT ( 'NONE',  ( 0.4644097342742976586, -8.200000000000015277, 9.488641820551100281 ) ) ;
#129986 = CARTESIAN_POINT ( 'NONE',  ( -4.771579997005698459, 7.654261532226910525, -1.199719254218452047 ) ) ;
#129987 = CARTESIAN_POINT ( 'NONE',  ( -4.817943484809863008, 6.714296380401858499, 1.599625672291263179 ) ) ;
#129988 = CARTESIAN_POINT ( 'NONE',  ( 3.545573561795499540, -1.865266050240913520, 0.7750044584247675061 ) ) ;
#129989 = CARTESIAN_POINT ( 'NONE',  ( 1.499999999999987121, 1.254166666666689300, 0.8660254037844524744 ) ) ;
#129990 = CARTESIAN_POINT ( 'NONE',  ( 9.327646496521982300, 11.90534021740758064, -1.443375672974057666 ) ) ;
#129991 = CARTESIAN_POINT ( 'NONE',  ( 7.579171565239241737, 8.801120566655981747, 1.199719254218462483 ) ) ;
#129992 = CARTESIAN_POINT ( 'NONE',  ( 3.168876024238317601, -1.903602637213364979, -0.7901525784780991657 ) ) ;
#129993 = CARTESIAN_POINT ( 'NONE',  ( 1.419999999999989049, 6.216000000000041048, -2.921333333333328675 ) ) ;
#129994 = CARTESIAN_POINT ( 'NONE',  ( 4.493637847925535667, 7.329995691633395261, -1.199719254218452047 ) ) ;
#129995 = CARTESIAN_POINT ( 'NONE',  ( -4.257741265285667431, 3.982435197156672491, 0.4597581080974452727 ) ) ;
#129996 = CARTESIAN_POINT ( 'NONE',  ( 1.763359053103892293, 0.9455654613358072114, 1.579637215005654349 ) ) ;
#129997 = CARTESIAN_POINT ( 'NONE',  ( 6.639307388351803674, -1.973492857608965423, 0.9879489342229507143 ) ) ;
#129998 = CARTESIAN_POINT ( 'NONE',  ( 4.376249722160992839, 8.327651452488305850, 0.000000000000000000 ) ) ;
#129999 = CARTESIAN_POINT ( 'NONE',  ( 2.987745815084281276, 1.526290923294726820, 1.530918043534036599 ) ) ;
#130000 = CARTESIAN_POINT ( 'NONE',  ( -3.578989364327652467, 6.158942777482099729, 1.082531754730560403 ) ) ;
#130001 = CARTESIAN_POINT ( 'NONE',  ( 1.622280145275534435, 1.995268681201247452, 0.2910785328335343536 ) ) ;
#130002 = DIRECTION ( 'NONE',  ( -0.000000000000000000, 1.000000000000000000, -0.000000000000000000 ) ) ;
#130003 = CARTESIAN_POINT ( 'NONE',  ( 0.8131078318618142342, -0.2785150557334699073, 1.849687307983488571 ) ) ;
#130004 = EDGE_CURVE ( 'NONE', #137303, #120691, #194765, .T. ) ;
#130005 = CARTESIAN_POINT ( 'NONE',  ( 4.170748999387418721, -1.839122178589139178, -0.7105754535856413368 ) ) ;
#130006 = CARTESIAN_POINT ( 'NONE',  ( 4.540250091716044878, 0.7762272601403925609, 1.861345588084816871 ) ) ;
#130008 = CARTESIAN_POINT ( 'NONE',  ( 10.34450801710256584, 11.17094022948226240, 0.7216878364870438212 ) ) ;
#130007 = CARTESIAN_POINT ( 'NONE',  ( -1.364683531249997417, 3.009375000341422801, 1.214306433183764966E-14 ) ) ;
#130010 = CARTESIAN_POINT ( 'NONE',  ( 6.024072228909682636, -1.168613738950954550, -1.751890494488865357 ) ) ;
#130009 = CARTESIAN_POINT ( 'NONE',  ( -5.228640796364566690, 9.251831362400652736, -0.7998128361456231517 ) ) ;
#130011 = CARTESIAN_POINT ( 'NONE',  ( 6.531696417657103737, 1.982406992490031383, -0.5971068152322634992 ) ) ;
#130012 = CARTESIAN_POINT ( 'NONE',  ( 5.307127064745490230, 8.279066444590018392, -1.199719254218452935 ) ) ;
#130013 = CARTESIAN_POINT ( 'NONE',  ( -6.470265622219711688, 8.571729197388226140, -1.599625672291263179 ) ) ;
#130014 = CARTESIAN_POINT ( 'NONE',  ( -1.524175555628288992, 8.756493634679708649, 2.487619788734857007 ) ) ;
#130015 = CARTESIAN_POINT ( 'NONE',  ( 4.996930482532231821, 1.639556309048403770, -1.094490209086243171 ) ) ;
#130016 = CARTESIAN_POINT ( 'NONE',  ( 6.363536886121980984, -1.624614756573187435, -1.199887179878684540 ) ) ;
#130017 = CARTESIAN_POINT ( 'NONE',  ( -1.201851678989727383E-14, 0.7437500006828187127, 1.732050807568877637 ) ) ;
#130018 = CARTESIAN_POINT ( 'NONE',  ( 4.582853619701852566, -2.237698958467302823, -0.5636369891960175682 ) ) ;
#130019 = CARTESIAN_POINT ( 'NONE',  ( 2.237243932873288710, -0.09700783546583501005, -2.060382906607181930 ) ) ;
#130020 = CARTESIAN_POINT ( 'NONE',  ( 6.480434237652115570, 10.50433101066207442, 0.7216878364870438212 ) ) ;
#130021 = CARTESIAN_POINT ( 'NONE',  ( 6.039231080244466199, 6.010467446565510130, 0.7998128361456352531 ) ) ;
#130022 = CARTESIAN_POINT ( 'NONE',  ( 4.167152111353856547, 5.955039778036558040, 1.599625672291262513 ) ) ;
#130023 = CARTESIAN_POINT ( 'NONE',  ( -1.201851678989727383E-14, 1.884375000341422135, 1.575800808251672791 ) ) ;
#130024 = CARTESIAN_POINT ( 'NONE',  ( 3.984117037569365305, 5.741498858621315371, 1.599625672291261402 ) ) ;
#130025 = CARTESIAN_POINT ( 'NONE',  ( 6.765155463094759014, 7.955398130774449683, 1.082531754730558626 ) ) ;
#130026 = CARTESIAN_POINT ( 'NONE',  ( 4.721225823269111110, -1.937324205527543253, -0.9803755122778281539 ) ) ;
#130027 = CARTESIAN_POINT ( 'NONE',  ( -5.356880090730904875, 7.343055753976412525, 1.443375672974058777 ) ) ;
#130029 = CARTESIAN_POINT ( 'NONE',  ( 2.647807870277216757, 0.6224553824519338807, 1.732961026760751366 ) ) ;
#130028 = CARTESIAN_POINT ( 'NONE',  ( -2.629918611371007575, 6.012062780000711371, 0.7216878364870317197 ) ) ;
#130030 = CARTESIAN_POINT ( 'NONE',  ( -1.364683531250010295, 5.280208333674758059, 0.7879004041258379498 ) ) ;
#130031 = CARTESIAN_POINT ( 'NONE',  ( 5.319949580897746166, 1.306013235697962571, -1.759773446019400778 ) ) ;
#130032 = CARTESIAN_POINT ( 'NONE',  ( -15.75000000000000000, 9.799999999999998934, 0.6999999999999992895 ) ) ;
#130033 = CARTESIAN_POINT ( 'NONE',  ( 6.034080775264698993, 1.121385855563570288, -1.965008656891243044 ) ) ;
#130034 = CARTESIAN_POINT ( 'NONE',  ( -4.646091124696241081, 7.101299429195864654, -1.386232413501260474 ) ) ;
#130035 = CARTESIAN_POINT ( 'NONE',  ( 4.783863686166085039, 8.265937597628173705, 0.8363946479656783062 ) ) ;
#130036 = CARTESIAN_POINT ( 'NONE',  ( -6.102578539482539810, 6.292298848917299736, 0.000000000000000000 ) ) ;
#130037 = FACE_OUTER_BOUND ( 'NONE', #111772, .T. ) ;
#130038 = CARTESIAN_POINT ( 'NONE',  ( 6.221911924188020748, -0.9849534058487903199, -1.470084644806458174 ) ) ;
#130039 = CARTESIAN_POINT ( 'NONE',  ( 1.364683531249996529, 11.96354166700806765, 0.7879004041258403923 ) ) ;
#130040 = CARTESIAN_POINT ( 'NONE',  ( 4.072905994182826284, -1.490248019560231452, 1.353564014653575009 ) ) ;
#130041 = CARTESIAN_POINT ( 'NONE',  ( 5.957918438201454059, 9.038323046955323292, -1.199719254218440723 ) ) ;
#130042 = CARTESIAN_POINT ( 'NONE',  ( 3.188603428895543601, -2.074531711476882201, -0.3615289903074799249 ) ) ;
#130043 = CARTESIAN_POINT ( 'NONE',  ( 2.478032317504985649, -1.910654254087537307, -0.1382841363062360662 ) ) ;
#130044 = CARTESIAN_POINT ( 'NONE',  ( 5.183294799126148433, 4.941598775268944976, 1.040834085586084257E-14 ) ) ;
#130045 = CARTESIAN_POINT ( 'NONE',  ( 3.543367420142525148, 1.781686863328624026, -0.8397465311346365979 ) ) ;
#130046 = CARTESIAN_POINT ( 'NONE',  ( 1.164687902950040321, -1.689591380799923215, -0.8031939614948147010 ) ) ;
#130047 = CARTESIAN_POINT ( 'NONE',  ( 1.644895634054041933, -0.2845770130874228365, -1.940982728367894206 ) ) ;
#130050 = VERTEX_POINT ( 'NONE', #67186 ) ;
#130049 = CARTESIAN_POINT ( 'NONE',  ( -0.2108831679770960255, -0.001785917861228669690, -1.896958272444612792 ) ) ;
#130048 = CARTESIAN_POINT ( 'NONE',  ( 4.019902842142981214, -0.8889698729942583366, -1.477996400630256613 ) ) ;
#130052 = CARTESIAN_POINT ( 'NONE',  ( 5.585596099150174965, 7.539614753807099667, -1.443375672974057666 ) ) ;
#130051 = CARTESIAN_POINT ( 'NONE',  ( 1.682535984017709874, -1.178549783888741320, 1.865657194899547733 ) ) ;
#130053 = CARTESIAN_POINT ( 'NONE',  ( -0.6823417656250246877, 0.3635416670080895973, 1.181850606188755259 ) ) ;
#130055 = DIRECTION ( 'NONE',  ( 0.9692622846690297500, 0.000000000000000000, -0.2460297208025335747 ) ) ;
#130054 = CIRCLE ( 'NONE', #36563, 1.852123800559096534 ) ;
#130056 = CARTESIAN_POINT ( 'NONE',  ( 0.1021010164683408550, 6.360493866598974755, -3.113991822131910059 ) ) ;
#130057 = CARTESIAN_POINT ( 'NONE',  ( -3.947104627881229622, 8.980740528189222971, 0.7749999999999996891 ) ) ;
#130058 = CARTESIAN_POINT ( 'NONE',  ( 6.666853767972947153, 1.538155548931797956, -1.385880503156889487 ) ) ;
#130059 = CARTESIAN_POINT ( 'NONE',  ( 0.8540665308606997241, -0.7467690478978536994, 1.931163149162813619 ) ) ;
#130061 = CARTESIAN_POINT ( 'NONE',  ( -1.500000000000013101, 1.670833333333355153, 0.8660254037844403729 ) ) ;
#130060 = AXIS2_PLACEMENT_3D ( 'NONE', #22802, #205835, #91052 ) ;
#130062 = CARTESIAN_POINT ( 'NONE',  ( 7.623762449586013901, 7.788811034138823253, 1.040834085586084257E-14 ) ) ;
#130063 = CARTESIAN_POINT ( 'NONE',  ( -6.503107236049161521, 10.73870887536603291, 0.7998128361456481317 ) ) ;
#130064 = CARTESIAN_POINT ( 'NONE',  ( 4.529305835417093640, 7.441884687032027657, -1.199719254218450271 ) ) ;
#130065 = CARTESIAN_POINT ( 'NONE',  ( 5.391314312714450274, -0.05227466736787074464, -2.120015263102632552 ) ) ;
#130066 = CARTESIAN_POINT ( 'NONE',  ( 4.435452530326143616, 5.203724702582467998, -1.199719254218452047 ) ) ;
#130067 = CARTESIAN_POINT ( 'NONE',  ( -1.364683531250012516, 2.988541667008091096, -0.7879004041258289570 ) ) ;
#130068 = CARTESIAN_POINT ( 'NONE',  ( 1.499999999999987121, 2.545833333333351156, -0.8660254037844262731 ) ) ;
#130070 = CARTESIAN_POINT ( 'NONE',  ( 2.333974999846879061, 5.874721266463329705, -0.7998128361456291469 ) ) ;
#130069 = CARTESIAN_POINT ( 'NONE',  ( 6.285602425426498385, -1.847771260692541162, 0.6596951833430019230 ) ) ;
#130071 = CARTESIAN_POINT ( 'NONE',  ( 4.657577273293715514, -0.4389639308803178208, -1.967586094827819654 ) ) ;
#130072 = CARTESIAN_POINT ( 'NONE',  ( 3.995261062014230813, -0.3217480215693402368, 1.888325751980689082 ) ) ;
#130073 = DIRECTION ( 'NONE',  ( 0.7592566023653005702, -0.6507913734559639396, 0.000000000000000000 ) ) ;
#130074 = CARTESIAN_POINT ( 'NONE',  ( 1.734175692058033347, 2.168326105380265378, 0.3173973903456903112 ) ) ;
#130075 = CARTESIAN_POINT ( 'NONE',  ( 6.471393748265519719, 5.229711127717882491, -2.419999999999995044 ) ) ;
#130076 = CARTESIAN_POINT ( 'NONE',  ( 1.499999999999987121, 1.285416667349485120, 0.8660254037844524744 ) ) ;
#130077 = CARTESIAN_POINT ( 'NONE',  ( -7.314787569772770226, 8.492672571945082183, -1.199719254218452935 ) ) ;
#130079 = CARTESIAN_POINT ( 'NONE',  ( 5.519199075762924345, -1.913696209152406125, 0.9060895950074706606 ) ) ;
#130078 = CARTESIAN_POINT ( 'NONE',  ( -4.284013352238262407, 6.021101549076499637, -1.443375672974053447 ) ) ;
#130080 = CARTESIAN_POINT ( 'NONE',  ( -1.316594279187295768, 13.29598046972190595, -0.6183304965053929569 ) ) ;
#130082 = CARTESIAN_POINT ( 'NONE',  ( -7.608060475923978494, 8.905100639113307182, 1.199719254218452047 ) ) ;
#130081 = CARTESIAN_POINT ( 'NONE',  ( 2.577772492168933116, -1.072305133946813260, 1.794659622045821079 ) ) ;
#130084 = ORIENTED_EDGE ( 'NONE', *, *, #129717, .T. ) ;
#130083 = CARTESIAN_POINT ( 'NONE',  ( 0.4281588809218932479, 1.648258183568848789, 0.5080355103465240552 ) ) ;
#130085 = CARTESIAN_POINT ( 'NONE',  ( 5.587931867126699537, 9.671004278289832001, -0.7998128361456291469 ) ) ;
#130086 = PRESENTATION_STYLE_ASSIGNMENT (( #43446 ) ) ;
#130087 = CARTESIAN_POINT ( 'NONE',  ( 7.778383330260374429, -6.134628647623487474, 7.778383330260353112 ) ) ;
#130088 = CARTESIAN_POINT ( 'NONE',  ( -9.333041836230020039, 14.55305236562984383, 7.472413793098202639 ) ) ;
#130090 = CARTESIAN_POINT ( 'NONE',  ( 9.395437264145964917, 10.06369101769952934, -0.7216878364870257245 ) ) ;
#130089 = CARTESIAN_POINT ( 'NONE',  ( 7.091078035147269532, 8.231678114882006625, 1.199719254218462483 ) ) ;
#130091 = ORIENTED_EDGE ( 'NONE', *, *, #82844, .T. ) ;
#130092 = CARTESIAN_POINT ( 'NONE',  ( 5.063152511717405879, 4.908155404373435005, -0.2552525419090029835 ) ) ;
#130093 = ORIENTED_EDGE ( 'NONE', *, *, #141806, .T. ) ;
#130095 = CARTESIAN_POINT ( 'NONE',  ( 1.857782056280156580, 0.6927856907082428073, -1.673962145341382435 ) ) ;
#130094 = CARTESIAN_POINT ( 'NONE',  ( 5.692444392891300886, 7.734547439830227411, -1.599625672291281386 ) ) ;
#130097 = CARTESIAN_POINT ( 'NONE',  ( -7.718669524881690336, 7.899535955317097624, 0.7998128361456462443 ) ) ;
#130096 = AXIS2_PLACEMENT_3D ( 'NONE', #141700, #207712, #189330 ) ;
#130098 = CARTESIAN_POINT ( 'NONE',  ( 5.867981556616276073, 5.740399992340775803, -0.7998128361456281477 ) ) ;
#130099 = CARTESIAN_POINT ( 'NONE',  ( 5.254667053748194760, 8.288139441751686931, 1.199719254218452047 ) ) ;
#130100 = CARTESIAN_POINT ( 'NONE',  ( 6.639320575229255006, 0.6011172813700341733, 1.850849092781511107 ) ) ;
#130101 =( LENGTH_UNIT ( ) NAMED_UNIT ( * ) SI_UNIT ( .MILLI., .METRE. ) );
#130102 = CARTESIAN_POINT ( 'NONE',  ( 4.023704138721054591, 7.562441369377219225, 0.3480857562657164173 ) ) ;
#130103 = CARTESIAN_POINT ( 'NONE',  ( 10.41229878561526512, 11.25002945941372623, -0.7216878364870257245 ) ) ;
#130104 = ADVANCED_FACE ( 'NONE', ( #134389 ), #201451, .F. ) ;
#130105 = CARTESIAN_POINT ( 'NONE',  ( 3.156551239342288095, -0.5378050974185369926, -1.781664776597549293 ) ) ;
#130106 = CARTESIAN_POINT ( 'NONE',  ( 0.2631137269465182449, 1.787087189245086583, -0.6902753917677264539 ) ) ;
#130107 = CARTESIAN_POINT ( 'NONE',  ( 6.721714886968523928, -1.868385559882647318, 0.4688378381374983528 ) ) ;
#130108 = CARTESIAN_POINT ( 'NONE',  ( 0.4019237886466884846, 11.67633545031536535, -1.499999999999994449 ) ) ;
#130109 = CARTESIAN_POINT ( 'NONE',  ( -1.858560999665793911, 8.965769984707671725, 0.7750000000000013545 ) ) ;
#130110 = AXIS2_PLACEMENT_3D ( 'NONE', #111580, #112649, #178658 ) ;
#130111 = STYLED_ITEM ( 'NONE', ( #119115 ), #91223 ) ;
#130112 = CARTESIAN_POINT ( 'NONE',  ( 4.620579464570812256, 8.341333509328540785, -0.3192730525469981151 ) ) ;
#130113 = CARTESIAN_POINT ( 'NONE',  ( 11.86145016429273191, 19.00000000000000000, 1.179999999999997051 ) ) ;
#130114 = CARTESIAN_POINT ( 'NONE',  ( -2.304522924643024773, 5.632434478818063361, 0.7216878364870317197 ) ) ;
#130115 = CARTESIAN_POINT ( 'NONE',  ( 7.239690840017413365, 10.42976116578691403, -1.082531754730537976 ) ) ;
#130116 = CARTESIAN_POINT ( 'NONE',  ( 4.188306824812327633, 1.057184280071225890, -1.661461291525099693 ) ) ;
#130117 = CARTESIAN_POINT ( 'NONE',  ( 1.664851754375612058, 0.6682523891239250391, 2.012492909199379731 ) ) ;
#130118 = CARTESIAN_POINT ( 'NONE',  ( -6.389970470742427189, 6.349387058821269747, -0.7998128361456291469 ) ) ;
#130119 = CARTESIAN_POINT ( 'NONE',  ( -5.070386261386537363, 5.017798181146802428, 1.214306433183764966E-14 ) ) ;
#130120 = CARTESIAN_POINT ( 'NONE',  ( 6.061904079085887354, 6.244845311787889486, 0.000000000000000000 ) ) ;
#130121 = AXIS2_PLACEMENT_3D ( 'NONE', #51235, #34962, #101032 ) ;
#130122 = CARTESIAN_POINT ( 'NONE',  ( 5.683573789218531402, -0.9880169931659465998, 1.956149625775935430 ) ) ;
#130123 = DIRECTION ( 'NONE',  ( -8.638326563840814399E-31, -0.000000000000000000, -1.000000000000000000 ) ) ;
#130124 = CARTESIAN_POINT ( 'NONE',  ( 5.209954918934378121, -1.917094737882633959, 0.1888984193934347133 ) ) ;
#130125 = CARTESIAN_POINT ( 'NONE',  ( -5.208303565944065738, 9.228104593576741621, -0.7998128361456231517 ) ) ;
#130126 = LINE ( 'NONE', #186228, #176296 ) ;
#130127 = CARTESIAN_POINT ( 'NONE',  ( 0.7685542157043163680, 1.090964843879228097, 1.918292034055509632 ) ) ;
#130128 = CARTESIAN_POINT ( 'NONE',  ( -6.096963755015523567, 7.027332905876572333, 0.9867296136132864826 ) ) ;
#130129 = CARTESIAN_POINT ( 'NONE',  ( 0.000000000000000000, -13.99999999999999822, 6.249999999999995559 ) ) ;
#130130 = ORIENTED_EDGE ( 'NONE', *, *, #131984, .F. ) ;
#130131 = EDGE_LOOP ( 'NONE', ( #30396, #147073, #168630, #207790, #19667, #65519, #160029, #132721 ) ) ;
#130132 = CARTESIAN_POINT ( 'NONE',  ( 6.209808219158968967, 0.5752867347804692111, -1.883509059051315271 ) ) ;
#130133 = CARTESIAN_POINT ( 'NONE',  ( 1.083423466712875260, -0.8719414265662344121, 1.735365470925637199 ) ) ;
#130134 = CARTESIAN_POINT ( 'NONE',  ( 0.8958609827393304581, 0.1455075039201655374, 2.010896580075637541 ) ) ;
#130136 = CARTESIAN_POINT ( 'NONE',  ( 5.313276548598107496, -1.570925495967404828, -0.9973500568975323111 ) ) ;
#130135 = CARTESIAN_POINT ( 'NONE',  ( -5.468734858265826837, 7.473552982767158070, 1.599625672291263179 ) ) ;
#130137 = CARTESIAN_POINT ( 'NONE',  ( 5.254667053748194760, 8.288139441751686931, 1.199719254218452047 ) ) ;
#130138 = DIRECTION ( 'NONE',  ( -0.9885327375000381167, 0.000000000000000000, -0.1510067114093955609 ) ) ;
#130139 = CARTESIAN_POINT ( 'NONE',  ( -4.706651882238427120, 8.642844295920152575, 1.040834085586084257E-14 ) ) ;
#130140 = CARTESIAN_POINT ( 'NONE',  ( -6.994027139803241866, 9.253060644560830994, -1.599625672291271394 ) ) ;
#130141 = CARTESIAN_POINT ( 'NONE',  ( 1.857222401600963302, 0.3706860215506869172, -2.159823580554325329 ) ) ;
#130142 = CARTESIAN_POINT ( 'NONE',  ( 3.795919822146273326, 5.451659097302528068, -1.443375672974051449 ) ) ;
#130143 = CARTESIAN_POINT ( 'NONE',  ( -1.326716514427061987E-15, 2.999999999999988454, -1.225000000000003864 ) ) ;
#130144 = DIRECTION ( 'NONE',  ( 0.000000000000000000, 0.000000000000000000, -1.000000000000000000 ) ) ;
#130145 = CARTESIAN_POINT ( 'NONE',  ( 2.015964598666186269, -0.8597642540715648707, -1.610575774528985704 ) ) ;
#130146 = CARTESIAN_POINT ( 'NONE',  ( -2.625475302540713152, 6.214804952939456228, -0.7998128361456281477 ) ) ;
#130147 = CARTESIAN_POINT ( 'NONE',  ( -0.3349625572557037856, 2.646409141035024781, -1.974606604270766619 ) ) ;
#130148 = CARTESIAN_POINT ( 'NONE',  ( 6.609000000000047059, 2.429201845222619394, 2.481963755843877628 ) ) ;
#130149 = CARTESIAN_POINT ( 'NONE',  ( 8.269583629331492602, 11.73526576994040482, 1.199719254218450271 ) ) ;
#130150 = CARTESIAN_POINT ( 'NONE',  ( 6.604126001430527637, -1.825160783932573860, 0.05055279568313279792 ) ) ;
#130151 = CARTESIAN_POINT ( 'NONE',  ( 4.610177715184628155, 1.961415711727178213, -0.04403062578262756377 ) ) ;
#130152 = CARTESIAN_POINT ( 'NONE',  ( -8.259941899223614215, 10.65968485389279508, -1.599625672291263179 ) ) ;
#130153 = CARTESIAN_POINT ( 'NONE',  ( 5.113396490648394632, 9.117379672398465473, 1.040834085586084257E-14 ) ) ;
#130154 = CARTESIAN_POINT ( 'NONE',  ( 4.353197867323560288, 0.4795420089713005041, -2.138300074133951068 ) ) ;
#130155 = CARTESIAN_POINT ( 'NONE',  ( -1.500000000000015099, 9.760416667349465669, -0.8660254037844309360 ) ) ;
#130156 = CARTESIAN_POINT ( 'NONE',  ( 3.678634981485491728, 1.317094234756083893, -1.597214816249421743 ) ) ;
#130157 = CARTESIAN_POINT ( 'NONE',  ( -1.201851678989727383E-14, 1.134375000341418582, 1.575800808251672791 ) ) ;
#130158 = ORIENTED_EDGE ( 'NONE', *, *, #53039, .F. ) ;
#130159 = CARTESIAN_POINT ( 'NONE',  ( 4.553568368667338717, -1.501836741657993191, 1.740358071397982265 ) ) ;
#130160 = CARTESIAN_POINT ( 'NONE',  ( 7.076992996653421741, 10.23994701519558781, -1.082531754730537976 ) ) ;
#130162 = CARTESIAN_POINT ( 'NONE',  ( 1.642778471875001811, -1.042708332855375009, 2.845375778867859751 ) ) ;
#130161 = CARTESIAN_POINT ( 'NONE',  ( 6.373741612200171325, 7.569024981389272710, 1.082531754730549967 ) ) ;
#130163 = CARTESIAN_POINT ( 'NONE',  ( 4.318600669050608687, 4.999583595936801572, -2.499999999999996891 ) ) ;
#130164 = CARTESIAN_POINT ( 'NONE',  ( -10.44468290228067353, 5.054123846477016180, -5.910681132699941998 ) ) ;
#130165 = CARTESIAN_POINT ( 'NONE',  ( 4.154194137148957466, -1.438218894771810641, 1.305048227774636915 ) ) ;
#130166 = ORIENTED_EDGE ( 'NONE', *, *, #195119, .F. ) ;
#130167 = CARTESIAN_POINT ( 'NONE',  ( -0.07995206772520195571, -9.200995477224077845, 9.499751636909056884 ) ) ;
#130168 = CARTESIAN_POINT ( 'NONE',  ( 4.201352949932454450, 1.705870964349815333, -0.8646410313453978258 ) ) ;
#130169 = FACE_OUTER_BOUND ( 'NONE', #175588, .T. ) ;
#130170 = CARTESIAN_POINT ( 'NONE',  ( 5.121954690102882957, -0.9251313946504275965, -1.455449238992040373 ) ) ;
#130171 = CARTESIAN_POINT ( 'NONE',  ( 4.663296154398564042, 1.879804967172087782, -0.7303043177912388328 ) ) ;
#130172 = CARTESIAN_POINT ( 'NONE',  ( 4.676596114989339803, 1.702786692269612212, 1.544373632959222586 ) ) ;
#130173 = CARTESIAN_POINT ( 'NONE',  ( -1.580000000000018723, 8.674529973577529418, 2.499999999999998668 ) ) ;
#130174 = CARTESIAN_POINT ( 'NONE',  ( 0.8739773845415178544, 2.125910683164092152, -0.5920798734769525673 ) ) ;
#130176 = CARTESIAN_POINT ( 'NONE',  ( -4.719646871332968452, 5.639247783710797712, 1.082531754730549078 ) ) ;
#130175 = CARTESIAN_POINT ( 'NONE',  ( -9.130526383799315582, 12.73969898348616070, 1.199719254218462483 ) ) ;
#130177 = CARTESIAN_POINT ( 'NONE',  ( 6.028513167084792457, 1.705988696259161719, 0.4703064415670314413 ) ) ;
#130179 = CARTESIAN_POINT ( 'NONE',  ( 1.553083273963658639, -1.967900166212281476, -1.175304309182874096 ) ) ;
#130178 = CARTESIAN_POINT ( 'NONE',  ( 6.412080304620304538, 6.445458208337293549, -0.7998128361456481317 ) ) ;
#130180 = CARTESIAN_POINT ( 'NONE',  ( 1.429236002152774576, 0.8600564655791165247, -1.512861638240108997 ) ) ;
#130181 = CARTESIAN_POINT ( 'NONE',  ( -1.387358672534890536, 7.315968950354793776, -4.254625267136668221 ) ) ;
#130182 = CARTESIAN_POINT ( 'NONE',  ( 0.9129801003131752246, 0.4962884120854795245, 1.661303041287894411 ) ) ;
#130183 = CARTESIAN_POINT ( 'NONE',  ( 0.6801582343749917881, 1.255208333674727506, 1.178068619123834759 ) ) ;
#130184 = CARTESIAN_POINT ( 'NONE',  ( -11.52469724861192901, 12.22000006648766934, 3.346365485506925808 ) ) ;
#130185 = CARTESIAN_POINT ( 'NONE',  ( 1.029994877853340762, 2.092549206400303063, -0.5788440209302682105 ) ) ;
#130186 = CARTESIAN_POINT ( 'NONE',  ( 2.272673044126482189, -0.3494851828299732621, -1.985868527484459634 ) ) ;
#130187 = CARTESIAN_POINT ( 'NONE',  ( -1.500000000000015099, 0.6604166673494823447, -0.8660254037844313801 ) ) ;
#130188 = CARTESIAN_POINT ( 'NONE',  ( 6.305299685587768543, 1.603216850002240124, 1.067941234924398852 ) ) ;
#130189 = CARTESIAN_POINT ( 'NONE',  ( -8.012344526598182026E-15, 12.79687500034139802, -1.575800808251669460 ) ) ;
#130190 = CARTESIAN_POINT ( 'NONE',  ( 2.022025532713614737, -0.4812968563913700981, 2.168513943247989850 ) ) ;
#130191 = ORIENTED_EDGE ( 'NONE', *, *, #9020, .T. ) ;
#130192 = CARTESIAN_POINT ( 'NONE',  ( 6.625366561259610876, -8.010031549403125339, 6.808607288253734069 ) ) ;
#130193 = CARTESIAN_POINT ( 'NONE',  ( -1.500000000000015099, -0.5791666666666476226, 0.8660254037844403729 ) ) ;
#130194 = CARTESIAN_POINT ( 'NONE',  ( 9.576136569953906275, 10.06658084123472641, 0.000000000000000000 ) ) ;
#130195 = CARTESIAN_POINT ( 'NONE',  ( -10.51568781791557328, 9.987432697960841210, 3.554797817682051164 ) ) ;
#130196 = CARTESIAN_POINT ( 'NONE',  ( 5.020954538418783031, -1.650374644951870806, 0.5528329121840831473 ) ) ;
#130197 = CARTESIAN_POINT ( 'NONE',  ( 4.017981030900905637, 1.947309607215493621, -0.2378496960543720617 ) ) ;
#130199 = CARTESIAN_POINT ( 'NONE',  ( -7.104109303880803417, 8.350844278358124484, 1.082531754730549967 ) ) ;
#130198 = CARTESIAN_POINT ( 'NONE',  ( 4.207107738942202246, 3.802713871720993399, 1.214306433183764966E-14 ) ) ;
#130200 = LINE ( 'NONE', #12097, #554 ) ;
#130201 = CARTESIAN_POINT ( 'NONE',  ( 4.604895111943496211, 1.752856212930454127, -1.430419756957083566 ) ) ;
#130202 = CARTESIAN_POINT ( 'NONE',  ( 1.258340527071156956, -2.062851378465610175, -0.001992840727984764547 ) ) ;
#130203 = CARTESIAN_POINT ( 'NONE',  ( -5.682838942422375084, 9.781729199468104596, 0.000000000000000000 ) ) ;
#130204 =( BOUNDED_SURFACE ( )  B_SPLINE_SURFACE ( 3, 2, ( 
 ( #22686, #68238, #20563 ),
 ( #38970, #72517, #54154 ),
 ( #69301, #135414, #138613 ),
 ( #86646, #155925, #119210 ),
 ( #201435, #137551, #71439 ),
 ( #70367, #4296, #172178 ) ),
 .UNSPECIFIED., .F., .F., .T. ) 
 B_SPLINE_SURFACE_WITH_KNOTS ( ( 4, 2, 4 ),
 ( 3, 3 ),
 ( 0.000000000000000000, 0.0003754689591423960443, 0.0007509379182847920886 ),
 ( 0.000000000000000000, 1.000000000000000000 ),
 .UNSPECIFIED. ) 
 GEOMETRIC_REPRESENTATION_ITEM ( )  RATIONAL_B_SPLINE_SURFACE ( (
 ( 1.000000000000000000, 0.7071067811865475727, 1.000000000000000000),
 ( 1.000000000000000000, 0.7018599272024074187, 1.000000000000000000),
 ( 1.000000000000000000, 0.6927733177260235742, 1.000000000000000000),
 ( 1.000000000000000000, 0.6772007068873748814, 1.000000000000000000),
 ( 1.000000000000000000, 0.6709974581637080382, 1.000000000000000000),
 ( 1.000000000000000000, 0.6711954675835395401, 1.000000000000000000) ) ) 
 REPRESENTATION_ITEM ( '' )  SURFACE ( )  );
#130205 = AXIS2_PLACEMENT_3D ( 'NONE', #77326, #146626, #80529 ) ;
#130206 = CARTESIAN_POINT ( 'NONE',  ( 2.764839853141934256, -1.560785778453818828, 1.638175023747280523 ) ) ;
#130207 = ORIENTED_EDGE ( 'NONE', *, *, #39457, .T. ) ;
#130208 = CARTESIAN_POINT ( 'NONE',  ( -0.7500000000000006661, 1.889583334016155192, -1.299038105676652011 ) ) ;
#130209 = CARTESIAN_POINT ( 'NONE',  ( 2.723731132150861711, -1.073666234122659713, -1.531540996774889640 ) ) ;
#130210 = CARTESIAN_POINT ( 'NONE',  ( 1.529482971743981734, -1.465093928883187901, 0.9274137557628134854 ) ) ;
#130211 = CARTESIAN_POINT ( 'NONE',  ( 5.179302069984247581, 1.471482994053765925, 1.624232740060495228 ) ) ;
#130212 = CARTESIAN_POINT ( 'NONE',  ( 0.3587983166186413109, 0.8468606107991830667, 2.038007455039527294 ) ) ;
#130213 = CARTESIAN_POINT ( 'NONE',  ( 3.995124980148881288, 1.827535992889782523, -1.154293374375232828 ) ) ;
#130214 = CARTESIAN_POINT ( 'NONE',  ( 4.435450497376713486, 0.8291751068889623433, -1.756158939159500276 ) ) ;
#130215 = CARTESIAN_POINT ( 'NONE',  ( -4.270455198180246548, 4.084545274072787890, 0.7216878364870317197 ) ) ;
#130216 = CARTESIAN_POINT ( 'NONE',  ( 6.608674649642057197, 1.385883050205028333, -1.256505298338560062 ) ) ;
#130217 = CARTESIAN_POINT ( 'NONE',  ( 0.4999999999999185651, 1.979557137443526406E-12, -2.052068128417952941 ) ) ;
#130218 = CARTESIAN_POINT ( 'NONE',  ( 5.039007818866061861, 6.552116822607409574, 1.229770346242751389 ) ) ;
#130219 = CARTESIAN_POINT ( 'NONE',  ( 0.08000000000000020983, -7.473374494045017968, -9.579665964948882007 ) ) ;
#130220 = CARTESIAN_POINT ( 'NONE',  ( 11.89942855770814312, 12.30000000000000071, 0.6999999999999992895 ) ) ;
#130221 = CARTESIAN_POINT ( 'NONE',  ( -0.6801582343750282034, 2.682291667008049441, 1.178068619123805227 ) ) ;
#130222 = CARTESIAN_POINT ( 'NONE',  ( 6.117814597332064785, 0.2004318333163370436, 2.006446488866588496 ) ) ;
#130223 = CARTESIAN_POINT ( 'NONE',  ( -8.469039510030723861, 13.03229652834454733, 1.040834085586084257E-14 ) ) ;
#130224 = CARTESIAN_POINT ( 'NONE',  ( 6.259060471003163428, 10.45398764947904624, -0.7998128361456291469 ) ) ;
#130225 = CARTESIAN_POINT ( 'NONE',  ( 2.659371061294801386, -0.4155010417826092151, -0.1333820918543257850 ) ) ;
#130227 = CARTESIAN_POINT ( 'NONE',  ( -4.163573865134853058, 7.871543801636343929, 0.01019316184158518962 ) ) ;
#130226 = CARTESIAN_POINT ( 'NONE',  ( 3.246530741642670304, 0.4443377543969920795, 1.770662692542070538 ) ) ;
#130228 = CARTESIAN_POINT ( 'NONE',  ( -0.1296875068448159474, 0.7431874094961617994, -1.910093690679348200 ) ) ;
#130229 = ORIENTED_EDGE ( 'NONE', *, *, #184537, .T. ) ;
#130230 = CARTESIAN_POINT ( 'NONE',  ( -5.167065940139584868, 6.161236697318522637, 1.082531754730549078 ) ) ;
#130231 = EDGE_CURVE ( 'NONE', #187025, #175932, #32138, .T. ) ;
#130232 = CARTESIAN_POINT ( 'NONE',  ( 1.001543065824772753E-15, -3.609374999522044547, 3.793834371823811669 ) ) ;
#130233 = CARTESIAN_POINT ( 'NONE',  ( -7.797910906154257304, 12.24931315715533486, 0.000000000000000000 ) ) ;
#130234 = CARTESIAN_POINT ( 'NONE',  ( -0.05247081622378191312, -1.844958069526716926, 0.8224554107575526851 ) ) ;
#130235 = CARTESIAN_POINT ( 'NONE',  ( 0.7859742890132662696, 2.042544534415400737, -0.5693509180391894686 ) ) ;
#130236 = VERTEX_POINT ( 'NONE', #4312 ) ;
#130237 = CARTESIAN_POINT ( 'NONE',  ( -5.204350862799341115, 7.165104988056252289, -1.599625672291271394 ) ) ;
#130238 = CARTESIAN_POINT ( 'NONE',  ( 3.897079088924235712, 6.634010472798538949, 1.199719254218462483 ) ) ;
#130239 = CARTESIAN_POINT ( 'NONE',  ( 6.491097285755237145, 1.794469726164525492, -1.013322515520258538 ) ) ;
#130240 = CYLINDRICAL_SURFACE ( 'NONE', #74614, 3.000000000000010214 ) ;
#130241 = ORIENTED_EDGE ( 'NONE', *, *, #212713, .F. ) ;
#130242 = ORIENTED_EDGE ( 'NONE', *, *, #106666, .T. ) ;
#130243 = CARTESIAN_POINT ( 'NONE',  ( -9.215791728987058562, 11.77484298861683598, -1.599625672291263179 ) ) ;
#130244 = CARTESIAN_POINT ( 'NONE',  ( -0.2108831679771203116, 0.7314853703891763814, -1.979988191570913880 ) ) ;
#130245 = PRESENTATION_LAYER_ASSIGNMENT (  '', '', ( #188901 ) ) ;
#130248 = ORIENTED_EDGE ( 'NONE', *, *, #44338, .T. ) ;
#130247 = CARTESIAN_POINT ( 'NONE',  ( 0.07680821025393863577, 5.725641208404781857, -2.404836704152548688 ) ) ;
#130246 = CARTESIAN_POINT ( 'NONE',  ( -6.330731382938325602, 6.350551133041632212, 0.7998128361456281477 ) ) ;
#130249 = CARTESIAN_POINT ( 'NONE',  ( 6.257994703896152089, 7.000112715747270009, 0.9732540237740094913 ) ) ;
#130250 = CARTESIAN_POINT ( 'NONE',  ( 5.800157620552712778, -1.823839058171864203, 0.8595007112896931867 ) ) ;
#130251 = CARTESIAN_POINT ( 'NONE',  ( 5.068220161613846031, -1.734768455660203434, -0.6171159064975312303 ) ) ;
#130252 = CARTESIAN_POINT ( 'NONE',  ( -10.99462144896568283, -5.166862915010298707, 0.3541067150203592862 ) ) ;
#130253 = CARTESIAN_POINT ( 'NONE',  ( 3.387651152892924955, 2.086375235072422285, -0.9864360317304238235 ) ) ;
#130254 = CARTESIAN_POINT ( 'NONE',  ( 6.475954649182838807, 7.584310507915338562, 1.199719254218452047 ) ) ;
#130255 = CARTESIAN_POINT ( 'NONE',  ( 5.712251288600169730, -0.9662322189689104279, -1.933677227328117532 ) ) ;
#130256 = CARTESIAN_POINT ( 'NONE',  ( 7.470706336329915764, 8.674577799595093452, -1.199719254218441611 ) ) ;
#130257 = CARTESIAN_POINT ( 'NONE',  ( 1.083423466712875260, -0.8719414265662344121, 1.735365470925637199 ) ) ;
#130258 = CARTESIAN_POINT ( 'NONE',  ( -4.894657149733403045, 5.669187081899118574, -1.199719254218446718 ) ) ;
#130259 = VERTEX_POINT ( 'NONE', #200392 ) ;
#130260 = PRESENTATION_LAYER_ASSIGNMENT (  '', '', ( #19443 ) ) ;
#130261 = CARTESIAN_POINT ( 'NONE',  ( 4.429307823785958220, 1.078883539000154324, 2.029420160895245129 ) ) ;
#130262 = CARTESIAN_POINT ( 'NONE',  ( 0.07516593201275459379, 0.0004601587237918110533, -2.044269526395313008 ) ) ;
#130263 = CARTESIAN_POINT ( 'NONE',  ( -3.657667580636712934, 7.489305620709952649, -0.7998128361456481317 ) ) ;
#130264 = CARTESIAN_POINT ( 'NONE',  ( 4.733189744967194024, -1.710186631362722531, 0.7584244158565585092 ) ) ;
#130265 = B_SPLINE_CURVE_WITH_KNOTS ( 'NONE', 3,
 ( #157907, #59316, #111339, #28956, #75573, #113474, #141682 ),
 .UNSPECIFIED., .F., .F.,
 ( 4, 3, 4 ),
 ( 0.0001135037245265591781, 0.001517139415464318795, 0.002007692284160929319 ),
 .UNSPECIFIED. ) ;
#130268 = CARTESIAN_POINT ( 'NONE',  ( -4.613517410400161722, 8.604463755433990002, -0.7998128361456362523 ) ) ;
#130267 = CARTESIAN_POINT ( 'NONE',  ( 0.7499999999999885647, 0.3479166673494848983, -1.299038105676652899 ) ) ;
#130266 = CARTESIAN_POINT ( 'NONE',  ( 1.072351618572921605, 0.7776387867773439933, 1.747342548420704800 ) ) ;
#130269 = CARTESIAN_POINT ( 'NONE',  ( 2.631697372267821855, -2.058793095894187353, 0.7952504953367269813 ) ) ;
#130270 = CARTESIAN_POINT ( 'NONE',  ( -1.445367865411041564, 8.714818166637975594, -2.590103969856726085 ) ) ;
#130271 = CARTESIAN_POINT ( 'NONE',  ( 3.999819011231439347, 4.625209253646830554, 1.199719254218464037 ) ) ;
#130272 = CARTESIAN_POINT ( 'NONE',  ( 5.356880090730857802, 8.303424968277756335, 1.082531754730548412 ) ) ;
#130273 = CARTESIAN_POINT ( 'NONE',  ( -4.457933580795036654, 4.095344020549286590, -0.7998128361456221525 ) ) ;
#130274 = TOROIDAL_SURFACE ( 'NONE', #78235, 3.599999999999999201, 0.4999999999999998890 ) ;
#130275 = CARTESIAN_POINT ( 'NONE',  ( -4.950135482320914271, 8.789258806100786359, -0.7216878364870338292 ) ) ;
#130276 = CARTESIAN_POINT ( 'NONE',  ( 1.862511354659317053, -1.396895987378836690, 1.391268958170795100 ) ) ;
#130277 = CARTESIAN_POINT ( 'NONE',  ( 1.149971759812302263, -1.820915985741960785, -1.417348977311111202 ) ) ;
#130278 = CARTESIAN_POINT ( 'NONE',  ( 1.099968687278202406, 0.7983322178258808188, -1.792280776234013828 ) ) ;
#130279 = CARTESIAN_POINT ( 'NONE',  ( 5.084863090169797317, 1.972218467801799102, 0.6036872243675943661 ) ) ;
#130280 = CARTESIAN_POINT ( 'NONE',  ( 3.687454593236936251, 7.245854758844324728, -0.7216878364870267237 ) ) ;
#130281 = CARTESIAN_POINT ( 'NONE',  ( 5.716698046817569434, 6.698511138489155137, -1.199719254218452047 ) ) ;
#130282 = ORIENTED_EDGE ( 'NONE', *, *, #165199, .T. ) ;
#130283 = CARTESIAN_POINT ( 'NONE',  ( 1.499999999999993117, 10.10416666666667140, 0.8660254037844408170 ) ) ;
#130284 = CARTESIAN_POINT ( 'NONE',  ( 10.90726532705803820, -6.287979527546280423, -0.008173644115955716258 ) ) ;
#130285 = CARTESIAN_POINT ( 'NONE',  ( 4.161989969270902812, 4.918371721313249623, 1.082531754730560403 ) ) ;
#130286 = CARTESIAN_POINT ( 'NONE',  ( 1.288188150525194642, -1.375441891341127265, -1.679832657438373511 ) ) ;
#130287 = CARTESIAN_POINT ( 'NONE',  ( -0.08058608058608254798, -9.900000000000005684, -10.99970480893080804 ) ) ;
#130288 = DIRECTION ( 'NONE',  ( -0.5994789404140892231, 4.843714549364036058E-15, -0.8003905296791067325 ) ) ;
#130289 = CARTESIAN_POINT ( 'NONE',  ( -9.549638505170037206, -6.527411821100059797, 0.4330238300980920885 ) ) ;
#130290 = CARTESIAN_POINT ( 'NONE',  ( 1.651402116136031051, 0.5479989942898423338, -1.788454331708405620 ) ) ;
#130291 = CARTESIAN_POINT ( 'NONE',  ( 5.993488848236776967, 1.632462841753023808, 1.416962642945495565 ) ) ;
#130292 = CARTESIAN_POINT ( 'NONE',  ( -5.775368881829861856, 6.228402001981104164, 1.032258425150527126 ) ) ;
#130293 = CARTESIAN_POINT ( 'NONE',  ( -0.02264175331117677936, 7.629137130509094256, -2.689100833419917347 ) ) ;
#130294 = CARTESIAN_POINT ( 'NONE',  ( 1.364683531249986537, -1.136458332991912235, 0.7879004041258500513 ) ) ;
#130295 = CARTESIAN_POINT ( 'NONE',  ( 2.543496672408153358, -1.783599581865771500, 0.6900697577220117340 ) ) ;
#130296 =( BOUNDED_SURFACE ( )  B_SPLINE_SURFACE ( 1, 2, ( 
 ( #52685, #87326, #89479, #86255, #72116, #23370, #54828, #205323, #120978, #36429, #35360, #19106, #103580, #123135, #155534, #7114, #85184, #151268, #71042, #4964, #73187, #102506, #119893, #101435, #22287, #6045, #152325, #68909, #137157, #204238, #3903, #168568, #201042, #55890, #88400, #139293, #69973, #38579, #136084, #167508, #20168, #135029, #138225, #118815, #184800, #202101, #53760, #185869, #186946, #37504, #104654, #154468, #169638, #122047, #21221, #203181, #170702, #188011, #39639, #105747, #171774, #26584, #42871, #172862, #43931, #12459, #141460, #60153, #77469, #193354, #190150, #157675, #159789, #125246, #191206, #75344, #126310, #176058, #108979, #40726, #107917, #207467, #156609, #78535, #62294, #144652, #210667, #173943, #28729, #143588, #11391, #189093, #94815, #25516, #106832, #59086, #192270, #24433, #208518, #27654, #41804, #61227, #160865, #91624, #140378, #58023, #9273, #44998, #76401, #92685, #174998, #90545, #110046, #8199, #158731, #93751, #209581, #111108, #10327, #142510, #127382, #177113, #74284, #206398, #124187, #81740, #212790, #128453, #129518, #163005, #95889, #447, #194421, #198661, #46062, #47134, #66515, #181366, #64427, #115374, #146774, #132657, #49253, #161943, #112184, #30878, #80682, #180314, #79605, #130572, #196561, #164072, #165122, #195498, #14586, #147822, #213840, #179255, #178188, #31934, #32990, #65458, #197609, #131608, #113250, #99068, #145724, #29803, #13535, #48203, #96957, #211723, #16713, #98016, #82798, #148872, #63360, #114315, #15652, #92329, #145355, #111811, #79237, #28355, #58723, #60852, #158370, #174635, #211356, #94450, #25144, #142143, #61927, #208157, #160489, #9963, #144294, #76040, #62980, #95523, #194043, #190839, #44626, #129149, #59787, #91246, #26211, #125946, #45696, #195125, #191902, #128086, #43564, #107541, #109684, #173575, #175687, #157306, #11020, #12096, #110741, #78164, #176741, #42500, #210287, #8896, #29432, #74976, #27276, #141085, #161573, #93383, #159420, #77095, #177816, #13160, #207095, #124874, #143222, #108607, #209212, #127015, #192974, #212413, #76, #97641, #113947, #18480, #182042, #178889, #81367, #1151, #147447, #33673, #31566, #83485, #163698, #84559, #34732, #133349, #130199, #198291, #68286, #15280, #30503, #179942, #213471, #199355, #134418, #65094, #67214, #131251, #2209, #197238, #150648, #48877, #46763, #149568, #112874, #166890, #114995, #96584, #180993, #49933, #162632, #66141, #99748, #47836, #51003, #14207, #32613, #64056, #196193, #98690, #117123, #148509, #164747, #16339, #80302, #116054, #146399, #82420, #132286, #183126, #100804, #165818, #17401, #143405, #48027, #178008, #46953, #195322, #176932, #59975, #193173, #44823, #62120, #110928, #127206, #28550, #29625, #163898, #126129, #160683, #27471, #192089, #114143, #14407, #211544, #80498, #43755, #144477, #146595, #12278, #209401, #94639, #112007, #210482, #15474, #208344, #159614, #128280, #30697, #61045, #78354, #194241, #212613, #45886, #95709, #161763, #13354, #79429, #81558, #109869, #11212, #145547, #96779, #63179, #129344, #180135, #175881, #113070, #179076, #162830, #64253, #93569, #77293, #31762, #130395, #196386, #97833, #181188, #19744, #16534, #32814, #198488, #164941, #199555, #201677, #50133, #184377, #135654, #167087, #103146, #18678, #148701, #147641, #131432, #1345, #20798, #53324, #119457, #197434, #49075, #183320, #51200, #185444, #270, #17596, #213660, #134611, #118388, #116255, #115195, #117322, #102077, #182243, #66340, #98889, #168145, #200615, #37064, #33869, #169206, #68485, #67407, #65285, #99946, #132486, #166011, #83680, #149770, #82616, #133548, #34924, #85825, #52262, #35996, #100997, #84757, #150844, #2406, #151903, #3478, #69545, #7757, #87960, #55459, #154034, #38149, #86894, #105300, #123757, #104221, #39209, #73846, #189720, #108544, #121614, #21853, #141024, #56533, #139940, #205967, #187582, #152960, #71681, #137795, #155104, #203814, #5600, #171336, #122695, #42439, #4535, #22931, #120540, #70609, #207033, #107483, #90112, #173508, #136724, #89046, #188657, #6688, #54400, #186517, #58662, #72764, #40287 ),
 ( #57599, #170267, #106396, #138863, #204880, #124814, #41372, #202748, #172421, #25080, #24010, #91183, #156178, #157244, #8837, #190777, #74916, #174575, #109626, #177754, #50659, #77031, #9903, #93322, #159359, #181707, #116785, #143160, #49593, #209154, #199014, #60793, #66869, #10957, #26152, #62920, #133014, #149226, #126952, #92266, #192910, #29369, #158311, #45631, #79174, #27217, #115717, #801, #44566, #191842, #175630, #110681, #99419, #128029, #78105, #94388, #75979, #95464, #142082, #176681, #111748, #129088, #33337, #28293, #160428, #12033, #144232, #210226, #43505, #161513, #13094, #61864, #208097, #193983, #145291, #59724, #125883, #211295, #195060, #165474, #17069, #83148, #137267, #184909, #71150, #52790, #22404, #153505, #166547, #138328, #19212, #135135, #86363, #150312, #201152, #102620, #70083, #54934, #117863, #69018, #120002, #185979, #101545, #154575, #152434, #21331, #37612, #118929, #88513, #5075, #18135, #204344, #85291, #36533, #4013, #1878, #168675, #20279, #136197, #121086, #183855, #202215, #103693, #169742, #167614, #6151, #53869, #87437, #203287, #187053, #38685, #35467, #104764, #84224, #170813, #56002, #151377, #67938, #72221, #182782, #34400, #100472, #134083, #200091, #51740, #2946, #106944, #159900, #126417, #93862, #42979, #73295, #75451, #172967, #189198, #11507, #109089, #39752, #156715, #76507, #8306, #175104, #24546, #158838, #90654, #77578, #110153, #208626, #205431, #59193, #143701, #74390, #105857, #40835, #140491, #60260, #209693, #206502, #142618, #58133, #122153, #124292, #188121, #190251, #171883, #10435, #23480, #27766, #41909, #89587, #108020, #125348, #155636, #141564, #26691, #123233, #192380, #7221, #174046, #139398, #57069, #25619, #44035, #9380, #91731, #157782, #207572, #191311, #92793, #176166, #146879, #164172, #65562, #62394, #29909, #128559, #63467, #145825, #78638, #212899, #48305, #195608, #127496, #194524, #79710, #28837, #99169, #148972, #16814, #82899, #46172, #115473, #15757, #129622, #81841, #211830, #94925, #165222, #61337, #193467, #45111, #112286, #181466, #147925, #47243, #213941, #113358, #33095, #32034, #111221, #177224, #178302, #13637, #179363, #160974, #30985, #97060, #163113, #131709, #210774, #162047, #64531, #130676, #95994, #12564, #14694, #114416, #196664, #180416, #98120, #80789, #197713, #144763, #49355, #170544, #67681, #182519, #54667, #200887, #167361, #52533, #185714, #169483, #22128, #104500, #199838, #38420, #4806, #186792, #135928, #166287, #168419, #51480, #133825, #88241, #201946, #132758, #35202, #21067, #101277, #53602, #117603, #37348, #183595, #546, #203025, #87165, #83961, #152176, #66611, #18949, #198761, #85033, #151121, #153235, #50410, #2687, #70887, #68760, #116529, #134880, #34149, #118667, #100219, #103422, #17876, #120815, #184650, #150050, #36271, #3745, #1622, #20016, #119736, #102348, #136998, #86104, #69820, #105582, #23210, #205162, #10183, #41649, #206245, #8039, #138067, #9121, #192123, #106678, #25365, #42721, #158583, #155370, #122974, #6955, #156454, #24279, #171616, #91465, #141308, #74129, #5883, #73036, #57870, #208375, #56804, #191056, #142366, #173789, #109901, #157526, #139134, #154311, #204080, #140224, #27504, #60007, #126160, #55733, #121887, #189999, #124033, #43789, #188933, #90385, #71957, #207320, #125098, #40572, #187857, #107763, #108829, #172701, #75196, #89323, #174855, #58941, #175913, #26433, #39484, #92543, #76257, #181217, #62152, #160714, #144509, #128311, #210517, #77324, #45919, #44854, #48059, #14437, #196414, #110960, #194274, #28584, #209434, #30727, #63208, #112038, #80527, #94672, #178040, #12308, #176967, #93604, #29656, #130429, #78389, #95742, #146624, #114172, #115227, #161793, #13384, #147674, #129372, #212641, #64283, #79460, #159649, #145576, #211574, #195351, #46983, #113099, #179105, #96810, #49106, #11246, #162859, #127238, #143437, #213691, #180166, #31792, #97866, #61078, #163927, #15502, #81589, #65313, #131462, #197463, #193207, #54431, #32843, #198517, #101026, #69576, #99978, #149802, #152993, #120573, #134639, #34955, #200644, #167117, #300, #132519 ) ),
 .UNSPECIFIED., .F., .F., .T. ) 
 B_SPLINE_SURFACE_WITH_KNOTS ( ( 2, 2 ),
 ( 3, 2, 2, 2, 2, 2, 2, 2, 2, 2, 2, 2, 2, 2, 2, 2, 2, 2, 2, 2, 2, 2, 2, 2, 2, 2, 2, 2, 2, 2, 2, 2, 2, 2, 2, 2, 2, 2, 2, 2, 2, 2, 2, 2, 2, 2, 2, 2, 2, 2, 2, 2, 2, 2, 2, 2, 2, 2, 2, 2, 2, 2, 2, 2, 2, 2, 2, 2, 2, 2, 2, 2, 2, 2, 2, 2, 2, 2, 2, 2, 2, 2, 2, 2, 2, 2, 2, 2, 2, 2, 2, 2, 2, 2, 2, 2, 2, 2, 2, 2, 2, 2, 2, 2, 2, 2, 2, 2, 2, 2, 2, 2, 2, 2, 2, 2, 2, 2, 2, 2, 2, 2, 2, 2, 2, 2, 2, 2, 2, 2, 2, 2, 2, 2, 2, 2, 2, 2, 2, 2, 2, 2, 2, 2, 2, 2, 2, 2, 2, 2, 2, 2, 2, 2, 2, 2, 2, 2, 2, 2, 2, 2, 2, 2, 2, 2, 2, 2, 2, 2, 2, 2, 2, 2, 2, 2, 2, 2, 2, 2, 2, 2, 2, 2, 2, 2, 2, 2, 2, 2, 2, 2, 2, 2, 2, 2, 2, 2, 2, 2, 2, 2, 2, 2, 2, 2, 2, 2, 2, 2, 2, 2, 2, 2, 2, 2, 2, 2, 2, 2, 2, 2, 2, 2, 2, 2, 2, 2, 2, 2, 2, 2, 2, 2, 2, 2, 2, 2, 2, 2, 3 ),
 ( 0.000000000000000000, 1.000000000000000000 ),
 ( 0.000000000000000000, 0.004166666666666666609, 0.008333333333333333218, 0.01250000000000000069, 0.01666666666666666644, 0.02083333333333333218, 0.02500000000000000139, 0.02916666666666666713, 0.03333333333333333287, 0.03749999999999999861, 0.04166666666666666435, 0.04583333333333333010, 0.05000000000000000278, 0.05416666666666666852, 0.05833333333333333426, 0.06250000000000000000, 0.06666666666666666574, 0.07083333333333333148, 0.07499999999999999722, 0.07916666666666666297, 0.08333333333333332871, 0.08749999999999999445, 0.09166666666666666019, 0.09583333333333333981, 0.1000000000000000056, 0.1041666666666666713, 0.1083333333333333370, 0.1125000000000000028, 0.1166666666666666685, 0.1208333333333333343, 0.1250000000000000000, 0.1291666666666666796, 0.1333333333333333315, 0.1375000000000000111, 0.1416666666666666630, 0.1458333333333333426, 0.1499999999999999944, 0.1541666666666666741, 0.1583333333333333259, 0.1625000000000000056, 0.1666666666666666574, 0.1708333333333333370, 0.1749999999999999889, 0.1791666666666666685, 0.1833333333333333204, 0.1875000000000000000, 0.1916666666666666796, 0.1958333333333333315, 0.2000000000000000111, 0.2041666666666666630, 0.2083333333333333426, 0.2124999999999999944, 0.2166666666666666741, 0.2208333333333333259, 0.2250000000000000056, 0.2291666666666666574, 0.2333333333333333370, 0.2374999999999999889, 0.2416666666666666685, 0.2458333333333333204, 0.2500000000000000000, 0.2541666666666666519, 0.2583333333333333592, 0.2625000000000000111, 0.2666666666666666630, 0.2708333333333333148, 0.2750000000000000222, 0.2791666666666666741, 0.2833333333333333259, 0.2874999999999999778, 0.2916666666666666852, 0.2958333333333333370, 0.2999999999999999889, 0.3041666666666666408, 0.3083333333333333481, 0.3125000000000000000, 0.3166666666666666519, 0.3208333333333333592, 0.3250000000000000111, 0.3291666666666666630, 0.3333333333333333148, 0.3375000000000000222, 0.3416666666666666741, 0.3458333333333333259, 0.3499999999999999778, 0.3541666666666666852, 0.3583333333333333370, 0.3624999999999999889, 0.3666666666666666408, 0.3708333333333333481, 0.3750000000000000000, 0.3791666666666666519, 0.3833333333333333592, 0.3875000000000000111, 0.3916666666666666630, 0.3958333333333333148, 0.4000000000000000222, 0.4041666666666666741, 0.4083333333333333259, 0.4124999999999999778, 0.4166666666666666852, 0.4208333333333333370, 0.4249999999999999889, 0.4291666666666666408, 0.4333333333333333481, 0.4375000000000000000, 0.4416666666666666519, 0.4458333333333333592, 0.4500000000000000111, 0.4541666666666666630, 0.4583333333333333148, 0.4625000000000000222, 0.4666666666666666741, 0.4708333333333333259, 0.4749999999999999778, 0.4791666666666666852, 0.4833333333333333370, 0.4874999999999999889, 0.4916666666666666408, 0.4958333333333333481, 0.5000000000000000000, 0.5041666666666666519, 0.5083333333333333037, 0.5124999999999999556, 0.5166666666666667185, 0.5208333333333333703, 0.5250000000000000222, 0.5291666666666666741, 0.5333333333333333259, 0.5374999999999999778, 0.5416666666666666297, 0.5458333333333332815, 0.5500000000000000444, 0.5541666666666666963, 0.5583333333333333481, 0.5625000000000000000, 0.5666666666666666519, 0.5708333333333333037, 0.5749999999999999556, 0.5791666666666667185, 0.5833333333333333703, 0.5875000000000000222, 0.5916666666666666741, 0.5958333333333333259, 0.5999999999999999778, 0.6041666666666666297, 0.6083333333333332815, 0.6125000000000000444, 0.6166666666666666963, 0.6208333333333333481, 0.6250000000000000000, 0.6291666666666666519, 0.6333333333333333037, 0.6374999999999999556, 0.6416666666666667185, 0.6458333333333333703, 0.6500000000000000222, 0.6541666666666666741, 0.6583333333333333259, 0.6624999999999999778, 0.6666666666666666297, 0.6708333333333332815, 0.6750000000000000444, 0.6791666666666666963, 0.6833333333333333481, 0.6875000000000000000, 0.6916666666666666519, 0.6958333333333333037, 0.6999999999999999556, 0.7041666666666667185, 0.7083333333333333703, 0.7125000000000000222, 0.7166666666666666741, 0.7208333333333333259, 0.7249999999999999778, 0.7291666666666666297, 0.7333333333333332815, 0.7375000000000000444, 0.7416666666666666963, 0.7458333333333333481, 0.7500000000000000000, 0.7541666666666666519, 0.7583333333333333037, 0.7624999999999999556, 0.7666666666666667185, 0.7708333333333333703, 0.7750000000000000222, 0.7791666666666666741, 0.7833333333333333259, 0.7874999999999999778, 0.7916666666666666297, 0.7958333333333332815, 0.8000000000000000444, 0.8041666666666666963, 0.8083333333333333481, 0.8125000000000000000, 0.8166666666666666519, 0.8208333333333333037, 0.8249999999999999556, 0.8291666666666667185, 0.8333333333333333703, 0.8375000000000000222, 0.8416666666666666741, 0.8458333333333333259, 0.8499999999999999778, 0.8541666666666666297, 0.8583333333333332815, 0.8625000000000000444, 0.8666666666666666963, 0.8708333333333333481, 0.8750000000000000000, 0.8791666666666666519, 0.8833333333333333037, 0.8874999999999999556, 0.8916666666666667185, 0.8958333333333333703, 0.9000000000000000222, 0.9041666666666666741, 0.9083333333333333259, 0.9124999999999999778, 0.9166666666666666297, 0.9208333333333332815, 0.9250000000000000444, 0.9291666666666666963, 0.9333333333333333481, 0.9375000000000000000, 0.9416666666666666519, 0.9458333333333333037, 0.9499999999999999556, 0.9541666666666667185, 0.9583333333333333703, 0.9625000000000000222, 0.9666666666666666741, 0.9708333333333333259, 0.9749999999999999778, 0.9791666666666666297, 0.9833333333333332815, 0.9875000000000000444, 0.9916666666666666963, 0.9958333333333333481, 1.000000000000000000 ),
 .UNSPECIFIED. ) 
 GEOMETRIC_REPRESENTATION_ITEM ( )  RATIONAL_B_SPLINE_SURFACE ( (
 ( 1.000000000000000000, 0.8660254037844387076, 1.000000000000000000, 0.8660254037844387076, 1.000000000000000000, 0.8660254037844387076, 1.000000000000000000, 0.8660254037844387076, 1.000000000000000000, 0.8660254037844387076, 1.000000000000000000, 0.8660254037844387076, 1.000000000000000000, 0.8660254037844387076, 1.000000000000000000, 0.8660254037844387076, 1.000000000000000000, 0.8660254037844387076, 1.000000000000000000, 0.8660254037844387076, 1.000000000000000000, 0.8660254037844387076, 1.000000000000000000, 0.8660254037844387076, 1.000000000000000000, 0.8660254037844387076, 1.000000000000000000, 0.8660254037844387076, 1.000000000000000000, 0.8660254037844387076, 1.000000000000000000, 0.8660254037844387076, 1.000000000000000000, 0.8660254037844387076, 1.000000000000000000, 0.8660254037844387076, 1.000000000000000000, 0.8660254037844387076, 1.000000000000000000, 0.8660254037844387076, 1.000000000000000000, 0.8660254037844387076, 1.000000000000000000, 0.8660254037844387076, 1.000000000000000000, 0.8660254037844387076, 1.000000000000000000, 0.8660254037844387076, 1.000000000000000000, 0.8660254037844387076, 1.000000000000000000, 0.8660254037844387076, 1.000000000000000000, 0.8660254037844387076, 1.000000000000000000, 0.8660254037844387076, 1.000000000000000000, 0.8660254037844387076, 1.000000000000000000, 0.8660254037844387076, 1.000000000000000000, 0.8660254037844387076, 1.000000000000000000, 0.8660254037844387076, 1.000000000000000000, 0.8660254037844387076, 1.000000000000000000, 0.8660254037844387076, 1.000000000000000000, 0.8660254037844387076, 1.000000000000000000, 0.8660254037844387076, 1.000000000000000000, 0.8660254037844387076, 1.000000000000000000, 0.8660254037844387076, 1.000000000000000000, 0.8660254037844387076, 1.000000000000000000, 0.8660254037844387076, 1.000000000000000000, 0.8660254037844387076, 1.000000000000000000, 0.8660254037844387076, 1.000000000000000000, 0.8660254037844387076, 1.000000000000000000, 0.8660254037844387076, 1.000000000000000000, 0.8660254037844387076, 1.000000000000000000, 0.8660254037844387076, 1.000000000000000000, 0.8660254037844387076, 1.000000000000000000, 0.8660254037844387076, 1.000000000000000000, 0.8660254037844387076, 1.000000000000000000, 0.8660254037844387076, 1.000000000000000000, 0.8660254037844387076, 1.000000000000000000, 0.8660254037844387076, 1.000000000000000000, 0.8660254037844387076, 1.000000000000000000, 0.8660254037844387076, 1.000000000000000000, 0.8660254037844387076, 1.000000000000000000, 0.8660254037844387076, 1.000000000000000000, 0.8660254037844387076, 1.000000000000000000, 0.8660254037844387076, 1.000000000000000000, 0.8660254037844387076, 1.000000000000000000, 0.8660254037844387076, 1.000000000000000000, 0.8660254037844387076, 1.000000000000000000, 0.8660254037844387076, 1.000000000000000000, 0.8660254037844387076, 1.000000000000000000, 0.8660254037844387076, 1.000000000000000000, 0.8660254037844387076, 1.000000000000000000, 0.8660254037844387076, 1.000000000000000000, 0.8660254037844387076, 1.000000000000000000, 0.8660254037844387076, 1.000000000000000000, 0.8660254037844387076, 1.000000000000000000, 0.8660254037844387076, 1.000000000000000000, 0.8660254037844387076, 1.000000000000000000, 0.8660254037844387076, 1.000000000000000000, 0.8660254037844387076, 1.000000000000000000, 0.8660254037844387076, 1.000000000000000000, 0.8660254037844387076, 1.000000000000000000, 0.8660254037844387076, 1.000000000000000000, 0.8660254037844387076, 1.000000000000000000, 0.8660254037844387076, 1.000000000000000000, 0.8660254037844387076, 1.000000000000000000, 0.8660254037844387076, 1.000000000000000000, 0.8660254037844387076, 1.000000000000000000, 0.8660254037844387076, 1.000000000000000000, 0.8660254037844387076, 1.000000000000000000, 0.8660254037844387076, 1.000000000000000000, 0.8660254037844387076, 1.000000000000000000, 0.8660254037844387076, 1.000000000000000000, 0.8660254037844387076, 1.000000000000000000, 0.8660254037844387076, 1.000000000000000000, 0.8660254037844387076, 1.000000000000000000, 0.8660254037844387076, 1.000000000000000000, 0.8660254037844387076, 1.000000000000000000, 0.8660254037844387076, 1.000000000000000000, 0.8660254037844387076, 1.000000000000000000, 0.8660254037844387076, 1.000000000000000000, 0.8660254037844387076, 1.000000000000000000, 0.8660254037844387076, 1.000000000000000000, 0.8660254037844387076, 1.000000000000000000, 0.8660254037844387076, 1.000000000000000000, 0.8660254037844387076, 1.000000000000000000, 0.8660254037844387076, 1.000000000000000000, 0.8660254037844387076, 1.000000000000000000, 0.8660254037844387076, 1.000000000000000000, 0.8660254037844387076, 1.000000000000000000, 0.8660254037844387076, 1.000000000000000000, 0.8660254037844387076, 1.000000000000000000, 0.8660254037844387076, 1.000000000000000000, 0.8660254037844387076, 1.000000000000000000, 0.8660254037844387076, 1.000000000000000000, 0.8660254037844387076, 1.000000000000000000, 0.8660254037844387076, 1.000000000000000000, 0.8660254037844387076, 1.000000000000000000, 0.8660254037844387076, 1.000000000000000000, 0.8660254037844387076, 1.000000000000000000, 0.8660254037844387076, 1.000000000000000000, 0.8660254037844387076, 1.000000000000000000, 0.8660254037844387076, 1.000000000000000000, 0.8660254037844387076, 1.000000000000000000, 0.8660254037844387076, 1.000000000000000000, 0.8660254037844387076, 1.000000000000000000, 0.8660254037844387076, 1.000000000000000000, 0.8660254037844387076, 1.000000000000000000, 0.8660254037844387076, 1.000000000000000000, 0.8660254037844387076, 1.000000000000000000, 0.8660254037844387076, 1.000000000000000000, 0.8660254037844387076, 1.000000000000000000, 0.8660254037844387076, 1.000000000000000000, 0.8660254037844387076, 1.000000000000000000, 0.8660254037844387076, 1.000000000000000000, 0.8660254037844387076, 1.000000000000000000, 0.8660254037844387076, 1.000000000000000000, 0.8660254037844387076, 1.000000000000000000, 0.8660254037844387076, 1.000000000000000000, 0.8660254037844387076, 1.000000000000000000, 0.8660254037844387076, 1.000000000000000000, 0.8660254037844387076, 1.000000000000000000, 0.8660254037844387076, 1.000000000000000000, 0.8660254037844387076, 1.000000000000000000, 0.8660254037844387076, 1.000000000000000000, 0.8660254037844387076, 1.000000000000000000, 0.8660254037844387076, 1.000000000000000000, 0.8660254037844387076, 1.000000000000000000, 0.8660254037844387076, 1.000000000000000000, 0.8660254037844387076, 1.000000000000000000, 0.8660254037844387076, 1.000000000000000000, 0.8660254037844387076, 1.000000000000000000, 0.8660254037844387076, 1.000000000000000000, 0.8660254037844387076, 1.000000000000000000, 0.8660254037844387076, 1.000000000000000000, 0.8660254037844387076, 1.000000000000000000, 0.8660254037844387076, 1.000000000000000000, 0.8660254037844387076, 1.000000000000000000, 0.8660254037844387076, 1.000000000000000000, 0.8660254037844387076, 1.000000000000000000, 0.8660254037844387076, 1.000000000000000000, 0.8660254037844387076, 1.000000000000000000, 0.8660254037844387076, 1.000000000000000000, 0.8660254037844387076, 1.000000000000000000, 0.8660254037844387076, 1.000000000000000000, 0.8660254037844387076, 1.000000000000000000, 0.8660254037844387076, 1.000000000000000000, 0.8660254037844387076, 1.000000000000000000, 0.8660254037844387076, 1.000000000000000000, 0.8660254037844387076, 1.000000000000000000, 0.8660254037844387076, 1.000000000000000000, 0.8660254037844387076, 1.000000000000000000, 0.8660254037844387076, 1.000000000000000000, 0.8660254037844387076, 1.000000000000000000, 0.8660254037844387076, 1.000000000000000000, 0.8660254037844387076, 1.000000000000000000, 0.8660254037844387076, 1.000000000000000000, 0.8660254037844387076, 1.000000000000000000, 0.8660254037844387076, 1.000000000000000000, 0.8660254037844387076, 1.000000000000000000, 0.8660254037844387076, 1.000000000000000000, 0.8660254037844387076, 1.000000000000000000, 0.8660254037844387076, 1.000000000000000000, 0.8660254037844387076, 1.000000000000000000, 0.8660254037844387076, 1.000000000000000000, 0.8660254037844387076, 1.000000000000000000, 0.8660254037844387076, 1.000000000000000000, 0.8660254037844387076, 1.000000000000000000, 0.8660254037844387076, 1.000000000000000000, 0.8660254037844387076, 1.000000000000000000, 0.8660254037844387076, 1.000000000000000000, 0.8660254037844387076, 1.000000000000000000, 0.8660254037844387076, 1.000000000000000000, 0.8660254037844387076, 1.000000000000000000, 0.8660254037844387076, 1.000000000000000000, 0.8660254037844387076, 1.000000000000000000, 0.8660254037844387076, 1.000000000000000000, 0.8660254037844387076, 1.000000000000000000, 0.8660254037844387076, 1.000000000000000000, 0.8660254037844387076, 1.000000000000000000, 0.8660254037844387076, 1.000000000000000000, 0.8660254037844387076, 1.000000000000000000, 0.8660254037844387076, 1.000000000000000000, 0.8660254037844387076, 1.000000000000000000, 0.8660254037844387076, 1.000000000000000000, 0.8660254037844387076, 1.000000000000000000, 0.8660254037844387076, 1.000000000000000000, 0.8660254037844387076, 1.000000000000000000, 0.8660254037844387076, 1.000000000000000000, 0.8660254037844387076, 1.000000000000000000, 0.8660254037844387076, 1.000000000000000000, 0.8660254037844387076, 1.000000000000000000, 0.8660254037844387076, 1.000000000000000000, 0.8660254037844387076, 1.000000000000000000, 0.8660254037844387076, 1.000000000000000000, 0.8660254037844387076, 1.000000000000000000, 0.8660254037844387076, 1.000000000000000000, 0.8660254037844387076, 1.000000000000000000, 0.8660254037844387076, 1.000000000000000000, 0.8660254037844387076, 1.000000000000000000, 0.8660254037844387076, 1.000000000000000000, 0.8660254037844387076, 1.000000000000000000, 0.8660254037844387076, 1.000000000000000000, 0.8660254037844387076, 1.000000000000000000, 0.8660254037844387076, 1.000000000000000000, 0.8660254037844387076, 1.000000000000000000, 0.8660254037844387076, 1.000000000000000000, 0.8660254037844387076, 1.000000000000000000, 0.8660254037844387076, 1.000000000000000000, 0.8660254037844387076, 1.000000000000000000, 0.8660254037844387076, 1.000000000000000000, 0.8660254037844387076, 1.000000000000000000, 0.8660254037844387076, 1.000000000000000000, 0.8660254037844387076, 1.000000000000000000, 0.8660254037844387076, 1.000000000000000000, 0.8660254037844387076, 1.000000000000000000, 0.8660254037844387076, 1.000000000000000000, 0.8660254037844387076, 1.000000000000000000, 0.8660254037844387076, 1.000000000000000000, 0.8660254037844387076, 1.000000000000000000, 0.8660254037844387076, 1.000000000000000000, 0.8660254037844387076, 1.000000000000000000, 0.8660254037844387076, 1.000000000000000000, 0.8660254037844387076, 1.000000000000000000, 0.8660254037844387076, 1.000000000000000000, 0.8660254037844387076, 1.000000000000000000, 0.8660254037844387076, 1.000000000000000000),
 ( 1.000000000000000000, 0.8660254037844387076, 1.000000000000000000, 0.8660254037844387076, 1.000000000000000000, 0.8660254037844387076, 1.000000000000000000, 0.8660254037844387076, 1.000000000000000000, 0.8660254037844387076, 1.000000000000000000, 0.8660254037844387076, 1.000000000000000000, 0.8660254037844387076, 1.000000000000000000, 0.8660254037844387076, 1.000000000000000000, 0.8660254037844387076, 1.000000000000000000, 0.8660254037844387076, 1.000000000000000000, 0.8660254037844387076, 1.000000000000000000, 0.8660254037844387076, 1.000000000000000000, 0.8660254037844387076, 1.000000000000000000, 0.8660254037844387076, 1.000000000000000000, 0.8660254037844387076, 1.000000000000000000, 0.8660254037844387076, 1.000000000000000000, 0.8660254037844387076, 1.000000000000000000, 0.8660254037844387076, 1.000000000000000000, 0.8660254037844387076, 1.000000000000000000, 0.8660254037844387076, 1.000000000000000000, 0.8660254037844387076, 1.000000000000000000, 0.8660254037844387076, 1.000000000000000000, 0.8660254037844387076, 1.000000000000000000, 0.8660254037844387076, 1.000000000000000000, 0.8660254037844387076, 1.000000000000000000, 0.8660254037844387076, 1.000000000000000000, 0.8660254037844387076, 1.000000000000000000, 0.8660254037844387076, 1.000000000000000000, 0.8660254037844387076, 1.000000000000000000, 0.8660254037844387076, 1.000000000000000000, 0.8660254037844387076, 1.000000000000000000, 0.8660254037844387076, 1.000000000000000000, 0.8660254037844387076, 1.000000000000000000, 0.8660254037844387076, 1.000000000000000000, 0.8660254037844387076, 1.000000000000000000, 0.8660254037844387076, 1.000000000000000000, 0.8660254037844387076, 1.000000000000000000, 0.8660254037844387076, 1.000000000000000000, 0.8660254037844387076, 1.000000000000000000, 0.8660254037844387076, 1.000000000000000000, 0.8660254037844387076, 1.000000000000000000, 0.8660254037844387076, 1.000000000000000000, 0.8660254037844387076, 1.000000000000000000, 0.8660254037844387076, 1.000000000000000000, 0.8660254037844387076, 1.000000000000000000, 0.8660254037844387076, 1.000000000000000000, 0.8660254037844387076, 1.000000000000000000, 0.8660254037844387076, 1.000000000000000000, 0.8660254037844387076, 1.000000000000000000, 0.8660254037844387076, 1.000000000000000000, 0.8660254037844387076, 1.000000000000000000, 0.8660254037844387076, 1.000000000000000000, 0.8660254037844387076, 1.000000000000000000, 0.8660254037844387076, 1.000000000000000000, 0.8660254037844387076, 1.000000000000000000, 0.8660254037844387076, 1.000000000000000000, 0.8660254037844387076, 1.000000000000000000, 0.8660254037844387076, 1.000000000000000000, 0.8660254037844387076, 1.000000000000000000, 0.8660254037844387076, 1.000000000000000000, 0.8660254037844387076, 1.000000000000000000, 0.8660254037844387076, 1.000000000000000000, 0.8660254037844387076, 1.000000000000000000, 0.8660254037844387076, 1.000000000000000000, 0.8660254037844387076, 1.000000000000000000, 0.8660254037844387076, 1.000000000000000000, 0.8660254037844387076, 1.000000000000000000, 0.8660254037844387076, 1.000000000000000000, 0.8660254037844387076, 1.000000000000000000, 0.8660254037844387076, 1.000000000000000000, 0.8660254037844387076, 1.000000000000000000, 0.8660254037844387076, 1.000000000000000000, 0.8660254037844387076, 1.000000000000000000, 0.8660254037844387076, 1.000000000000000000, 0.8660254037844387076, 1.000000000000000000, 0.8660254037844387076, 1.000000000000000000, 0.8660254037844387076, 1.000000000000000000, 0.8660254037844387076, 1.000000000000000000, 0.8660254037844387076, 1.000000000000000000, 0.8660254037844387076, 1.000000000000000000, 0.8660254037844387076, 1.000000000000000000, 0.8660254037844387076, 1.000000000000000000, 0.8660254037844387076, 1.000000000000000000, 0.8660254037844387076, 1.000000000000000000, 0.8660254037844387076, 1.000000000000000000, 0.8660254037844387076, 1.000000000000000000, 0.8660254037844387076, 1.000000000000000000, 0.8660254037844387076, 1.000000000000000000, 0.8660254037844387076, 1.000000000000000000, 0.8660254037844387076, 1.000000000000000000, 0.8660254037844387076, 1.000000000000000000, 0.8660254037844387076, 1.000000000000000000, 0.8660254037844387076, 1.000000000000000000, 0.8660254037844387076, 1.000000000000000000, 0.8660254037844387076, 1.000000000000000000, 0.8660254037844387076, 1.000000000000000000, 0.8660254037844387076, 1.000000000000000000, 0.8660254037844387076, 1.000000000000000000, 0.8660254037844387076, 1.000000000000000000, 0.8660254037844387076, 1.000000000000000000, 0.8660254037844387076, 1.000000000000000000, 0.8660254037844387076, 1.000000000000000000, 0.8660254037844387076, 1.000000000000000000, 0.8660254037844387076, 1.000000000000000000, 0.8660254037844387076, 1.000000000000000000, 0.8660254037844387076, 1.000000000000000000, 0.8660254037844387076, 1.000000000000000000, 0.8660254037844387076, 1.000000000000000000, 0.8660254037844387076, 1.000000000000000000, 0.8660254037844387076, 1.000000000000000000, 0.8660254037844387076, 1.000000000000000000, 0.8660254037844387076, 1.000000000000000000, 0.8660254037844387076, 1.000000000000000000, 0.8660254037844387076, 1.000000000000000000, 0.8660254037844387076, 1.000000000000000000, 0.8660254037844387076, 1.000000000000000000, 0.8660254037844387076, 1.000000000000000000, 0.8660254037844387076, 1.000000000000000000, 0.8660254037844387076, 1.000000000000000000, 0.8660254037844387076, 1.000000000000000000, 0.8660254037844387076, 1.000000000000000000, 0.8660254037844387076, 1.000000000000000000, 0.8660254037844387076, 1.000000000000000000, 0.8660254037844387076, 1.000000000000000000, 0.8660254037844387076, 1.000000000000000000, 0.8660254037844387076, 1.000000000000000000, 0.8660254037844387076, 1.000000000000000000, 0.8660254037844387076, 1.000000000000000000, 0.8660254037844387076, 1.000000000000000000, 0.8660254037844387076, 1.000000000000000000, 0.8660254037844387076, 1.000000000000000000, 0.8660254037844387076, 1.000000000000000000, 0.8660254037844387076, 1.000000000000000000, 0.8660254037844387076, 1.000000000000000000, 0.8660254037844387076, 1.000000000000000000, 0.8660254037844387076, 1.000000000000000000, 0.8660254037844387076, 1.000000000000000000, 0.8660254037844387076, 1.000000000000000000, 0.8660254037844387076, 1.000000000000000000, 0.8660254037844387076, 1.000000000000000000, 0.8660254037844387076, 1.000000000000000000, 0.8660254037844387076, 1.000000000000000000, 0.8660254037844387076, 1.000000000000000000, 0.8660254037844387076, 1.000000000000000000, 0.8660254037844387076, 1.000000000000000000, 0.8660254037844387076, 1.000000000000000000, 0.8660254037844387076, 1.000000000000000000, 0.8660254037844387076, 1.000000000000000000, 0.8660254037844387076, 1.000000000000000000, 0.8660254037844387076, 1.000000000000000000, 0.8660254037844387076, 1.000000000000000000, 0.8660254037844387076, 1.000000000000000000, 0.8660254037844387076, 1.000000000000000000, 0.8660254037844387076, 1.000000000000000000, 0.8660254037844387076, 1.000000000000000000, 0.8660254037844387076, 1.000000000000000000, 0.8660254037844387076, 1.000000000000000000, 0.8660254037844387076, 1.000000000000000000, 0.8660254037844387076, 1.000000000000000000, 0.8660254037844387076, 1.000000000000000000, 0.8660254037844387076, 1.000000000000000000, 0.8660254037844387076, 1.000000000000000000, 0.8660254037844387076, 1.000000000000000000, 0.8660254037844387076, 1.000000000000000000, 0.8660254037844387076, 1.000000000000000000, 0.8660254037844387076, 1.000000000000000000, 0.8660254037844387076, 1.000000000000000000, 0.8660254037844387076, 1.000000000000000000, 0.8660254037844387076, 1.000000000000000000, 0.8660254037844387076, 1.000000000000000000, 0.8660254037844387076, 1.000000000000000000, 0.8660254037844387076, 1.000000000000000000, 0.8660254037844387076, 1.000000000000000000, 0.8660254037844387076, 1.000000000000000000, 0.8660254037844387076, 1.000000000000000000, 0.8660254037844387076, 1.000000000000000000, 0.8660254037844387076, 1.000000000000000000, 0.8660254037844387076, 1.000000000000000000, 0.8660254037844387076, 1.000000000000000000, 0.8660254037844387076, 1.000000000000000000, 0.8660254037844387076, 1.000000000000000000, 0.8660254037844387076, 1.000000000000000000, 0.8660254037844387076, 1.000000000000000000, 0.8660254037844387076, 1.000000000000000000, 0.8660254037844387076, 1.000000000000000000, 0.8660254037844387076, 1.000000000000000000, 0.8660254037844387076, 1.000000000000000000, 0.8660254037844387076, 1.000000000000000000, 0.8660254037844387076, 1.000000000000000000, 0.8660254037844387076, 1.000000000000000000, 0.8660254037844387076, 1.000000000000000000, 0.8660254037844387076, 1.000000000000000000, 0.8660254037844387076, 1.000000000000000000, 0.8660254037844387076, 1.000000000000000000, 0.8660254037844387076, 1.000000000000000000, 0.8660254037844387076, 1.000000000000000000, 0.8660254037844387076, 1.000000000000000000, 0.8660254037844387076, 1.000000000000000000, 0.8660254037844387076, 1.000000000000000000, 0.8660254037844387076, 1.000000000000000000, 0.8660254037844387076, 1.000000000000000000, 0.8660254037844387076, 1.000000000000000000, 0.8660254037844387076, 1.000000000000000000, 0.8660254037844387076, 1.000000000000000000, 0.8660254037844387076, 1.000000000000000000, 0.8660254037844387076, 1.000000000000000000, 0.8660254037844387076, 1.000000000000000000, 0.8660254037844387076, 1.000000000000000000, 0.8660254037844387076, 1.000000000000000000, 0.8660254037844387076, 1.000000000000000000, 0.8660254037844387076, 1.000000000000000000, 0.8660254037844387076, 1.000000000000000000, 0.8660254037844387076, 1.000000000000000000, 0.8660254037844387076, 1.000000000000000000, 0.8660254037844387076, 1.000000000000000000, 0.8660254037844387076, 1.000000000000000000, 0.8660254037844387076, 1.000000000000000000, 0.8660254037844387076, 1.000000000000000000, 0.8660254037844387076, 1.000000000000000000, 0.8660254037844387076, 1.000000000000000000, 0.8660254037844387076, 1.000000000000000000, 0.8660254037844387076, 1.000000000000000000, 0.8660254037844387076, 1.000000000000000000, 0.8660254037844387076, 1.000000000000000000, 0.8660254037844387076, 1.000000000000000000, 0.8660254037844387076, 1.000000000000000000, 0.8660254037844387076, 1.000000000000000000, 0.8660254037844387076, 1.000000000000000000, 0.8660254037844387076, 1.000000000000000000, 0.8660254037844387076, 1.000000000000000000, 0.8660254037844387076, 1.000000000000000000, 0.8660254037844387076, 1.000000000000000000, 0.8660254037844387076, 1.000000000000000000, 0.8660254037844387076, 1.000000000000000000, 0.8660254037844387076, 1.000000000000000000, 0.8660254037844387076, 1.000000000000000000, 0.8660254037844387076, 1.000000000000000000, 0.8660254037844387076, 1.000000000000000000, 0.8660254037844387076, 1.000000000000000000, 0.8660254037844387076, 1.000000000000000000) ) ) 
 REPRESENTATION_ITEM ( '' )  SURFACE ( )  );
#130297 = CARTESIAN_POINT ( 'NONE',  ( 4.574921169738827231, -0.001286399002502561879, -1.770032026507301515 ) ) ;
#130298 = CARTESIAN_POINT ( 'NONE',  ( 0.4692111731946085884, -1.615589042895089200, -1.022764193708516789 ) ) ;
#130299 = CARTESIAN_POINT ( 'NONE',  ( -5.253948220495577637, 6.088359997788290734, 1.199719254218450271 ) ) ;
#130301 = CARTESIAN_POINT ( 'NONE',  ( 4.956599115817130752, -1.805213640821627052, -0.6413244422398997058 ) ) ;
#130300 = CARTESIAN_POINT ( 'NONE',  ( 2.579764790942817854, -3.169229722560920504, -2.142845477429654810 ) ) ;
#130302 = CARTESIAN_POINT ( 'NONE',  ( 6.602011381505620946, 0.7551138498248446407, -1.819252348156335852 ) ) ;
#130303 = CARTESIAN_POINT ( 'NONE',  ( -1.201851678989727383E-14, 4.337500000000023448, -1.732050807568863648 ) ) ;
#130304 = CARTESIAN_POINT ( 'NONE',  ( 1.986737319265439394, -1.300789755646198476, 1.674730562594067829 ) ) ;
#130305 = SURFACE_SIDE_STYLE ('',( #31668 ) ) ;
#130306 = CARTESIAN_POINT ( 'NONE',  ( 4.610133579271312954, -0.8000244862099057386, -1.691074300901610261 ) ) ;
#130308 = ORIENTED_EDGE ( 'NONE', *, *, #186461, .T. ) ;
#130307 = CARTESIAN_POINT ( 'NONE',  ( 0.5041868517345666767, -0.6120625888205477594, -1.720162557568189809 ) ) ;
#130310 = CARTESIAN_POINT ( 'NONE',  ( 4.693755526227673336, 8.251780594207492214, -0.6034641085399840010 ) ) ;
#130309 = CARTESIAN_POINT ( 'NONE',  ( 4.582781371344160526, -2.140174514510746029, -0.5380331057033281850 ) ) ;
#130311 = CARTESIAN_POINT ( 'NONE',  ( -0.6823417656250246877, -1.198958332991911790, 1.181850606188755259 ) ) ;
#130312 = CARTESIAN_POINT ( 'NONE',  ( 1.820832581213110313, -1.460207654653251419, 1.457104742506893036 ) ) ;
#130313 = CARTESIAN_POINT ( 'NONE',  ( 6.148786358997489820, 7.132337826040578754, -1.199719254218446718 ) ) ;
#130314 = CARTESIAN_POINT ( 'NONE',  ( -7.018317073368468328, 11.33978701890523233, -0.7998128361456291469 ) ) ;
#130315 = SURFACE_STYLE_FILL_AREA ( #210400 ) ;
#130316 = CARTESIAN_POINT ( 'NONE',  ( 9.297140650669039275, 11.86975006391249643, 1.599625672291281386 ) ) ;
#130317 = SURFACE_STYLE_USAGE ( .BOTH. , #77207 ) ;
#130318 = CARTESIAN_POINT ( 'NONE',  ( 8.154303043976348420, 8.478051404252736845, 0.7998128361456281477 ) ) ;
#130319 = VERTEX_POINT ( 'NONE', #82404 ) ;
#130320 = CARTESIAN_POINT ( 'NONE',  ( 3.807136610393092813, -1.694265131726957252, 1.189645435975445809 ) ) ;
#130321 = CARTESIAN_POINT ( 'NONE',  ( 1.499999999999990896, 5.775000000000023448, 1.040834085586084257E-14 ) ) ;
#130322 = CARTESIAN_POINT ( 'NONE',  ( 1.405796033167511894, -0.5266655099175953092, 2.096309153942426562 ) ) ;
#130323 = CARTESIAN_POINT ( 'NONE',  ( -5.686128154004278734, 7.329579007619248188, -1.223094714244008729 ) ) ;
#130324 = CARTESIAN_POINT ( 'NONE',  ( 2.051431352050979040, -1.803145959232739237, 0.9099833227969624794 ) ) ;
#130325 = CARTESIAN_POINT ( 'NONE',  ( 4.324687812634882000, 7.028924300507257250, 1.082531754730558626 ) ) ;
#130326 = PRODUCT_DEFINITION_SHAPE ( 'NONE', 'NONE',  #214425 ) ;
#130327 = ORIENTED_EDGE ( 'NONE', *, *, #177138, .T. ) ;
#130329 = CARTESIAN_POINT ( 'NONE',  ( 6.751597309925441159, 9.860318714012938912, -1.082531754730537088 ) ) ;
#130328 = CARTESIAN_POINT ( 'NONE',  ( 0.07479286986305369589, 0.004866263145587855152, -1.855573292446037970 ) ) ;
#130330 = CARTESIAN_POINT ( 'NONE',  ( -0.01167607004468995333, -5.765528217051257620, 11.00020965659534156 ) ) ;
#130331 = CARTESIAN_POINT ( 'NONE',  ( -4.841670253411603397, 5.781608396135871075, 1.082531754730549078 ) ) ;
#130332 = CARTESIAN_POINT ( 'NONE',  ( 0.1984543448181053105, 1.387095780679182377, -1.463931301963219855 ) ) ;
#130333 = CARTESIAN_POINT ( 'NONE',  ( 5.267185993530860699, 2.112242253262315739, -0.5839428218426812034 ) ) ;
#130334 = CARTESIAN_POINT ( 'NONE',  ( -1.001543065824772872E-14, 4.493750000682820378, 1.732050807568877637 ) ) ;
#130335 = CARTESIAN_POINT ( 'NONE',  ( 4.113462262696740979, 1.539102623358613586, 1.134910093507961237 ) ) ;
#130336 = CARTESIAN_POINT ( 'NONE',  ( -4.762992037102518950, 4.451245552908022596, -0.7998128361456221525 ) ) ;
#130337 = CARTESIAN_POINT ( 'NONE',  ( 5.287316719205157334, 9.112360572473935605, 1.040834085586084257E-14 ) ) ;
#130339 = CARTESIAN_POINT ( 'NONE',  ( 2.284780001213771783, 1.617805504991537635, -1.203372706716873575 ) ) ;
#130338 = CARTESIAN_POINT ( 'NONE',  ( -10.42585693878457853, 11.26584730477792284, -0.7216878364870267237 ) ) ;
#130340 = CARTESIAN_POINT ( 'NONE',  ( -0.6823417656250039265, 12.38020833367473017, -1.181850606188755259 ) ) ;
#130342 = CARTESIAN_POINT ( 'NONE',  ( -5.652823702255029836, 5.559658838911111900, -0.7998128361456362523 ) ) ;
#130341 = CARTESIAN_POINT ( 'NONE',  ( 0.3106431952284515741, 1.574884954006963600, -1.665989127006389126 ) ) ;
#130343 = CARTESIAN_POINT ( 'NONE',  ( 3.733171248123872132, -1.593707704047672591, 0.6599822260907485250 ) ) ;
#130344 = FACE_OUTER_BOUND ( 'NONE', #100884, .T. ) ;
#130345 = CARTESIAN_POINT ( 'NONE',  ( 4.196412238629597447, 4.854568018944682706, -1.199719254218452047 ) ) ;
#130346 = CARTESIAN_POINT ( 'NONE',  ( 1.499999999999990896, 3.806250000682819046, 1.214306433183764966E-14 ) ) ;
#130347 = CARTESIAN_POINT ( 'NONE',  ( 2.295757763869426871, 5.519548059767960702, 0.4031905389056070765 ) ) ;
#130348 = FILL_AREA_STYLE_COLOUR ( '', #203262 ) ;
#130349 = VERTEX_POINT ( 'NONE', #112857 ) ;
#130350 = CARTESIAN_POINT ( 'NONE',  ( 5.197853184559683370, 1.220981990389960581, 1.338314830865680261 ) ) ;
#130351 = VERTEX_POINT ( 'NONE', #178873 ) ;
#130352 = CARTESIAN_POINT ( 'NONE',  ( 6.378184920586140727, 6.405913593630768510, 0.000000000000000000 ) ) ;
#130353 = DIRECTION ( 'NONE',  ( 1.214306433183764966E-17, 1.000000000000000000, 5.200009205990155575E-32 ) ) ;
#130354 = CARTESIAN_POINT ( 'NONE',  ( 6.111934181110398434, -0.6035781192351510338, 1.708109960999981469 ) ) ;
#130355 = CARTESIAN_POINT ( 'NONE',  ( 6.875393295461478260, 8.154285278527437342, -1.082531754730548412 ) ) ;
#130356 = CYLINDRICAL_SURFACE ( 'NONE', #17603, 6.200000000000000178 ) ;
#130357 = CARTESIAN_POINT ( 'NONE',  ( 2.748186945943337012, 0.7392028471469233031, 2.063141171074922120 ) ) ;
#130358 = ORIENTED_EDGE ( 'NONE', *, *, #145267, .T. ) ;
#130359 = EDGE_CURVE ( 'NONE', #197229, #160913, #162615, .T. ) ;
#130360 = AXIS2_PLACEMENT_3D ( 'NONE', #183451, #1472, #117457 ) ;
#130362 = CARTESIAN_POINT ( 'NONE',  ( 8.860417081730671995, 10.29590700256267155, 1.199719254218453823 ) ) ;
#130361 = CARTESIAN_POINT ( 'NONE',  ( 5.846130809274892925, -0.8361890816445856078, 1.662715158673214066 ) ) ;
#130363 = CARTESIAN_POINT ( 'NONE',  ( 3.814002402653454027, 1.021707883093534885, -1.620180217528136568 ) ) ;
#130364 = CARTESIAN_POINT ( 'NONE',  ( 0.000000000000000000, 2.880000000000021210, 1.214306433183764966E-14 ) ) ;
#130365 = DIRECTION ( 'NONE',  ( 1.000000000000000000, 0.000000000000000000, -0.000000000000000000 ) ) ;
#130366 = CARTESIAN_POINT ( 'NONE',  ( 0.6823417656249882723, 0.4260416670080896528, -1.181850606188749264 ) ) ;
#130367 = CARTESIAN_POINT ( 'NONE',  ( 5.843201017809841247, 5.919415396974013532, 1.040834085586084257E-14 ) ) ;
#130368 = CARTESIAN_POINT ( 'NONE',  ( -8.459924665247381625, 11.85336729522185806, 1.082531754730560403 ) ) ;
#130369 = CARTESIAN_POINT ( 'NONE',  ( 1.604591590977550108, -0.7782141685120853580, -2.016947388195994062 ) ) ;
#130370 = CARTESIAN_POINT ( 'NONE',  ( -5.635349125135588721, 6.603604063193491136, 1.199719254218452935 ) ) ;
#130371 = EDGE_CURVE ( 'NONE', #80292, #126977, #101227, .T. ) ;
#130372 = CARTESIAN_POINT ( 'NONE',  ( 3.067887898442204442, 6.801229324816399746, 0.7998128361456271485 ) ) ;
#130373 = CARTESIAN_POINT ( 'NONE',  ( 2.397230751819504402, 1.409552409829779140, 1.160114028286141075 ) ) ;
#130374 = CARTESIAN_POINT ( 'NONE',  ( -4.776550190716183586, 4.467063398790632966, 1.214306433183764966E-14 ) ) ;
#130375 = CARTESIAN_POINT ( 'NONE',  ( 3.821172736587064023, -0.1348131347885111742, 1.820669774636254568 ) ) ;
#130376 = CARTESIAN_POINT ( 'NONE',  ( 9.413505227241941498, 12.55540351140892597, 8.860593473029982903 ) ) ;
#130377 = CARTESIAN_POINT ( 'NONE',  ( 2.601700882821424976, 1.355260107747566334, 1.349524769375435973 ) ) ;
#130378 = ORIENTED_EDGE ( 'NONE', *, *, #158993, .T. ) ;
#130379 = CARTESIAN_POINT ( 'NONE',  ( 4.053143702687862060, 1.665121224333296235, -1.051576502219366605 ) ) ;
#130380 = ORIENTED_EDGE ( 'NONE', *, *, #189291, .F. ) ;
#130381 = CARTESIAN_POINT ( 'NONE',  ( 4.845229750085990439, 0.6055439843271113176, -1.845326283916528753 ) ) ;
#130382 = ORIENTED_EDGE ( 'NONE', *, *, #17999, .T. ) ;
#130383 = CARTESIAN_POINT ( 'NONE',  ( -5.576146316970437944, 9.727530813099326323, 0.000000000000000000 ) ) ;
#130385 = CARTESIAN_POINT ( 'NONE',  ( 4.763993809689464065, 0.6627061821620899851, -2.014485251161435286 ) ) ;
#130384 = CARTESIAN_POINT ( 'NONE',  ( 5.342795052237045539, 8.390955439988655229, -1.199719254218450271 ) ) ;
#130386 = DIRECTION ( 'NONE',  ( 0.000000000000000000, -1.000000000000000000, 0.000000000000000000 ) ) ;
#130387 = CARTESIAN_POINT ( 'NONE',  ( 5.693912546396379781, 6.288398852508453096, -1.088204328156989087 ) ) ;
#130388 = CARTESIAN_POINT ( 'NONE',  ( -9.500587730663498931, -7.019129742887085577, 0.03636482241358145878 ) ) ;
#130389 = CARTESIAN_POINT ( 'NONE',  ( 3.366167277942881064, 7.149221934233827014, -0.7998128361456362523 ) ) ;
#130390 = CARTESIAN_POINT ( 'NONE',  ( 5.172599298813543633, 5.993452922492633839, -1.199719254218452047 ) ) ;
#130391 = CARTESIAN_POINT ( 'NONE',  ( 3.615888430654935259, -0.5820857220382947839, 1.927115488332105553 ) ) ;
#130392 = CARTESIAN_POINT ( 'NONE',  ( -11.92619526913699524, 11.02780024161488193, 1.328859060402684866 ) ) ;
#130393 = CARTESIAN_POINT ( 'NONE',  ( 5.285714101943871590, 1.228958891529348785, 1.350286652578087665 ) ) ;
#130394 = CARTESIAN_POINT ( 'NONE',  ( 0.6607010325807397555, -0.6960017893198193750, -1.950014918625786020 ) ) ;
#130395 = CARTESIAN_POINT ( 'NONE',  ( -8.568389894156720032, 10.05917163368005163, 1.082531754730558626 ) ) ;
#130396 = VECTOR ( 'NONE', #119959, 1000.000000000000000 ) ;
#130397 = CARTESIAN_POINT ( 'NONE',  ( -6.483603504774570148, 6.769331023298949646, -0.2299166613418425487 ) ) ;
#130398 = CARTESIAN_POINT ( 'NONE',  ( 0.9311234436981455920, -3.003119629485602182, 3.475000000000003197 ) ) ;
#130399 = CARTESIAN_POINT ( 'NONE',  ( 5.559403950928493821, 0.3636877230743483236, -1.834782481876767291 ) ) ;
#130400 = CARTESIAN_POINT ( 'NONE',  ( 7.623762449586013901, 7.788811034138823253, 1.040834085586084257E-14 ) ) ;
#130401 = EDGE_CURVE ( 'NONE', #132173, #78057, #175852, .T. ) ;
#130402 = CARTESIAN_POINT ( 'NONE',  ( -4.894657149733403045, 5.669187081899118574, -1.199719254218446718 ) ) ;
#130403 = B_SPLINE_CURVE_WITH_KNOTS ( 'NONE', 3,
 ( #55979, #118901, #188095, #39727, #105833, #117840, #183832, #35441, #101518, #167589 ),
 .UNSPECIFIED., .F., .F.,
 ( 4, 1, 1, 1, 1, 1, 1, 4 ),
 ( 0.000000000000000000, 0.09489293188423997272, 0.1878783894049059211, 0.2584743716234961797, 0.3617987437640678983, 0.5212292184658617877, 0.7337638816394396191, 1.000000000000000000 ),
 .UNSPECIFIED. ) ;
#130404 = AXIS2_PLACEMENT_3D ( 'NONE', #126518, #78735, #176261 ) ;
#130405 = CARTESIAN_POINT ( 'NONE',  ( -8.012344526598182026E-15, 10.10937500034140157, -1.575800808251669460 ) ) ;
#130406 = CARTESIAN_POINT ( 'NONE',  ( -4.076197739202962467, 7.907314462378773001, 1.040834085586084257E-14 ) ) ;
#130408 = CARTESIAN_POINT ( 'NONE',  ( -4.950135482320939140, 4.947781948895412008, -0.7216878364870338292 ) ) ;
#130407 = CARTESIAN_POINT ( 'NONE',  ( -11.89197816957260478, 11.29999999999999893, -0.8055420615339585755 ) ) ;
#130409 = CARTESIAN_POINT ( 'NONE',  ( -5.850506979496850057, 6.784345216623154151, -1.199719254218446718 ) ) ;
#130410 = CARTESIAN_POINT ( 'NONE',  ( 0.9013344411078340057, -1.777497804657724334, 1.061070337243313455 ) ) ;
#130411 = CARTESIAN_POINT ( 'NONE',  ( 1.968512934334982978, -2.077085554295199810, -0.4095441970272342136 ) ) ;
#130412 = CARTESIAN_POINT ( 'NONE',  ( 8.914649696185335870, 10.35917838609310593, -1.199719254218446718 ) ) ;
#130414 = EDGE_CURVE ( 'NONE', #145598, #176704, #78147, .T. ) ;
#130413 = DIRECTION ( 'NONE',  ( -5.578564026256490882E-16, -1.000000000000000000, -9.066213480720158442E-32 ) ) ;
#130415 = CARTESIAN_POINT ( 'NONE',  ( 0.3913703952206915027, -1.802969083500185477, 0.7928767443170018359 ) ) ;
#130416 = CARTESIAN_POINT ( 'NONE',  ( 4.326045746746942200, 7.429495238844160632, 1.107669923005821344 ) ) ;
#130417 = CARTESIAN_POINT ( 'NONE',  ( 3.850152436600926542, 7.435668909435648288, -0.7216878364870197293 ) ) ;
#130419 = DIRECTION ( 'NONE',  ( 1.014813233446432150E-15, 1.000000000000000000, -4.583713267641621330E-32 ) ) ;
#130418 = CARTESIAN_POINT ( 'NONE',  ( -3.475000000000000533, -2.800000000000000266, 0.000000000000000000 ) ) ;
#130420 = CARTESIAN_POINT ( 'NONE',  ( 2.801036929584544311, 1.937030572335847856, 1.225446795713614589 ) ) ;
#130421 = CARTESIAN_POINT ( 'NONE',  ( 0.6799654140086827114, -1.016662149479659494, 1.516215539243186639 ) ) ;
#130422 = CARTESIAN_POINT ( 'NONE',  ( 2.672007700615218528, 1.902801012812182169, -0.1915479950082218386 ) ) ;
#130423 = CIRCLE ( 'NONE', #137314, 0.08000000000000020983 ) ;
#130424 = ADVANCED_FACE ( 'NONE', ( #61 ), #8300, .T. ) ;
#130425 = EDGE_LOOP ( 'NONE', ( #7489, #124591, #193539, #122128, #46868, #152378 ) ) ;
#130426 = CARTESIAN_POINT ( 'NONE',  ( 8.256552360598020002, 8.734991963560254646, -0.7216878364870267237 ) ) ;
#130427 = CARTESIAN_POINT ( 'NONE',  ( 1.740491373288379995, 1.155656410672186496, -1.648304894270665510 ) ) ;
#130428 = CARTESIAN_POINT ( 'NONE',  ( 1.516376426791886445, 0.7900930292849810410, 1.795789229542772647 ) ) ;
#130429 = CARTESIAN_POINT ( 'NONE',  ( -9.484092147959342967, 11.02352791316275216, 1.199719254218462483 ) ) ;
#130430 = CARTESIAN_POINT ( 'NONE',  ( -7.877450944739929461, 9.149113176073413456, 1.199719254218462483 ) ) ;
#130431 = CARTESIAN_POINT ( 'NONE',  ( -11.52460864928265138, 9.719999999999998863, -3.346683403123526190 ) ) ;
#130433 = CARTESIAN_POINT ( 'NONE',  ( 2.482954129442132452, 1.619277697627572676, -0.7147633530761726695 ) ) ;
#130432 = CARTESIAN_POINT ( 'NONE',  ( 4.400388060213418662, 1.616114658936588011, -1.326231919226998901 ) ) ;
#130434 = CARTESIAN_POINT ( 'NONE',  ( 1.499999999999996891, 12.14583333333333748, -0.8660254037844378194 ) ) ;
#130435 = CARTESIAN_POINT ( 'NONE',  ( 5.332074485713341971, 2.257618135992002895, 0.3962004586785839444 ) ) ;
#130436 = CARTESIAN_POINT ( 'NONE',  ( 4.382551862494687533, 1.553031517084975555, -0.7855321229453329224 ) ) ;
#130437 = CARTESIAN_POINT ( 'NONE',  ( 9.511208455186636712, 11.05516360492796935, 1.199719254218453823 ) ) ;
#130438 = CARTESIAN_POINT ( 'NONE',  ( -7.863746947443979174, -5.507058666270983949, 7.245729715095587053 ) ) ;
#130439 = CARTESIAN_POINT ( 'NONE',  ( 4.393670956608656475, 0.08463240572039069931, 1.731882585348672343 ) ) ;
#130440 = CARTESIAN_POINT ( 'NONE',  ( 4.404835846824251888, 0.5749587956990888094, 2.093619418667266530 ) ) ;
#130441 = CARTESIAN_POINT ( 'NONE',  ( 3.225950485047770933, 5.851027101609320269, 1.199719254218450271 ) ) ;
#130442 = CARTESIAN_POINT ( 'NONE',  ( 5.296111364736042937, -0.9110065213352031011, -1.799124599017036585 ) ) ;
#130443 = CARTESIAN_POINT ( 'NONE',  ( 0.5312500000000220934, -0.7852924748305555314, -1.895863743164076576 ) ) ;
#130444 = CARTESIAN_POINT ( 'NONE',  ( -4.199533704925234368, 7.510932310329544670, -0.9222493318717175370 ) ) ;
#130445 = CARTESIAN_POINT ( 'NONE',  ( 3.346621647027960833, 0.4665833272349695360, 1.868923817322089453 ) ) ;
#130446 = CARTESIAN_POINT ( 'NONE',  ( 1.499999999999993117, 10.13541666734946745, 0.8660254037844409281 ) ) ;
#130447 = CARTESIAN_POINT ( 'NONE',  ( 6.135052730014136202, 2.072377209612641824, 0.8004311911904669063 ) ) ;
#130448 = VERTEX_POINT ( 'NONE', #212396 ) ;
#130449 = CARTESIAN_POINT ( 'NONE',  ( 6.883263157960370471, 7.053006342242538196, 2.444342378444531949 ) ) ;
#130450 = CARTESIAN_POINT ( 'NONE',  ( 0.7499999999999902300, 2.983333333333351600, 1.299038105676669330 ) ) ;
#130451 = CARTESIAN_POINT ( 'NONE',  ( 6.474182045725470402, 7.511966127223233869, -1.199719254218446718 ) ) ;
#130452 = CARTESIAN_POINT ( 'NONE',  ( 1.735333443468607184, 2.074102030253548445, 0.7956244722606919950 ) ) ;
#130453 = CARTESIAN_POINT ( 'NONE',  ( 1.499999999999970912, 4.795833333333354709, -0.8660254037844417052 ) ) ;
#130454 = CARTESIAN_POINT ( 'NONE',  ( 6.317736394288122170, 10.31451686007074997, 0.7216878364870438212 ) ) ;
#130455 = CARTESIAN_POINT ( 'NONE',  ( 0.07118442604959854259, 7.078193277237673442, 2.121339347286374633 ) ) ;
#130456 = CARTESIAN_POINT ( 'NONE',  ( 3.902768115887398803, 5.646591783325653147, -1.599625672291269396 ) ) ;
#130457 = CARTESIAN_POINT ( 'NONE',  ( -4.719646871332968452, 5.639247783710797712, 1.082531754730549078 ) ) ;
#130459 = CARTESIAN_POINT ( 'NONE',  ( 4.352046829380719295, -0.7922827022245787498, 1.904640004429495326 ) ) ;
#130458 = CARTESIAN_POINT ( 'NONE',  ( 9.297140650669039275, 11.86975006391249643, 1.599625672291281386 ) ) ;
#130460 = CARTESIAN_POINT ( 'NONE',  ( -4.711622075948912247, 5.455646162483875017, -1.199719254218446718 ) ) ;
#130461 = CARTESIAN_POINT ( 'NONE',  ( -0.7500000000000215383, 4.722916667349482012, 1.299038105676671107 ) ) ;
#130462 = CARTESIAN_POINT ( 'NONE',  ( -1.364683531250014514, -0.2614583329919080157, -0.7879004041258359514 ) ) ;
#130463 = CARTESIAN_POINT ( 'NONE',  ( 6.520764494017629254, 1.745421825204738431, 0.6730592012400560264 ) ) ;
#130464 = CARTESIAN_POINT ( 'NONE',  ( 6.082590270738484683, -0.5753628732939282120, 1.636087478734444600 ) ) ;
#130465 = CARTESIAN_POINT ( 'NONE',  ( 4.792390001771311248, 1.443284891743993770, -0.9723301709525405956 ) ) ;
#130466 = CARTESIAN_POINT ( 'NONE',  ( 4.708759422647839976, 4.387974169377582001, -0.7998128361456211532 ) ) ;
#130467 = CARTESIAN_POINT ( 'NONE',  ( 3.087719631786550956, -0.9270648334414759439, 2.096714421332421807 ) ) ;
#130468 = CARTESIAN_POINT ( 'NONE',  ( 0.6823417656249917140, 5.405208333674749177, 1.181850606188765695 ) ) ;
#130469 = CARTESIAN_POINT ( 'NONE',  ( 1.288719586054212884, 1.393062650230517674, 1.203921758438614376 ) ) ;
#130470 = DIRECTION ( 'NONE',  ( 5.578564026256491869E-16, 1.000000000000000000, 9.066213480720160632E-32 ) ) ;
#130471 = CARTESIAN_POINT ( 'NONE',  ( 2.045663570152244315, 0.7015605659913305425, -1.685594894050304493 ) ) ;
#130472 = CARTESIAN_POINT ( 'NONE',  ( 3.217422812353257555, 1.967887761762876941, 0.4390297752325384995 ) ) ;
#130473 = CARTESIAN_POINT ( 'NONE',  ( 0.9553299046189435151, 0.4242123182428610972, -2.149831459026855907 ) ) ;
#130474 = CARTESIAN_POINT ( 'NONE',  ( 7.845839667831243425, 15.84947785439367074, -8.676411862874921610 ) ) ;
#130475 = CARTESIAN_POINT ( 'NONE',  ( 4.542079205076994697, 0.9026690382304535243, -1.902845716346044158 ) ) ;
#130476 = CARTESIAN_POINT ( 'NONE',  ( -6.581593504430098385, 9.765943957555402122, -1.199719254218440723 ) ) ;
#130477 = CARTESIAN_POINT ( 'NONE',  ( 8.399612633245173043, 14.34265028463549108, 8.120044275143325052 ) ) ;
#130478 =( BOUNDED_CURVE ( )  B_SPLINE_CURVE ( 2, ( #154896, #6478, #123550, #21643, #137588 ),
 .UNSPECIFIED., .F., .T. ) 
 B_SPLINE_CURVE_WITH_KNOTS ( ( 3, 2, 3 ),
 ( 0.1116300932268863011, 0.1125000000000000028, 0.1135379806157290478 ),
 .UNSPECIFIED. ) 
 CURVE ( )  GEOMETRIC_REPRESENTATION_ITEM ( )  RATIONAL_B_SPLINE_CURVE ( ( 0.9557375992086956096, 0.9720291019184583714, 1.000000000000000000, 0.9666248718707491916, 0.9498782570434034511 ) ) 
 REPRESENTATION_ITEM ( '' )  );
#130479 = CARTESIAN_POINT ( 'NONE',  ( 1.891162872569674080, 0.2007839719405465906, 2.060584128686280714 ) ) ;
#130480 = CARTESIAN_POINT ( 'NONE',  ( 5.518332215962025167, 6.396807992499198292, -1.199719254218445830 ) ) ;
#130481 = CARTESIAN_POINT ( 'NONE',  ( -1.360316468750034868, 2.619791667008062319, -0.7853790794159261068 ) ) ;
#130482 = CARTESIAN_POINT ( 'NONE',  ( 3.158948766716848766, 0.5171890032967979556, 2.056314737185329644 ) ) ;
#130484 = AXIS2_PLACEMENT_3D ( 'NONE', #19013, #118723, #169546 ) ;
#130483 = CONTEXT_DEPENDENT_SHAPE_REPRESENTATION ( #54788, #190596 ) ;
#130485 = CARTESIAN_POINT ( 'NONE',  ( 0.6823417656249882723, 0.09270833367475139752, 1.181850606188755259 ) ) ;
#130486 = CARTESIAN_POINT ( 'NONE',  ( 0.1352084326644766299, -1.761967750658991028, 0.7794309377431463126 ) ) ;
#130487 = VERTEX_POINT ( 'NONE', #95507 ) ;
#130488 = CARTESIAN_POINT ( 'NONE',  ( -5.010620288702242853, 8.003418215864698482, -1.199719254218453823 ) ) ;
#130489 = ADVANCED_FACE ( 'NONE', ( #176725 ), #184150, .T. ) ;
#130490 = CARTESIAN_POINT ( 'NONE',  ( 10.57266086055835075, 11.22919251360659310, 0.000000000000000000 ) ) ;
#130491 = CARTESIAN_POINT ( 'NONE',  ( 5.926322542504858681, 8.007405281046052536, -1.443375672974078761 ) ) ;
#130492 = CARTESIAN_POINT ( 'NONE',  ( -3.474999999999998312, -3.077083332377416713, 2.006292185433951047 ) ) ;
#130493 = CARTESIAN_POINT ( 'NONE',  ( -5.880485940025243607, 7.883652901494672349, 1.599625672291269396 ) ) ;
#130494 = CARTESIAN_POINT ( 'NONE',  ( 3.779560859189102562, 0.2429267963163626032, -2.005027992008329818 ) ) ;
#130495 = CARTESIAN_POINT ( 'NONE',  ( 1.501149451381103672, 1.721883814275385616, -1.212229816669802895 ) ) ;
#130496 = CARTESIAN_POINT ( 'NONE',  ( -6.967964602780620353, 7.093989889524320525, 0.000000000000000000 ) ) ;
#130497 = CARTESIAN_POINT ( 'NONE',  ( 8.809047120577066181, 11.30030761213851953, 1.599625672291281386 ) ) ;
#130498 = CARTESIAN_POINT ( 'NONE',  ( 5.524199568661091853, 0.9153802634506421620, 1.620121770064205213 ) ) ;
#130499 = CARTESIAN_POINT ( 'NONE',  ( 7.456094412511537151, 10.78619501698377370, 1.199719254218460707 ) ) ;
#130500 = CARTESIAN_POINT ( 'NONE',  ( -0.5997958527293503206, 4.283086937630856461, -0.2585301179639542535 ) ) ;
#130501 = CARTESIAN_POINT ( 'NONE',  ( -8.026063749610043985, 12.30756544127966912, -0.7216878364870267237 ) ) ;
#130502 = CARTESIAN_POINT ( 'NONE',  ( -6.669721502918952716, 9.868759955792373972, 1.199719254218452047 ) ) ;
#130503 = CARTESIAN_POINT ( 'NONE',  ( 0.4093245661422850734, 1.881582470445356314, 1.064130679222355491 ) ) ;
#130505 = CARTESIAN_POINT ( 'NONE',  ( -4.027792083363366693, 7.778134382787397882, 0.5015608049221946807 ) ) ;
#130504 = CARTESIAN_POINT ( 'NONE',  ( -4.936050443827081580, 7.916420063510339666, 1.199719254218452935 ) ) ;
#130506 = CARTESIAN_POINT ( 'NONE',  ( 0.6823417656249882723, 0.3427083336747516196, 1.181850606188755259 ) ) ;
#130507 = CARTESIAN_POINT ( 'NONE',  ( 2.864235035935404738, -0.5475380835847867278, 1.645162456946830831 ) ) ;
#130508 = CARTESIAN_POINT ( 'NONE',  ( 1.095196197045473774, -1.740516465796032586, -0.003461242977918776564 ) ) ;
#130510 = CARTESIAN_POINT ( 'NONE',  ( 7.795575138177731844, 8.197185204069915798, 1.040834085586084257E-14 ) ) ;
#130509 = CARTESIAN_POINT ( 'NONE',  ( 6.410760325301650298, 1.714854236211732941, -1.544436965994408828 ) ) ;
#130511 = CARTESIAN_POINT ( 'NONE',  ( -11.79409034920973021, 4.782243044590097192, -4.941202808084400822 ) ) ;
#130512 = CARTESIAN_POINT ( 'NONE',  ( 2.530605077378933920, 1.998055600607269833, 0.5039824654343558752 ) ) ;
#130513 = CARTESIAN_POINT ( 'NONE',  ( 1.194685229111978497, -1.276845315561925931, -1.560263297373874813 ) ) ;
#130514 = CARTESIAN_POINT ( 'NONE',  ( 6.925078400183521055, 0.5534609092465185842, 2.295239920751692253 ) ) ;
#130515 = CARTESIAN_POINT ( 'NONE',  ( -6.445975688654487001, 6.485002823043819475, -0.7998128361456362523 ) ) ;
#130516 = CARTESIAN_POINT ( 'NONE',  ( 0.6726557866889815163, -1.855577277548149828, -0.6663020492489196700 ) ) ;
#130518 = CARTESIAN_POINT ( 'NONE',  ( -6.129694847154220305, 8.244672969803623630, -1.443375672974066548 ) ) ;
#130517 = CARTESIAN_POINT ( 'NONE',  ( 4.517770118113122457, -0.5046507728132009207, 1.844564425022446885 ) ) ;
#130519 = CARTESIAN_POINT ( 'NONE',  ( -7.553300976144794454, 7.984808358356614733, -0.7216878364870338292 ) ) ;
#130520 = CARTESIAN_POINT ( 'NONE',  ( 5.528692779322568640, 9.672168352510192690, 0.7998128361456341429 ) ) ;
#130521 = CARTESIAN_POINT ( 'NONE',  ( -7.282664789195997912, 8.525472337930658284, 1.199719254218452047 ) ) ;
#130522 = CARTESIAN_POINT ( 'NONE',  ( 0.1705770660650838266, 0.7750864355984161680, 1.865232097879976125 ) ) ;
#130523 = CARTESIAN_POINT ( 'NONE',  ( 4.858593139428769803, 0.8780750695473713563, 2.134189430172124702 ) ) ;
#130524 = CARTESIAN_POINT ( 'NONE',  ( 5.916451087343006954, 0.7937011933104149985, 1.794315766958521241 ) ) ;
#130525 = CARTESIAN_POINT ( 'NONE',  ( 1.533958681542445301, 1.164210590399002321, 1.578835587694705334 ) ) ;
#130526 = CARTESIAN_POINT ( 'NONE',  ( -4.911894908834722351, 4.738238661368090021, 0.4458799699701230246 ) ) ;
#130527 = CARTESIAN_POINT ( 'NONE',  ( -9.372067988369742864, 14.58092609327329292, 7.405912380423360197 ) ) ;
#130528 = ORIENTED_EDGE ( 'NONE', *, *, #158732, .T. ) ;
#130529 = CARTESIAN_POINT ( 'NONE',  ( 0.1459223332197969736, 2.093306735845179567, -0.3175718533311999714 ) ) ;
#130531 = CARTESIAN_POINT ( 'NONE',  ( -6.333630315878337136, 10.54098580183340772, 0.000000000000000000 ) ) ;
#130530 = CARTESIAN_POINT ( 'NONE',  ( -4.089755892816631544, 7.923132308261379819, -0.7998128361456281477 ) ) ;
#130532 = CARTESIAN_POINT ( 'NONE',  ( 1.112948326906910035, -1.796673262952220629, 0.4014371099074555693 ) ) ;
#130533 = ORIENTED_EDGE ( 'NONE', *, *, #135864, .T. ) ;
#130534 = CARTESIAN_POINT ( 'NONE',  ( 4.206061555090504278, 0.7368182104705008895, -2.042320221205825792 ) ) ;
#130535 = CARTESIAN_POINT ( 'NONE',  ( 11.22634050851384657, 8.811580666534183592, -4.110909495814070169 ) ) ;
#130536 = CARTESIAN_POINT ( 'NONE',  ( 2.355864820516640812, -1.574449018071517825, -1.420800595792824028 ) ) ;
#130537 = CARTESIAN_POINT ( 'NONE',  ( -0.7500000000000215383, 3.472916667349487785, 1.299038105676671107 ) ) ;
#130538 = CARTESIAN_POINT ( 'NONE',  ( 7.228468454380276853, 11.58496363008569574, 1.040834085586084257E-14 ) ) ;
#130539 = CARTESIAN_POINT ( 'NONE',  ( -1.845715822548411822, 2.495237285644507086, -2.490652812252487358 ) ) ;
#130540 = CARTESIAN_POINT ( 'NONE',  ( 3.620434630758031069, 1.310268768930487937, -1.590567769477232662 ) ) ;
#130542 = CARTESIAN_POINT ( 'NONE',  ( 0.3449248370967008537, 0.5783895242766275979, -1.748133987124582012 ) ) ;
#130541 = CARTESIAN_POINT ( 'NONE',  ( -7.655550293210764856, 12.08322577538792331, 0.000000000000000000 ) ) ;
#130543 = CARTESIAN_POINT ( 'NONE',  ( 0.6823417656249882723, 2.926041667008084879, -1.181850606188754593 ) ) ;
#130544 = CARTESIAN_POINT ( 'NONE',  ( -0.02264175331117417728, 0.7142767504201595896, -2.172799776233569791 ) ) ;
#130545 = CARTESIAN_POINT ( 'NONE',  ( 1.300073763039447883, 4.107155158418582808, -0.4337670944212108082 ) ) ;
#130546 = AXIS2_PLACEMENT_3D ( 'NONE', #47864, #98719, #183157 ) ;
#130547 = CARTESIAN_POINT ( 'NONE',  ( 11.84668730067608244, 10.09363775091781079, -1.400000000000002132 ) ) ;
#130548 = CARTESIAN_POINT ( 'NONE',  ( 1.441102657128832121, 0.4411821743415585417, 2.218815533503415871 ) ) ;
#130549 = CARTESIAN_POINT ( 'NONE',  ( -10.30383355670593737, 11.12348669235284504, -0.7216878364870267237 ) ) ;
#130550 = CARTESIAN_POINT ( 'NONE',  ( 1.388595261843462714, -1.720809334905664567, -0.5665428721913360333 ) ) ;
#130551 = CARTESIAN_POINT ( 'NONE',  ( 1.586979130512996772, 1.594871783843774260, 1.060967117046989427 ) ) ;
#130552 = CARTESIAN_POINT ( 'NONE',  ( 2.945825538390862697, 1.462269270728074222, 1.465923284304726737 ) ) ;
#130553 = CARTESIAN_POINT ( 'NONE',  ( -1.364683531250014514, 1.801041667008085767, -0.7879004041258289570 ) ) ;
#130554 = AXIS2_PLACEMENT_3D ( 'NONE', #72342, #124407, #121203 ) ;
#130555 = CARTESIAN_POINT ( 'NONE',  ( 1.358210660854881402, 0.7971155783631430625, 1.803302576489584697 ) ) ;
#130556 = CARTESIAN_POINT ( 'NONE',  ( 5.268162717194916134, 0.9514403766726580169, 1.675093392909310142 ) ) ;
#130557 = EDGE_CURVE ( 'NONE', #29173, #121012, #7841, .T. ) ;
#130559 = CARTESIAN_POINT ( 'NONE',  ( 6.206332990038123221, 6.936436922908462144, -0.8583981852504622978 ) ) ;
#130558 = CARTESIAN_POINT ( 'NONE',  ( 0.7687468715882056491, 1.142267183891092053, 2.005099294460314319 ) ) ;
#130560 = CARTESIAN_POINT ( 'NONE',  ( -1.402160292154681736E-14, 2.446875000341416584, -1.575800808251660134 ) ) ;
#130561 = CARTESIAN_POINT ( 'NONE',  ( 5.793442459296725744, -1.866233137118753715, 0.8787832743982221251 ) ) ;
#130562 = CARTESIAN_POINT ( 'NONE',  ( -6.084912014434944894, 5.993485526462540847, -0.7998128361456291469 ) ) ;
#130563 = CARTESIAN_POINT ( 'NONE',  ( 7.721532178182734185, 8.967207948423393304, 1.199719254218462483 ) ) ;
#130564 = CARTESIAN_POINT ( 'NONE',  ( -1.400320522945621482, 3.349376740025014954, -0.06109695461879691841 ) ) ;
#130565 = CARTESIAN_POINT ( 'NONE',  ( 6.247117736759643769, -1.781108002423707592, 1.123397916191863244 ) ) ;
#130566 = CARTESIAN_POINT ( 'NONE',  ( -1.201851678989727383E-14, 3.384375000341421469, 1.575800808251672791 ) ) ;
#130567 = CARTESIAN_POINT ( 'NONE',  ( 6.432923066502826082, 0.2047513753351773713, 2.151863363619124225 ) ) ;
#130568 = CARTESIAN_POINT ( 'NONE',  ( 0.3625324912872701089, 0.1813134127766780901, -1.832273687604975665 ) ) ;
#130569 = CARTESIAN_POINT ( 'NONE',  ( 5.373696804382912973, 0.3918686645382524203, -1.981109099827490949 ) ) ;
#130570 = DIRECTION ( 'NONE',  ( -0.000000000000000000, -1.000000000000000000, -0.000000000000000000 ) ) ;
#130571 = CIRCLE ( 'NONE', #213486, 0.05000000000000012768 ) ;
#130572 = CARTESIAN_POINT ( 'NONE',  ( -6.073689629242176480, 6.188318776978391611, -0.7216878364870278340 ) ) ;
#130575 = CARTESIAN_POINT ( 'NONE',  ( 4.148431816101584957, 6.823292304551739740, -1.082531754730548412 ) ) ;
#130574 = CARTESIAN_POINT ( 'NONE',  ( 3.285556943750000070, -2.034374999522043481, 0.000000000000000000 ) ) ;
#130573 = CARTESIAN_POINT ( 'NONE',  ( -5.580797839525510007, 14.55306906467030181, -10.58276376127103013 ) ) ;
#130576 = CARTESIAN_POINT ( 'NONE',  ( -4.522526758610270647, 7.433975764090723359, -1.199719254218453823 ) ) ;
#130577 = CARTESIAN_POINT ( 'NONE',  ( 3.309780021317248355, -1.205041885261768808, -1.616693488061982098 ) ) ;
#130578 = CARTESIAN_POINT ( 'NONE',  ( -7.283754839039664475, 9.520799950344851936, -1.599625672291263179 ) ) ;
#130580 = CARTESIAN_POINT ( 'NONE',  ( -8.054952659850432184, 8.570068656013202002, 0.000000000000000000 ) ) ;
#130579 = CARTESIAN_POINT ( 'NONE',  ( -4.613852347352193739, 4.277249248199312071, 1.214306433183764966E-14 ) ) ;
#130581 = CARTESIAN_POINT ( 'NONE',  ( -1.364683531250010295, 5.238541667008086655, -0.7879004041258300672 ) ) ;
#130583 = CARTESIAN_POINT ( 'NONE',  ( -1.364683531250010740, 9.880208333674728394, 0.7879004041258445001 ) ) ;
#130582 = CARTESIAN_POINT ( 'NONE',  ( 5.014612968065254250, 1.493337269798940881, -1.563205770552501761 ) ) ;
#130584 = CARTESIAN_POINT ( 'NONE',  ( -11.86145016429273191, 10.90000000000000036, 1.099999999999996758 ) ) ;
#130585 = CARTESIAN_POINT ( 'NONE',  ( -11.82588180490283492, 7.634079919984739782, -2.050956402321635785 ) ) ;
#130587 = CARTESIAN_POINT ( 'NONE',  ( 5.941029844038744123, -1.730876725876070221, -1.034150010194856417 ) ) ;
#130586 = CARTESIAN_POINT ( 'NONE',  ( -5.816084710138169633, 8.768887347594400694, 1.082531754730548412 ) ) ;
#130588 = CARTESIAN_POINT ( 'NONE',  ( -1.402160292154681736E-14, -1.115624999658584082, 1.575800808251672791 ) ) ;
#130589 = EDGE_CURVE ( 'NONE', #48908, #209385, #18350, .T. ) ;
#130590 = CARTESIAN_POINT ( 'NONE',  ( 1.576317393346495344, -1.636983117988626946, -0.5438251031371076349 ) ) ;
#130591 = CARTESIAN_POINT ( 'NONE',  ( 6.059568310664962709, 6.034194215389424798, 0.7998128361456352531 ) ) ;
#130593 = CARTESIAN_POINT ( 'NONE',  ( 5.668190738965027897, 8.770583741171307679, -1.199719254218452047 ) ) ;
#130592 = CARTESIAN_POINT ( 'NONE',  ( 6.155038550924139429, 9.164333495178082600, 1.082531754730558626 ) ) ;
#130594 = CARTESIAN_POINT ( 'NONE',  ( -10.83006501599620641, 6.402595425522297212, -5.185414522284083283 ) ) ;
#130595 = CARTESIAN_POINT ( 'NONE',  ( 6.573518820989787237, 1.789947451694915204, -0.5432430119688207437 ) ) ;
#130596 = CARTESIAN_POINT ( 'NONE',  ( 1.207682405589046937, 1.525905122249699319, 1.313188400431253955 ) ) ;
#130597 = DIRECTION ( 'NONE',  ( 0.000000000000000000, 1.000000000000000000, 0.000000000000000000 ) ) ;
#130598 = CARTESIAN_POINT ( 'NONE',  ( 3.311752114541001379, -0.4323003076652854881, 2.163846791405985570 ) ) ;
#130599 = CARTESIAN_POINT ( 'NONE',  ( 4.961888193860729324, -0.5853885669280403103, 2.090577497978749477 ) ) ;
#130600 = ORIENTED_EDGE ( 'NONE', *, *, #26315, .T. ) ;
#130601 = CARTESIAN_POINT ( 'NONE',  ( 9.544576953896278582, 10.23768732240824164, 0.000000000000000000 ) ) ;
#130603 = CARTESIAN_POINT ( 'NONE',  ( 1.528922965942226986, -1.701935853630029083, 1.081086586856384590 ) ) ;
#130602 = CARTESIAN_POINT ( 'NONE',  ( 2.578903501431661915, -1.460476376761214556, 1.537597662120089081 ) ) ;
#130605 = ORIENTED_EDGE ( 'NONE', *, *, #124072, .T. ) ;
#130604 = CARTESIAN_POINT ( 'NONE',  ( 1.722643027415799999, 1.340613184126436597, -1.218586174478804907 ) ) ;
#130606 = EDGE_CURVE ( 'NONE', #73830, #195274, #163567, .T. ) ;
#130607 = CARTESIAN_POINT ( 'NONE',  ( 7.049313524462606395, 7.188896964819984525, 0.000000000000000000 ) ) ;
#130608 = CARTESIAN_POINT ( 'NONE',  ( 5.774883364416965037, 8.824782127540085952, -1.199719254218440723 ) ) ;
#130610 = CARTESIAN_POINT ( 'NONE',  ( 1.710024596074321002, 1.099767263899156244, -1.568400350156524459 ) ) ;
#130609 = CARTESIAN_POINT ( 'NONE',  ( -3.093231602212184850, 6.760520635889515795, -0.7998128361456281477 ) ) ;
#130611 = LINE ( 'NONE', #195541, #41921 ) ;
#130612 = CARTESIAN_POINT ( 'NONE',  ( 6.114364089638795186, 7.196141528409145671, 1.082531754730558626 ) ) ;
#130613 = CARTESIAN_POINT ( 'NONE',  ( 1.364683531249986537, 0.4677083336747514530, -0.7879004041258309554 ) ) ;
#130614 = DIRECTION ( 'NONE',  ( 0.000000000000000000, 0.000000000000000000, 1.000000000000000000 ) ) ;
#130615 = CARTESIAN_POINT ( 'NONE',  ( -7.811469059767924605, 12.26513100303794168, -0.7998128361456281477 ) ) ;
#130616 = CARTESIAN_POINT ( 'NONE',  ( 5.049776242366147194, 0.6816224847111511664, -2.051488706027407183 ) ) ;
#130617 = CARTESIAN_POINT ( 'NONE',  ( -4.828112100242279325, 8.646898193675708555, -0.7216878364870338292 ) ) ;
#130618 = EDGE_CURVE ( 'NONE', #78199, #17720, #200403, .T. ) ;
#130619 = CARTESIAN_POINT ( 'NONE',  ( 6.387299765813869712, 6.624473612970537495, 0.000000000000000000 ) ) ;
#130620 = CARTESIAN_POINT ( 'NONE',  ( 1.881254504445781794, -1.940830296247602949, -0.8548571619346672090 ) ) ;
#130621 = CARTESIAN_POINT ( 'NONE',  ( -0.1296875068447882473, 5.724785194352729256, -2.420566058096422779 ) ) ;
#130622 = CARTESIAN_POINT ( 'NONE',  ( 3.303940151695891281, -1.969246965329603638, 0.09337747576219912471 ) ) ;
#130623 = CARTESIAN_POINT ( 'NONE',  ( 5.168181644781757456, 1.909928461159452251, -0.09994665148223277895 ) ) ;
#130624 = ORIENTED_EDGE ( 'NONE', *, *, #69865, .T. ) ;
#130625 = AXIS2_PLACEMENT_3D ( 'NONE', #97377, #110480, #15014 ) ;
#130626 = CARTESIAN_POINT ( 'NONE',  ( 0.3794556558127279988, -0.1030994254981997954, 2.067933115924729837 ) ) ;
#130627 = CARTESIAN_POINT ( 'NONE',  ( 1.833828351339358287, 1.920785844388651409, 0.2851290042146270576 ) ) ;
#130628 = VERTEX_POINT ( 'NONE', #134401 ) ;
#130629 = DIRECTION ( 'NONE',  ( 0.000000000000000000, 1.000000000000000000, 0.000000000000000000 ) ) ;
#130631 = CARTESIAN_POINT ( 'NONE',  ( 7.014364370223726830, 9.276787413384745662, -1.599625672291269396 ) ) ;
#130630 = CARTESIAN_POINT ( 'NONE',  ( -7.444835747679825033, 7.858265591814152629, 0.000000000000000000 ) ) ;
#130633 = CARTESIAN_POINT ( 'NONE',  ( 7.630541526392844887, 7.796719957080126662, 0.7998128361456341429 ) ) ;
#130632 = CARTESIAN_POINT ( 'NONE',  ( 2.501997717985538383, -0.8009308590465279432, -1.931334861377894008 ) ) ;
#130634 = CARTESIAN_POINT ( 'NONE',  ( 4.204437033569277560, 7.919277282557212416, 0.000000000000000000 ) ) ;
#130636 = ORIENTED_EDGE ( 'NONE', *, *, #131120, .F. ) ;
#130635 = CARTESIAN_POINT ( 'NONE',  ( 5.901015568784107934, -0.2851453878830525479, -1.890788771128081969 ) ) ;
#130637 = CARTESIAN_POINT ( 'NONE',  ( 4.266400587755204477, 1.039063272370500668, 1.946970035688735612 ) ) ;
#130638 = CARTESIAN_POINT ( 'NONE',  ( 2.046200460737709559, 0.8445575735530999051, -2.038961412367201298 ) ) ;
#130639 = DIRECTION ( 'NONE',  ( 0.7592566023653005702, 0.6507913734559639396, 0.000000000000000000 ) ) ;
#130640 = CARTESIAN_POINT ( 'NONE',  ( 1.770022778749248182, 1.907080152163560971, -0.1419829583147319274 ) ) ;
#130641 = CARTESIAN_POINT ( 'NONE',  ( 0.4356160240586413046, -9.063431457505064515, -9.626717610576614348 ) ) ;
#130642 = CARTESIAN_POINT ( 'NONE',  ( 10.39640486358069360, 11.02356051713265650, 0.7998128361456462443 ) ) ;
#130644 = CARTESIAN_POINT ( 'NONE',  ( 3.982925052038261526, 1.964963782255540359, 0.6523228965355857278 ) ) ;
#130643 = B_SPLINE_CURVE_WITH_KNOTS ( 'NONE', 3,
 ( #139674, #25880, #191574, #140755, #187323, #171072 ),
 .UNSPECIFIED., .F., .F.,
 ( 4, 2, 4 ),
 ( 0.0006258038130483376113, 0.0009388807108837884767, 0.001251957608719239451 ),
 .UNSPECIFIED. ) ;
#130646 = CARTESIAN_POINT ( 'NONE',  ( 2.149508875876861236, -1.735919364271593768, -1.288018159417112729 ) ) ;
#130645 = CARTESIAN_POINT ( 'NONE',  ( -2.656508033273816238, 5.186677574539687363, -1.199719254218446718 ) ) ;
#130647 = CARTESIAN_POINT ( 'NONE',  ( 4.054362073078698891, -1.623213109359676443, 1.472610181411204922 ) ) ;
#130648 = DIRECTION ( 'NONE',  ( -5.578564026256490882E-16, -1.000000000000000000, -9.066213480720158442E-32 ) ) ;
#130649 =( NAMED_UNIT ( * ) SI_UNIT ( $, .STERADIAN. ) SOLID_ANGLE_UNIT ( ) );
#130650 = CARTESIAN_POINT ( 'NONE',  ( 0.006913841192817556623, 8.234242197375175820, 1.999988128101762408 ) ) ;
#130651 = CARTESIAN_POINT ( 'NONE',  ( 4.376249722160992839, 8.327651452488305850, 0.000000000000000000 ) ) ;
#130652 = CARTESIAN_POINT ( 'NONE',  ( -1.364683531250010295, 14.69270833367472839, 0.7879004041258445001 ) ) ;
#130653 = CARTESIAN_POINT ( 'NONE',  ( -4.842197138736131556, 5.678260079060780008, 1.199719254218452935 ) ) ;
#130654 = PRODUCT_DEFINITION_CONTEXT ( 'detailed design', #58896, 'design' ) ;
#130655 = CARTESIAN_POINT ( 'NONE',  ( 0.5455463417442986129, -1.458554840210561476, 1.392547631435703037 ) ) ;
#130656 = CARTESIAN_POINT ( 'NONE',  ( -8.012505595996376684, 12.29174759539704986, 0.000000000000000000 ) ) ;
#130657 = AXIS2_PLACEMENT_3D ( 'NONE', #127717, #177443, #178509 ) ;
#130658 = CARTESIAN_POINT ( 'NONE',  ( 4.557524383921963462, 1.659614545607337677, 1.237363147772299721 ) ) ;
#130659 = CARTESIAN_POINT ( 'NONE',  ( 3.281779325460960628, 1.222525406819600757, 1.488901545882119759 ) ) ;
#130660 = CARTESIAN_POINT ( 'NONE',  ( 5.519199075762924345, -1.913696209152406125, 0.9060895950074706606 ) ) ;
#130661 = CARTESIAN_POINT ( 'NONE',  ( 5.392392409933256303, 7.314210449720692786, 1.599625672291267398 ) ) ;
#130663 = EDGE_CURVE ( 'NONE', #133272, #187716, #59807, .T. ) ;
#130662 = CARTESIAN_POINT ( 'NONE',  ( -0.6823417656249969321, 5.467708333674756283, -1.181850606188749264 ) ) ;
#130664 = CARTESIAN_POINT ( 'NONE',  ( 3.836728334651629879, -1.896773656598240709, -0.5296851528490874594 ) ) ;
#130665 = CARTESIAN_POINT ( 'NONE',  ( 5.999983301813878178, -0.8195729662384824143, -2.140910441102741313 ) ) ;
#130666 = CARTESIAN_POINT ( 'NONE',  ( 4.055160972438559774, -1.518969423100406946, -1.012540670841777013 ) ) ;
#130667 = ADVANCED_FACE ( 'NONE', ( #184165 ), #3263, .T. ) ;
#130668 = CARTESIAN_POINT ( 'NONE',  ( 6.211043768836173484, 8.339580045099285854, 1.443375672974065660 ) ) ;
#130669 = CARTESIAN_POINT ( 'NONE',  ( 5.300874872818840622, 6.247070775452521652, 1.082531754730560403 ) ) ;
#130670 = CARTESIAN_POINT ( 'NONE',  ( -6.444921918449773024, 8.612437886315108315, 1.599625672291269396 ) ) ;
#130671 = CARTESIAN_POINT ( 'NONE',  ( 6.879836604291781121, 6.991173891287354003, -0.7998128361456341429 ) ) ;
#130672 = ORIENTED_EDGE ( 'NONE', *, *, #103048, .F. ) ;
#130673 = CARTESIAN_POINT ( 'NONE',  ( 5.379157392057874354, -1.821786014368693252, -0.8570216514257876783 ) ) ;
#130674 = CARTESIAN_POINT ( 'NONE',  ( 6.188148266813070286, 1.908752161701723571, 1.280650486962619627 ) ) ;
#130675 = CARTESIAN_POINT ( 'NONE',  ( 4.504711789546460565, 0.5192035298374733099, 1.891763301562799260 ) ) ;
#130676 = CARTESIAN_POINT ( 'NONE',  ( -6.181627972826976958, 9.299317504018391745, 1.199719254218452047 ) ) ;
#130677 = CARTESIAN_POINT ( 'NONE',  ( -3.761497552787613330, 6.475832013972435242, 1.199719254218464037 ) ) ;
#130678 = CARTESIAN_POINT ( 'NONE',  ( -0.9999999999999965583, 6.120000000000022311, 1.226552901175238481E-14 ) ) ;
#130679 = CARTESIAN_POINT ( 'NONE',  ( -4.776215253764153346, 8.794277906025310898, -0.7998128361456362523 ) ) ;
#130681 = CARTESIAN_POINT ( 'NONE',  ( 6.807488043635657959, -0.3792581958518992935, 1.734866861734218446 ) ) ;
#130680 = CARTESIAN_POINT ( 'NONE',  ( 0.3805629577237649719, -0.2597898305938106112, -2.074488238918821725 ) ) ;
#130682 = CARTESIAN_POINT ( 'NONE',  ( -1.201851678989727383E-14, 2.962500000000025224, 1.732050807568877637 ) ) ;
#130683 = CARTESIAN_POINT ( 'NONE',  ( 6.386669098100576036, 1.688287130807873293, -0.9594923298414399504 ) ) ;
#130684 = CARTESIAN_POINT ( 'NONE',  ( -0.2102771530458276972, 0.6786276403282426317, -2.283427277113641019 ) ) ;
#130685 = CARTESIAN_POINT ( 'NONE',  ( 1.329236136963531489, 0.8583591509643221373, -1.513936452999464555 ) ) ;
#130686 = CARTESIAN_POINT ( 'NONE',  ( 6.810273232766058449, 6.839740281182199233, 1.040834085586084257E-14 ) ) ;
#130687 = CARTESIAN_POINT ( 'NONE',  ( 3.633072077242065861E-15, -6.802539632833518519E-15, -0.2598076211376265099 ) ) ;
#130688 = CARTESIAN_POINT ( 'NONE',  ( 1.400563108759992792, 1.411875272319111696, -0.9905557981151734692 ) ) ;
#130689 = CARTESIAN_POINT ( 'NONE',  ( 2.138457411672203712, 0.4836887423533155483, 2.137355272389021899 ) ) ;
#130690 = CARTESIAN_POINT ( 'NONE',  ( 3.985166894971280183, -0.2153072539897090687, -2.196357064762343825 ) ) ;
#130691 = AXIS2_PLACEMENT_3D ( 'NONE', #26797, #158948, #110263 ) ;
#130692 = CARTESIAN_POINT ( 'NONE',  ( 1.569424903267138571, 1.913428125876670549, 1.025899993198212901 ) ) ;
#130693 = CARTESIAN_POINT ( 'NONE',  ( -1.270904146967334336, 2.959693569853255823, 0.7750000000000152323 ) ) ;
#130694 = CARTESIAN_POINT ( 'NONE',  ( 2.554045646286424276, 1.136978842527110123, 1.786019645988563997 ) ) ;
#130695 = VERTEX_POINT ( 'NONE', #199338 ) ;
#130697 = CARTESIAN_POINT ( 'NONE',  ( -1.402160292154681736E-14, 0.1343750003414218575, 1.575800808251672791 ) ) ;
#130696 = CARTESIAN_POINT ( 'NONE',  ( 3.070184882724129594, -1.363667385223182871, 1.842535374393680980 ) ) ;
#130698 = CARTESIAN_POINT ( 'NONE',  ( 2.333974999846879061, 5.874721266463329705, -0.7998128361456291469 ) ) ;
#130699 = CARTESIAN_POINT ( 'NONE',  ( 3.683011284406639607, 7.448596931783069586, 0.7998128361456321445 ) ) ;
#130700 = VECTOR ( 'NONE', #153099, 1000.000000000000000 ) ;
#130701 = CARTESIAN_POINT ( 'NONE',  ( 5.303485788544977098, 1.959706058537356910, -1.045853978123905570 ) ) ;
#130702 = CARTESIAN_POINT ( 'NONE',  ( -7.876924059859742755, 8.292092279365579799, 1.040834085586084257E-14 ) ) ;
#130703 = DIRECTION ( 'NONE',  ( 1.000000000000000000, 1.725633230170963762E-31, 8.638326563840814399E-31 ) ) ;
#130704 = CARTESIAN_POINT ( 'NONE',  ( 3.687454593236936251, 7.245854758844324728, -0.7216878364870267237 ) ) ;
#130705 = CARTESIAN_POINT ( 'NONE',  ( -6.521108698048772467, 9.591415333490143524, -1.082531754730537976 ) ) ;
#130706 = CARTESIAN_POINT ( 'NONE',  ( 5.573810548993915148, 5.675402860013913475, 0.000000000000000000 ) ) ;
#130707 = VERTEX_POINT ( 'NONE', #84541 ) ;
#130708 = CARTESIAN_POINT ( 'NONE',  ( 3.006482587178582300, -1.942541511447487990, 0.5404910644229294903 ) ) ;
#130710 = CARTESIAN_POINT ( 'NONE',  ( 1.885666897375902096, -1.943580278752204515, 0.6908589954031388869 ) ) ;
#130709 = CARTESIAN_POINT ( 'NONE',  ( 7.558834334818744338, 8.777393797832065303, 1.199719254218462483 ) ) ;
#130711 = CARTESIAN_POINT ( 'NONE',  ( -11.92619526913699879, 13.39999999999998259, 1.328859060402682868 ) ) ;
#130712 = CARTESIAN_POINT ( 'NONE',  ( 5.682275777458854371, 5.801945626556378244, 0.7216878364870328300 ) ) ;
#130713 = CARTESIAN_POINT ( 'NONE',  ( -5.599154252763867134, 5.634694171087028636, 0.000000000000000000 ) ) ;
#130714 = CARTESIAN_POINT ( 'NONE',  ( -0.6823417656249969321, 3.717708333674754506, -1.181850606188749264 ) ) ;
#130715 = CARTESIAN_POINT ( 'NONE',  ( 4.681673494351117348, -1.034495392153191418, 1.931897795048514554 ) ) ;
#130716 = CARTESIAN_POINT ( 'NONE',  ( 1.969375177810539945, -1.978050944945686673, -0.3905967402937361443 ) ) ;
#130717 = CARTESIAN_POINT ( 'NONE',  ( 0.5558949066124979632, -1.334021266253348381, 1.269314063962425854 ) ) ;
#130718 = CARTESIAN_POINT ( 'NONE',  ( 8.471147050440139381, 8.777426401801974976, -0.7998128361456281477 ) ) ;
#130719 = CARTESIAN_POINT ( 'NONE',  ( 5.139593076133685656, -1.292025762983131099, -1.289991942498528665 ) ) ;
#130720 = CARTESIAN_POINT ( 'NONE',  ( 6.293592298849589817, 1.492257802130890765, -1.356297202127904944 ) ) ;
#130721 = CARTESIAN_POINT ( 'NONE',  ( -7.771848369131641121, 10.09024240211882351, -1.599625672291263179 ) ) ;
#130723 = CARTESIAN_POINT ( 'NONE',  ( -4.945692173934974178, 8.992000979557944973, 0.000000000000000000 ) ) ;
#130722 = CARTESIAN_POINT ( 'NONE',  ( 4.610415411315283762, -0.9635332438130711497, -2.047219928730920291 ) ) ;
#130724 = CARTESIAN_POINT ( 'NONE',  ( 0.7332070197069834316, 0.1568218392365756941, 2.100289424198895194 ) ) ;
#130725 = CARTESIAN_POINT ( 'NONE',  ( -6.936931872047518155, 8.122117267924091166, 1.199719254218452047 ) ) ;
#130726 = CARTESIAN_POINT ( 'NONE',  ( 5.160626937512653001, -0.6942339714755951796, -1.950645400549338104 ) ) ;
#130727 = CARTESIAN_POINT ( 'NONE',  ( 9.901532256681887745, 10.44620914241737530, 0.000000000000000000 ) ) ;
#130728 = CARTESIAN_POINT ( 'NONE',  ( 2.857643957345961550, 20.33553470530817719, 19.20483188695337162 ) ) ;
#130729 = CARTESIAN_POINT ( 'NONE',  ( -8.503988664269602538, 10.94440607977979063, 1.599625672291269396 ) ) ;
#130730 = DIRECTION ( 'NONE',  ( -0.6507913734559640506, -0.7592566023653004592, 0.000000000000000000 ) ) ;
#130731 = CARTESIAN_POINT ( 'NONE',  ( 6.984385409695311964, 8.177479728513226576, 1.199719254218452935 ) ) ;
#130732 = CARTESIAN_POINT ( 'NONE',  ( 4.540820729390463661, 6.975461451583557348, -1.175308324676842542 ) ) ;
#130733 = CARTESIAN_POINT ( 'NONE',  ( -9.408995418203979000, 12.00024729270324286, 1.443375672974076540 ) ) ;
#130735 = CARTESIAN_POINT ( 'NONE',  ( 1.934110000270176322, -2.153362505827714823, 0.5451143137677332273 ) ) ;
#130734 = CARTESIAN_POINT ( 'NONE',  ( 1.740644586495963431, 1.216819214799185866, -1.736574482785017359 ) ) ;
#130736 = FACE_OUTER_BOUND ( 'NONE', #62878, .T. ) ;
#130737 = CARTESIAN_POINT ( 'NONE',  ( -6.622231685632140596, 6.690634819517756959, 0.000000000000000000 ) ) ;
#130738 = CARTESIAN_POINT ( 'NONE',  ( 4.625302960556422427, 8.547937220624488575, 1.040834085586084257E-14 ) ) ;
#130739 = CARTESIAN_POINT ( 'NONE',  ( 3.683996026499200660, -1.166640140252427793, -1.577160851978461009 ) ) ;
#130740 = CARTESIAN_POINT ( 'NONE',  ( 5.229694566569264680, 7.124396299129368337, 1.599625672291267398 ) ) ;
#130741 = CARTESIAN_POINT ( 'NONE',  ( -4.264599663924041550, 7.301641052403419430, 0.9184948912712449509 ) ) ;
#130742 = CARTESIAN_POINT ( 'NONE',  ( 4.708759422647839976, 4.387974169377582001, -0.7998128361456211532 ) ) ;
#130743 = CARTESIAN_POINT ( 'NONE',  ( -4.936577329151611515, 7.813071746435248599, 1.082531754730549967 ) ) ;
#130744 = CARTESIAN_POINT ( 'NONE',  ( -6.724481002698126098, 8.868313807946373473, -1.443375672974059665 ) ) ;
#130745 = CARTESIAN_POINT ( 'NONE',  ( 2.654661980655496301, 2.105093816413053709, 0.2552270188876659129 ) ) ;
#130746 = CARTESIAN_POINT ( 'NONE',  ( -6.771371375382467583, 6.864631124226471037, -0.7998128361456362523 ) ) ;
#130747 = CARTESIAN_POINT ( 'NONE',  ( 6.109812101310618360, 0.5708666350849945781, -1.876949146916474298 ) ) ;
#130748 = CARTESIAN_POINT ( 'NONE',  ( 4.575171270262055501, 0.003154952768896768234, -2.161883445794945846 ) ) ;
#130749 = CARTESIAN_POINT ( 'NONE',  ( 2.911469271472226339, -0.9098125248445630975, -1.600700954789348263 ) ) ;
#130750 = CARTESIAN_POINT ( 'NONE',  ( -4.789689200157987159, 6.785576372466274542, 1.244997348908165602 ) ) ;
#130751 = CARTESIAN_POINT ( 'NONE',  ( -0.6823417656250246877, -0.3864583329919110688, 1.181850606188755259 ) ) ;
#130752 = CARTESIAN_POINT ( 'NONE',  ( 5.507646315527288117, -0.7876679103963373230, -1.551952608056671457 ) ) ;
#130753 = CARTESIAN_POINT ( 'NONE',  ( -5.777182852754558340, 5.912670547734647286, 0.000000000000000000 ) ) ;
#130754 = CARTESIAN_POINT ( 'NONE',  ( 3.985733972737593778, 6.633478153960411738, -1.082531754730548412 ) ) ;
#130755 = CARTESIAN_POINT ( 'NONE',  ( -1.499999999999997780, 3.681250000682819046, 1.214306433183764966E-14 ) ) ;
#130756 = CARTESIAN_POINT ( 'NONE',  ( 3.010779355932476253, 1.566693023359872372, -1.489686202715050145 ) ) ;
#130757 = CARTESIAN_POINT ( 'NONE',  ( 5.044295983762377311, 1.882185518538554314, -0.7230303062365079914 ) ) ;
#130758 = CARTESIAN_POINT ( 'NONE',  ( -9.639484029191951464, 10.34841224358651601, 0.7216878364870438212 ) ) ;
#130759 = CARTESIAN_POINT ( 'NONE',  ( 1.920999885407469243, 2.016935458891587096, 0.7782144962657986387 ) ) ;
#130760 = CARTESIAN_POINT ( 'NONE',  ( 2.530492563074437928, 1.911271491015430035, 0.4824842627236708426 ) ) ;
#130761 = CARTESIAN_POINT ( 'NONE',  ( -11.07790593930098311, 12.30000000000000071, -0.7000000000000009548 ) ) ;
#130762 = CARTESIAN_POINT ( 'NONE',  ( 4.142085694530703854, 0.5209831505245207106, 1.870798910701749973 ) ) ;
#130765 = EDGE_LOOP ( 'NONE', ( #22148, #141825, #19596, #12687, #35410, #130308, #20170, #16378, #161190, #204616, #1230, #53822, #63929, #118844, #203647, #58422, #45755, #101760, #2254, #173969, #144566, #209177, #43052, #101889 ) ) ;
#130764 =( LENGTH_UNIT ( ) NAMED_UNIT ( * ) SI_UNIT ( .MILLI., .METRE. ) );
#130763 = CARTESIAN_POINT ( 'NONE',  ( -8.961576348508637935, 12.43862759236002269, -1.082531754730543083 ) ) ;
#130766 = CARTESIAN_POINT ( 'NONE',  ( -7.781453819600577582, 8.043060642480948985, 0.000000000000000000 ) ) ;
#130767 = CARTESIAN_POINT ( 'NONE',  ( 5.422335090822693715, 5.290755458906732933, 0.000000000000000000 ) ) ;
#130769 = EDGE_LOOP ( 'NONE', ( #166210, #146321, #88839 ) ) ;
#130768 = CARTESIAN_POINT ( 'NONE',  ( -6.306477729012051725, 7.386587434382707151, 1.199719254218452047 ) ) ;
#130770 = CARTESIAN_POINT ( 'NONE',  ( -8.853111119599343937, 10.39134639669645566, 1.082531754730558626 ) ) ;
#130771 = CARTESIAN_POINT ( 'NONE',  ( 0.7455094363101981703, -1.891729906373079029, 1.136061337225414913 ) ) ;
#130772 = CARTESIAN_POINT ( 'NONE',  ( -3.285556943750000514, -2.238541666188709200, -1.896917185911906500 ) ) ;
#130773 = CARTESIAN_POINT ( 'NONE',  ( 4.803538753074391821, -1.513872852549098091, -1.247617340562396926 ) ) ;
#130774 = CARTESIAN_POINT ( 'NONE',  ( 1.364683531249990311, 4.676041667008083103, 0.7879004041258500513 ) ) ;
#130775 = CARTESIAN_POINT ( 'NONE',  ( -1.500000000000011324, 2.952083334016149418, 0.8660254037844403729 ) ) ;
#130776 = CARTESIAN_POINT ( 'NONE',  ( 0.1745949693968692484, 0.009193469831055355729, -1.755468632744116242 ) ) ;
#130777 = CARTESIAN_POINT ( 'NONE',  ( 3.714658492009088153, -0.1339090230784937274, 1.836323816731308067 ) ) ;
#130778 = VERTEX_POINT ( 'NONE', #116039 ) ;
#130779 = APPLICATION_CONTEXT ( 'automotive_design' ) ;
#130780 = CARTESIAN_POINT ( 'NONE',  ( -0.6125000000000105915, 1.604166667349450570, 1.060881119635899816 ) ) ;
#130781 = CARTESIAN_POINT ( 'NONE',  ( -7.320512876374914768, 10.62801655815766999, 1.199719254218453823 ) ) ;
#130782 = DIRECTION ( 'NONE',  ( 0.000000000000000000, -1.000000000000000000, 0.000000000000000000 ) ) ;
#130783 = CARTESIAN_POINT ( 'NONE',  ( 4.922192346260840345, -2.110166376318895587, 0.2103620946037400852 ) ) ;
#130784 = CARTESIAN_POINT ( 'NONE',  ( 4.788000803920411386, 8.737751371215816576, 1.040834085586084257E-14 ) ) ;
#130785 = EDGE_CURVE ( 'NONE', #18108, #192481, #118178, .T. ) ;
#130786 = CARTESIAN_POINT ( 'NONE',  ( 6.345006307232072373, -1.743395995315766056, 1.098490678494741912 ) ) ;
#130789 = CARTESIAN_POINT ( 'NONE',  ( 3.192734241421916419, 1.453351889590439816, 1.130385295574042104 ) ) ;
#130788 = CARTESIAN_POINT ( 'NONE',  ( 1.099803389655891195, 0.7588869020343449456, -1.699499299819209108 ) ) ;
#130787 = CARTESIAN_POINT ( 'NONE',  ( 3.147653791585804051, 8.919999999999937756, -2.420000000000002149 ) ) ;
#130790 = CARTESIAN_POINT ( 'NONE',  ( 7.099665995050449041, 11.43469409420089455, 0.7998128361456462443 ) ) ;
#130791 = CARTESIAN_POINT ( 'NONE',  ( 8.902524791715917374, 3.162178953954597471, 7.495381307383154557 ) ) ;
#130792 = CARTESIAN_POINT ( 'NONE',  ( -6.312203035614172286, 9.521931420595302953, -1.199719254218452047 ) ) ;
#130793 = CARTESIAN_POINT ( 'NONE',  ( 4.161989969715248705, 4.726297878971393196, -2.500000000000000444 ) ) ;
#130794 = CIRCLE ( 'NONE', #123859, 0.09999999999999971412 ) ;
#130795 = CARTESIAN_POINT ( 'NONE',  ( 3.405080638938757343, 1.739790774466195789, -1.357627211771177178 ) ) ;
#130796 = CARTESIAN_POINT ( 'NONE',  ( 5.026804934256954738, 2.162974397647707825, 0.6633081500663459140 ) ) ;
#130797 = CARTESIAN_POINT ( 'NONE',  ( -5.422898255786186006, 9.270539031818461950, -0.7216878364870207285 ) ) ;
#130798 = CARTESIAN_POINT ( 'NONE',  ( 5.414259967653319627, -1.811767230315189048, 0.008324397547932599339 ) ) ;
#130799 = B_SPLINE_CURVE_WITH_KNOTS ( 'NONE', 3,
 ( #174929, #75271, #77398, #158660, #143514, #209510, #61151, #44928 ),
 .UNSPECIFIED., .F., .F.,
 ( 4, 2, 2, 4 ),
 ( 2.544396950703400505E-07, 0.0002984430161323410840, 0.0005966315925696118964, 0.001193008745444153196 ),
 .UNSPECIFIED. ) ;
#130800 = CARTESIAN_POINT ( 'NONE',  ( 5.067565384200278800, 1.291559945344708638, 1.415018661930996569 ) ) ;
#130801 = EDGE_CURVE ( 'NONE', #29604, #158693, #42667, .T. ) ;
#130802 = CARTESIAN_POINT ( 'NONE',  ( -0.6823417656250212460, 5.613541667008087543, 1.181850606188767472 ) ) ;
#130803 = CARTESIAN_POINT ( 'NONE',  ( 6.104356062600288624, -0.6750377415852754082, -1.744797942764392928 ) ) ;
#130804 = EDGE_CURVE ( 'NONE', #127875, #83638, #163208, .T. ) ;
#130805 = CARTESIAN_POINT ( 'NONE',  ( 5.441811508714582857, 1.250024229543914567, 1.378945535785504051 ) ) ;
#130806 = CARTESIAN_POINT ( 'NONE',  ( -7.334597915313094241, 9.580116872663850813, 1.040834085586084257E-14 ) ) ;
#130807 = CARTESIAN_POINT ( 'NONE',  ( 0.1626889888870358680, -1.668787113083155305, -0.8454427722031019332 ) ) ;
#130808 = AXIS2_PLACEMENT_3D ( 'NONE', #166256, #97029, #15726 ) ;
#130809 = CARTESIAN_POINT ( 'NONE',  ( 1.270720652900014791, -0.3006520276036573902, -1.993892820393451615 ) ) ;
#130811 = CARTESIAN_POINT ( 'NONE',  ( 2.455815469989936606, 0.5610288669116151317, -2.029897440403311215 ) ) ;
#130810 = CARTESIAN_POINT ( 'NONE',  ( -9.480175724453545172, 12.08329098332774265, 1.599625672291281386 ) ) ;
#130812 = CARTESIAN_POINT ( 'NONE',  ( 7.072549687823125097, 11.40305840243567381, -0.7998128361456291469 ) ) ;
#130814 = CARTESIAN_POINT ( 'NONE',  ( -8.143643823302737061, 12.65266822716189843, 0.000000000000000000 ) ) ;
#130813 = DIRECTION ( 'NONE',  ( -3.330669073875478989E-16, 3.330669073875478989E-16, 1.000000000000000000 ) ) ;
#130815 = CARTESIAN_POINT ( 'NONE',  ( 11.92619526913699879, 10.90000000000000036, -1.328859060402686199 ) ) ;
#130816 = CARTESIAN_POINT ( 'NONE',  ( 1.318624316974380317, -0.7310098426952565953, -1.883032709213072975 ) ) ;
#130817 = CARTESIAN_POINT ( 'NONE',  ( -0.6823417656250003738, 2.217708333674753174, -1.181850606188749264 ) ) ;
#130818 = CARTESIAN_POINT ( 'NONE',  ( 2.171277156482887882, 5.684907115872006145, -0.7998128361456291469 ) ) ;
#130819 = CARTESIAN_POINT ( 'NONE',  ( 2.899875653925917174, -0.6810940995312758650, 2.051530325002319799 ) ) ;
#130820 = CARTESIAN_POINT ( 'NONE',  ( 6.883263157960367806, 7.629137130509066722, 2.653810918356712900 ) ) ;
#130822 = CARTESIAN_POINT ( 'NONE',  ( 3.469446951953614189E-15, 8.900000000000025224, 1.214306433183764966E-14 ) ) ;
#130821 = CARTESIAN_POINT ( 'NONE',  ( 5.408776937209000657, 5.274937613024121674, 0.7998128361456352531 ) ) ;
#130823 = CARTESIAN_POINT ( 'NONE',  ( 8.378575743120986630, 12.71882943370911789, 1.040834085586084257E-14 ) ) ;
#130824 = CARTESIAN_POINT ( 'NONE',  ( 11.86145016429272836, 10.19999999999999929, -1.100000000000000311 ) ) ;
#130825 = CARTESIAN_POINT ( 'NONE',  ( -6.561783159334121152, 10.59923808595773664, -0.7216878364870278340 ) ) ;
#130826 = CARTESIAN_POINT ( 'NONE',  ( 0.6823417656249882723, 0.4260416670080896528, -1.181850606188749264 ) ) ;
#130827 = CARTESIAN_POINT ( 'NONE',  ( 1.382659466718983543, -0.3261178763579902218, -2.167053615394160637 ) ) ;
#130828 = CARTESIAN_POINT ( 'NONE',  ( 0.2828007905113860132, 7.102855049428861811, 1.981079112686755517 ) ) ;
#130829 = CARTESIAN_POINT ( 'NONE',  ( 2.571453329723889958, 0.1116048768269807673, -2.259888279461387040 ) ) ;
#130830 = CARTESIAN_POINT ( 'NONE',  ( -8.128276786592724790, 9.441743324901704426, -1.199719254218446718 ) ) ;
#130831 = CARTESIAN_POINT ( 'NONE',  ( -4.460269348771590536, 5.266364330730674226, 1.082531754730558626 ) ) ;
#130832 = CARTESIAN_POINT ( 'NONE',  ( 1.364683531249988535, 3.926041667008087543, 0.7879004041258500513 ) ) ;
#130833 = CARTESIAN_POINT ( 'NONE',  ( 4.812442952513422689, 8.115120723895499211, -0.8517184758452013282 ) ) ;
#130834 = CARTESIAN_POINT ( 'NONE',  ( -1.500000000000001110, 10.52083333333333037, 0.8660254037844419273 ) ) ;
#130835 = CARTESIAN_POINT ( 'NONE',  ( 3.444653546323793947, 6.176457016423196222, 1.199719254218451159 ) ) ;
#130836 = CARTESIAN_POINT ( 'NONE',  ( 3.075218854414006220, 1.681628227459546432, -0.5517178611392310472 ) ) ;
#130837 = CIRCLE ( 'NONE', #85780, 0.08000000000000020983 ) ;
#130838 = CARTESIAN_POINT ( 'NONE',  ( 6.475609205405274515, 2.113627995098281254, -0.6344055572156809264 ) ) ;
#130839 = CARTESIAN_POINT ( 'NONE',  ( 1.364683531249997417, 9.484375000341396245, 2.602085213965210642E-15 ) ) ;
#130840 = CARTESIAN_POINT ( 'NONE',  ( -4.990283058281743678, 7.979691447040783814, -1.199719254218453823 ) ) ;
#130841 = CARTESIAN_POINT ( 'NONE',  ( 5.185172808627552143, 1.650094130669476522, 1.158673036085342112 ) ) ;
#130842 = ORIENTED_EDGE ( 'NONE', *, *, #101284, .F. ) ;
#130843 = CARTESIAN_POINT ( 'NONE',  ( 2.131529507118444133, -1.219933349377068099, -1.418231869465089057 ) ) ;
#130844 = CARTESIAN_POINT ( 'NONE',  ( 3.661042849074844785, 1.635018244968543977, -1.269851595989857085 ) ) ;
#130845 = CARTESIAN_POINT ( 'NONE',  ( -7.715998819508785189, 8.174622508947939181, -0.7216878364870338292 ) ) ;
#130846 = DIRECTION ( 'NONE',  ( 0.000000000000000000, -0.7996470168499970610, 0.6004703560067728985 ) ) ;
#130847 = CARTESIAN_POINT ( 'NONE',  ( 9.534401699824593734, 3.538070456466941849, 7.287265385874707846 ) ) ;
#130848 = CARTESIAN_POINT ( 'NONE',  ( -1.364683531250010295, 4.342708333674753618, 0.7879004041258379498 ) ) ;
#130849 = CARTESIAN_POINT ( 'NONE',  ( 1.582132296805271787, 0.9858968508435607125, 1.638552900098678045 ) ) ;
#130850 = CARTESIAN_POINT ( 'NONE',  ( 2.980854556682940526, 1.846358069237159949, 0.6635599008937702603 ) ) ;
#130851 = CARTESIAN_POINT ( 'NONE',  ( 1.229842044428463010, -1.821462008879136896, -0.8645945014377558469 ) ) ;
#130852 = EDGE_CURVE ( 'NONE', #209619, #199345, #93395, .T. ) ;
#130853 = CARTESIAN_POINT ( 'NONE',  ( -3.800028193580205382, 7.655393002477360653, -0.7998128361456481317 ) ) ;
#130855 = PRESENTATION_STYLE_ASSIGNMENT (( #177415 ) ) ;
#130854 = CARTESIAN_POINT ( 'NONE',  ( 9.284636267260101050, 9.726497154758602548, -0.7998128361456281477 ) ) ;
#130856 = CARTESIAN_POINT ( 'NONE',  ( 6.415303688471941435, -0.2438443212883933120, 1.956177878852760177 ) ) ;
#130857 = CARTESIAN_POINT ( 'NONE',  ( -1.364683531249997417, 2.759375000341422801, 1.214306433183764966E-14 ) ) ;
#130859 = CARTESIAN_POINT ( 'NONE',  ( 1.880608475893473353, -0.5680388087716014001, -2.039528425668888811 ) ) ;
#130858 = CARTESIAN_POINT ( 'NONE',  ( -6.236387472606145010, 9.259240570473746601, -1.082531754730538864 ) ) ;
#130860 = DIRECTION ( 'NONE',  ( 0.000000000000000000, -1.000000000000000000, 0.000000000000000000 ) ) ;
#130861 = CARTESIAN_POINT ( 'NONE',  ( 3.525891238081061640, 2.020528833579691597, -0.4508363271973143682 ) ) ;
#130862 = CARTESIAN_POINT ( 'NONE',  ( 5.246079093845007257, 5.085123462432798114, 0.7998128361456352531 ) ) ;
#130864 = CARTESIAN_POINT ( 'NONE',  ( 5.217190183160311356, 4.981143389975473568, -0.7998128361456211532 ) ) ;
#130863 = CARTESIAN_POINT ( 'NONE',  ( 5.490208796768200727, -0.5072484191241812823, -2.028029781992314096 ) ) ;
#130866 = ORIENTED_EDGE ( 'NONE', *, *, #35714, .T. ) ;
#130865 = CARTESIAN_POINT ( 'NONE',  ( 4.735264887803245060, -1.668767028523497675, 0.7406363711058363553 ) ) ;
#130867 = CARTESIAN_POINT ( 'NONE',  ( 9.887974103068218668, 10.43039129653476493, 0.7998128361456462443 ) ) ;
#130868 = MECHANICAL_DESIGN_GEOMETRIC_PRESENTATION_REPRESENTATION (  '', ( #96360 ), #92803 ) ;
#130869 = PRESENTATION_STYLE_ASSIGNMENT (( #64726 ) ) ;
#130870 = CARTESIAN_POINT ( 'NONE',  ( 10.25278263059461636, 12.94063552693930497, 7.030852149930005623 ) ) ;
#130871 = CARTESIAN_POINT ( 'NONE',  ( 6.071336392737415544, 0.1682094380959769098, -2.200428349287026908 ) ) ;
#130873 =( BOUNDED_CURVE ( )  B_SPLINE_CURVE ( 3, ( #76962, #112746, #178758, #13023 ),
 .UNSPECIFIED., .F., .T. ) 
 B_SPLINE_CURVE_WITH_KNOTS ( ( 4, 4 ),
 ( 0.5000000000000018874, 1.000000000000000000 ),
 .UNSPECIFIED. ) 
 CURVE ( )  GEOMETRIC_REPRESENTATION_ITEM ( )  RATIONAL_B_SPLINE_CURVE ( ( 0.9999999999999974465, 0.3333333333333333703, 0.3333333333333358683, 1.000000000000000000 ) ) 
 REPRESENTATION_ITEM ( '' )  );
#130872 = CARTESIAN_POINT ( 'NONE',  ( 1.364683531250000748, 10.06770833367473017, -0.7879004041258355073 ) ) ;
#130874 = EDGE_CURVE ( 'NONE', #167392, #117162, #126065, .T. ) ;
#130875 = ORIENTED_EDGE ( 'NONE', *, *, #50048, .T. ) ;
#130876 = CARTESIAN_POINT ( 'NONE',  ( 4.775979982822478931, 1.890921987351320777, -0.2842533987747336566 ) ) ;
#130877 = CARTESIAN_POINT ( 'NONE',  ( -3.810004860640155311, 4.403759411290286252, 1.199719254218462483 ) ) ;
#130878 = CARTESIAN_POINT ( 'NONE',  ( 8.145751363712157911, 8.397798100619326078, -0.7998128361456281477 ) ) ;
#130879 = CARTESIAN_POINT ( 'NONE',  ( -3.755786496842899057E-14, 1.109375000341423112, -1.570758158831814466 ) ) ;
#130880 = CARTESIAN_POINT ( 'NONE',  ( 4.406036734316882253, 6.163462161501577441, -1.443375672974051449 ) ) ;
#130881 = CARTESIAN_POINT ( 'NONE',  ( 11.00009153390426420, -6.553298220693314136, -0.005414006223990005216 ) ) ;
#130882 = CARTESIAN_POINT ( 'NONE',  ( 7.947034306432539275, 14.34752413088959422, -8.932881469798775953 ) ) ;
#130883 = CARTESIAN_POINT ( 'NONE',  ( 0.4679805871025365382, -1.733519288248483559, -0.6209854868195128219 ) ) ;
#130884 = ORIENTED_EDGE ( 'NONE', *, *, #153998, .T. ) ;
#130885 = CARTESIAN_POINT ( 'NONE',  ( -5.589704470584107909, 9.743348658981940247, -0.7998128361456362523 ) ) ;
#130886 = CARTESIAN_POINT ( 'NONE',  ( 5.219927230130699591, -0.9996001844756461363, -1.580852690948472361 ) ) ;
#130887 = CARTESIAN_POINT ( 'NONE',  ( -1.651451222920911732, 0.8386022738108426244, 1.021479198850123060 ) ) ;
#130888 = CARTESIAN_POINT ( 'NONE',  ( 0.4019237886466847653, 10.82366454968463110, 1.499999999999997113 ) ) ;
#130889 = CARTESIAN_POINT ( 'NONE',  ( -0.2108831679770960255, -0.001785917861228669690, -1.896958272444612792 ) ) ;
#130890 = CARTESIAN_POINT ( 'NONE',  ( -7.429504990608782222, 8.730472579540773381, 1.082531754730549967 ) ) ;
#130891 = CARTESIAN_POINT ( 'NONE',  ( 5.172599298813543633, 5.993452922492633839, -1.199719254218452047 ) ) ;
#130892 = CARTESIAN_POINT ( 'NONE',  ( 0.9187298884396404297, -1.430263011927451311, 1.354180262349208075 ) ) ;
#130893 = CARTESIAN_POINT ( 'NONE',  ( 2.618767733003044551, 0.2496279305150179983, 2.000855661889962445 ) ) ;
#130894 = CARTESIAN_POINT ( 'NONE',  ( -8.345207244411405156, 9.694828859023472134, 1.199719254218462483 ) ) ;
#130895 = CARTESIAN_POINT ( 'NONE',  ( 4.016958651398847557, 7.908478536599129249, -0.7998128361456362523 ) ) ;
#130897 = EDGE_CURVE ( 'NONE', #81410, #29860, #77268, .T. ) ;
#130896 = CARTESIAN_POINT ( 'NONE',  ( 6.710127771514622808, -7.162053774861990796, 6.725445687907760650 ) ) ;
#130898 = CARTESIAN_POINT ( 'NONE',  ( 2.097856687836355150, -2.190910012095201420, 0.05558666267656967030 ) ) ;
#130899 = CARTESIAN_POINT ( 'NONE',  ( 2.325000000000003730, 0.05106627235655090274, -0.4999999999999941713 ) ) ;
#130900 = CARTESIAN_POINT ( 'NONE',  ( -8.513630394377489807, 12.01998699582738972, -1.199719254218446718 ) ) ;
#130901 = CARTESIAN_POINT ( 'NONE',  ( 3.701012746850603996, 7.261672604726938651, 1.040834085586084257E-14 ) ) ;
#130902 = ADVANCED_FACE ( 'NONE', ( #85606 ), #170250, .T. ) ;
#130903 = CARTESIAN_POINT ( 'NONE',  ( 3.282482588284323821, 6.843663763058119187, 0.7216878364870257245 ) ) ;
#130904 = CARTESIAN_POINT ( 'NONE',  ( 7.235247531187115833, 11.59287255302699648, -0.7998128361456291469 ) ) ;
#130905 = CARTESIAN_POINT ( 'NONE',  ( 6.661133543015731462, 6.665743976473484267, -0.7998128361456281477 ) ) ;
#130906 = CARTESIAN_POINT ( 'NONE',  ( -9.406910906341044765, 14.61725638504506364, 7.349368793364711827 ) ) ;
#130907 = CARTESIAN_POINT ( 'NONE',  ( 5.546694241766559230, 9.485244025454063532, 0.000000000000000000 ) ) ;
#130908 = ORIENTED_EDGE ( 'NONE', *, *, #84677, .F. ) ;
#130910 = CARTESIAN_POINT ( 'NONE',  ( 2.227199469478642335, 1.799111979166287512, 0.9032904990664193390 ) ) ;
#130909 = CARTESIAN_POINT ( 'NONE',  ( 5.214338956685347526, 1.703448749313410282, 0.6994016148276983591 ) ) ;
#130911 = CARTESIAN_POINT ( 'NONE',  ( 2.759436883174094746, -2.292065780239035178, -0.1713596109048869109 ) ) ;
#130913 = CARTESIAN_POINT ( 'NONE',  ( 1.938117168453708627, -1.000761817645494212, 1.568762535561243121 ) ) ;
#130912 = CARTESIAN_POINT ( 'NONE',  ( 3.714570900464285064, 4.396382807705524698, 1.082531754730560403 ) ) ;
#130914 = CARTESIAN_POINT ( 'NONE',  ( 0.000000000000000000, -2.296874999522042327, -3.793834371823813001 ) ) ;
#130915 = CARTESIAN_POINT ( 'NONE',  ( 6.117437049485344502, 1.593764408019750389, 1.056661447057717362 ) ) ;
#130916 = CARTESIAN_POINT ( 'NONE',  ( -8.158255747121117452, 10.54105100977322174, 1.599625672291295375 ) ) ;
#130917 = CARTESIAN_POINT ( 'NONE',  ( -4.990809943606269172, 8.836712344267034780, -0.7216878364870338292 ) ) ;
#130919 = CARTESIAN_POINT ( 'NONE',  ( 3.326877442632663939, 0.04465521416292458912, 1.870282673472216439 ) ) ;
#130918 = CARTESIAN_POINT ( 'NONE',  ( 5.372635804747151411, -0.05242855794247149731, -2.090268718351683930 ) ) ;
#130920 = CARTESIAN_POINT ( 'NONE',  ( 7.944714827928050838, 9.331550723079971021, 1.082531754730558626 ) ) ;
#130921 = CARTESIAN_POINT ( 'NONE',  ( 6.181194517112824194, 1.274813594131599226, 1.328792456347933637 ) ) ;
#130922 = CARTESIAN_POINT ( 'NONE',  ( 2.822068529938852155, 6.444163718237301275, -0.7998128361456291469 ) ) ;
#130924 = CARTESIAN_POINT ( 'NONE',  ( 5.515469562660962666, 5.329135999392899947, 0.7998128361456341429 ) ) ;
#130923 = CARTESIAN_POINT ( 'NONE',  ( 0.4382560683119230416, -7.700000000000008171, -10.99126615174918165 ) ) ;
#130925 = CARTESIAN_POINT ( 'NONE',  ( 4.652814366283819503, -1.382804000779764619, 1.030830748262304253 ) ) ;
#130926 = CARTESIAN_POINT ( 'NONE',  ( -5.575427483717760424, 7.527751369135936343, 1.599625672291269396 ) ) ;
#130927 = CARTESIAN_POINT ( 'NONE',  ( 0.000000000000000000, 4.000000000000003553, 0.000000000000000000 ) ) ;
#130928 = CARTESIAN_POINT ( 'NONE',  ( 1.907862554904949492, 3.236716050607333361, 0.4606469147255249919 ) ) ;
#130929 =( BOUNDED_CURVE ( )  B_SPLINE_CURVE ( 1, ( #143889, #13819 ),
 .UNSPECIFIED., .F., .T. ) 
 B_SPLINE_CURVE_WITH_KNOTS ( ( 2, 2 ),
 ( 0.000000000000000000, 6.249999999999788711E-05 ),
 .UNSPECIFIED. ) 
 CURVE ( )  GEOMETRIC_REPRESENTATION_ITEM ( )  RATIONAL_B_SPLINE_CURVE ( ( 0.9345202395942815432, 0.9345202395942815432 ) ) 
 REPRESENTATION_ITEM ( '' )  );
#130930 = VECTOR ( 'NONE', #96248, 1000.000000000000000 ) ;
#130931 = CARTESIAN_POINT ( 'NONE',  ( 9.578219923806454261, -9.914766490055704651, -0.1663656176996578528 ) ) ;
#130932 = CARTESIAN_POINT ( 'NONE',  ( 4.997030173247643425, 0.3645372836193886967, 2.140096573681660619 ) ) ;
#130933 = CARTESIAN_POINT ( 'NONE',  ( 3.264084022359412529, 0.8216391472936382945, 1.630427331384458833 ) ) ;
#130934 = CARTESIAN_POINT ( 'NONE',  ( 1.533958681542445301, 1.164210590399002321, 1.578835587694705334 ) ) ;
#130935 = CARTESIAN_POINT ( 'NONE',  ( 6.016841150788749815, 0.2099786098018930069, 2.106937748889408546 ) ) ;
#130937 = CARTESIAN_POINT ( 'NONE',  ( 1.364683531249990311, 4.446875000341417028, 1.214306433183764966E-14 ) ) ;
#130936 = CARTESIAN_POINT ( 'NONE',  ( 5.899983332490822185, -0.8214817842997054198, -2.140285636048167017 ) ) ;
#130938 = CARTESIAN_POINT ( 'NONE',  ( -4.257741265285667431, 3.982435197156672491, 0.4597581080974452172 ) ) ;
#130939 = CARTESIAN_POINT ( 'NONE',  ( 7.391166297744269365, 11.77477778067701664, 1.040834085586084257E-14 ) ) ;
#130940 = CARTESIAN_POINT ( 'NONE',  ( 1.858217301831434964, 0.8087058978607818416, -1.960417502992222838 ) ) ;
#130941 = CARTESIAN_POINT ( 'NONE',  ( -3.633221978782299910, 5.261844946711204507, -1.443375672974053447 ) ) ;
#130942 = CARTESIAN_POINT ( 'NONE',  ( 5.595604037360608629, 5.769690798462138837, 0.6831429992372698434 ) ) ;
#130943 = CARTESIAN_POINT ( 'NONE',  ( -3.917943204224914933, 6.554388924028945240, -1.082531754730548412 ) ) ;
#130945 = PRESENTATION_LAYER_ASSIGNMENT (  '', '', ( #23569 ) ) ;
#130944 = VECTOR ( 'NONE', #23378, 1000.000000000000000 ) ;
#130946 = CARTESIAN_POINT ( 'NONE',  ( 6.684450694706582929, 1.257157530024972658, -1.769884466434832548 ) ) ;
#130948 = CARTESIAN_POINT ( 'NONE',  ( 0.7500000000000006661, 12.86458333401613352, 1.299038105676657340 ) ) ;
#130947 = CARTESIAN_POINT ( 'NONE',  ( 6.983263157960363010, -0.009046620988246899253, 2.153544821522495489 ) ) ;
#130949 = EDGE_LOOP ( 'NONE', ( #208112, #167079, #68961, #154270, #13270 ) ) ;
#130951 = ORIENTED_EDGE ( 'NONE', *, *, #167443, .T. ) ;
#130950 = CARTESIAN_POINT ( 'NONE',  ( 2.069254833283964867, -1.714886923611224745, 1.411838272681579687 ) ) ;
#130952 = CARTESIAN_POINT ( 'NONE',  ( -0.1335965759122420549, -0.1551069838626080166, -2.263292908747056131 ) ) ;
#130954 = CARTESIAN_POINT ( 'NONE',  ( 5.875849835592577897, -2.013560656311346619, 0.4463529024570592751 ) ) ;
#130953 = CARTESIAN_POINT ( 'NONE',  ( 4.955668840994886359, 5.740367388370866131, 1.199719254218462483 ) ) ;
#130956 = CARTESIAN_POINT ( 'NONE',  ( 0.000000000000000000, -3.937499999999998224, -4.012584370867899430 ) ) ;
#130955 = CARTESIAN_POINT ( 'NONE',  ( 6.717138760927786834, 6.801359740696030443, -0.7998128361456481317 ) ) ;
#130957 = CARTESIAN_POINT ( 'NONE',  ( 5.254667053748194760, 8.288139441751686931, 1.199719254218452047 ) ) ;
#130958 = CARTESIAN_POINT ( 'NONE',  ( 1.642778471875000035, -3.463541666188708845, -2.845375778867859751 ) ) ;
#130959 = CARTESIAN_POINT ( 'NONE',  ( 0.2331563151865729544, 2.882199166944008795, -2.434502449063076224 ) ) ;
#130960 = CARTESIAN_POINT ( 'NONE',  ( 4.194743914777058436, 1.481411246205705412, 1.093257649623424754 ) ) ;
#130961 = CARTESIAN_POINT ( 'NONE',  ( 5.005985031943777308, 6.863401842066294556, -1.599625672291256295 ) ) ;
#130962 = CARTESIAN_POINT ( 'NONE',  ( 2.274029058727170316, -1.063862581237082550, 1.357477553621669442 ) ) ;
#130963 = CARTESIAN_POINT ( 'NONE',  ( 0.4621254960020631519, -1.116205757145168231, 1.679226196708947016 ) ) ;
#130964 = CARTESIAN_POINT ( 'NONE',  ( 1.512731952202387653, -2.162554957723664462, 0.7796286979407650586 ) ) ;
#130965 = CARTESIAN_POINT ( 'NONE',  ( 1.364683531249988535, 3.676041667008087099, 0.7879004041258500513 ) ) ;
#130966 = CARTESIAN_POINT ( 'NONE',  ( 1.898125948304218547, -0.7631055018291610370, 2.129926759817270199 ) ) ;
#130967 = CARTESIAN_POINT ( 'NONE',  ( 3.985071343692931034, -0.2060594512321256011, -2.095964026187596918 ) ) ;
#130968 = CARTESIAN_POINT ( 'NONE',  ( -4.146814880933400005, 5.931313009212638931, 1.599625672291270506 ) ) ;
#130969 = CARTESIAN_POINT ( 'NONE',  ( 2.055556868256277259, 1.765410544359298894, -0.1243799924028898551 ) ) ;
#130970 = CARTESIAN_POINT ( 'NONE',  ( 5.991813822235618758, 9.077867661661846554, 1.199719254218462483 ) ) ;
#130972 = EDGE_CURVE ( 'NONE', #4829, #131029, #80684, .T. ) ;
#130971 = CARTESIAN_POINT ( 'NONE',  ( 5.194182247366878613, 6.192872389083746043, 1.082531754730549078 ) ) ;
#130973 = B_SPLINE_CURVE_WITH_KNOTS ( 'NONE', 3,
 ( #116674, #34294, #100367, #47386 ),
 .UNSPECIFIED., .F., .F.,
 ( 4, 4 ),
 ( 0.000000000000000000, 0.0002909236271752587821 ),
 .UNSPECIFIED. ) ;
#130974 = CARTESIAN_POINT ( 'NONE',  ( -6.274726165026268454, 6.214935368819085149, 0.7998128361456341429 ) ) ;
#130975 = CARTESIAN_POINT ( 'NONE',  ( 0.7499999999999885647, 2.816666666666689522, -1.299038105676658228 ) ) ;
#130976 = CARTESIAN_POINT ( 'NONE',  ( -0.004779673669230537214, -2.156333359934967220, -0.5329991086745686779 ) ) ;
#130977 = CARTESIAN_POINT ( 'NONE',  ( 3.996163734398257894, -0.6867376513691285655, -2.081127982183433645 ) ) ;
#130978 = CARTESIAN_POINT ( 'NONE',  ( -4.786191920824102830, 5.542644314838231168, 1.199719254218462483 ) ) ;
#130979 = CARTESIAN_POINT ( 'NONE',  ( 0.006158830626129450057, 7.078243236992583398, -2.121324627965403220 ) ) ;
#130980 = CARTESIAN_POINT ( 'NONE',  ( 6.586587867412674768, -1.305319418013479948, 1.671791285998667442 ) ) ;
#130981 = CARTESIAN_POINT ( 'NONE',  ( 1.364683531249990311, 3.384375000341416140, 1.214306433183764966E-14 ) ) ;
#130982 = CARTESIAN_POINT ( 'NONE',  ( -0.6823417656250003738, 8.401041667008064096, 1.181850606188754593 ) ) ;
#130983 = CARTESIAN_POINT ( 'NONE',  ( -4.772106882330247046, 4.669805572247793357, -0.7216878364870207285 ) ) ;
#130984 = CARTESIAN_POINT ( 'NONE',  ( 5.924112389714110805, -2.104401743431310923, 0.2612745606217213856 ) ) ;
#130985 = CARTESIAN_POINT ( 'NONE',  ( -6.211043768836215229, 8.339580045099285854, 1.443375672974064550 ) ) ;
#130986 = VERTEX_POINT ( 'NONE', #25932 ) ;
#130988 = CARTESIAN_POINT ( 'NONE',  ( 3.967488985650382549, 3.999290593069634081, -0.7827604779067200980 ) ) ;
#130987 = CARTESIAN_POINT ( 'NONE',  ( -4.177320726786315497, 7.887641591310407208, -0.7216878364870458196 ) ) ;
#130989 = CARTESIAN_POINT ( 'NONE',  ( 4.222474775652216294, 7.013638773981186958, 1.199719254218462483 ) ) ;
#130990 = CARTESIAN_POINT ( 'NONE',  ( 6.603072989126265391, -0.3962418105841297167, 1.804722624154910360 ) ) ;
#130991 = CARTESIAN_POINT ( 'NONE',  ( -5.599738924909661186, 5.745725798494749625, 0.2540040342395213369 ) ) ;
#130992 = CARTESIAN_POINT ( 'NONE',  ( 0.4682352675917088591, 6.596815194046603104, -3.429086925395263385 ) ) ;
#130993 = CARTESIAN_POINT ( 'NONE',  ( -1.364683531250010295, 4.342708333674753618, 0.7879004041258379498 ) ) ;
#130994 = CARTESIAN_POINT ( 'NONE',  ( 2.120290817172516551, 0.0009401564262049438847, 1.740626721131139698 ) ) ;
#130995 = DIRECTION ( 'NONE',  ( 0.000000000000000000, 0.000000000000000000, 1.000000000000000000 ) ) ;
#130997 = CARTESIAN_POINT ( 'NONE',  ( 0.5726126529861443881, 1.355618539282506640, -1.418395753018865113 ) ) ;
#130996 = AXIS2_PLACEMENT_3D ( 'NONE', #113323, #66582, #45074 ) ;
#130998 = CARTESIAN_POINT ( 'NONE',  ( -0.6823417656250246877, 0.3635416670080895973, 1.181850606188755259 ) ) ;
#130999 = CARTESIAN_POINT ( 'NONE',  ( -0.4032277238576692513, 3.019957635004392404, -0.4115402804778547363 ) ) ;
#131000 = CARTESIAN_POINT ( 'NONE',  ( 6.086834708314957432, -0.3123483334277510348, -2.138898144987111838 ) ) ;
#131001 = CARTESIAN_POINT ( 'NONE',  ( -9.110189153378817295, 12.71597221466224603, 1.199719254218462483 ) ) ;
#131002 = CARTESIAN_POINT ( 'NONE',  ( -7.361714222096077620, 7.691014135307965738, 0.7216878364870317197 ) ) ;
#131003 = CARTESIAN_POINT ( 'NONE',  ( 5.629794960336353071, -1.368038101806166029, -1.673757646710342550 ) ) ;
#131005 = ORIENTED_EDGE ( 'NONE', *, *, #48325, .F. ) ;
#131004 = CARTESIAN_POINT ( 'NONE',  ( -4.065465959251405081, 5.836405933916976707, -1.599625672291271394 ) ) ;
#131006 = CARTESIAN_POINT ( 'NONE',  ( 1.364683531249988535, 2.863541667008082658, 0.7879004041258500513 ) ) ;
#131007 = CARTESIAN_POINT ( 'NONE',  ( 5.606699263565281477, 1.494642942781895023, -1.285547057225975509 ) ) ;
#131008 = CARTESIAN_POINT ( 'NONE',  ( 5.114428339645875177, 0.5428861372157275378, -1.646692512460482982 ) ) ;
#131010 = CARTESIAN_POINT ( 'NONE',  ( 2.261505105119133052, 2.148611799745976381, -0.4309092228176118478 ) ) ;
#131009 = CARTESIAN_POINT ( 'NONE',  ( -1.360316468750040642, -0.3802083329919277999, -0.7853790794159161148 ) ) ;
#131011 = CARTESIAN_POINT ( 'NONE',  ( 3.171242727813221585, -2.131442559959194849, -0.8847066026466602340 ) ) ;
#131012 = CARTESIAN_POINT ( 'NONE',  ( 4.288392841435205938, -2.037809284099707074, -0.3060936983758227870 ) ) ;
#131013 = CARTESIAN_POINT ( 'NONE',  ( 1.025216207372595223, -1.231406509999972254, -1.501593997598904995 ) ) ;
#131014 = CARTESIAN_POINT ( 'NONE',  ( -4.731432421044865499, 8.463828891286912182, -0.7216878364870257245 ) ) ;
#131015 = CARTESIAN_POINT ( 'NONE',  ( -5.815521545619021460, 5.749472989502435460, -0.7998128361456362523 ) ) ;
#131016 = CARTESIAN_POINT ( 'NONE',  ( -5.608757509019071108, 5.629766575892905855, -0.3787719694710602325 ) ) ;
#131017 = CARTESIAN_POINT ( 'NONE',  ( 4.359710196644346780, -1.641147893522959089, -1.343014508298406628 ) ) ;
#131018 = CARTESIAN_POINT ( 'NONE',  ( 5.320709023819174099, 7.653582423498873410, -1.267626751378515326 ) ) ;
#131019 = CARTESIAN_POINT ( 'NONE',  ( 2.742814741689561853, 2.006446121045248887, -0.2004354718553730264 ) ) ;
#131020 = CARTESIAN_POINT ( 'NONE',  ( -5.761852095683518193, 6.784877535461274256, 1.082531754730546636 ) ) ;
#131021 = CARTESIAN_POINT ( 'NONE',  ( 5.016741729952475914, 1.524926965779101140, -1.595359541877178877 ) ) ;
#131022 = DIRECTION ( 'NONE',  ( 0.6507913734559640506, -0.7592566023653003482, 0.000000000000000000 ) ) ;
#131023 = B_SPLINE_CURVE_WITH_KNOTS ( 'NONE', 3,
 ( #188007, #40721, #7109, #59082, #75339, #106827, #156605, #172857, #90540, #58019, #141456, #39633, #124183, #190146, #173939, #207463, #125242, #191202, #100632, #166709, #87320, #153388, #192267, #160862, #80678, #27649, #92682, #29800, #12456, #130567, #43928, #42867, #26579, #111104, #113246, #179251, #158727, #30874, #127379, #60150, #62290, #112181, #10324, #146769, #212786, #126307, #128450, #177110, #11388, #46059, #28726, #64423, #76398, #14582, #142507, #208515, #93748, #95885, #94812, #108975, #161939, #194417, #210664, #78531, #110043, #77466, #193351, #178185, #176055, #96953, #195495, #144649, #174994, #13532, #159786, #143585, #163001, #209578, #44995, #145721, #61223, #79602, #211720, #63356, #129515, #47131, #69726, #183492, #32987, #67581, #149948, #50307, #81737, #165118, #132654, #35101, #99064, #1517, #102249, #182416, #166181, #117501, #133726, #196557, #48200, #100119, #147818, #17769, #444, #199732, #83858, #164069, #115371, #3647, #51378, #101172, #31931, #167261, #168323, #16710, #18846, #84931, #151020, #82795, #148869, #118566, #36172, #114312, #19918, #98013, #213837, #65455, #34046, #2587, #134780, #68657, #200789, #180311, #52440, #131605, #49250, #181363, #184551, #198658, #86003, #66512, #197606, #152077, #116425, #15648, #72935, #135830, #87066, #203986, #172600, #55633, #136899, #154209, #171514, #23108, #137965, #139039, #173685, #202928, #106573, #24179, #104395, #121789, #54570, #90282, #187756, #88139, #39385, #156351, #205064, #7935, #74024, #105481, #89223, #155276, #6856, #9013, #120718, #201855, #119636, #56706, #206140, #57771, #185620, #123932, #5779, #153138, #71858, #4712, #122873, #186691, #189900, #140114, #188834, #53499, #40470, #41542, #170442, #107656, #25261, #91362, #37252, #157422, #103322, #169384, #38319, #20969, #70786, #22030, #62050, #126054, #160607, #28472, #143331, #174750, #43679, #92437, #26323, #45813, #208268, #109798, #158476, #79358, #210408, #94564, #162759, #75089, #193097, #10076, #110852, #93497, #12209, #44746, #42614, #59901, #96710, #141201, #129273, #78280, #112994, #207212, #128205, #195246, #194166, #111933, #175805, #27397, #211471, #46882, #58836, #179007, #124991, #76152, #142256, #60971, #127127, #30621, #209324, #159537, #190950, #11135, #192016, #95640, #77212, #177935, #176859, #161691, #144408, #29548, #13285, #145476, #63105, #108724, #14333, #180063, #82541, #195, #184299, #134535, #66264, #67331, #17521, #149690, #165936, #52187, #81490, #199477, #51121, #197359, #132412, #147567, #117244, #198414, #181116, #50058, #183244, #163820, #116179, #118313, #213588, #64181, #1273, #182164, #102001, #15399, #80423, #212541, #148629, #84683, #150770, #130322, #2332, #33795, #65213, #68408, #167011, #35924, #97762, #99873, #83609, #49002, #133475, #34848, #146522, #196312, #200541, #47956, #114071, #131364, #100923, #18603, #31686, #115120, #32735, #98815, #164867, #16461, #172597, #23104, #105478, #187753, #58832, #6853, #56703, #39382, #92431, #9009, #107651, #175800, #88136, #206137, #171511, #123928, #106569, #173681, #57767, #72932, #109792, #157418, #25257, #137962, #91357, #59896, #122870, #124987, #174745, #71854, #189896, #203983, #155272, #154206, #90279, #188831, #41538, #75084, #26319, #74020, #140111, #158471, #10071, #141197, #5775 ),
 .UNSPECIFIED., .F., .F.,
 ( 4, 1, 1, 1, 1, 1, 1, 1, 1, 1, 1, 1, 1, 1, 1, 1, 1, 1, 1, 1, 1, 1, 1, 1, 1, 1, 1, 1, 1, 1, 1, 1, 1, 1, 1, 1, 1, 1, 1, 1, 1, 1, 1, 1, 1, 1, 1, 1, 1, 1, 1, 1, 1, 1, 1, 1, 1, 1, 1, 1, 1, 1, 1, 1, 1, 1, 1, 1, 1, 1, 1, 1, 1, 1, 1, 1, 1, 1, 1, 1, 1, 1, 1, 1, 1, 1, 1, 1, 1, 1, 1, 1, 1, 1, 1, 1, 1, 1, 1, 1, 1, 1, 1, 1, 1, 1, 1, 1, 1, 1, 1, 1, 1, 1, 1, 1, 1, 1, 1, 1, 1, 1, 1, 1, 1, 1, 1, 1, 1, 1, 1, 1, 1, 1, 1, 1, 1, 1, 1, 1, 1, 1, 1, 1, 1, 1, 1, 1, 1, 1, 1, 1, 1, 1, 1, 1, 1, 1, 1, 1, 1, 1, 1, 1, 1, 1, 1, 1, 1, 1, 1, 1, 1, 1, 1, 1, 1, 1, 1, 1, 1, 1, 1, 1, 1, 1, 1, 1, 1, 1, 1, 1, 1, 1, 1, 1, 1, 1, 1, 1, 1, 1, 1, 1, 1, 1, 1, 1, 1, 1, 1, 1, 1, 1, 1, 1, 1, 1, 1, 1, 1, 1, 1, 1, 1, 1, 1, 1, 1, 1, 1, 1, 1, 1, 1, 1, 1, 1, 1, 1, 1, 1, 1, 1, 1, 1, 1, 1, 1, 1, 1, 1, 1, 1, 1, 1, 1, 1, 1, 1, 1, 1, 1, 1, 1, 1, 1, 1, 1, 1, 1, 1, 1, 1, 1, 1, 1, 1, 1, 1, 1, 1, 1, 1, 1, 1, 1, 1, 1, 1, 1, 1, 1, 1, 1, 1, 1, 1, 1, 1, 1, 1, 1, 1, 1, 1, 1, 1, 1, 1, 1, 1, 1, 1, 1, 1, 1, 1, 1, 1, 1, 1, 1, 1, 1, 1, 1, 1, 1, 1, 1, 1, 1, 1, 1, 1, 1, 1, 1, 1, 1, 1, 1, 1, 1, 1, 1, 1, 1, 1, 1, 1, 1, 1, 1, 1, 1, 1, 1, 1, 1, 1, 1, 1, 1, 1, 1, 1, 1, 1, 1, 1, 1, 1, 1, 1, 1, 1, 1, 1, 1, 1, 1, 1, 4 ),
 ( 0.000000000000000000, 0.002599909708945224215, 0.005208776875251038344, 0.007813105021672143990, 0.01041684075506122895, 0.01302033053878596733, 0.01562516449037322508, 0.01822901888718816976, 0.02083333248856494152, 0.02343767784666880849, 0.02604151204071371642, 0.02864616705684025488, 0.03124974664057501156, 0.03385445107693609706, 0.03645811663825353210, 0.03906264587105176544, 0.04166673705245293319, 0.04427082116499847508, 0.04687535697974040683, 0.04947901875943551409, 0.05208372524935509645, 0.05468730636643894666, 0.05729195276349181160, 0.05989578571700067411, 0.06250012971910297310, 0.06510448174046053194, 0.06770830932160050442, 0.07031296016926287529, 0.07291653972921435800, 0.07552124384959360559, 0.07812490789241745281, 0.08072943556986492131, 0.08333352577934262373, 0.08593760861062926804, 0.08854214333088818167, 0.09114580385899402615, 0.09375050919907033931, 0.09635408915385039463, 0.09895873428887830281, 0.1015625661591952889, 0.1041669088510773916, 0.1067712598504420435, 0.1093750861808121810, 0.1119797359579501050, 0.1145833143474069837, 0.1171880172914337714, 0.1197916802446672702, 0.1223962066585842084, 0.1250002958591681090, 0.1276043774339237491, 0.1302089111537957367, 0.1328125705047451810, 0.1354172747579587832, 0.1380208536162275679, 0.1406254975582941213, 0.1432293284131295197, 0.1458336698625422867, 0.1484380199076493767, 0.1510418450546419100, 0.1536464938294531402, 0.1562500711155297428, 0.1588547729514310503, 0.1614584348822658832, 0.1640629601007041471, 0.1666670483599762276, 0.1692711287458052438, 0.1718756615333107141, 0.1744793197742946778, 0.1770840230088624179, 0.1796876008377196188, 0.1822922436549848091, 0.1848960735616705098, 0.1875004138364584350, 0.1901047629951247708, 0.1927085870260826783, 0.1953132348667029061, 0.1979168111164897881, 0.2005215119124719170, 0.2031251728880697216, 0.2057296969790492203, 0.2083337843645647058, 0.2109378636290424602, 0.2135423955521746908, 0.2161460527503557827, 0.2187507550344668650, 0.2213543319009846355, 0.2239589736615800464, 0.2265628026874214052, 0.2291671418554001027, 0.2317714901954165685, 0.2343753131776551424, 0.2369799601521939414, 0.2395835354327550959, 0.2421882352569974250, 0.2447918953444941648, 0.2473964183760076208, 0.2500005049552969649, 0.2526045831659717300, 0.2552091142926994904, 0.2578127705152143956, 0.2604174719170327390, 0.2630210478882585856, 0.2656256886602897938, 0.2682295168725681855, 0.2708338550015275126, 0.2734382025906618163, 0.2760420245914711468, 0.2786466707680146371, 0.2812502451463897990, 0.2838549440670474211, 0.2864586033335557724, 0.2890631253735708728, 0.2916672112141422968, 0.2942712884385379479, 0.2968758188368077477, 0.2994794741507696423, 0.3020841747384366283, 0.3046877498813952978, 0.3072923897329448151, 0.3098962171989202430, 0.3125005543566263810, 0.3151049012626256918, 0.3177087223492732204, 0.3203133677958864278, 0.3229169413390938770, 0.3255216394243000688, 0.3281252979369121969, 0.3307298190533745630, 0.3333339042227165261, 0.3359379805283350118, 0.3385425102660742369, 0.3411461647385755636, 0.3437508645802123675, 0.3463544389619092612, 0.3489590779610384774, 0.3515629047479519320, 0.3541672410021501904, 0.3567715872927431642, 0.3593754075324762653, 0.3619800523172059803, 0.3645836250922447341, 0.3671883224101137877, 0.3697919802359038166, 0.3723965004967392245, 0.3750005850623230885, 0.3776046605166471504, 0.3802091896617659783, 0.3828128433598806946, 0.3854175425235913388, 0.3880211162110140388, 0.3906257544257662473, 0.3932295806008425099, 0.3958339160192597128, 0.3984382617621595180, 0.4010420812222079689, 0.4036467254130849946, 0.4062502974869375283, 0.4088549941055670267, 0.4114586513115932598, 0.4140631707847102772, 0.4166672548139925825, 0.4192713294844879757, 0.4218758581048823730, 0.4244795110956688933, 0.4270842096495421902, 0.4296877827096635682, 0.4322924202080664635, 0.4348962458385162155, 0.4375005804888632555, 0.4401049257517701263, 0.4427087444993486054, 0.4453133881643903114, 0.4479169596040251111, 0.4505216555914985932, 0.4531253122448062887, 0.4557298309980991058, 0.4583339145585244578, 0.4609379885126426157, 0.4635425166761967808, 0.4661461690266998081, 0.4687508670388120247, 0.4713544395385928509, 0.4739590763886608604, 0.4765629015416836811, 0.4791672354916582388, 0.4817715803422617515, 0.4843753984445725025, 0.4869800416517858221, 0.4895836125241597725, 0.4921883079485492862, 0.4947919641161733773, 0.4973964822175238609, 0.5000005653765271507, 0.5026046386817077938, 0.5052091664562964324, 0.5078128182335502894, 0.5104175157719683664, 0.5130210877783591972, 0.5156257240480961457, 0.5182295487908826770, 0.5208338821081714975, 0.5234382266141532902, 0.5260420441383883983, 0.5286466869557716608, 0.5312502573278325979, 0.5338549522572011430, 0.5364586080061681805, 0.5390631255234488162, 0.5416672083484578293, 0.5442712810721315186, 0.5468758085256230084, 0.5494794597966533578, 0.5520841569294364648, 0.5546877285093810839, 0.5572923642667827471, 0.5598961886665174692, 0.5625005214187991376, 0.5651048656478350196, 0.5677086826611791315, 0.5703133251567252815, 0.5729168950954143247, 0.5755215895978186280, 0.5781252449951498340, 0.5807297619962258350, 0.5833338445546641937, 0.5859379167642547737, 0.5885424439645127181, 0.5911460947963396162, 0.5937507915915425372, 0.5963543628119793993, 0.5989589981250363904, 0.6015628222488997867, 0.6041671545038470592, 0.6067714985236103420, 0.6093753150932430529, 0.6119799573349418154, 0.6145835269071964202, 0.6171882210506893784, 0.6197918761634028106, 0.6223963927161352272, 0.6250004750754242222, 0.6276045468383509851, 0.6302090738532378777, 0.6328127243128783830, 0.6354174208385534595, 0.6380209917664191321, 0.6406256267031188445, 0.6432294506182901772, 0.6458337824435727015, 0.6484381263217364744, 0.6510419425148348260, 0.6536465845706755928, 0.6562501538434313275, 0.6588548476960643940, 0.6614585025911776661, 0.6640630187634258830, 0.6666671009909873602, 0.6692711723746683772, 0.6718756992720475996, 0.6744793494265174383, 0.6770840457507175669, 0.6796876164529486175, 0.6822922510812780006, 0.6848960748549377531, 0.6875004063182246217, 0.6901047501224634173, 0.6927085660062048955, 0.6953132079441787239, 0.6979167769843723779, 0.7005214706141982273, 0.7031251253587310623, 0.7057296412183544643, 0.7083337233816132672, 0.7109377944534676086, 0.7135423213012055399, 0.7161459712175226588, 0.7187506674083037339, 0.7213542379518396164, 0.7239588723397878400, 0.7265626960391206035, 0.7291670272080824633, 0.7317713710060759214, 0.7343751866476402324, 0.7369798285357428425, 0.7395833974103146469, 0.7421880908853900616, 0.7447917455463664016, 0.7473962611612280371, 0.7500003433276148934, 0.7526044141550642941, 0.7552089410210337528, 0.7578125907662203176, 0.7604172868916432293, 0.7630208573434285046, 0.7656254915589897347, 0.7682293152511859846, 0.7708336461934980344, 0.7734379900529331220, 0.7760418055195050790, 0.7786464474257392965, 0.7812500162016354777, 0.7838547095900232353, 0.7864583642344741277, 0.7890628796724428184, 0.7916669619093961163, 0.7942710325598689725, 0.7968755595119511037, 0.7994792091530360523, 0.8020839052811703507, 0.8046874757081575735, 0.8072921098193328593, 0.8098959335715922858, 0.8125002643549369408, 0.8151046083435100620, 0.8177084237022821389, 0.8203130656946604482, 0.8229166344388356702, 0.8255213278086077633, 0.8281249825035741363, 0.8307294978325265866, 0.8333335802074958165, 0.8359376507484286289, 0.8385421778545157911, 0.8411458274585372763, 0.8437505236574627254, 0.8463540941266142204, 0.8489587282014147140, 0.8515625520809478877, 0.8541668827730166669, 0.8567712269584367712, 0.8593750422766117669, 0.8619796844231587540, 0.8645832532025788941, 0.8671879466218186394, 0.8697916014343529678, 0.8723961167221769841, 0.8750001993026245151, 0.8776042698014647758, 0.8802087971294628721, 0.8828124467634709260, 0.8854171431012803906, 0.8880207136795719158, 0.8906253477860208712, 0.8932291718600525732, 0.8958335025285494302, 0.8984378469785403443, 0.9010416623233333810, 0.9036463046920883979, 0.9062498735737328781, 0.9088545671105374701, 0.9114582221077071056, 0.9140627374223044832, 0.9166668202757080053, 0.9192708907999164181, 0.9218754184177497812, 0.9244790681488107564, 0.9270837646936044285, 0.9296873354480212903, 0.9322919696541906998, 0.9348957939899811276, 0.9375001247025137596, 0.9401044694846933947, 0.9427082849236875228, 0.9453129275835465695, 0.9479164966330613229, 0.9505211903504858784, 0.9531248456066239161, 0.9557293610412391782, 0.9583334441921064206, 0.9609375147049603605, 0.9635420428945489224, 0.9661456931510739032, 0.9687503890924937799, 0.9713539588735070618, 0.9739585961357111188, 0.9765624261165479769, 0.9791667493207181217, 0.9817710620974646751, 0.9843748983037424738, 0.9869797303524157073, 0.9895832060093603388, 0.9921869237806116848, 0.9947912468131487884, 0.9974000922265050528, 0.9999999999999998890 ),
 .UNSPECIFIED. ) ;
#131024 = CARTESIAN_POINT ( 'NONE',  ( -7.846302513400014611, -6.700642373080271774, 7.709579522695861442 ) ) ;
#131025 = CARTESIAN_POINT ( 'NONE',  ( -7.449279056065764237, 7.655523418356991350, 0.7998128361456341429 ) ) ;
#131027 = CARTESIAN_POINT ( 'NONE',  ( 0.000000000000000000, -9.006862915010128035, 0.000000000000000000 ) ) ;
#131026 = CARTESIAN_POINT ( 'NONE',  ( -4.749858536263919184, 8.300932276130108534, 0.7929127856809523589 ) ) ;
#131028 = SURFACE_SIDE_STYLE ('',( #115835 ) ) ;
#131029 = VERTEX_POINT ( 'NONE', #172207 ) ;
#131030 = CARTESIAN_POINT ( 'NONE',  ( 4.539950165727339559, 0.8829098278404916567, -1.862335138179547211 ) ) ;
#131031 = CARTESIAN_POINT ( 'NONE',  ( -6.089020385868850305, 10.11795786024005572, -0.7216878364870338292 ) ) ;
#131032 = CARTESIAN_POINT ( 'NONE',  ( 0.3909723190919997537, -8.176244038173743789, 9.516020521605820903 ) ) ;
#131033 = CARTESIAN_POINT ( 'NONE',  ( -5.362413449404877852, 6.214902764849178141, -1.199719254218446718 ) ) ;
#131034 = CARTESIAN_POINT ( 'NONE',  ( 3.563153132451855054, -1.649810593967064865, 1.164694042050371303 ) ) ;
#131035 = CARTESIAN_POINT ( 'NONE',  ( 1.499999999999987566, -0.2249999999999821587, 0.000000000000000000 ) ) ;
#131036 = VECTOR ( 'NONE', #85181, 1000.000000000000000 ) ;
#131037 = CARTESIAN_POINT ( 'NONE',  ( 8.270110514656016321, 12.59228666716665401, 0.7216878364870438212 ) ) ;
#131038 = CARTESIAN_POINT ( 'NONE',  ( 6.608709811657416999, 9.797579649320619311, -1.199719254218440723 ) ) ;
#131039 = CARTESIAN_POINT ( 'NONE',  ( 3.080987681966301572, -0.1499786273361273514, -2.055480798767507444 ) ) ;
#131040 = CARTESIAN_POINT ( 'NONE',  ( 3.795362611133989095, 4.068874996780127873, 0.8733349908450734889 ) ) ;
#131041 = CARTESIAN_POINT ( 'NONE',  ( 6.003563092752934871, 5.898578451166879510, 0.7998128361456341429 ) ) ;
#131043 = EDGE_LOOP ( 'NONE', ( #61669, #91288, #197103, #97766, #186324 ) ) ;
#131042 = CARTESIAN_POINT ( 'NONE',  ( -0.1411974294642124317, 6.947781193150396994, -2.495311724135263809 ) ) ;
#131044 = CARTESIAN_POINT ( 'NONE',  ( 1.271164299617353333, 1.095269041189731452, 1.479763895647051353 ) ) ;
#131045 = CARTESIAN_POINT ( 'NONE',  ( 0.1359762249627448627, -2.107041879058098033, 0.9415998322012062438 ) ) ;
#131046 = CARTESIAN_POINT ( 'NONE',  ( 6.900173834712277632, 7.014900660111269559, -0.7998128361456341429 ) ) ;
#131047 = CARTESIAN_POINT ( 'NONE',  ( 3.145949958485740883, 0.7812230816454240889, -2.015650884352723882 ) ) ;
#131048 = AXIS2_PLACEMENT_3D ( 'NONE', #35895, #104113, #188548 ) ;
#131049 = CARTESIAN_POINT ( 'NONE',  ( -3.470524135418300737, 6.032400010421219427, -1.082531754730549967 ) ) ;
#131050 = CARTESIAN_POINT ( 'NONE',  ( 1.938685741270998797, -1.555697844595272716, 1.282991390469834458 ) ) ;
#131051 = EDGE_CURVE ( 'NONE', #114731, #157260, #188471, .T. ) ;
#131052 = CARTESIAN_POINT ( 'NONE',  ( 2.601245504928787700, 1.085180258111384077, -2.026094289238103752 ) ) ;
#131053 = CARTESIAN_POINT ( 'NONE',  ( 9.876669921572342990E-13, -7.246166700193024113, -9.500331257164619458 ) ) ;
#131054 = CARTESIAN_POINT ( 'NONE',  ( -0.3275477585932070057, 6.485062452714529080, 3.280083270285460983 ) ) ;
#131055 = CARTESIAN_POINT ( 'NONE',  ( 4.680523324745738734, -1.912062325676016306, -0.4798145647967356764 ) ) ;
#131056 = CARTESIAN_POINT ( 'NONE',  ( 4.592982591267942283, 1.756852934926198317, 0.9896879400849432074 ) ) ;
#131058 = CARTESIAN_POINT ( 'NONE',  ( 10.07334494482924292, 11.81495252613139257, -1.082531754730537088 ) ) ;
#131057 = CARTESIAN_POINT ( 'NONE',  ( -1.201851678989727383E-14, 3.946875000341423689, -1.575800808251660134 ) ) ;
#131060 = CARTESIAN_POINT ( 'NONE',  ( 5.725249284967181218, -0.05305106314347144553, 2.105570132020935237 ) ) ;
#131059 = CARTESIAN_POINT ( 'NONE',  ( -5.201524489137236529, 9.220195670635433771, 0.7998128361456481317 ) ) ;
#131061 = CARTESIAN_POINT ( 'NONE',  ( 6.057099581687969803, 1.694805161836069107, -1.188877858866774107 ) ) ;
#131062 = CARTESIAN_POINT ( 'NONE',  ( 4.821896187954575197, 8.777295985922343391, 0.7998128361456462443 ) ) ;
#131063 = CARTESIAN_POINT ( 'NONE',  ( -6.063521013809733518, 8.097193820909906137, 1.599625672291283607 ) ) ;
#131064 = CARTESIAN_POINT ( 'NONE',  ( 6.639320575229244348, 1.270172395628932360, 2.119701008677194132 ) ) ;
#131065 = CARTESIAN_POINT ( 'NONE',  ( 5.818619510638624703, -0.7308962487734929070, -1.883076464014792117 ) ) ;
#131066 = CARTESIAN_POINT ( 'NONE',  ( -0.7500000000000006661, 0.1395833340161536928, -1.299038105676652011 ) ) ;
#131067 = CARTESIAN_POINT ( 'NONE',  ( 2.913035970020665388, 1.671030660360285802, -1.591803581779531074 ) ) ;
#131068 = CARTESIAN_POINT ( 'NONE',  ( 1.745062578162811073, -0.2986309630071918853, -2.040702096407704058 ) ) ;
#131069 = CARTESIAN_POINT ( 'NONE',  ( 7.782016984564065432, 8.181367358187307204, 0.7216878364870458196 ) ) ;
#131070 = ADVANCED_FACE ( 'NONE', ( #9685 ), #189506, .T. ) ;
#131071 = CARTESIAN_POINT ( 'NONE',  ( 7.530627977747744062, 7.750430493652658015, -0.7998128361456341429 ) ) ;
#131072 = CARTESIAN_POINT ( 'NONE',  ( 5.794130544993763898, 7.853181283949808744, 1.599625672291269396 ) ) ;
#131073 = CARTESIAN_POINT ( 'NONE',  ( -1.364683531250000748, 0.5718750003414208027, 0.000000000000000000 ) ) ;
#131074 = CARTESIAN_POINT ( 'NONE',  ( 3.054329744828568227, 6.785411478933790264, 0.000000000000000000 ) ) ;
#131075 = CARTESIAN_POINT ( 'NONE',  ( 7.415946836550727284, 7.754285518838408109, 0.7216878364870317197 ) ) ;
#131077 = PRESENTATION_STYLE_ASSIGNMENT (( #41516 ) ) ;
#131076 = CARTESIAN_POINT ( 'NONE',  ( 4.615793470729397718, 0.4799340867196815741, -2.117318520224883205 ) ) ;
#131079 = CARTESIAN_POINT ( 'NONE',  ( 3.421284184235491743, -1.099380227797893905, -1.476844927387373163 ) ) ;
#131078 = CARTESIAN_POINT ( 'NONE',  ( -5.938108093105513241, 6.030140318152288792, 0.7216878364870317197 ) ) ;
#131080 = CARTESIAN_POINT ( 'NONE',  ( -1.201851678989727383E-14, 4.071875000341425022, 1.575800808251672791 ) ) ;
#131081 = CARTESIAN_POINT ( 'NONE',  ( 5.407841436338867602, -0.9846607899807978681, -1.957994596084790206 ) ) ;
#131082 = CARTESIAN_POINT ( 'NONE',  ( 7.301865417239311817, 14.53770032347495800, 9.470102474007479287 ) ) ;
#131083 = CARTESIAN_POINT ( 'NONE',  ( 6.139586942761116717, -1.633760600410700592, -1.565427815648293031 ) ) ;
#131084 = CARTESIAN_POINT ( 'NONE',  ( -5.796555320980813164, 6.214368590181693186, -1.006237437275556257 ) ) ;
#131085 = CARTESIAN_POINT ( 'NONE',  ( 5.098657496608274720, 7.938328561423579011, 1.202842226815619142 ) ) ;
#131086 = CARTESIAN_POINT ( 'NONE',  ( -4.299344108864949554, 8.030002203735486788, -0.7216878364870338292 ) ) ;
#131087 = CARTESIAN_POINT ( 'NONE',  ( 5.885648082108200896, 6.039213315313952002, 0.7216878364870328300 ) ) ;
#131088 = CARTESIAN_POINT ( 'NONE',  ( 6.919227944281516329, -0.1317407762830881124, 1.740281130587753688 ) ) ;
#131090 = CARTESIAN_POINT ( 'NONE',  ( 4.442045433088864570, -1.240138855636420567, -1.585653348822992026 ) ) ;
#131089 = AXIS2_PLACEMENT_3D ( 'NONE', #179375, #28848, #14706 ) ;
#131091 = CARTESIAN_POINT ( 'NONE',  ( 5.770966940911189447, 9.884545197705074671, -0.7998128361456291469 ) ) ;
#131092 = CARTESIAN_POINT ( 'NONE',  ( 2.696425475562960195, -2.100245048574858497, -0.1560501473716560672 ) ) ;
#131093 = CARTESIAN_POINT ( 'NONE',  ( 1.845192132668025176, 0.3254238344292461060, -1.887580106770263999 ) ) ;
#131094 = CARTESIAN_POINT ( 'NONE',  ( 4.196412238629597447, 4.854568018944682706, -1.199719254218452047 ) ) ;
#131095 = CARTESIAN_POINT ( 'NONE',  ( 2.840245056987787287, -1.014795158497614036, 1.687856822838776916 ) ) ;
#131096 = CARTESIAN_POINT ( 'NONE',  ( 0.6197280442463182215, -0.9970892369244135356, -1.582582228963416160 ) ) ;
#131097 = CARTESIAN_POINT ( 'NONE',  ( 0.9241798626423223251, 0.9638202082158978667, 1.708698881219716137 ) ) ;
#131099 = ORIENTED_EDGE ( 'NONE', *, *, #159943, .F. ) ;
#131098 = CARTESIAN_POINT ( 'NONE',  ( 0.6680393924826667496, 1.910109291395128972, -0.09634788558426229943 ) ) ;
#131100 = CARTESIAN_POINT ( 'NONE',  ( 5.504247177468186258, 6.484338464210099851, 1.082531754730558626 ) ) ;
#131101 = CARTESIAN_POINT ( 'NONE',  ( -0.6823417656250246877, 0.6135416670080897639, 1.181850606188755259 ) ) ;
#131102 = CARTESIAN_POINT ( 'NONE',  ( 11.43195036480942051, 12.44475503714742182, -3.649565797774410036 ) ) ;
#131103 = CARTESIAN_POINT ( 'NONE',  ( 6.783773228136841027, -6.684699857435559167, -6.634380643896355068 ) ) ;
#131104 = CARTESIAN_POINT ( 'NONE',  ( 6.737176827083626307, -0.09545985418329960837, -2.068160202195384656 ) ) ;
#131105 = VECTOR ( 'NONE', #31332, 1000.000000000000114 ) ;
#131106 = DIRECTION ( 'NONE',  ( 0.3162277660168376636, 0.9486832980505138790, 0.000000000000000000 ) ) ;
#131107 = CARTESIAN_POINT ( 'NONE',  ( 1.135311898753359472, -0.04898221611688948623, -2.069941200615910581 ) ) ;
#131108 = CARTESIAN_POINT ( 'NONE',  ( -0.7500000000000006661, 1.358333333333357151, -1.299038105676652011 ) ) ;
#131109 = CARTESIAN_POINT ( 'NONE',  ( 5.940443861082012944, 10.08226827123770697, 0.7998128361456462443 ) ) ;
#131110 = CARTESIAN_POINT ( 'NONE',  ( -6.991200766141138168, 11.30815132714001159, 0.7998128361456481317 ) ) ;
#131111 = CARTESIAN_POINT ( 'NONE',  ( 4.342354338126830804, 8.288106837781779035, -0.7998128361456381397 ) ) ;
#131112 = CARTESIAN_POINT ( 'NONE',  ( 5.233110275169113201, 1.959380141031796585, 0.8112103084707968925 ) ) ;
#131113 = CARTESIAN_POINT ( 'NONE',  ( 4.869313445963426190, 5.709895770826003414, 1.199719254218452935 ) ) ;
#131114 = CARTESIAN_POINT ( 'NONE',  ( -0.6823417656250212460, 0.8010416670080899859, 1.181850606188755259 ) ) ;
#131115 = ORIENTED_EDGE ( 'NONE', *, *, #3337, .F. ) ;
#131116 = CARTESIAN_POINT ( 'NONE',  ( 1.499999999999989120, 2.025000000000019895, 1.214306433183764966E-14 ) ) ;
#131118 = CARTESIAN_POINT ( 'NONE',  ( 5.196852952739813070, 4.957416621151553571, -0.7998128361456221525 ) ) ;
#131117 = CARTESIAN_POINT ( 'NONE',  ( 6.197705743426439540, -1.420020466879829302, -1.353909852041992767 ) ) ;
#131119 = CARTESIAN_POINT ( 'NONE',  ( 4.780624950969222020, -1.977747464269607347, 0.3905396900540994420 ) ) ;
#131120 = EDGE_CURVE ( 'NONE', #183827, #70986, #24863, .T. ) ;
#131121 = CARTESIAN_POINT ( 'NONE',  ( 3.397576204589338733, -1.886455135561039942, 0.3326623127566808447 ) ) ;
#131122 = CARTESIAN_POINT ( 'NONE',  ( 11.92619526913699701, 10.19999999999999929, -1.328859060402686199 ) ) ;
#131123 = CARTESIAN_POINT ( 'NONE',  ( 1.909981697816802049, -1.036543071415759298, -1.930953618257096993 ) ) ;
#131124 = CARTESIAN_POINT ( 'NONE',  ( 3.462029368274913477, 0.8381641302350505418, 1.672297462726477946 ) ) ;
#131125 = CARTESIAN_POINT ( 'NONE',  ( -1.402160292154681736E-14, -0.8812499993171809543, -1.732050807568870754 ) ) ;
#131126 = CARTESIAN_POINT ( 'NONE',  ( 4.693612458567416823, 1.876924737948972188, -0.7285200738881071336 ) ) ;
#131127 = CARTESIAN_POINT ( 'NONE',  ( -7.528855374290365887, 7.678086112960552434, -0.7998128361456291469 ) ) ;
#131129 = CARTESIAN_POINT ( 'NONE',  ( 5.448860601978118723, -1.914358274237770496, -0.9046119500179942152 ) ) ;
#131128 = CARTESIAN_POINT ( 'NONE',  ( -4.989037340148921196, 5.883260320670900434, 1.082531754730560403 ) ) ;
#131130 = FACE_OUTER_BOUND ( 'NONE', #42035, .T. ) ;
#131132 = CARTESIAN_POINT ( 'NONE',  ( -6.688968683495758683, 8.897159112202094988, -1.599625672291271394 ) ) ;
#131131 = CARTESIAN_POINT ( 'NONE',  ( 1.874669627338154454, -0.1056657526060876956, -2.088216114563210102 ) ) ;
#131134 = ORIENTED_EDGE ( 'NONE', *, *, #198698, .F. ) ;
#131133 = CARTESIAN_POINT ( 'NONE',  ( 0.4458014021226979207, 1.719615392401403708, 0.1342584403209358679 ) ) ;
#131135 = CARTESIAN_POINT ( 'NONE',  ( 7.124973419181436007, 8.271222729588529887, -1.199719254218446718 ) ) ;
#131136 = CARTESIAN_POINT ( 'NONE',  ( 3.834746474454188013E-15, 12.09375000068279604, 1.500000000000001554 ) ) ;
#131137 = CARTESIAN_POINT ( 'NONE',  ( 0.07804408512527075126, -9.997559919034475939, 9.579522898042023726 ) ) ;
#131138 = TOROIDAL_SURFACE ( 'NONE', #6421, 2.400000000000000355, 0.1000000000000000056 ) ;
#131139 = CARTESIAN_POINT ( 'NONE',  ( 0.000000000000000000, -1.399999999999998579, 0.000000000000000000 ) ) ;
#131141 = CARTESIAN_POINT ( 'NONE',  ( 8.554831740098649107, 11.96409221588171157, 1.082531754730546636 ) ) ;
#131140 = CARTESIAN_POINT ( 'NONE',  ( 4.971035877704902184, 8.951292290631053916, 1.040834085586084257E-14 ) ) ;
#131143 = CARTESIAN_POINT ( 'NONE',  ( 1.242487904981701252, 1.745646600027310980, 0.4836494453460266074 ) ) ;
#131142 = CARTESIAN_POINT ( 'NONE',  ( 7.028976294042106332, 7.165170195996068969, 0.000000000000000000 ) ) ;
#131144 = CARTESIAN_POINT ( 'NONE',  ( -8.044065211609668253, 8.279164256499745633, 0.7998128361456602331 ) ) ;
#131145 = CARTESIAN_POINT ( 'NONE',  ( 4.436542580169809291, 6.199052314996659874, 1.599625672291267398 ) ) ;
#131146 = CARTESIAN_POINT ( 'NONE',  ( 5.417364897112183719, 8.477953592343014932, 1.199719254218451159 ) ) ;
#131147 = CARTESIAN_POINT ( 'NONE',  ( 6.539320575229256249, 4.699150603835311912, 2.459441311396874941 ) ) ;
#131148 = CARTESIAN_POINT ( 'NONE',  ( 0.7500000000000006661, 9.166666666666669627, -1.299038105676657340 ) ) ;
#131149 = CARTESIAN_POINT ( 'NONE',  ( 4.012968703617612931, 7.577496623363801476, 0.2782505873175616373 ) ) ;
#131150 = CARTESIAN_POINT ( 'NONE',  ( 9.246297574839974942, 11.81043314211192019, 1.443375672974076540 ) ) ;
#131151 = CARTESIAN_POINT ( 'NONE',  ( 2.681907113330802339, -1.068898278170841598, -1.523273593526828673 ) ) ;
#131152 = AXIS2_PLACEMENT_3D ( 'NONE', #129267, #142249, #195239 ) ;
#131153 = CARTESIAN_POINT ( 'NONE',  ( 0.2806859451011362583, 1.592165405827509650, -1.064819009530016958 ) ) ;
#131154 = CARTESIAN_POINT ( 'NONE',  ( 6.651400849050447484, -1.547811450530303778, -1.146644766597894938 ) ) ;
#131155 = CARTESIAN_POINT ( 'NONE',  ( 5.934052368846653991, 1.230181698326970663, 1.665117723180092213 ) ) ;
#131156 = CARTESIAN_POINT ( 'NONE',  ( 4.637820276784100137, 8.319831082953612622, -0.4078742439591088731 ) ) ;
#131157 = CARTESIAN_POINT ( 'NONE',  ( 0.000000000000000000, 0.000000000000000000, 0.000000000000000000 ) ) ;
#131158 = DIRECTION ( 'NONE',  ( 0.2684563758389304500, 5.821219718043054220E-15, 0.9632918427306581544 ) ) ;
#131159 = CARTESIAN_POINT ( 'NONE',  ( 9.910647101909615841, 10.66476916175714607, 0.000000000000000000 ) ) ;
#131160 = CARTESIAN_POINT ( 'NONE',  ( 4.592606226310515183, 1.930599660924517957, 0.3882996684868595394 ) ) ;
#131161 = CARTESIAN_POINT ( 'NONE',  ( 1.752743329737327826, 2.097873456429504735, 0.3079802404963858931 ) ) ;
#131162 = CARTESIAN_POINT ( 'NONE',  ( -5.850506979496850057, 6.784345216623154151, -1.199719254218446718 ) ) ;
#131163 = CARTESIAN_POINT ( 'NONE',  ( -11.04635347860243932, 7.050416898779586106, 4.576031291579900184 ) ) ;
#131165 = EDGE_CURVE ( 'NONE', #41470, #133393, #56564, .T. ) ;
#131164 = CARTESIAN_POINT ( 'NONE',  ( 9.479415819240319507, -6.570271182191715020, -0.2417854191286350762 ) ) ;
#131166 = CARTESIAN_POINT ( 'NONE',  ( 6.404242042726283834, 1.626525233829802408, -1.468802942141099299 ) ) ;
#131167 = DIRECTION ( 'NONE',  ( 0.6507913734559627184, 0.7592566023653016805, 0.000000000000000000 ) ) ;
#131168 = CARTESIAN_POINT ( 'NONE',  ( 4.225552302291880835, -1.843726210754624173, 0.5582998813679838079 ) ) ;
#131169 = CARTESIAN_POINT ( 'NONE',  ( -6.181627972826976958, 9.299317504018391745, 1.199719254218452047 ) ) ;
#131170 = CARTESIAN_POINT ( 'NONE',  ( -1.500000000000022204, 6.120000000000041851, 2.500000000000011102 ) ) ;
#131171 = CARTESIAN_POINT ( 'NONE',  ( 0.6982365061397632910, -0.7907169553198112322, 2.060542492664858560 ) ) ;
#131172 = CARTESIAN_POINT ( 'NONE',  ( -6.158576598851958295, 6.984695343647041810, 0.9239717604232693393 ) ) ;
#131173 = CARTESIAN_POINT ( 'NONE',  ( 4.232369794311310053E-13, -9.350066838357705024, 9.500000000000001776 ) ) ;
#131174 = VERTEX_POINT ( 'NONE', #109405 ) ;
#131175 =( LENGTH_UNIT ( ) NAMED_UNIT ( * ) SI_UNIT ( .MILLI., .METRE. ) );
#131176 = ORIENTED_EDGE ( 'NONE', *, *, #86952, .F. ) ;
#131177 = CARTESIAN_POINT ( 'NONE',  ( 6.420757345757475143, -1.395243968761919362, 1.390232514205336001 ) ) ;
#131178 = CARTESIAN_POINT ( 'NONE',  ( 1.065847985493496797, -1.230715344637549391, 1.502334450403658206 ) ) ;
#131179 = CARTESIAN_POINT ( 'NONE',  ( 6.380222486609858912, -0.2913964880489598452, 2.279815279960105467 ) ) ;
#131181 = CARTESIAN_POINT ( 'NONE',  ( 4.908966729185230804, -1.496192014157717631, 1.106395937811145203 ) ) ;
#131180 = CARTESIAN_POINT ( 'NONE',  ( -7.605197822622922210, 7.837428646007010613, -0.7998128361456362523 ) ) ;
#131182 = CARTESIAN_POINT ( 'NONE',  ( 4.929271367020211514, 7.908511140569038922, 1.199719254218452047 ) ) ;
#131184 = ADVANCED_FACE ( 'NONE', ( #175411 ), #26994, .F. ) ;
#131183 = DIRECTION ( 'NONE',  ( -0.000000000000000000, -1.000000000000000000, 0.000000000000000000 ) ) ;
#131185 = DIRECTION ( 'NONE',  ( -1.000000000000000000, 0.000000000000000000, 0.000000000000000000 ) ) ;
#131186 = CARTESIAN_POINT ( 'NONE',  ( -6.742482464697739708, 6.760651051769146491, 0.7998128361456341429 ) ) ;
#131187 = CARTESIAN_POINT ( 'NONE',  ( -4.990809943606294929, 4.995235487061662205, -0.7216878364870338292 ) ) ;
#131188 = CARTESIAN_POINT ( 'NONE',  ( 1.452940684028160234, -1.882004992133184285, -1.122693704575933316 ) ) ;
#131189 = CARTESIAN_POINT ( 'NONE',  ( 4.528060117284229413, 7.266191989264828344, 1.082531754730558626 ) ) ;
#131190 = AXIS2_PLACEMENT_3D ( 'NONE', #67522, #66456, #69664 ) ;
#131191 = CARTESIAN_POINT ( 'NONE',  ( 4.344593448898664693E-13, 13.36537488277823371, -1.375075632470054154 ) ) ;
#131192 = DIRECTION ( 'NONE',  ( 1.000000000000000000, 0.000000000000000000, 0.000000000000000000 ) ) ;
#131193 = CARTESIAN_POINT ( 'NONE',  ( 1.488595654847742145, -0.2661386877833261111, -1.806066791206423439 ) ) ;
#131194 = CARTESIAN_POINT ( 'NONE',  ( -1.387358672534711346, 7.251968950353628429, 4.302625267138136422 ) ) ;
#131195 = CARTESIAN_POINT ( 'NONE',  ( -6.392190997713585787, 6.905894197498253284, -0.8087526810517248199 ) ) ;
#131196 = CARTESIAN_POINT ( 'NONE',  ( 6.509000000000013664, 7.052434016701248254, 2.698154332336550887 ) ) ;
#131197 = CARTESIAN_POINT ( 'NONE',  ( 8.727698198895078363, 11.20540053684285553, -1.599625672291257406 ) ) ;
#131198 = CARTESIAN_POINT ( 'NONE',  ( 6.516225534515442952, -0.8655890497146904172, -1.607451055071248636 ) ) ;
#131199 = CARTESIAN_POINT ( 'NONE',  ( 4.680490258543752446, 1.210089798712219000, -1.543956201849092436 ) ) ;
#131200 = CARTESIAN_POINT ( 'NONE',  ( -8.552495972122143186, 8.872333477097637200, 0.7998128361456462443 ) ) ;
#131201 = CARTESIAN_POINT ( 'NONE',  ( 7.311924916471702396, 7.425000578838787391, -0.7998128361456281477 ) ) ;
#131202 = CARTESIAN_POINT ( 'NONE',  ( 4.195009555701286530, 1.760677850468267414, 1.304791629949946019 ) ) ;
#131203 = ADVANCED_FACE ( 'NONE', ( #154886 ), #6470, .F. ) ;
#131204 = CARTESIAN_POINT ( 'NONE',  ( 6.609000000000038177, 2.443064466336189788, 2.382833824652215160 ) ) ;
#131205 = CARTESIAN_POINT ( 'NONE',  ( 2.448173108494243078, -0.8891298726186761536, 1.869765896676472083 ) ) ;
#131207 = CARTESIAN_POINT ( 'NONE',  ( 1.364683531249986537, 1.467708333674748289, -0.7879004041258239610 ) ) ;
#131206 = CARTESIAN_POINT ( 'NONE',  ( 11.94105721237523277, 19.00000000000000000, -1.187919463087249827 ) ) ;
#131208 = ORIENTED_EDGE ( 'NONE', *, *, #57012, .T. ) ;
#131209 = CARTESIAN_POINT ( 'NONE',  ( 3.375889859521400194, -0.4501408176796182770, -2.254053602989118499 ) ) ;
#131210 = CARTESIAN_POINT ( 'NONE',  ( 8.785320351975350661, 9.351887953500479966, -0.7216878364870197293 ) ) ;
#131212 = CARTESIAN_POINT ( 'NONE',  ( 1.642778471875001811, -0.6927083328553753638, 2.845375778867859751 ) ) ;
#131211 = CARTESIAN_POINT ( 'NONE',  ( 7.200788982633824276, 7.573544365927161515, 0.000000000000000000 ) ) ;
#131213 = CARTESIAN_POINT ( 'NONE',  ( 6.720655732516652492, 7.053303974100803231, 2.424416723604695179 ) ) ;
#131214 = CARTESIAN_POINT ( 'NONE',  ( -9.976780902586998678, 4.600322429387547984, -6.670003923370737553 ) ) ;
#131215 = CARTESIAN_POINT ( 'NONE',  ( 3.380740619721524620, 1.755215216048062521, -0.8311813869739079763 ) ) ;
#131216 = EDGE_LOOP ( 'NONE', ( #116702, #13340, #11721, #115490 ) ) ;
#131217 = CARTESIAN_POINT ( 'NONE',  ( 5.178851490740205676, 6.104710163027444736, 1.082531754730558626 ) ) ;
#131218 = CARTESIAN_POINT ( 'NONE',  ( 3.673993457511487204, 1.897360377298975553, -0.2389773157873422427 ) ) ;
#131219 = CARTESIAN_POINT ( 'NONE',  ( -3.231779075379149546, 6.036511184309971689, -0.9899555337401846344 ) ) ;
#131220 = CARTESIAN_POINT ( 'NONE',  ( 5.262619041473771020, -1.246969283750315460, 1.191858809209481285 ) ) ;
#131221 = CARTESIAN_POINT ( 'NONE',  ( 3.907435596788138010, -1.928258004016227378, 0.5899861904685861358 ) ) ;
#131222 = CARTESIAN_POINT ( 'NONE',  ( 4.764420831138592938, 2.145307606383870969, -0.8259888504972175971 ) ) ;
#131223 = CARTESIAN_POINT ( 'NONE',  ( 11.41381675112460847, 12.56983264508522602, 3.704697986577264235 ) ) ;
#131224 = CARTESIAN_POINT ( 'NONE',  ( 0.2587985324217950689, 0.8487602207661277820, 2.037339956011212649 ) ) ;
#131225 = CARTESIAN_POINT ( 'NONE',  ( -5.980555157403903976, 6.149938236492225485, 0.000000000000000000 ) ) ;
#131226 = CARTESIAN_POINT ( 'NONE',  ( 5.923074920120706466, -0.04171666621876138348, 1.769427632397130079 ) ) ;
#131228 = CARTESIAN_POINT ( 'NONE',  ( 1.992491592054939531, -0.6139151001693385901, -2.208460184710277385 ) ) ;
#131227 = CARTESIAN_POINT ( 'NONE',  ( 7.035755370848908896, 7.173079118937375931, 0.7998128361456352531 ) ) ;
#131229 = CARTESIAN_POINT ( 'NONE',  ( 0.7787878715554141795, 1.165832476461704292, 1.292284986363402055 ) ) ;
#131230 =( LENGTH_UNIT ( ) NAMED_UNIT ( * ) SI_UNIT ( .MILLI., .METRE. ) );
#131231 = CARTESIAN_POINT ( 'NONE',  ( -4.625266680917477835, 5.425174544939014964, -1.199719254218453823 ) ) ;
#131232 = CARTESIAN_POINT ( 'NONE',  ( -0.6801582343750316451, 0.2135416670080853008, 1.178068619123807004 ) ) ;
#131233 = CARTESIAN_POINT ( 'NONE',  ( -11.97929049433705373, 13.88000000000000078, -0.7046979865771821894 ) ) ;
#131234 = CARTESIAN_POINT ( 'NONE',  ( 1.820994678651502330, -1.536134449795123480, 1.534618252339227329 ) ) ;
#131235 = CARTESIAN_POINT ( 'NONE',  ( 1.885954221117658092, -2.015980662343511032, 0.05432778586660082232 ) ) ;
#131236 = AXIS2_PLACEMENT_3D ( 'NONE', #213188, #178587, #194818 ) ;
#131237 = CARTESIAN_POINT ( 'NONE',  ( 0.7499999999999867883, 0.09791666734948467621, -1.299038105676652899 ) ) ;
#131238 = CARTESIAN_POINT ( 'NONE',  ( 5.285741052758629266, 1.295255816434317753, 1.426247342039884014 ) ) ;
#131239 = EDGE_CURVE ( 'NONE', #173465, #162142, #39238, .T. ) ;
#131240 = CARTESIAN_POINT ( 'NONE',  ( -1.364683531250010295, 13.63020833367473017, 0.7879004041258445001 ) ) ;
#131241 = CARTESIAN_POINT ( 'NONE',  ( 2.426306324659221136, -2.196553987802750907, 0.3307981192552343352 ) ) ;
#131242 = ORIENTED_EDGE ( 'NONE', *, *, #19314, .T. ) ;
#131243 = CARTESIAN_POINT ( 'NONE',  ( -9.578659721986371167, -9.971093151297267809, 0.1384029864568004642 ) ) ;
#131244 = CARTESIAN_POINT ( 'NONE',  ( -1.500000000000013101, -0.3291666666666463459, 0.8660254037844403729 ) ) ;
#131245 = CARTESIAN_POINT ( 'NONE',  ( 8.367353357928214663, 12.91366268422496688, 1.040834085586084257E-14 ) ) ;
#131246 = SURFACE_STYLE_USAGE ( .BOTH. , #180989 ) ;
#131247 = CARTESIAN_POINT ( 'NONE',  ( -5.817856928050925802, 5.960123635580414359, -1.359047942450207100E-08 ) ) ;
#131248 = CARTESIAN_POINT ( 'NONE',  ( 5.108843383178156117, -0.2480618215125965365, 1.722539690991312877 ) ) ;
#131249 = CARTESIAN_POINT ( 'NONE',  ( 3.965250677406896962, 1.681448970545707855, 1.010551734412237668 ) ) ;
#131251 = CARTESIAN_POINT ( 'NONE',  ( -7.727784370109414880, 8.118095974656867497, 0.7216878364870578100 ) ) ;
#131250 = CARTESIAN_POINT ( 'NONE',  ( 3.147464216666835402, 6.823792019419957278, -0.7998128361456291469 ) ) ;
#131252 = CARTESIAN_POINT ( 'NONE',  ( -1.467639082483196855, 4.376379912524843263, 0.3198401300024801830 ) ) ;
#131253 = CARTESIAN_POINT ( 'NONE',  ( 4.622535034725678393, 1.396675434457357756, -1.779734664907887343 ) ) ;
#131254 = CARTESIAN_POINT ( 'NONE',  ( 1.012259994385706019, 2.060384570222949741, -0.09942193159017187476 ) ) ;
#131255 = CARTESIAN_POINT ( 'NONE',  ( -6.826694039680798021, 7.923230120171105284, -1.199719254218446718 ) ) ;
#131256 = CARTESIAN_POINT ( 'NONE',  ( -4.744990574658554117, 4.638169879964154418, 1.214306433183764966E-14 ) ) ;
#131257 = CARTESIAN_POINT ( 'NONE',  ( 2.395744609331447172, 1.748901261223069437, 1.435362524944477025 ) ) ;
#131258 = ORIENTED_EDGE ( 'NONE', *, *, #65459, .F. ) ;
#131259 = CARTESIAN_POINT ( 'NONE',  ( -1.500000000000013101, 0.9520833340161557468, 0.8660254037844403729 ) ) ;
#131260 = CARTESIAN_POINT ( 'NONE',  ( 2.389737607000471442, -0.8038258883538218491, 1.689183408448757362 ) ) ;
#131261 = CARTESIAN_POINT ( 'NONE',  ( 1.845948222207854483, 0.2957656664513158007, -1.708526460754287157 ) ) ;
#131262 = CARTESIAN_POINT ( 'NONE',  ( 5.196902890030515643, 1.791362914573800369, 1.262263373074036688 ) ) ;
#131263 = CARTESIAN_POINT ( 'NONE',  ( 0.1830476545506658226, -2.141193618969746471, -0.5335393285625378290 ) ) ;
#131264 = CARTESIAN_POINT ( 'NONE',  ( 3.696290335837215668, -2.159122111672501454, -0.1082323872379290647 ) ) ;
#131265 = CARTESIAN_POINT ( 'NONE',  ( 4.136618238866495822, -1.688923885309162376, 0.9583718017313649362 ) ) ;
#131266 = CARTESIAN_POINT ( 'NONE',  ( -3.673896439178936824, 5.309298483840612093, 1.443375672974064550 ) ) ;
#131267 = CARTESIAN_POINT ( 'NONE',  ( 0.000000000000000000, -5.166862915010145052, 0.000000000000000000 ) ) ;
#131268 = CARTESIAN_POINT ( 'NONE',  ( 0.5312500000000220934, -0.7852924748305555314, -1.895863743164076576 ) ) ;
#131269 = CARTESIAN_POINT ( 'NONE',  ( 3.998873522394119195, 7.597518543056763995, -0.1390531931140040478 ) ) ;
#131270 = CARTESIAN_POINT ( 'NONE',  ( -0.1048463755018592264, -0.8645036352170620830, -1.819965476435807306 ) ) ;
#131271 = CARTESIAN_POINT ( 'NONE',  ( -3.956095110007851991E-14, 2.328125000341396689, -1.570758158831800255 ) ) ;
#131272 = CARTESIAN_POINT ( 'NONE',  ( 5.203750078570229753, 1.864167652161516031, 0.7691231355932278690 ) ) ;
#131273 = CARTESIAN_POINT ( 'NONE',  ( -8.967828540435322182, 12.54988483289483980, 1.199719254218462483 ) ) ;
#131274 = CARTESIAN_POINT ( 'NONE',  ( 8.606728586576791074, 8.935604860628076906, 0.7998128361456462443 ) ) ;
#131275 = CARTESIAN_POINT ( 'NONE',  ( 3.203469434578891661, 6.959407783642502565, -0.7998128361456362523 ) ) ;
#131277 = CYLINDRICAL_SURFACE ( 'NONE', #109121, 0.08000000000000020983 ) ;
#131276 = CARTESIAN_POINT ( 'NONE',  ( 2.262075381241589245, 0.7800679334904643270, 1.650788133108482825 ) ) ;
#131278 = DIRECTION ( 'NONE',  ( 0.000000000000000000, 0.000000000000000000, 1.000000000000000000 ) ) ;
#131279 = CARTESIAN_POINT ( 'NONE',  ( -1.807185592549641395, 2.518115318451403795, 2.500000000000000444 ) ) ;
#131280 = ORIENTED_EDGE ( 'NONE', *, *, #127420, .T. ) ;
#131281 = CARTESIAN_POINT ( 'NONE',  ( -5.953438849732214599, 6.118302544208584770, 0.7216878364870257245 ) ) ;
#131282 = UNCERTAINTY_MEASURE_WITH_UNIT (LENGTH_MEASURE( 1.000000000000000082E-05 ), #177501, 'distance_accuracy_value', 'NONE');
#131283 = CARTESIAN_POINT ( 'NONE',  ( 1.642778471875000035, -3.463541666188708845, -2.845375778867859751 ) ) ;
#131284 = CARTESIAN_POINT ( 'NONE',  ( -9.481229494658258261, 9.955855920056455588, -0.7998128361456291469 ) ) ;
#131285 = CARTESIAN_POINT ( 'NONE',  ( 6.586581121665559202, -1.240835222743674526, 1.594039115436784337 ) ) ;
#131286 = CARTESIAN_POINT ( 'NONE',  ( 0.9266185682500321930, -0.9568284065921551784, -1.892426592148554132 ) ) ;
#131287 = EDGE_LOOP ( 'NONE', ( #58344, #135804, #133400, #26968 ) ) ;
#131288 = CARTESIAN_POINT ( 'NONE',  ( -5.692444392891315097, 7.734547439830227411, -1.599625672291271394 ) ) ;
#131289 = CARTESIAN_POINT ( 'NONE',  ( 3.680148631105580215, 6.380924938676771241, -1.199719254218446718 ) ) ;
#131290 = CARTESIAN_POINT ( 'NONE',  ( 6.209851105358469958, -2.045643633555578766, 0.2495701479476707119 ) ) ;
#131291 = CARTESIAN_POINT ( 'NONE',  ( 5.115861365725079324, 0.1511377038382749338, 2.010826595755777824 ) ) ;
#131292 = EDGE_LOOP ( 'NONE', ( #52247, #127346, #112562, #177895 ) ) ;
#131293 = CARTESIAN_POINT ( 'NONE',  ( -8.971744963941075568, 11.49012176272984931, 1.599625672291269396 ) ) ;
#131294 = CARTESIAN_POINT ( 'NONE',  ( -0.4500000000000302647, 3.949999999999953548, 0.4999999999999553690 ) ) ;
#131296 = ORIENTED_EDGE ( 'NONE', *, *, #18560, .F. ) ;
#131295 = CARTESIAN_POINT ( 'NONE',  ( -5.607179047703544583, 8.699403434699558346, 1.199719254218454489 ) ) ;
#131297 = CARTESIAN_POINT ( 'NONE',  ( 6.440439394220377700, 6.875545743132385645, 0.7017714770480776298 ) ) ;
#131298 = CARTESIAN_POINT ( 'NONE',  ( 5.501327308730313170, 1.985796898448642933, 0.3474119236192701465 ) ) ;
#131299 = CARTESIAN_POINT ( 'NONE',  ( 4.523293815724619193, -1.134750198001058585, -1.449786353205910538 ) ) ;
#131300 = CARTESIAN_POINT ( 'NONE',  ( -0.02319159430949797526, 7.629137130509074716, -2.410989586153565067 ) ) ;
#131301 = CARTESIAN_POINT ( 'NONE',  ( 3.141587237543626454, -2.035091569058588679, 1.088060180353218165 ) ) ;
#131302 = CARTESIAN_POINT ( 'NONE',  ( 5.169401708560450004, 9.252995436621013425, 0.000000000000000000 ) ) ;
#131303 = CARTESIAN_POINT ( 'NONE',  ( 6.468072252983536607, 1.105043713804385153, 1.857642994352682653 ) ) ;
#131304 = CARTESIAN_POINT ( 'NONE',  ( 6.283314124929436417, 9.417951348137970413, -1.199719254218440723 ) ) ;
#131305 = CARTESIAN_POINT ( 'NONE',  ( 1.645936167706591569, 0.6108386606893880799, 1.843543891229272313 ) ) ;
#131306 = CARTESIAN_POINT ( 'NONE',  ( -2.761056838677368397, 6.372983411765559048, 0.7998128361456341429 ) ) ;
#131307 = ORIENTED_EDGE ( 'NONE', *, *, #8949, .F. ) ;
#131308 = EDGE_CURVE ( 'NONE', #84713, #125323, #63362, .T. ) ;
#131309 = AXIS2_PLACEMENT_3D ( 'NONE', #14076, #162506, #80166 ) ;
#131310 = DIRECTION ( 'NONE',  ( 0.000000000000000000, 1.000000000000000000, 0.000000000000000000 ) ) ;
#131311 = CARTESIAN_POINT ( 'NONE',  ( -3.305155586681401303, 7.078041627762083898, 0.7998128361456352531 ) ) ;
#131312 = CARTESIAN_POINT ( 'NONE',  ( 3.221420234344949840, -1.803205065257794004, 0.4975683872451354683 ) ) ;
#131315 = CARTESIAN_POINT ( 'NONE',  ( -4.938913097128142304, 8.984092056616635347, -0.7998128361456362523 ) ) ;
#131314 = CARTESIAN_POINT ( 'NONE',  ( -1.402160292154681736E-14, 0.8687500006828192678, -1.732050807568863648 ) ) ;
#131313 = CARTESIAN_POINT ( 'NONE',  ( 1.670022949053862948, 1.907054940702714863, -0.1439945843566131367 ) ) ;
#131316 = CARTESIAN_POINT ( 'NONE',  ( 2.491098823239074278, -0.3784457004711218042, -2.174036671264235387 ) ) ;
#131317 = CARTESIAN_POINT ( 'NONE',  ( 6.883263157960366918, 3.696842586722656865, 2.460469087180997327 ) ) ;
#131318 = CARTESIAN_POINT ( 'NONE',  ( 6.821160681006788629, 8.091013894996997635, 1.082531754730549967 ) ) ;
#131319 = CARTESIAN_POINT ( 'NONE',  ( -4.485049888022365927, 4.126979712314507331, 0.7998128361456341429 ) ) ;
#131320 = CARTESIAN_POINT ( 'NONE',  ( -6.658462837642833421, 8.861568958707010779, 1.443375672974064550 ) ) ;
#131321 = CARTESIAN_POINT ( 'NONE',  ( 1.106637804720354668, 1.495658270405418877, -1.284366697391533529 ) ) ;
#131322 = CARTESIAN_POINT ( 'NONE',  ( 0.8510977523443744586, 0.6731378975963157041, 2.207243034677327298 ) ) ;
#131323 = CARTESIAN_POINT ( 'NONE',  ( 1.135121963537696566, -0.04462593873827064989, -1.961518378280776354 ) ) ;
#131324 = CARTESIAN_POINT ( 'NONE',  ( 5.295784840496287060, -1.454754056633072778, -1.462402424637335052 ) ) ;
#131325 = CARTESIAN_POINT ( 'NONE',  ( 3.863710590214593399, 7.451486755318259547, 1.040834085586084257E-14 ) ) ;
#131326 = CARTESIAN_POINT ( 'NONE',  ( 5.071631979963703962, 8.074598522336444262, 1.199719254218451159 ) ) ;
#131327 = ORIENTED_EDGE ( 'NONE', *, *, #133268, .T. ) ;
#131328 = CARTESIAN_POINT ( 'NONE',  ( -0.6823417656250212460, 4.863541667008086655, 1.181850606188767472 ) ) ;
#131329 = CARTESIAN_POINT ( 'NONE',  ( -4.932336382548663245, 4.883384536077152838, 0.5336735327908896931 ) ) ;
#131330 = CARTESIAN_POINT ( 'NONE',  ( 3.158686601859607368, 6.628958768904106513, -0.7216878364870267237 ) ) ;
#131331 = CARTESIAN_POINT ( 'NONE',  ( 0.9894204570943666566, 0.1578702891864954827, 2.165348367497366144 ) ) ;
#131332 = CARTESIAN_POINT ( 'NONE',  ( 6.005383971424570255, -1.826508537601937432, 0.2321369796495567073 ) ) ;
#131333 = CARTESIAN_POINT ( 'NONE',  ( 11.45842088241064793, 11.09306470877039885, -3.566211699757709574 ) ) ;
#131334 = CARTESIAN_POINT ( 'NONE',  ( -2.995508107964761191, 6.411541510041463887, -0.7147908198718248007 ) ) ;
#131335 = CARTESIAN_POINT ( 'NONE',  ( 1.282252794574537447, -1.823689378192733912, -0.4153219600965887826 ) ) ;
#131336 = CARTESIAN_POINT ( 'NONE',  ( 6.028642311625867833, 2.081422104948245533, 0.5829617784755269927 ) ) ;
#131337 = CARTESIAN_POINT ( 'NONE',  ( -6.113138475847556208, 6.011394290285472231, -0.2943476003282770037 ) ) ;
#131338 = DIRECTION ( 'NONE',  ( 0.000000000000000000, 0.000000000000000000, 1.000000000000000000 ) ) ;
#131339 = CARTESIAN_POINT ( 'NONE',  ( -0.6823417656250003738, -0.2822916663252489355, -1.181850606188749264 ) ) ;
#131340 = CARTESIAN_POINT ( 'NONE',  ( 1.840342752298686380, 1.099902316243700939, -1.564109231055022864 ) ) ;
#131341 = CARTESIAN_POINT ( 'NONE',  ( 2.535733614153494742, 0.8364609567749015095, -1.559706200981937352 ) ) ;
#131342 = CARTESIAN_POINT ( 'NONE',  ( 0.4516295384478058450, -1.352486712789633172, -1.352142238705160704 ) ) ;
#131344 = CARTESIAN_POINT ( 'NONE',  ( 5.589432567506730010, -0.4607417488133085381, 1.859251224981002482 ) ) ;
#131343 = CARTESIAN_POINT ( 'NONE',  ( 3.293788687723198105, -3.198457330048023017, 0.4502801952423823306 ) ) ;
#131345 = CARTESIAN_POINT ( 'NONE',  ( 6.268014395358870061, -1.954855384380562722, 0.2394079155795188485 ) ) ;
#131346 = CARTESIAN_POINT ( 'NONE',  ( 1.499999999999989120, 5.254166666666684193, 0.8660254037844524744 ) ) ;
#131347 = CARTESIAN_POINT ( 'NONE',  ( 1.248456593208754795, 1.040400552670465162, -1.847740296886036582 ) ) ;
#131348 = CARTESIAN_POINT ( 'NONE',  ( 4.891396039733495016, 1.386484060982313249, 1.255958711209571810 ) ) ;
#131350 = ORIENTED_EDGE ( 'NONE', *, *, #79132, .F. ) ;
#131349 = CARTESIAN_POINT ( 'NONE',  ( 0.7678472254676466102, 0.8974085622692473674, 1.589837017038860045 ) ) ;
#131352 = CARTESIAN_POINT ( 'NONE',  ( -2.609770642201835855, -0.3830433331901521576, 0.000000000000000000 ) ) ;
#131351 = CARTESIAN_POINT ( 'NONE',  ( 5.092482806099829062, -2.189899077852827780, -0.2726905915074183673 ) ) ;
#131353 = AXIS2_PLACEMENT_3D ( 'NONE', #79617, #29818, #111122 ) ;
#131354 = CARTESIAN_POINT ( 'NONE',  ( -1.001543065824772872E-14, 5.134375000341421469, 1.575800808251672791 ) ) ;
#131355 = CARTESIAN_POINT ( 'NONE',  ( 1.645062733043511027, -0.3006328960593112054, -2.040525779345269797 ) ) ;
#131356 = CARTESIAN_POINT ( 'NONE',  ( 7.149227073107712549, 7.235186428247455837, -0.7998128361456281477 ) ) ;
#131357 = CARTESIAN_POINT ( 'NONE',  ( -8.311311860377216476, 9.655284244316948872, -1.199719254218446718 ) ) ;
#131358 = FACE_OUTER_BOUND ( 'NONE', #36385, .T. ) ;
#131359 = CARTESIAN_POINT ( 'NONE',  ( -3.423725384795993421, -0.02120445489797120192, -0.4190739096163836885 ) ) ;
#131360 = DIRECTION ( 'NONE',  ( 7.387867266669436732E-31, -1.000000000000000000, -8.546850786086424434E-32 ) ) ;
#131361 = ORIENTED_EDGE ( 'NONE', *, *, #126096, .F. ) ;
#131362 = CARTESIAN_POINT ( 'NONE',  ( 4.686024408448190570, -1.271122505372159539, -1.634150330299996012 ) ) ;
#131363 = CARTESIAN_POINT ( 'NONE',  ( 1.499999999999989120, 5.295833333333356485, -0.8660254037844323793 ) ) ;
#131364 = CARTESIAN_POINT ( 'NONE',  ( 1.089409339093825979, 1.906878951332368732, -1.017924135055588541 ) ) ;
#131365 = CARTESIAN_POINT ( 'NONE',  ( -5.448385796200811981, 7.521903143423984694, -1.249286997217812223 ) ) ;
#131366 = CARTESIAN_POINT ( 'NONE',  ( 2.332681060731033540, 1.317659697769531624, -1.530744237074317171 ) ) ;
#131367 = CARTESIAN_POINT ( 'NONE',  ( 6.720655732516647163, -0.004400176169771369272, 2.173773060281408931 ) ) ;
#131368 = ORIENTED_EDGE ( 'NONE', *, *, #27912, .T. ) ;
#131370 = CARTESIAN_POINT ( 'NONE',  ( 8.188761592974039161, 10.57664116326830595, -1.443375672974063439 ) ) ;
#131369 = CARTESIAN_POINT ( 'NONE',  ( 0.000000000000000000, -2.887499999999999289, -4.012584370867899430 ) ) ;
#131371 = DIRECTION ( 'NONE',  ( 0.000000000000000000, 0.000000000000000000, 1.000000000000000000 ) ) ;
#131372 = CARTESIAN_POINT ( 'NONE',  ( 0.07540816263147330500, 1.497505997221737273, 1.350731191893522976 ) ) ;
#131373 = CARTESIAN_POINT ( 'NONE',  ( 4.845371438081495619, 0.6875289519675978900, -2.081009137124201658 ) ) ;
#131374 = CARTESIAN_POINT ( 'NONE',  ( -1.499999999999997780, 5.181250000682820378, 1.214306433183764966E-14 ) ) ;
#131375 = CARTESIAN_POINT ( 'NONE',  ( 3.603681638446740720, 1.388520161702249567, 1.315275747533505069 ) ) ;
#131376 = CARTESIAN_POINT ( 'NONE',  ( -3.255929445576174697, 6.950334786480840243, -0.7998128361456281477 ) ) ;
#131378 = CARTESIAN_POINT ( 'NONE',  ( 6.439759776366775768, 7.575769829591800786, 1.082531754730558626 ) ) ;
#131377 = B_SPLINE_CURVE_WITH_KNOTS ( 'NONE', 3,
 ( #120288, #170017, #21605, #87712, #153783, #5353, #24831, #207846, #23765, #73589, #76779 ),
 .UNSPECIFIED., .F., .F.,
 ( 4, 1, 1, 1, 1, 1, 1, 1, 4 ),
 ( 0.000000000000000000, 0.2256926809922864541, 0.3979886288388991278, 0.5260859906349554249, 0.6192013483571605637, 0.6864504996671639825, 0.7364865548622955282, 0.7772638159577213157, 1.000000000000000000 ),
 .UNSPECIFIED. ) ;
#131380 = CARTESIAN_POINT ( 'NONE',  ( 2.091422941747251851, -0.4390073250180903663, 1.967893905867940996 ) ) ;
#131379 = CARTESIAN_POINT ( 'NONE',  ( -10.27671724903424888, 11.09185100006920877, 1.040834085586084257E-14 ) ) ;
#131381 = CARTESIAN_POINT ( 'NONE',  ( -1.364683531250000748, 12.67187500034139980, 0.000000000000000000 ) ) ;
#131383 = CARTESIAN_POINT ( 'NONE',  ( -3.318713740295064163, 7.093859473644694269, 0.000000000000000000 ) ) ;
#131382 = CARTESIAN_POINT ( 'NONE',  ( 0.9785521075769167965, -2.238008663356937156, -0.4956820494700850399 ) ) ;
#131384 = CARTESIAN_POINT ( 'NONE',  ( 4.119902764342167956, -0.8871895459346083035, -1.478924549062347049 ) ) ;
#131385 = CARTESIAN_POINT ( 'NONE',  ( -0.1394461523061195918, 6.947787103499363681, -2.875373568546248482 ) ) ;
#131386 = CARTESIAN_POINT ( 'NONE',  ( 2.686486993802192913, 6.285985259411197568, 0.7998128361456362523 ) ) ;
#131387 = CARTESIAN_POINT ( 'NONE',  ( 4.517335436343476118, 8.499999999999996447, -0.7749999999999996891 ) ) ;
#131388 = CARTESIAN_POINT ( 'NONE',  ( 4.864678189204997949, 4.569879397027603929, 0.7998128361456341429 ) ) ;
#131389 = CARTESIAN_POINT ( 'NONE',  ( 0.1755611466353786954, 2.859968053823423784, -2.732108412375580109 ) ) ;
#131390 = ORIENTED_EDGE ( 'NONE', *, *, #70626, .F. ) ;
#131391 = ORIENTED_EDGE ( 'NONE', *, *, #94915, .F. ) ;
#131392 = CARTESIAN_POINT ( 'NONE',  ( 4.934136933359813071, -0.9735637292621384109, -1.527415209752202019 ) ) ;
#131393 = ORIENTED_EDGE ( 'NONE', *, *, #76686, .T. ) ;
#131394 = CARTESIAN_POINT ( 'NONE',  ( 5.337069745634900997, 6.255611453776062980, 1.199719254218452047 ) ) ;
#131395 = CARTESIAN_POINT ( 'NONE',  ( 5.695833931072550094, 5.817763472438987726, 0.000000000000000000 ) ) ;
#131396 = CARTESIAN_POINT ( 'NONE',  ( 6.358062532015329005, 0.6862230018901045447, -1.676680497432983641 ) ) ;
#131397 = CARTESIAN_POINT ( 'NONE',  ( 6.821160681006793070, 7.130644680695653825, 0.7216878364870328300 ) ) ;
#131398 = CARTESIAN_POINT ( 'NONE',  ( -11.92619526913699879, 10.19999999999999929, -1.328859060402686199 ) ) ;
#131399 = CARTESIAN_POINT ( 'NONE',  ( 2.959115643078192637, 0.3208686883675835877, -2.167707805308824121 ) ) ;
#131401 = CARTESIAN_POINT ( 'NONE',  ( 7.540305987494599016, 11.94877408538573427, -0.7998128361456291469 ) ) ;
#131400 = CARTESIAN_POINT ( 'NONE',  ( 6.795359140062033454, -1.661660808857531313, 0.8381669064597346841 ) ) ;
#131402 = CARTESIAN_POINT ( 'NONE',  ( 3.392102565403580350, -0.7792391910043224845, -1.750150251150209391 ) ) ;
#131403 = CARTESIAN_POINT ( 'NONE',  ( -1.499999999999995559, 8.266799604815048497, 3.162088779279327966 ) ) ;
#131404 = CARTESIAN_POINT ( 'NONE',  ( 1.364683531249986537, -0.6364583329919177856, 0.7879004041258500513 ) ) ;
#131405 = CARTESIAN_POINT ( 'NONE',  ( 5.829642864196168617, 6.863966765392747860, 1.082531754730558626 ) ) ;
#131407 = CARTESIAN_POINT ( 'NONE',  ( 5.788306078712673219, -0.7643476728274435361, -1.974717070840046107 ) ) ;
#131406 = CARTESIAN_POINT ( 'NONE',  ( -9.327646496521984076, 11.90534021740758064, -1.443375672974059665 ) ) ;
#131408 = CARTESIAN_POINT ( 'NONE',  ( 1.182749364907993206, -2.109161078630458430, -0.4729781282231394490 ) ) ;
#131409 = CARTESIAN_POINT ( 'NONE',  ( -6.123442655227560927, 7.173046514967467147, 1.199719254218452047 ) ) ;
#131410 = CARTESIAN_POINT ( 'NONE',  ( 5.225741863424510747, 5.061396693608882558, 0.7998128361456352531 ) ) ;
#131411 = CARTESIAN_POINT ( 'NONE',  ( 0.9381830591699467092, 1.797733097909786304, 0.3167546781352030272 ) ) ;
#131412 = CARTESIAN_POINT ( 'NONE',  ( -4.440459003675619520, 5.139289244831666714, 1.199719254218462483 ) ) ;
#131413 = CARTESIAN_POINT ( 'NONE',  ( 3.082817581614716307, -0.1327354176642106531, -1.820802398864965088 ) ) ;
#131414 = CARTESIAN_POINT ( 'NONE',  ( 9.898415338264832997, 12.56653357618227318, -7.886274193477667893 ) ) ;
#131415 = ORIENTED_EDGE ( 'NONE', *, *, #54909, .T. ) ;
#131416 = CARTESIAN_POINT ( 'NONE',  ( 3.226963424687212090, -1.818787540941589009, -0.7562359814760648558 ) ) ;
#131417 = ORIENTED_EDGE ( 'NONE', *, *, #200594, .T. ) ;
#131418 = CARTESIAN_POINT ( 'NONE',  ( 4.440924170176640651, -1.503556815104054811, -1.229221392163130755 ) ) ;
#131419 = CARTESIAN_POINT ( 'NONE',  ( -3.709037541790315640, 6.484905011134099340, -1.199719254218450271 ) ) ;
#131421 = CARTESIAN_POINT ( 'NONE',  ( 5.344028447597857223, -1.346983732444573256, -1.637812552581649594 ) ) ;
#131420 = CARTESIAN_POINT ( 'NONE',  ( 5.508355548902068577, 9.648441583686274470, 0.7998128361456331437 ) ) ;
#131422 = EDGE_CURVE ( 'NONE', #136049, #147669, #108427, .T. ) ;
#131423 = CARTESIAN_POINT ( 'NONE',  ( 2.490748672031910083, -1.830495558572857728, -0.5533032672612181457 ) ) ;
#131424 = CARTESIAN_POINT ( 'NONE',  ( 5.854153468347242040, 6.181931306435468620, -0.8879621099797951889 ) ) ;
#131425 = CARTESIAN_POINT ( 'NONE',  ( 0.2331563151865486128, 1.372759770070256291, -2.202161770551560149 ) ) ;
#131426 = ORIENTED_EDGE ( 'NONE', *, *, #27605, .T. ) ;
#131427 = CARTESIAN_POINT ( 'NONE',  ( 5.578253857379852576, 5.472660686556754861, -0.7998128361456481317 ) ) ;
#131428 = CARTESIAN_POINT ( 'NONE',  ( 4.231111847260408787, 1.841413651135707985, 0.8138496092669408322 ) ) ;
#131429 = CARTESIAN_POINT ( 'NONE',  ( 11.07124251632621537, 12.30000000000000071, -0.8054525327832628978 ) ) ;
#131430 = CARTESIAN_POINT ( 'NONE',  ( 4.916531288042031989, 1.256637652550334883, -1.324621001416517840 ) ) ;
#131431 = CARTESIAN_POINT ( 'NONE',  ( 1.205626512970816355, -1.630946839658468983, -1.275175305487465049 ) ) ;
#131432 = CARTESIAN_POINT ( 'NONE',  ( -8.351459436338037889, 10.76645531385962862, -1.443375672974059665 ) ) ;
#131433 = CARTESIAN_POINT ( 'NONE',  ( -6.612576056032890115, 6.759750829040511277, 0.1256891304984939506 ) ) ;
#131434 = CARTESIAN_POINT ( 'NONE',  ( -1.225000000000008304, 1.583333334016155503, 0.7072540797572817173 ) ) ;
#131435 = CARTESIAN_POINT ( 'NONE',  ( 5.594569530875262764, -0.4557361262383100020, -1.814172972432124720 ) ) ;
#131436 = CARTESIAN_POINT ( 'NONE',  ( 7.298366762858032430, 7.409182732956175244, 1.040834085586084257E-14 ) ) ;
#131437 = CARTESIAN_POINT ( 'NONE',  ( -3.438964519360664607, 7.163875705896082913, -0.7998128361456282587 ) ) ;
#131438 = CARTESIAN_POINT ( 'NONE',  ( 0.6823417656249934904, 10.25520833367472839, 1.181850606188764807 ) ) ;
#131439 = CARTESIAN_POINT ( 'NONE',  ( -4.388035272317281077, 8.271124917678806199, 0.7998128361456481317 ) ) ;
#131440 = CARTESIAN_POINT ( 'NONE',  ( 2.333974999846879061, 5.874721266463329705, -0.7998128361456291469 ) ) ;
#131441 = AXIS2_PLACEMENT_3D ( 'NONE', #92593, #108881, #191106 ) ;
#131442 = CARTESIAN_POINT ( 'NONE',  ( -6.933015448541747006, 9.181880338089085214, 1.599625672291269396 ) ) ;
#131443 = CARTESIAN_POINT ( 'NONE',  ( -5.717788096661253761, 7.693838750903348789, 1.599625672291269396 ) ) ;
#131444 = CARTESIAN_POINT ( 'NONE',  ( 1.270471156847551075, -0.9273748054965322840, -1.850965650132020635 ) ) ;
#131446 = EDGE_CURVE ( 'NONE', #172377, #163352, #139607, .T. ) ;
#131445 =( BOUNDED_CURVE ( )  B_SPLINE_CURVE ( 3, ( #51986, #199271, #171047, #149482 ),
 .UNSPECIFIED., .F., .T. ) 
 B_SPLINE_CURVE_WITH_KNOTS ( ( 4, 4 ),
 ( 1.420228054018210395, 1.445468495626831107 ),
 .UNSPECIFIED. ) 
 CURVE ( )  GEOMETRIC_REPRESENTATION_ITEM ( )  RATIONAL_B_SPLINE_CURVE ( ( 1.000000000000000000, 0.9999469107135832147, 0.9999469107135832147, 1.000000000000000000 ) ) 
 REPRESENTATION_ITEM ( '' )  );
#131447 = CARTESIAN_POINT ( 'NONE',  ( 1.792722901331974761, 1.566437577840825712, -1.424566180320179010 ) ) ;
#131448 = CARTESIAN_POINT ( 'NONE',  ( 8.215351014876830504, 11.67199438640995801, -1.199719254218446718 ) ) ;
#131449 = CARTESIAN_POINT ( 'NONE',  ( 11.37385970535889257, 1.000000000000000888, -3.825613075418463627 ) ) ;
#131450 = CARTESIAN_POINT ( 'NONE',  ( 6.262565978045822490, -0.7396069823457154246, -1.933831554736538338 ) ) ;
#131451 = CARTESIAN_POINT ( 'NONE',  ( 4.188544580023894071, 7.586160867502751870, 0.8937768461303140510 ) ) ;
#131452 = CARTESIAN_POINT ( 'NONE',  ( 4.311129659465574804, 7.013106455143060636, -1.082531754730548412 ) ) ;
#131454 = CARTESIAN_POINT ( 'NONE',  ( 6.471393748265540147, 5.229711127717882491, 2.420000000000010587 ) ) ;
#131453 = CARTESIAN_POINT ( 'NONE',  ( 11.44791656467458552, 9.800000000000002487, -3.303228920649581291 ) ) ;
#131455 = CARTESIAN_POINT ( 'NONE',  ( 2.590095216689162427, -2.286210222917249180, -0.1672752534159216153 ) ) ;
#131456 = CARTESIAN_POINT ( 'NONE',  ( -6.966220764712148572, 6.002124920821316323, 2.500000000000000444 ) ) ;
#131457 = CARTESIAN_POINT ( 'NONE',  ( 2.408343312057196872, -1.907530749141531423, -0.1368029246449145864 ) ) ;
#131458 = VERTEX_POINT ( 'NONE', #194837 ) ;
#131459 = CARTESIAN_POINT ( 'NONE',  ( 6.277061933002774374, 9.306694107603160404, 1.082531754730558626 ) ) ;
#131460 = CARTESIAN_POINT ( 'NONE',  ( 0.7736903856863480700, 0.3886292558455446411, -1.975178614941161870 ) ) ;
#131461 = CARTESIAN_POINT ( 'NONE',  ( 1.305434336737832490, -1.543085766649286317, -1.211208057394968618 ) ) ;
#131462 = CARTESIAN_POINT ( 'NONE',  ( -10.48453286206953727, 11.12637651536962125, 0.7998128361456462443 ) ) ;
#131463 = CARTESIAN_POINT ( 'NONE',  ( -8.037286134802835491, 8.271255333558444889, -0.7998128361456291469 ) ) ;
#131464 = CARTESIAN_POINT ( 'NONE',  ( -11.45681933918879380, 6.923721555720867116, -3.421067468575024417 ) ) ;
#131466 = CARTESIAN_POINT ( 'NONE',  ( 2.676313443976061190, -1.692906749566702507, -0.5160995803213176414 ) ) ;
#131465 = CARTESIAN_POINT ( 'NONE',  ( 4.277343952648727132, 1.365583793738689655, 1.583094835029410063 ) ) ;
#131467 = CARTESIAN_POINT ( 'NONE',  ( 0.4019237886466814902, 12.07366454968463110, 1.499999999999999334 ) ) ;
#131469 = CARTESIAN_POINT ( 'NONE',  ( 5.876963737413220201, 2.120050906709324501, -0.8721662429640556491 ) ) ;
#131468 = DIRECTION ( 'NONE',  ( 0.000000000000000000, 0.000000000000000000, -1.000000000000000000 ) ) ;
#131470 = CARTESIAN_POINT ( 'NONE',  ( 4.628681372238307112, -1.589566819310319845, 0.7089629299102307991 ) ) ;
#131471 = CARTESIAN_POINT ( 'NONE',  ( 9.134442807305049428, 11.67993591332117376, 1.599625672291281386 ) ) ;
#131472 = CARTESIAN_POINT ( 'NONE',  ( 5.061990249855835344, 6.999017606288843396, -1.599625672291273393 ) ) ;
#131473 = CARTESIAN_POINT ( 'NONE',  ( 4.534371549175888028, 1.681635666518576988, -0.4216726850935527127 ) ) ;
#131474 = CARTESIAN_POINT ( 'NONE',  ( 4.527882006162959883, 2.107076143796441592, -0.5232759588417631447 ) ) ;
#131475 = CARTESIAN_POINT ( 'NONE',  ( 3.334415713957098681, 5.977569868670206787, -1.199719254218446718 ) ) ;
#131476 = CARTESIAN_POINT ( 'NONE',  ( 6.069546051295945155, 1.394081536189460069, 1.457239770841619597 ) ) ;
#131477 = CARTESIAN_POINT ( 'NONE',  ( 0.4999999999999185651, 1.979557137443526406E-12, -2.052068128417952941 ) ) ;
#131478 = CARTESIAN_POINT ( 'NONE',  ( 0.7499999999999902300, 3.514583334016149863, 1.299038105676669330 ) ) ;
#131479 = CARTESIAN_POINT ( 'NONE',  ( 2.151277967514260592, -1.545957563563664650, -1.149148694925563596 ) ) ;
#131480 = CARTESIAN_POINT ( 'NONE',  ( 0.7500000000000006661, 9.447916667349467446, -1.299038105676657340 ) ) ;
#131481 = CARTESIAN_POINT ( 'NONE',  ( 5.273765199871699672, 0.4330091245797212385, -2.178642023334904199 ) ) ;
#131482 = EDGE_LOOP ( 'NONE', ( #183159, #90407, #13348, #72169 ) ) ;
#131483 = CARTESIAN_POINT ( 'NONE',  ( 6.883263157960391787, -0.001104538646235289417, 1.946037152736757925 ) ) ;
#131484 = CARTESIAN_POINT ( 'NONE',  ( 0.7499999999999902300, 2.733333333333351600, 1.299038105676669330 ) ) ;
#131485 = CARTESIAN_POINT ( 'NONE',  ( 7.474622759835693131, 7.614814729430110951, -0.7998128361456281477 ) ) ;
#131486 = CARTESIAN_POINT ( 'NONE',  ( 1.981385142061100835, -2.032350350298214980, -0.8968915317347254668 ) ) ;
#131488 = DIRECTION ( 'NONE',  ( 0.000000000000000000, 0.000000000000000000, 1.000000000000000000 ) ) ;
#131487 = VECTOR ( 'NONE', #60494, 1000.000000000000000 ) ;
#131489 = CARTESIAN_POINT ( 'NONE',  ( 7.266807147244743526, 11.42176607185347414, -0.7216878364870267237 ) ) ;
#131490 = DIRECTION ( 'NONE',  ( 8.638326563840809144E-31, 5.962633348652903386E-61, -1.000000000000000000 ) ) ;
#131491 = CARTESIAN_POINT ( 'NONE',  ( 6.536439455564150514, 9.679577560583279450, 1.082531754730549078 ) ) ;
#131492 = CARTESIAN_POINT ( 'NONE',  ( -5.316205630334276400, 5.374863788244313767, -0.7216878364870338292 ) ) ;
#131494 = CARTESIAN_POINT ( 'NONE',  ( 4.738769042418014443, -1.999979230503599048, -0.5042011814720639418 ) ) ;
#131493 = CARTESIAN_POINT ( 'NONE',  ( 10.71502147350184231, 11.39527989537399755, 0.000000000000000000 ) ) ;
#131495 = CARTESIAN_POINT ( 'NONE',  ( -3.415764635639130020, 6.072476943965863683, 1.199719254218462483 ) ) ;
#131496 = CARTESIAN_POINT ( 'NONE',  ( -15.75000000000000000, 9.799999999999998934, -1.800000000000001155 ) ) ;
#131497 = CARTESIAN_POINT ( 'NONE',  ( -0.6823417656250246877, 0.05104166700808931978, 1.181850606188755259 ) ) ;
#131498 = CARTESIAN_POINT ( 'NONE',  ( 5.975831987570860981, 1.113884111790110820, 1.502598383168303409 ) ) ;
#131499 = CARTESIAN_POINT ( 'NONE',  ( 4.939963660092479891, -1.468890173064988147, -0.9213945099728354515 ) ) ;
#131500 = CARTESIAN_POINT ( 'NONE',  ( 4.106796630993492236, -0.2923914088966376723, 1.715523938624329281 ) ) ;
#131501 = CARTESIAN_POINT ( 'NONE',  ( 3.225950485047770933, 5.851027101609320269, 1.199719254218450271 ) ) ;
#131502 = CARTESIAN_POINT ( 'NONE',  ( 2.384684040179287479, -0.3955501765894597344, -2.257852644028814915 ) ) ;
#131503 = CARTESIAN_POINT ( 'NONE',  ( -0.6823417656249969321, 5.280208333674756283, -1.181850606188749264 ) ) ;
#131504 = CARTESIAN_POINT ( 'NONE',  ( 5.601146835291897830, -0.5070800215070477845, 2.028203315493964709 ) ) ;
#131505 = CARTESIAN_POINT ( 'NONE',  ( 0.9195641160042143936, 1.098457714822091091, -1.477412082521646575 ) ) ;
#131506 = DIRECTION ( 'NONE',  ( 0.000000000000000000, 0.000000000000000000, 1.000000000000000000 ) ) ;
#131507 = SURFACE_SIDE_STYLE ('',( #97912 ) ) ;
#131508 = CARTESIAN_POINT ( 'NONE',  ( 3.235000160576475992, 2.016597019841442240, -0.002811030766311505089 ) ) ;
#131509 = CARTESIAN_POINT ( 'NONE',  ( 0.9377431681640016059, 0.8850447378907432272, -2.004962588275795543 ) ) ;
#131510 = CARTESIAN_POINT ( 'NONE',  ( 9.998113830209401698, 14.27718261535635058, -7.519171174559423854 ) ) ;
#131511 = CARTESIAN_POINT ( 'NONE',  ( -7.335124800193271177, 8.516399340768996851, -1.199719254218452935 ) ) ;
#131512 = CARTESIAN_POINT ( 'NONE',  ( 1.768117254402020277, -2.054967671486531255, 0.2513356459030794410 ) ) ;
#131513 = CARTESIAN_POINT ( 'NONE',  ( 5.843727902690005749, 6.776436293681846301, -1.199719254218445830 ) ) ;
#131514 = CARTESIAN_POINT ( 'NONE',  ( -1.151774525698488676E-14, -0.7656249996585936524, 1.570758158831776052 ) ) ;
#131515 = CARTESIAN_POINT ( 'NONE',  ( 3.369896858953734142, 0.5134250039646214292, -2.057278921464212207 ) ) ;
#131516 = CARTESIAN_POINT ( 'NONE',  ( 1.364683531249986537, -0.8864583329919110133, 0.7879004041258500513 ) ) ;
#131517 = CARTESIAN_POINT ( 'NONE',  ( 6.445924739416000193, 0.6936395621829589686, -1.688995215704327313 ) ) ;
#131518 = ORIENTED_EDGE ( 'NONE', *, *, #114579, .F. ) ;
#131519 = CARTESIAN_POINT ( 'NONE',  ( -4.685224601974262271, 7.623789914682047808, -1.199719254218453823 ) ) ;
#131520 = CARTESIAN_POINT ( 'NONE',  ( 9.049177462117294013, 12.64479190819049670, -1.199719254218446718 ) ) ;
#131521 = CARTESIAN_POINT ( 'NONE',  ( 7.471952054462756010, 7.889901283060952508, 0.7216878364870267237 ) ) ;
#131522 = CARTESIAN_POINT ( 'NONE',  ( 1.737500000000001155, -2.289583332377418401, 3.009438278150922130 ) ) ;
#131523 = CARTESIAN_POINT ( 'NONE',  ( -6.338600509588822263, 7.353787668397130162, -1.199719254218446718 ) ) ;
#131524 = CARTESIAN_POINT ( 'NONE',  ( 3.217061457047249551, 1.589534765328611154, -1.246005657720136606 ) ) ;
#131525 = CARTESIAN_POINT ( 'NONE',  ( 0.5519644926167607268, 0.6605455615449079554, -1.999741160550670527 ) ) ;
#131526 = CARTESIAN_POINT ( 'NONE',  ( -6.805266759416629618, 6.904175738932996964, 0.000000000000000000 ) ) ;
#131527 = CARTESIAN_POINT ( 'NONE',  ( 9.725276259704228821, 10.24057714594344048, 0.7998128361456462443 ) ) ;
#131528 = CARTESIAN_POINT ( 'NONE',  ( 4.891365455385704664, -1.702569429429393599, 0.7516348641289184451 ) ) ;
#131529 = CARTESIAN_POINT ( 'NONE',  ( 9.576136569953906275, 10.06658084123472641, 0.000000000000000000 ) ) ;
#131530 = CARTESIAN_POINT ( 'NONE',  ( 4.885223684246801312, 4.924875305092577982, -0.7419332605567361405 ) ) ;
#131531 = CARTESIAN_POINT ( 'NONE',  ( -3.079673448598517549, 6.744702790006905424, 1.040834085586084257E-14 ) ) ;
#131532 =( BOUNDED_SURFACE ( )  B_SPLINE_SURFACE ( 3, 2, ( 
 ( #188008, #137153, #203178 ),
 ( #54825, #120975, #38576 ),
 ( #138222, #170698, #204235 ),
 ( #122044, #39635, #212521 ),
 ( #79340, #209309, #205320 ),
 ( #62033, #81474, #47939 ) ),
 .UNSPECIFIED., .F., .F., .F. ) 
 B_SPLINE_SURFACE_WITH_KNOTS ( ( 4, 2, 4 ),
 ( 3, 3 ),
 ( 6.938893903907228378E-18, 0.002403677751102634413, 0.004807355502205261887 ),
 ( 0.000000000000000000, 1.000000000000000000 ),
 .UNSPECIFIED. ) 
 GEOMETRIC_REPRESENTATION_ITEM ( )  RATIONAL_B_SPLINE_SURFACE ( (
 ( 1.000000000000000000, 0.7789607113619931855, 1.000000000000000000),
 ( 1.000000000000000000, 0.7844575505954987094, 1.000000000000000000),
 ( 1.000000000000000000, 0.7910273759756240031, 1.000000000000000000),
 ( 1.000000000000000000, 0.8087931444444612650, 1.000000000000000000),
 ( 1.000000000000000000, 0.8199986536752662536, 1.000000000000000000),
 ( 1.000000000000000000, 0.8356624583022091990, 1.000000000000000000) ) ) 
 REPRESENTATION_ITEM ( '' )  SURFACE ( )  );
#131533 = CARTESIAN_POINT ( 'NONE',  ( -7.314787569772770226, 8.492672571945082183, -1.199719254218452935 ) ) ;
#131534 = CARTESIAN_POINT ( 'NONE',  ( 0.2862814217290919894, -1.017545141758866789, 1.907252267444502269 ) ) ;
#131536 = CARTESIAN_POINT ( 'NONE',  ( -5.084594181526506773, 6.727074486938107611, 1.441884573159227578 ) ) ;
#131535 = CARTESIAN_POINT ( 'NONE',  ( -5.237192476628793614, 9.332084666034067055, 0.7998128361456291469 ) ) ;
#131537 = CARTESIAN_POINT ( 'NONE',  ( -1.364683531250014514, 0.2385416670080863499, -0.7879004041258359514 ) ) ;
#131538 = CARTESIAN_POINT ( 'NONE',  ( 2.266548906626513649, -1.733607756391885912, 0.03760194650299571173 ) ) ;
#131539 = CARTESIAN_POINT ( 'NONE',  ( 1.218268023815568535, -0.04584277261814385940, 1.739893813429808311 ) ) ;
#131541 = CARTESIAN_POINT ( 'NONE',  ( 6.155038550924139429, 9.164333495178082600, 1.082531754730558626 ) ) ;
#131540 = CARTESIAN_POINT ( 'NONE',  ( 6.358097629954328589, 2.302029506726857466, -0.1628147022267756039 ) ) ;
#131542 = CARTESIAN_POINT ( 'NONE',  ( -10.91675076000969113, 4.673595418013491987, -4.467283485442433921 ) ) ;
#131543 = CARTESIAN_POINT ( 'NONE',  ( 2.864585088123726919, -1.423607738919046906, 1.490243374215278971 ) ) ;
#131544 = CARTESIAN_POINT ( 'NONE',  ( 4.143988507271280319, 7.986403691791820414, -0.7998128361456221525 ) ) ;
#131545 = ADVANCED_FACE ( 'NONE', ( #110465 ), #148119, .T. ) ;
#131546 = CARTESIAN_POINT ( 'NONE',  ( 1.335314297916901927, -1.281167425915705316, 1.556668322744148014 ) ) ;
#131547 = CARTESIAN_POINT ( 'NONE',  ( 6.925078400183553029, 2.941156041390875941, 2.696161060448130975 ) ) ;
#131548 = CARTESIAN_POINT ( 'NONE',  ( -4.447956913735107598, 7.346977611736363656, 1.199719254218452935 ) ) ;
#131549 = CARTESIAN_POINT ( 'NONE',  ( 6.455916552660014851, 1.865467424361374249, -0.1398750677365916961 ) ) ;
#131551 = CARTESIAN_POINT ( 'NONE',  ( -5.777182853198894463, 9.754147405458438058, 0.7216878364870267237 ) ) ;
#131550 = CARTESIAN_POINT ( 'NONE',  ( 4.218947473185084007, 1.474887410857337100, -1.217315437338606365 ) ) ;
#131552 = CARTESIAN_POINT ( 'NONE',  ( 5.707716145626243964, -0.5396369327701348029, 2.139774205771049154 ) ) ;
#131553 = CARTESIAN_POINT ( 'NONE',  ( -6.739811759324828344, 8.956476034002674780, -1.443375672974066548 ) ) ;
#131554 = CARTESIAN_POINT ( 'NONE',  ( 6.393551957296131683, 9.616838495890963401, 1.199719254218452047 ) ) ;
#131555 = ADVANCED_FACE ( 'NONE', ( #111529 ), #132952, .T. ) ;
#131556 = CARTESIAN_POINT ( 'NONE',  ( -5.126391479298592735, 5.153413945369351268, 0.000000000000000000 ) ) ;
#131557 = CARTESIAN_POINT ( 'NONE',  ( 0.6100282365348074221, -0.7248652973187595938, 1.885305865817282323 ) ) ;
#131558 = ORIENTED_EDGE ( 'NONE', *, *, #195142, .T. ) ;
#131559 = FACE_OUTER_BOUND ( 'NONE', #83636, .T. ) ;
#131560 = CARTESIAN_POINT ( 'NONE',  ( 4.911288641948820199, 2.004953420984519674, 1.142316731622401882 ) ) ;
#131561 = CARTESIAN_POINT ( 'NONE',  ( 4.756279191188107269, -1.961398630904508833, -0.05015466537350299348 ) ) ;
#131562 = CARTESIAN_POINT ( 'NONE',  ( 1.692165188054130187, 0.9715730843921737137, -1.704227633833883759 ) ) ;
#131563 = CARTESIAN_POINT ( 'NONE',  ( 8.536830278099042602, 13.11138575775759563, -0.7998128361456352531 ) ) ;
#131564 = CARTESIAN_POINT ( 'NONE',  ( -9.417646481151111360, 14.63844056099971347, 7.338279069377040997 ) ) ;
#131565 = VERTEX_POINT ( 'NONE', #167678 ) ;
#131566 = CARTESIAN_POINT ( 'NONE',  ( 0.5853561509586381328, 1.734793994416533369, 1.213709793590052932 ) ) ;
#131568 = CARTESIAN_POINT ( 'NONE',  ( -8.505042434474312074, 8.816971016508505343, -0.7998128361456291469 ) ) ;
#131567 = CARTESIAN_POINT ( 'NONE',  ( -4.843287188579803448, 6.673587691474970107, -1.599625672291256295 ) ) ;
#131569 = CARTESIAN_POINT ( 'NONE',  ( 0.6558947131179297951, -1.335331635844772880, 1.267786537210900510 ) ) ;
#131570 = VERTEX_POINT ( 'NONE', #18206 ) ;
#131571 = CARTESIAN_POINT ( 'NONE',  ( 4.469693783504245843, -0.3772167039018388124, 2.137918043537301305 ) ) ;
#131572 = CARTESIAN_POINT ( 'NONE',  ( 0.3373309291320715220, 2.648944349799879472, 1.974167966546634956 ) ) ;
#131573 = CARTESIAN_POINT ( 'NONE',  ( 2.039458538997685366, 0.004855507148140979744, 2.120778211687989856 ) ) ;
#131574 = CARTESIAN_POINT ( 'NONE',  ( 1.499999999999989120, 3.535416667349488229, 0.8660254037844524744 ) ) ;
#131575 = CARTESIAN_POINT ( 'NONE',  ( 9.589694723567584234, 10.08239868711733855, -0.7998128361456281477 ) ) ;
#131576 = CARTESIAN_POINT ( 'NONE',  ( -1.878807924852155864, 2.480000000000016858, -2.465802685833468288 ) ) ;
#131577 = CARTESIAN_POINT ( 'NONE',  ( 6.296370465541430761, 6.973533528358998979, 0.9269300130883666444 ) ) ;
#131578 = CARTESIAN_POINT ( 'NONE',  ( 2.477870184918748997, 1.265364588504451548, 1.626488340418334566 ) ) ;
#131580 = FACE_OUTER_BOUND ( 'NONE', #170645, .T. ) ;
#131579 = CARTESIAN_POINT ( 'NONE',  ( -8.799405390469187793, 10.22472669609091689, -1.199719254218446718 ) ) ;
#131581 = CARTESIAN_POINT ( 'NONE',  ( -1.364683531250012516, 2.780208333674754506, 0.7879004041258379498 ) ) ;
#131582 = CARTESIAN_POINT ( 'NONE',  ( 0.07755575628183573877, 1.325091491099144259, -2.441202027401535357 ) ) ;
#131583 = CARTESIAN_POINT ( 'NONE',  ( -3.741371894207468074, 7.428709027653146890, 2.448389769268642713 ) ) ;
#131584 = CARTESIAN_POINT ( 'NONE',  ( 5.197880135092803222, 1.287283252470315720, 1.414272151883423589 ) ) ;
#131585 = CARTESIAN_POINT ( 'NONE',  ( 0.08304785351339466493, -2.141800023564765620, -0.5316218738360134477 ) ) ;
#131586 = CARTESIAN_POINT ( 'NONE',  ( 1.511376755312091591, 1.995097771225157635, 1.066857341152693373 ) ) ;
#131587 = CARTESIAN_POINT ( 'NONE',  ( -9.219181267612684749, 10.81842823604534765, 1.082531754730558626 ) ) ;
#131589 = ADVANCED_FACE ( 'NONE', ( #19278 ), #74741, .T. ) ;
#131588 = CARTESIAN_POINT ( 'NONE',  ( 1.107327745774109529, 1.372724574380719043, 1.182278994020573792 ) ) ;
#131590 = CARTESIAN_POINT ( 'NONE',  ( 2.131924177892559058, 1.915402082336896461, 0.04262488632780260522 ) ) ;
#131591 = CARTESIAN_POINT ( 'NONE',  ( 3.490741092712910998, 2.019281663078629219, 0.4563312328872348722 ) ) ;
#131592 = CARTESIAN_POINT ( 'NONE',  ( -1.364683531250012516, 1.342708333674755616, 0.7879004041258379498 ) ) ;
#131593 = CARTESIAN_POINT ( 'NONE',  ( 1.393369717069929514, 1.491581312685308580, 1.289216981855696664 ) ) ;
#131594 = CARTESIAN_POINT ( 'NONE',  ( 5.777940811437299651, 1.149350900142607879, 1.545952477797669200 ) ) ;
#131596 = CARTESIAN_POINT ( 'NONE',  ( 5.535985025370705692, 7.434063834270491000, -1.247683609459742549 ) ) ;
#131595 = CARTESIAN_POINT ( 'NONE',  ( 1.225685606067970612, -0.05223309053147862785, 2.307267396272806970 ) ) ;
#131597 = CARTESIAN_POINT ( 'NONE',  ( -1.364683531250000748, 1.259375000341421469, 0.000000000000000000 ) ) ;
#131598 = CARTESIAN_POINT ( 'NONE',  ( 5.582507124453381486, 1.231422846540839666, -1.654610746699414214 ) ) ;
#131599 = CARTESIAN_POINT ( 'NONE',  ( -5.762378981008047241, 6.681529218386182301, 1.199719254218450271 ) ) ;
#131600 = CARTESIAN_POINT ( 'NONE',  ( 8.098297826064319693, 8.342435640030188893, 0.7998128361456481317 ) ) ;
#131602 = CARTESIAN_POINT ( 'NONE',  ( -0.7499999999999972244, 5.358333333333353821, -1.299038105676652011 ) ) ;
#131601 = CARTESIAN_POINT ( 'NONE',  ( 6.282269041519704444, -1.129704631681987204, 1.777121156631493726 ) ) ;
#131603 = EDGE_CURVE ( 'NONE', #1299, #31691, #121431, .T. ) ;
#131604 = CARTESIAN_POINT ( 'NONE',  ( -1.364683531250012516, 3.092708333674755838, 0.7879004041258379498 ) ) ;
#131605 = CARTESIAN_POINT ( 'NONE',  ( 4.499409293453607184, 1.733128992574247684, 1.291583502853070886 ) ) ;
#131606 = CARTESIAN_POINT ( 'NONE',  ( 5.092447094119275874, -1.120170962321866082, 1.680348583886650315 ) ) ;
#131607 = DIRECTION ( 'NONE',  ( 0.000000000000000000, 0.000000000000000000, -1.000000000000000000 ) ) ;
#131608 = CARTESIAN_POINT ( 'NONE',  ( -6.263503779833496488, 6.409768619334935913, 0.7216878364870317197 ) ) ;
#131609 = EDGE_CURVE ( 'NONE', #179029, #137516, #155083, .T. ) ;
#131610 = B_SPLINE_SURFACE_WITH_KNOTS ( 'NONE', 1, 3, ( 
 ( #188870, #24218, #140157, #144446, #164646, #78322, #45854, #198190, #66037, #49825, #126095, #50893, #16229, #109836, #44789, #114888, #1042, #210449, #214406, #175847, #17298, #166779, #28515, #12247, #117018, #176901, #62087, #192057, #99642, #128245, #82313, #208310, #160647, #115950, #133241, #83376, #180887, #127171, #132184, #183015, #98584, #194209, #193141, #181940, #33570, #32509, #110895, #165709, #94606, #77255, #148407, #149459, #199246, #67105, #34632, #100703, #61013, #43721, #18375, #142300, #59941, #27438, #93536, #159580, #11177, #143370, #209368, #2104, #200316, #167839, #68178, #150540, #134309, #51967, #35695, #101771, #84452, #118091, #184076, #207213, #194167, #140115, #12210, #144409, #127128, #128206, #141202, #43680, #210409, #42615, #108725, #60972, #161692, #189901, #76153, #109799, #44747, #77213, #157423, #75090, #62051, #111934, #159538, #58837, #25262, #208269, #94565, #45814, #173686, #93498, #78281, #177936, #28473, #193098, #192017, #175806, #29549, #142257, #10077, #107657, #143332, #124992, #95641, #190951, #209325, #91363, #74025, #160608, #110853, #176861, #41543, #59902, #11136, #126055, #27398, #206141, #57772, #123933, #9014, #174751, #26324, #92438, #158477, #197360, #83610, #15400, #82542, #195247, #99874, #34849, #114072, #97763, #199478, #47957, #147568, #63106, #182165, #213589, #98816, #79359, #31687, #132413, #1274, #165937, #131365, #212542, #196, #51122, #181117, #65214, #64182, #50059, #198415, #49003, #130323, #116180, #196313, #162760, #180064, #33796, #67332, #16462, #149691, #163822, #146523, #211472, #17522, #100924, #13286, #66265, #81491, #115121, #32736, #164868, #129274, #14334, #148630, #145477, #133476, #46883, #112995, #80424, #117245, #183245, #179008, #30622, #96711, #85750, #72688, #18604, #105220, #2333, #122614, #19671, #151832, #22854, #150771, #3405 ),
 ( #69474, #200542, #134536, #135581, #121538, #39137, #155023, #84684, #202674, #201603, #138783, #68409, #171260, #88968, #53251, #204803, #20723, #86817, #152883, #36991, #6607, #167012, #4461, #103074, #168071, #70531, #56454, #102002, #118314, #5525, #136649, #54322, #52188, #119382, #188577, #169129, #35925, #55383, #40209, #185368, #184300, #120463, #21776, #186435, #38073, #104143, #170190, #87885, #153959, #71606, #137717, #203737, #187508, #179718, #47600, #110510, #161333, #62743, #212183, #81140, #147225, #61690, #31335, #96349, #97412, #146168, #112643, #93148, #176510, #127859, #194884, #144056, #159185, #163467, #45458, #192734, #160256, #145113, #63820, #193809, #95285, #10786, #15047, #44389, #129978, #76861, #111574, #213250, #43330, #11857, #80066, #64880, #177582, #77935, #142980, #131026, #109448, #208980, #175455, #210051, #27039, #12917, #60617, #126776, #28122, #94216, #162404, #29196, #78997, #211119, #13982, #46521, #128903, #178652, #30263, #195965, #113714, #49704, #166661, #52901, #165588, #17181, #183964, #70193, #98460, #199125, #18251, #167723, #200198, #65919, #198077, #119035, #20390, #68051, #115833, #148287, #116898, #3056, #185018, #82193, #1988, #201261, #36644, #151487, #35575, #100587, #84335, #102728, #50769, #133127, #16109, #51851, #181819, #168785, #33451, #86474, #152538, #99528, #150423, #134189, #69126, #4124, #197017, #920, #48653, #101655, #114770, #85401, #117971, #32394, #83256, #66988, #19324, #149341, #164524, #180766, #182898, #132066, #34514, #135248, #214286, #72335, #188228, #186093, #42019, #71262, #24657, #37723, #154679, #91837, #136305, #104874, #173076, #25727, #6264, #170917, #21439, #9488, #157895, #103802, #202327, #88624, #174155, #39868, #169851, #87547, #137376, #53977, #189304, #153615, #138441, #120113, #107050, #139514, #5187, #203392, #55045, #121195 ) ),
 .UNSPECIFIED., .F., .T., .F.,
 ( 2, 2 ),
 ( 4, 2, 2, 2, 2, 2, 2, 2, 2, 2, 2, 2, 2, 2, 2, 2, 2, 2, 2, 2, 2, 2, 2, 2, 2, 2, 2, 2, 2, 2, 2, 2, 2, 2, 2, 2, 2, 2, 2, 2, 2, 2, 2, 2, 2, 2, 2, 2, 2, 2, 2, 2, 2, 2, 2, 2, 2, 2, 2, 2, 2, 2, 2, 2, 2, 2, 2, 2, 2, 2, 2, 2, 2, 2, 2, 2, 2, 2, 2, 2, 2, 2, 2, 2, 2, 2, 2, 2, 2, 2, 2, 2, 2, 2, 2, 2, 2, 2, 2, 2, 2, 2, 2, 2, 2, 2, 2, 2, 4 ),
 ( 0.000000000000000000, 1.000000000000000000 ),
 ( -5.017377349295429334E-06, 6.045441312669188748E-05, 0.0001259262036026792043, 0.0002568697845546538379, 0.0003878133655066284716, 0.0004205492607446221706, 0.0004532851559826158155, 0.0005187569464586031052, 0.0005842287369345903949, 0.0006497005274105776846, 0.0007806441083625523724, 0.0008461158988385397706, 0.0009115876893145270603, 0.0009770594797905143500, 0.001042531270266501640, 0.001173474851218476219, 0.001238946641694463509, 0.001304418432170450799, 0.001369890222646438088, 0.001435362013122425378, 0.001500833803598412668, 0.001566305594074400174, 0.001631777384550387681, 0.001697249175026374970, 0.001762720965502362260, 0.001828192755978349550, 0.001893664546454336840, 0.001959136336930324129, 0.002090079917882298709, 0.002155551708358285998, 0.002221023498834273288, 0.002286495289310260578, 0.002351967079786247868, 0.002482910660738222447, 0.002548382451214209737, 0.002613854241690197026, 0.002679326032166184316, 0.002744797822642171606, 0.002810269613118158896, 0.002875741403594146185, 0.003006684984546120765, 0.003072156775022108488, 0.003137628565498095778, 0.003203100355974083067, 0.003268572146450070791, 0.003399515727402045370, 0.003530459308354019950, 0.003563195203592013811, 0.003595931098830007239, 0.003661402889305994529, 0.003726874679781981819, 0.003792346470257969109, 0.003923290051209943688, 0.003988761841685931411, 0.004054233632161918267, 0.004119705422637905123, 0.004185177213113892847, 0.004250649003589880570, 0.004316120794065867426, 0.004381592584541854282, 0.004447064375017842006, 0.004578007955969816585, 0.004643479746445803441, 0.004708951536921791164, 0.004774423327397778888, 0.004839895117873765744, 0.004970838698825740323, 0.005101782279777714903, 0.005232725860729689482, 0.005363669441681664062, 0.005494613022633638641, 0.005625556603585613220, 0.005691028394061600076, 0.005756500184537587800, 0.005821971975013575523, 0.005887443765489562379, 0.006018387346441536959, 0.006083859136917524682, 0.006149330927393512405, 0.006214802717869500129, 0.006280274508345486985, 0.006411218089297461564, 0.006476689879773449288, 0.006542161670249437011, 0.006607633460725424734, 0.006673105251201411590, 0.006738577041677398446, 0.006804048832153386170, 0.006869520622629373893, 0.006934992413105360749, 0.007000464203581347605, 0.007065935994057335329, 0.007131407784533323052, 0.007196879575009309908, 0.007327823155961284488, 0.007393294946437272211, 0.007458766736913259067, 0.007491502632151252061, 0.007524238527389245923, 0.007589710317865233646, 0.007720653898817208226, 0.007786125689293195082, 0.007851597479769182805, 0.007917069270245168794, 0.007982541060721156517, 0.008113484641673131964, 0.008244428222625107411, 0.008309900013101095134, 0.008375371803577081123 ),
 .UNSPECIFIED. ) ;
#131613 = CARTESIAN_POINT ( 'NONE',  ( 5.517805331081858888, 5.539787095791365523, 1.040834085586084257E-14 ) ) ;
#131612 = CARTESIAN_POINT ( 'NONE',  ( -1.642778471875000035, -1.217708332855376607, -2.845375778867859751 ) ) ;
#131611 = CARTESIAN_POINT ( 'NONE',  ( 5.691390622686558487, 9.861982503101517139, 0.7998128361456341429 ) ) ;
#131614 = CARTESIAN_POINT ( 'NONE',  ( -6.303615075710993665, 6.318915441276411471, -0.7998128361456362523 ) ) ;
#131615 = CARTESIAN_POINT ( 'NONE',  ( 3.626185617424378282, 2.007256095728218614, 0.1928357053486499662 ) ) ;
#131616 = CARTESIAN_POINT ( 'NONE',  ( -9.027031348600448979, 9.425958082989001952, 1.040834085586084257E-14 ) ) ;
#131618 = FACE_OUTER_BOUND ( 'NONE', #208621, .T. ) ;
#131617 = CARTESIAN_POINT ( 'NONE',  ( -9.869972641068651242, 11.57768483841065787, 1.082531754730558626 ) ) ;
#131619 = CARTESIAN_POINT ( 'NONE',  ( -1.001543065824772872E-14, 4.821875000341419693, 1.575800808251672791 ) ) ;
#131621 = CARTESIAN_POINT ( 'NONE',  ( 1.364683531249996529, 9.463541667008062319, 0.7879004041258403923 ) ) ;
#131620 = CARTESIAN_POINT ( 'NONE',  ( 5.032170685167933755, 1.114402916724830161, -1.852182961850391774 ) ) ;
#131622 = CARTESIAN_POINT ( 'NONE',  ( -1.124828079527723457, 3.298464558332917740, -0.7749999999999970246 ) ) ;
#131623 = CARTESIAN_POINT ( 'NONE',  ( -11.56423468642480401, 7.060487068201201311, -3.212550277156387857 ) ) ;
#131625 = CARTESIAN_POINT ( 'NONE',  ( 5.853138716089107518, 0.1455171034051294665, -2.011206573937059261 ) ) ;
#131624 = CARTESIAN_POINT ( 'NONE',  ( -7.822691444960716112, 8.228820895316715678, -0.7216878364870267237 ) ) ;
#131626 = CARTESIAN_POINT ( 'NONE',  ( -1.500000000000011324, 5.879166666666686858, -0.8660254037844313801 ) ) ;
#131627 = CARTESIAN_POINT ( 'NONE',  ( 0.3985097114710112742, 1.437023721582047830, -0.9536953323180746844 ) ) ;
#131628 = CARTESIAN_POINT ( 'NONE',  ( 4.441177836928239309, 7.339068688795062911, 1.199719254218452047 ) ) ;
#131630 = CARTESIAN_POINT ( 'NONE',  ( 7.018280793729500644, 8.217024343219755167, -1.199719254218452047 ) ) ;
#131629 = CARTESIAN_POINT ( 'NONE',  ( 8.595506201384020883, 9.130438111143927671, 0.7216878364870438212 ) ) ;
#131631 = CARTESIAN_POINT ( 'NONE',  ( -11.29536259237624485, 7.646265759024179154, -3.923153468842301983 ) ) ;
#131632 = CARTESIAN_POINT ( 'NONE',  ( 6.714126539417144102, -0.8821443205445091973, -1.649434700640100226 ) ) ;
#131633 = CARTESIAN_POINT ( 'NONE',  ( 0.7682272020711936600, 2.010684543107125410, -0.1010625827991030873 ) ) ;
#131634 = CARTESIAN_POINT ( 'NONE',  ( 3.206306947805489305, -2.204311952916749640, 0.1065802224688369715 ) ) ;
#131635 = CARTESIAN_POINT ( 'NONE',  ( -5.872089928050201024, 8.904503111816948646, 1.082531754730550855 ) ) ;
#131636 = ORIENTED_EDGE ( 'NONE', *, *, #138826, .T. ) ;
#131637 = CARTESIAN_POINT ( 'NONE',  ( 9.558135107509954764, 10.25350516829085379, -0.7216878364870257245 ) ) ;
#131639 = CARTESIAN_POINT ( 'NONE',  ( 2.021111450618333194, -1.799914642762674433, 0.9091633978678403949 ) ) ;
#131638 = CARTESIAN_POINT ( 'NONE',  ( 1.963691422110905638, -1.704870618661393999, -1.260721693921822428 ) ) ;
#131641 = EDGE_LOOP ( 'NONE', ( #132540, #103870, #122599, #54598, #98439, #30723, #105224, #187087, #195811, #143142, #65558, #86980, #143876, #109960, #44962, #39974, #190092, #123228, #144260, #102999, #188608, #161649, #9741, #145236, #98978, #210010, #196239, #195458, #194456, #180117, #169343, #141742, #95421, #19465, #165809, #57628, #103292, #174001, #182208, #161530, #67138, #145270, #126089, #179676 ) ) ;
#131640 = CARTESIAN_POINT ( 'NONE',  ( 2.496125854487367235, -0.9279945471987390837, 1.555666070890851627 ) ) ;
#131642 = CARTESIAN_POINT ( 'NONE',  ( 6.502017186205484300, 9.743381262951846367, -1.199719254218452047 ) ) ;
#131643 = STYLED_ITEM ( 'NONE', ( #112015 ), #161027 ) ;
#131644 = CARTESIAN_POINT ( 'NONE',  ( 6.799577732453452761, 7.891594428405881878, -1.199719254218446718 ) ) ;
#131646 = CARTESIAN_POINT ( 'NONE',  ( 0.4092221944725178417, -1.818073194988058194, 0.6039046695034550050 ) ) ;
#131645 = CARTESIAN_POINT ( 'NONE',  ( -4.066556009095094737, 6.831733546331167695, 1.199719254218464037 ) ) ;
#131647 = CARTESIAN_POINT ( 'NONE',  ( 1.843739406749204335, 8.928444911142053186, 0.7750000000000004663 ) ) ;
#131648 = DIRECTION ( 'NONE',  ( -5.578564026256490882E-16, -1.000000000000000000, -9.066213480720158442E-32 ) ) ;
#131649 = CARTESIAN_POINT ( 'NONE',  ( 6.439759776366780208, 6.615400615290456088, 0.7216878364870317197 ) ) ;
#131650 = CARTESIAN_POINT ( 'NONE',  ( 1.364683531249988757, -0.3031249996585799744, 0.000000000000000000 ) ) ;
#131651 = DIRECTION ( 'NONE',  ( 1.000000000000000000, 0.000000000000000000, 0.000000000000000000 ) ) ;
#131652 = CARTESIAN_POINT ( 'NONE',  ( -9.969323024750229578, 10.52529837183042716, -0.7998128361456291469 ) ) ;
#131653 = CARTESIAN_POINT ( 'NONE',  ( 4.680646922328831394, -2.095996545452833981, -0.5284188670612933736 ) ) ;
#131654 = CARTESIAN_POINT ( 'NONE',  ( -6.129694847154222970, 7.284303755502281597, -1.082531754730549967 ) ) ;
#131655 = CARTESIAN_POINT ( 'NONE',  ( 5.316205630334249754, 7.295602216847000498, -1.443375672974078761 ) ) ;
#131656 = CARTESIAN_POINT ( 'NONE',  ( 2.338272602237463360, -1.224740070204191511, -1.730971256048131401 ) ) ;
#131657 = CARTESIAN_POINT ( 'NONE',  ( 4.175484721775176489, 3.976419294354625933, -0.06592222766770190756 ) ) ;
#131658 = CARTESIAN_POINT ( 'NONE',  ( 2.987526725409937800, 1.391544230491305933, 1.396620715705886084 ) ) ;
#131659 = CARTESIAN_POINT ( 'NONE',  ( 5.853752780977106163, -1.389761788226477002, -1.313969904969368496 ) ) ;
#131660 = ORIENTED_EDGE ( 'NONE', *, *, #143969, .T. ) ;
#131661 = DIRECTION ( 'NONE',  ( 0.000000000000000000, -0.000000000000000000, 1.000000000000000000 ) ) ;
#131662 = CARTESIAN_POINT ( 'NONE',  ( 6.268014395358870061, -1.954855384380562722, 0.2394079155795188485 ) ) ;
#131663 = CARTESIAN_POINT ( 'NONE',  ( 1.605311038211139740, -1.927294583035423114, 0.2376585312828301821 ) ) ;
#131664 = EDGE_LOOP ( 'NONE', ( #11171, #81544, #69267, #38679 ) ) ;
#131665 = CARTESIAN_POINT ( 'NONE',  ( 2.282078984650023123, 5.585856895725574311, 0.4608960419188404822 ) ) ;
#131667 = CARTESIAN_POINT ( 'NONE',  ( 1.841070778277279718, 2.501489970915801830, -2.494084679671781046 ) ) ;
#131666 = CARTESIAN_POINT ( 'NONE',  ( -6.943184063974186415, 7.273005294157565359, -0.7216878364870338292 ) ) ;
#131669 = CARTESIAN_POINT ( 'NONE',  ( 5.933664784275179294, 10.07435934829639912, -0.7998128361456291469 ) ) ;
#131668 = CARTESIAN_POINT ( 'NONE',  ( 2.097712127064654819, -2.090152927352141532, 0.05235412406051109108 ) ) ;
#131672 = EDGE_CURVE ( 'NONE', #171990, #193490, #2381, .T. ) ;
#131671 = CARTESIAN_POINT ( 'NONE',  ( 4.163762572728282763, 6.911454530608037494, -1.082531754730548412 ) ) ;
#131670 = CARTESIAN_POINT ( 'NONE',  ( 6.096362627639171805, 10.26417349888772179, -0.7998128361456291469 ) ) ;
#131674 = ORIENTED_EDGE ( 'NONE', *, *, #63108, .F. ) ;
#131673 = CARTESIAN_POINT ( 'NONE',  ( 5.830699381415811899, 1.280921311228696347, -1.420062396151056117 ) ) ;
#131675 = CARTESIAN_POINT ( 'NONE',  ( 4.213639274598267370, -0.3785452818781535611, 2.174016619501429215 ) ) ;
#131676 = CARTESIAN_POINT ( 'NONE',  ( 2.485638465518677176, 2.017858404210779888, -0.8937526715337427152 ) ) ;
#131677 = SURFACE_STYLE_FILL_AREA ( #160939 ) ;
#131678 = CARTESIAN_POINT ( 'NONE',  ( 0.9262460828363194842, -0.8603794558708977025, -1.707882697979688391 ) ) ;
#131679 = CARTESIAN_POINT ( 'NONE',  ( -10.50000000000000000, 12.69999999999998153, 3.599999999999999201 ) ) ;
#131680 = CARTESIAN_POINT ( 'NONE',  ( 11.41126283316785361, 13.75874606908454822, -3.405403429622925415 ) ) ;
#131681 = CARTESIAN_POINT ( 'NONE',  ( 3.807136610393092813, -1.694265131726957252, 1.189645435975445809 ) ) ;
#131683 = CARTESIAN_POINT ( 'NONE',  ( 1.956163130892615731, 2.155914767609674598, -0.1587918856347721730 ) ) ;
#131682 = CARTESIAN_POINT ( 'NONE',  ( -3.521367211247373508, 5.131347717920458962, -1.599625672291256295 ) ) ;
#131684 = CARTESIAN_POINT ( 'NONE',  ( 3.562233144267571650, -1.470601008620987749, 1.625073949779440419 ) ) ;
#131685 = LINE ( 'NONE', #64505, #173050 ) ;
#131686 = DIRECTION ( 'NONE',  ( 3.122502256758252154E-17, 2.602085213965210950E-17, 1.000000000000000000 ) ) ;
#131687 = CARTESIAN_POINT ( 'NONE',  ( 0.4299312922663348080, -6.708819892820487851, 9.481437597266053174 ) ) ;
#131688 = CARTESIAN_POINT ( 'NONE',  ( -0.6823417656250003738, 14.71354166700806410, 1.181850606188754593 ) ) ;
#131689 = CARTESIAN_POINT ( 'NONE',  ( -5.004894982100124068, 5.868074229652107121, 1.199719254218452935 ) ) ;
#131690 = CARTESIAN_POINT ( 'NONE',  ( 0.2115648487451895210, 1.930418618556551946, 0.5826528611774861588 ) ) ;
#131691 = CARTESIAN_POINT ( 'NONE',  ( -8.324343129110692630, 12.65555805069709550, 0.7216878364870338292 ) ) ;
#131692 = CARTESIAN_POINT ( 'NONE',  ( 5.102424979711988051, 2.064335680360945169, 0.1577259720206558580 ) ) ;
#131693 = CARTESIAN_POINT ( 'NONE',  ( 5.360994948850416719, -0.05292929278505505153, -2.116735950649220932 ) ) ;
#131694 = CARTESIAN_POINT ( 'NONE',  ( 4.937140493670735708, 8.911747675924535983, -0.7998128361456281477 ) ) ;
#131695 = CARTESIAN_POINT ( 'NONE',  ( 1.364683531249988535, 5.655208333674751842, -0.7879004041258300672 ) ) ;
#131696 = CARTESIAN_POINT ( 'NONE',  ( 3.748844217038479698, -0.3797678475170936929, -1.932296744971262692 ) ) ;
#131697 = CARTESIAN_POINT ( 'NONE',  ( 5.613300874620239078, -2.237517390240588711, 0.4973276143641935931 ) ) ;
#131698 = CARTESIAN_POINT ( 'NONE',  ( 3.211362085483655981, -0.3553965070040401852, 1.790585553824732612 ) ) ;
#131699 = EDGE_CURVE ( 'NONE', #49891, #7711, #174095, .T. ) ;
#131700 = CARTESIAN_POINT ( 'NONE',  ( 3.607351389687783794, 6.366271167014519783, 1.199719254218451159 ) ) ;
#131701 = CARTESIAN_POINT ( 'NONE',  ( 5.626270559546826533, 5.666329862333828515, 0.7216878364870317197 ) ) ;
#131702 = CARTESIAN_POINT ( 'NONE',  ( -6.073162743917628781, 9.172774736957510555, -1.199719254218440723 ) ) ;
#131703 = CARTESIAN_POINT ( 'NONE',  ( 4.857564175446106525, 8.889184981320973122, 0.7998128361456331437 ) ) ;
#131704 =( BOUNDED_SURFACE ( )  B_SPLINE_SURFACE ( 3, 2, ( 
 ( #126418, #58134, #175105 ),
 ( #154576, #6152, #190252 ),
 ( #192381, #44036, #124293 ),
 ( #188122, #39753, #105858 ) ),
 .UNSPECIFIED., .F., .F., .T. ) 
 B_SPLINE_SURFACE_WITH_KNOTS ( ( 4, 4 ),
 ( 3, 3 ),
 ( 0.01126995942960227343, 0.01373815140602663992 ),
 ( 0.000000000000000000, 1.000000000000000000 ),
 .UNSPECIFIED. ) 
 GEOMETRIC_REPRESENTATION_ITEM ( )  RATIONAL_B_SPLINE_SURFACE ( (
 ( 1.000000000000000000, 0.6947640035331656971, 1.000000000000000000),
 ( 1.000000000000000000, 0.6955505939616358768, 1.000000000000000000),
 ( 1.000000000000000000, 0.6961913616428402340, 1.000000000000000000),
 ( 1.000000000000000000, 0.6967468848049985786, 1.000000000000000000) ) ) 
 REPRESENTATION_ITEM ( '' )  SURFACE ( )  );
#131705 = EDGE_LOOP ( 'NONE', ( #38018, #189933, #20225, #177427 ) ) ;
#131706 = CARTESIAN_POINT ( 'NONE',  ( 3.797138801009732667, -0.2017130330635922841, -2.003102573442970158 ) ) ;
#131707 = CARTESIAN_POINT ( 'NONE',  ( 6.416599408848439268, -1.497502150434773194, -1.744030381972218047 ) ) ;
#131708 = CARTESIAN_POINT ( 'NONE',  ( 4.821123798404616245, -1.750560105953799184, -0.8856655065374097191 ) ) ;
#131709 = CARTESIAN_POINT ( 'NONE',  ( -7.705111371268023923, 7.883718109434487253, 1.040834085586084257E-14 ) ) ;
#131710 = CARTESIAN_POINT ( 'NONE',  ( -5.057354993097396445, 5.859001232490445688, -1.199719254218446718 ) ) ;
#131711 = CARTESIAN_POINT ( 'NONE',  ( -8.013579835756335257, -5.223163706540480788, 7.501945787865621718 ) ) ;
#131712 = CARTESIAN_POINT ( 'NONE',  ( -4.599959256786493533, 8.588645909551377855, 0.000000000000000000 ) ) ;
#131714 = CARTESIAN_POINT ( 'NONE',  ( 5.453870971094811004, 1.767685242813926250, -0.08968725887432274502 ) ) ;
#131713 = CARTESIAN_POINT ( 'NONE',  ( 0.5036076356924833464, -2.080315145378656805, 0.2087293992604210557 ) ) ;
#131715 = DIRECTION ( 'NONE',  ( 0.7592566023652995710, -0.6507913734559650498, 0.000000000000000000 ) ) ;
#131716 = CARTESIAN_POINT ( 'NONE',  ( 1.851786237446376049, 2.185420115623282200, -0.1633297828415938846 ) ) ;
#131717 = CARTESIAN_POINT ( 'NONE',  ( 1.346757998634398712, 0.5060278187854657661, -1.665264516905233361 ) ) ;
#131718 = CARTESIAN_POINT ( 'NONE',  ( 6.205881626753210867, 8.263281202677319470, 1.599625672291281386 ) ) ;
#131719 = FACE_OUTER_BOUND ( 'NONE', #55199, .T. ) ;
#131720 = CARTESIAN_POINT ( 'NONE',  ( 2.086159243269372521, -1.691233086580298695, -0.3380474007560717031 ) ) ;
#131721 = CARTESIAN_POINT ( 'NONE',  ( 1.171705676731093604, 1.309414992938146893, 1.757219779060022580 ) ) ;
#131722 = CARTESIAN_POINT ( 'NONE',  ( 3.774219598512587037, 1.225428716765289749, 1.835190637982798023 ) ) ;
#131723 = CARTESIAN_POINT ( 'NONE',  ( 1.165147980530324201, 1.645521545068162617, -1.416405498411864583 ) ) ;
#131724 = CARTESIAN_POINT ( 'NONE',  ( -1.230728480726517748, 2.980010058876359835, 0.7750000000000170086 ) ) ;
#131725 = CARTESIAN_POINT ( 'NONE',  ( 2.044302899665669138, 0.9103292306275132528, 1.911821358334654608 ) ) ;
#131726 = CARTESIAN_POINT ( 'NONE',  ( 6.827182134110222123, 7.629137130509067610, 2.789055895399249252 ) ) ;
#131727 = ORIENTED_EDGE ( 'NONE', *, *, #208458, .F. ) ;
#131729 = CARTESIAN_POINT ( 'NONE',  ( -1.402160292154681736E-14, 0.3843750003414230232, 1.575800808251672791 ) ) ;
#131728 = CARTESIAN_POINT ( 'NONE',  ( 2.736170862265740578, 2.275407485025813692, 0.2777600125268233633 ) ) ;
#131730 = CARTESIAN_POINT ( 'NONE',  ( 0.07755575628183573877, 5.720052600789671260, -2.782970829007725744 ) ) ;
#131731 = CARTESIAN_POINT ( 'NONE',  ( 5.518332215962025167, 6.396807992499198292, -1.199719254218445830 ) ) ;
#131732 = CARTESIAN_POINT ( 'NONE',  ( 4.442156590966897411, -1.366343709131916828, -1.751266766990001944 ) ) ;
#131733 = CARTESIAN_POINT ( 'NONE',  ( -8.026063749610063525, 8.466088584074293877, -0.7216878364870278340 ) ) ;
#131734 = EDGE_CURVE ( 'NONE', #157380, #196200, #177578, .T. ) ;
#131735 = CARTESIAN_POINT ( 'NONE',  ( -3.740297717422789159, 7.429476292658450554, -2.448395595369508015 ) ) ;
#131736 = CARTESIAN_POINT ( 'NONE',  ( 5.341549334104194635, 6.294524313618772737, 1.082531754730558626 ) ) ;
#131737 = CARTESIAN_POINT ( 'NONE',  ( -6.507550544435101614, 10.53596670190887963, 0.000000000000000000 ) ) ;
#131738 = CIRCLE ( 'NONE', #204322, 0.1000000000000000333 ) ;
#131739 = CARTESIAN_POINT ( 'NONE',  ( 5.234856708652235291, 5.279956712948652431, 0.7216878364870338292 ) ) ;
#131740 = ORIENTED_EDGE ( 'NONE', *, *, #161304, .T. ) ;
#131741 = CARTESIAN_POINT ( 'NONE',  ( 3.516250148862578584, -1.862017090670412767, 0.7743150488077471527 ) ) ;
#131743 = CARTESIAN_POINT ( 'NONE',  ( 0.6376417299419987472, 1.925892387546113582, -0.7388170802648945656 ) ) ;
#131742 = CARTESIAN_POINT ( 'NONE',  ( 6.425674737872927089, 9.584038729905381970, -1.199719254218440723 ) ) ;
#131744 = CARTESIAN_POINT ( 'NONE',  ( 6.983263157960366563, -0.003091553303710344557, 1.945923119799706669 ) ) ;
#131745 = CARTESIAN_POINT ( 'NONE',  ( 4.380693030546905398, 8.124909279031149012, 0.7216878364870247253 ) ) ;
#131746 = CARTESIAN_POINT ( 'NONE',  ( 0.7500000000000006661, 8.697916667349467446, -1.299038105676657340 ) ) ;
#131747 = CARTESIAN_POINT ( 'NONE',  ( 0.6823417656249917140, 3.342708333674754506, 1.181850606188765695 ) ) ;
#131748 = CARTESIAN_POINT ( 'NONE',  ( 4.119203469048302146, -2.097337170177868693, 0.6352863671069891582 ) ) ;
#131749 = CARTESIAN_POINT ( 'NONE',  ( 1.828750219146151323, 0.7691198443132395424, -1.864169014999479623 ) ) ;
#131750 = CARTESIAN_POINT ( 'NONE',  ( 0.8547319020580852467, 0.3593373433725781108, -1.805665335529122784 ) ) ;
#131751 = CARTESIAN_POINT ( 'NONE',  ( 8.118635056484817980, 8.366162408854107113, 0.7998128361456481317 ) ) ;
#131752 =( NAMED_UNIT ( * ) PLANE_ANGLE_UNIT ( ) SI_UNIT ( $, .RADIAN. ) );
#131753 = CARTESIAN_POINT ( 'NONE',  ( 4.770415466175468744, -1.191763575130764696, 1.382976834283907053 ) ) ;
#131754 = CARTESIAN_POINT ( 'NONE',  ( 6.082657761774013849, -0.6767167302549759178, 1.899617564980569995 ) ) ;
#131755 = CARTESIAN_POINT ( 'NONE',  ( -7.283754839039664475, 9.520799950344851936, -1.599625672291263179 ) ) ;
#131757 = CARTESIAN_POINT ( 'NONE',  ( -5.956828388357799042, 8.042995434541133193, 1.599625672291263179 ) ) ;
#131756 = CARTESIAN_POINT ( 'NONE',  ( 4.100629699907013759, -0.7064081464536530186, -2.149486123859779330 ) ) ;
#131758 = CARTESIAN_POINT ( 'NONE',  ( 0.6277293814327978838, -1.999128025905463568, 0.6627883249872651428 ) ) ;
#131759 = CARTESIAN_POINT ( 'NONE',  ( -5.427006627220116286, 9.553534508390610469, -0.7998128361456362523 ) ) ;
#131760 = CARTESIAN_POINT ( 'NONE',  ( 4.703616579153604427, -1.598285800263723910, -1.315984976451072930 ) ) ;
#131761 = CARTESIAN_POINT ( 'NONE',  ( 10.24048609702354717, 10.84165528948263457, -0.7998128361456281477 ) ) ;
#131762 = CARTESIAN_POINT ( 'NONE',  ( -1.360316468750026875, 2.671875000341383810, -2.602085213965210642E-14 ) ) ;
#131763 = APPLICATION_PROTOCOL_DEFINITION ( 'draft international standard', 'automotive_design', 1998, #211010 ) ;
#131764 = CARTESIAN_POINT ( 'NONE',  ( -7.934546212495630968, 10.28005655271014795, -1.599625672291263179 ) ) ;
#131765 = UNCERTAINTY_MEASURE_WITH_UNIT (LENGTH_MEASURE( 1.000000000000000082E-05 ), #160410, 'distance_accuracy_value', 'NONE');
#131766 = LINE ( 'NONE', #179422, #30205 ) ;
#131767 = CARTESIAN_POINT ( 'NONE',  ( 5.854088466050551887, 10.05179665369283981, 0.7998128361456341429 ) ) ;
#131768 = CARTESIAN_POINT ( 'NONE',  ( 5.718470792885002041, 6.083800970187063228, -0.6820517675651931455 ) ) ;
#131769 = CARTESIAN_POINT ( 'NONE',  ( -9.110716038703348119, 12.61262389758715408, 1.082531754730560403 ) ) ;
#131771 = CARTESIAN_POINT ( 'NONE',  ( 1.652877544743835969, 2.198119390704804665, 0.3199964322739051736 ) ) ;
#131770 = CARTESIAN_POINT ( 'NONE',  ( 0.2992908618118708675, -0.2657624787030036240, -2.103842954668332599 ) ) ;
#131772 = CARTESIAN_POINT ( 'NONE',  ( -1.500000000000022204, 7.388542872122518368, 4.154462424328226433 ) ) ;
#131774 = CARTESIAN_POINT ( 'NONE',  ( -7.286581212701773502, 7.465709267765667789, 0.7998128361456341429 ) ) ;
#131773 = AXIS2_PLACEMENT_3D ( 'NONE', #8241, #7157, #42912 ) ;
#131775 = CARTESIAN_POINT ( 'NONE',  ( 5.113396490648394632, 9.117379672398465473, 1.040834085586084257E-14 ) ) ;
#131776 = CARTESIAN_POINT ( 'NONE',  ( 3.156644782993088150, -0.5669402238272451822, -1.878178299617596192 ) ) ;
#131777 = CARTESIAN_POINT ( 'NONE',  ( 5.986088515633498197, 6.942523675449257858, -1.199719254218446718 ) ) ;
#131778 = CARTESIAN_POINT ( 'NONE',  ( -4.274576072154308903, 7.290118009659216192, 0.9321895248279310486 ) ) ;
#131779 = CARTESIAN_POINT ( 'NONE',  ( 3.440018289565364817, 5.036440642624797626, 1.599625672291267398 ) ) ;
#131780 = CARTESIAN_POINT ( 'NONE',  ( -6.129694847154222970, 7.284303755502281597, -1.082531754730549967 ) ) ;
#131781 = CARTESIAN_POINT ( 'NONE',  ( -7.456621297836087514, 9.722477485607340597, 1.443375672974090751 ) ) ;
#131782 = CARTESIAN_POINT ( 'NONE',  ( 1.810938747355747447, -0.5704394276861005642, -2.042344090522000055 ) ) ;
#131783 = CARTESIAN_POINT ( 'NONE',  ( -6.784929528996132220, 6.880448970109080520, 0.000000000000000000 ) ) ;
#131784 = CARTESIAN_POINT ( 'NONE',  ( 4.053139552913617827, 1.658577106941661272, -1.047563642765911185 ) ) ;
#131785 = CARTESIAN_POINT ( 'NONE',  ( 2.835029207381420502, 0.2633842809251253358, 2.145520918749081574 ) ) ;
#131786 = CARTESIAN_POINT ( 'NONE',  ( 3.052128622409277181, -1.392423357299840792, 1.204796875372941667 ) ) ;
#131787 = CARTESIAN_POINT ( 'NONE',  ( -4.105200985651542567, 7.499488806860944656, 0.5979674706809139373 ) ) ;
#131788 = CARTESIAN_POINT ( 'NONE',  ( 1.364683531249986537, -1.073958332991911790, 0.7879004041258500513 ) ) ;
#131789 = ADVANCED_FACE ( 'NONE', ( #82190 ), #94619, .F. ) ;
#131790 = CARTESIAN_POINT ( 'NONE',  ( 4.945099085969404840, 0.5415675326034079529, -1.653987846916603610 ) ) ;
#131791 = CARTESIAN_POINT ( 'NONE',  ( -1.123270288250318494, 3.297697346350006331, -0.7749999999993560929 ) ) ;
#131792 = CARTESIAN_POINT ( 'NONE',  ( 5.205967797967541166, 5.175976640491323444, -0.7216878364870197293 ) ) ;
#131793 = CARTESIAN_POINT ( 'NONE',  ( -10.44369227015510404, 5.112964020592957404, 5.232143560358708534 ) ) ;
#131794 = CARTESIAN_POINT ( 'NONE',  ( 2.044033295145482043, 0.8276103948961744949, -1.997198329219296742 ) ) ;
#131795 = CARTESIAN_POINT ( 'NONE',  ( 4.464220131058834085, 1.617570847575640736, 1.203168917025834839 ) ) ;
#131796 = CARTESIAN_POINT ( 'NONE',  ( -9.666600336419303829, 11.34041714965307968, 1.082531754730558626 ) ) ;
#131797 = CARTESIAN_POINT ( 'NONE',  ( 1.165152350680317195, -1.954565670758709128, -0.9236901323337529668 ) ) ;
#131798 = CARTESIAN_POINT ( 'NONE',  ( 2.600799297785437947, 1.585616864491301348, -1.171192495528531330 ) ) ;
#131799 = CARTESIAN_POINT ( 'NONE',  ( -6.599398278744054380, 6.760864547338558239, 0.4146307598744238820 ) ) ;
#131800 = CARTESIAN_POINT ( 'NONE',  ( 3.104954810669264376, -0.3761875069782861236, 1.905116956637223913 ) ) ;
#131803 = ORIENTED_EDGE ( 'NONE', *, *, #163561, .T. ) ;
#131802 = CARTESIAN_POINT ( 'NONE',  ( -5.343321937561608337, 5.406499480009534508, 0.7216878364870257245 ) ) ;
#131801 = CARTESIAN_POINT ( 'NONE',  ( -1.115562610750309283E-14, 11.56249999999999822, 1.500000000000001554 ) ) ;
#131804 = CARTESIAN_POINT ( 'NONE',  ( -4.624739795592948788, 5.528522862014106920, -1.082531754730549967 ) ) ;
#131805 = CARTESIAN_POINT ( 'NONE',  ( 5.273195401072370281, 5.116759154198018855, -0.7998128361456481317 ) ) ;
#131806 = ADVANCED_FACE ( 'NONE', ( #96345 ), #46516, .T. ) ;
#131808 = ORIENTED_EDGE ( 'NONE', *, *, #120547, .T. ) ;
#131807 = CARTESIAN_POINT ( 'NONE',  ( -5.926849427829407269, 6.943687749669614995, -1.199719254218453823 ) ) ;
#131809 = CARTESIAN_POINT ( 'NONE',  ( -9.531018800282611281, 12.14260790512831889, 1.443375672974076540 ) ) ;
#131810 = CARTESIAN_POINT ( 'NONE',  ( 1.220068447022312652, -2.152735442661047216, 0.4846846590640523367 ) ) ;
#131811 = CARTESIAN_POINT ( 'NONE',  ( 3.285556943750000070, -3.784374999522041705, 0.000000000000000000 ) ) ;
#131812 = CARTESIAN_POINT ( 'NONE',  ( 5.787936641206399280, -1.241742415844361291, -1.518776266119965745 ) ) ;
#131813 = ORIENTED_EDGE ( 'NONE', *, *, #116113, .T. ) ;
#131814 = CARTESIAN_POINT ( 'NONE',  ( 3.345011933649364444, -1.869310496227539531, -0.9943253416123465360 ) ) ;
#131815 = CARTESIAN_POINT ( 'NONE',  ( -1.201851678989727383E-14, 2.993750000682821266, 1.732050807568877637 ) ) ;
#131816 = CARTESIAN_POINT ( 'NONE',  ( 0.07459516483346911864, 0.7642615113957001993, -1.841455071455591064 ) ) ;
#131817 = CARTESIAN_POINT ( 'NONE',  ( 4.277188459880359339, 1.204364621523913437, 1.392669941884729035 ) ) ;
#131818 = ORIENTED_EDGE ( 'NONE', *, *, #168064, .F. ) ;
#131819 = CARTESIAN_POINT ( 'NONE',  ( -9.643927338022246332, 10.14567007064778004, -0.7998128361456291469 ) ) ;
#131820 = CARTESIAN_POINT ( 'NONE',  ( -4.284013352238262407, 6.021101549076499637, -1.443375672974053892 ) ) ;
#131821 = CARTESIAN_POINT ( 'NONE',  ( 5.326475955075804514, -0.9554483686352827077, -1.893264085526874974 ) ) ;
#131822 = CARTESIAN_POINT ( 'NONE',  ( -5.514013019825418915, 5.994650414344389056, -0.9619886414689113874 ) ) ;
#131823 = CARTESIAN_POINT ( 'NONE',  ( 5.099838337034727331, 9.101561826515851550, -0.7998128361456281477 ) ) ;
#131824 = ORIENTED_EDGE ( 'NONE', *, *, #77409, .T. ) ;
#131825 = CARTESIAN_POINT ( 'NONE',  ( 5.307911771147946212, -2.051258671218537444, 0.1976249854395220606 ) ) ;
#131828 = CARTESIAN_POINT ( 'NONE',  ( 3.104851637799400876, -0.3563606998662186554, 1.806257425991746546 ) ) ;
#131827 = CARTESIAN_POINT ( 'NONE',  ( 0.7306206827372868640, -1.750454575335522067, -0.6323700682324316924 ) ) ;
#131826 = CARTESIAN_POINT ( 'NONE',  ( -6.343551558972118976, 6.506286488053500072, -2.500000000000000000 ) ) ;
#131829 = CARTESIAN_POINT ( 'NONE',  ( 8.769426429940780920, 9.125419011219408461, 0.7998128361456462443 ) ) ;
#131830 = PRODUCT_DEFINITION_FORMATION_WITH_SPECIFIED_SOURCE ( 'ANY', '', #192368, .NOT_KNOWN. ) ;
#131831 = CARTESIAN_POINT ( 'NONE',  ( -4.826164018371312814, 5.074823732154670530, -0.9293088092043750859 ) ) ;
#131833 = ORIENTED_EDGE ( 'NONE', *, *, #121592, .F. ) ;
#131832 = CARTESIAN_POINT ( 'NONE',  ( -0.06856108760742431196, -7.850763007174490049, -9.549252947205625119 ) ) ;
#131834 = CARTESIAN_POINT ( 'NONE',  ( 3.897267319706390065, 1.864829029706360330, -1.179861312946443697 ) ) ;
#131835 = CARTESIAN_POINT ( 'NONE',  ( 4.446707141204663039, 0.5976617499744775186, 2.181999625662895959 ) ) ;
#131836 = CARTESIAN_POINT ( 'NONE',  ( -6.073689629242160493, 8.109057205581079231, -1.443375672974059665 ) ) ;
#131837 = CARTESIAN_POINT ( 'NONE',  ( 4.992358684838777982, -0.9999893916136384231, 1.510367140083505699 ) ) ;
#131838 = CARTESIAN_POINT ( 'NONE',  ( 5.383970194100923479, -1.915903400165029469, 0.006849619181082886032 ) ) ;
#131839 = CARTESIAN_POINT ( 'NONE',  ( -0.6823417656250212460, 4.863541667008086655, 1.181850606188767472 ) ) ;
#131840 = CARTESIAN_POINT ( 'NONE',  ( 5.682452175617663137, -1.825344843996518529, -0.4084625512627630406 ) ) ;
#131841 = CARTESIAN_POINT ( 'NONE',  ( 6.478945253086064504, 1.736940705955980269, 0.6686975948369151546 ) ) ;
#131842 = CARTESIAN_POINT ( 'NONE',  ( 6.455894400631252417, 1.764744506579400962, -0.1349141608881914423 ) ) ;
#131843 = FACE_OUTER_BOUND ( 'NONE', #138252, .T. ) ;
#131845 = CARTESIAN_POINT ( 'NONE',  ( 2.789785578339375238, 1.489779160094312660, 1.488918557309417467 ) ) ;
#131844 = CARTESIAN_POINT ( 'NONE',  ( -2.941756144040963417, 6.375873234782333476, -0.7216878364870257245 ) ) ;
#131846 = EDGE_CURVE ( 'NONE', #155820, #97415, #96913, .T. ) ;
#131847 = CARTESIAN_POINT ( 'NONE',  ( 3.728129053633592704, 4.412200653069714207, -1.082531754730543083 ) ) ;
#131849 = CARTESIAN_POINT ( 'NONE',  ( -10.17947440576205054, 10.77047498301088346, 0.7998128361456462443 ) ) ;
#131848 = FACE_OUTER_BOUND ( 'NONE', #87649, .T. ) ;
#131850 = DIRECTION ( 'NONE',  ( 0.000000000000000000, 1.000000000000000000, 0.000000000000000000 ) ) ;
#131851 = CARTESIAN_POINT ( 'NONE',  ( 1.810812951734928511, -0.5429070200502202903, -1.945354291398709412 ) ) ;
#131852 = CARTESIAN_POINT ( 'NONE',  ( 1.364683531249986537, 1.905208333674750287, -0.7879004041258239610 ) ) ;
#131853 = ADVANCED_FACE ( 'NONE', ( #61686 ), #51334, .T. ) ;
#131854 = CARTESIAN_POINT ( 'NONE',  ( 2.835626683552519012, 6.459981564119914310, 0.000000000000000000 ) ) ;
#131855 = CARTESIAN_POINT ( 'NONE',  ( 3.532649767544591590, 2.108058052951222283, 0.4773693597190583060 ) ) ;
#131856 = CARTESIAN_POINT ( 'NONE',  ( 6.609999999999999432, 2.404169510734831761, 2.660384318335922149 ) ) ;
#131859 = DIRECTION ( 'NONE',  ( -0.000000000000000000, -1.000000000000000000, -0.000000000000000000 ) ) ;
#131858 = CARTESIAN_POINT ( 'NONE',  ( 11.97929049433705551, 9.799999999999998934, -0.7046979865771820783 ) ) ;
#131857 = CARTESIAN_POINT ( 'NONE',  ( 3.410758162289653672, 6.136912401716668519, -1.199719254218453823 ) ) ;
#131860 = CARTESIAN_POINT ( 'NONE',  ( 9.124274191872634887, 11.66807252865000244, -1.443375672974058777 ) ) ;
#131861 = CARTESIAN_POINT ( 'NONE',  ( 6.925078400183548588, 0.0006614011395407459748, 1.855452278108092656 ) ) ;
#131862 = CARTESIAN_POINT ( 'NONE',  ( -6.399085315970132193, 10.40942393536641397, -0.7216878364870278340 ) ) ;
#131863 = CARTESIAN_POINT ( 'NONE',  ( -1.364683531250000748, 0.7593750003414210248, 0.000000000000000000 ) ) ;
#131864 = CARTESIAN_POINT ( 'NONE',  ( 1.136565065649897344, 0.4323997850379875385, 2.148315308122191514 ) ) ;
#131865 = CARTESIAN_POINT ( 'NONE',  ( 0.4886806171078367234, 7.337544960129623206, 1.941936010599545792 ) ) ;
#131866 = CARTESIAN_POINT ( 'NONE',  ( 1.921153072736818013, 2.111338651666348376, 0.8135812809707074766 ) ) ;
#131867 = CARTESIAN_POINT ( 'NONE',  ( -8.532158741701643123, 8.848606708273724308, 0.7998128361456462443 ) ) ;
#131868 = CARTESIAN_POINT ( 'NONE',  ( -5.246642258364192735, 5.223430177620739023, 0.7216878364870317197 ) ) ;
#131869 = CARTESIAN_POINT ( 'NONE',  ( -0.6823417656250212460, 3.113541667008084879, 1.181850606188767472 ) ) ;
#131870 = CARTESIAN_POINT ( 'NONE',  ( 4.789099507923308963, 8.141322699134850183, 0.8117711051834965996 ) ) ;
#131871 = CARTESIAN_POINT ( 'NONE',  ( -1.402160292154681736E-14, 10.56250000000000178, 1.732050807568881190 ) ) ;
#131872 = CARTESIAN_POINT ( 'NONE',  ( 5.239300017038202917, 5.077214539491492928, 0.000000000000000000 ) ) ;
#131873 = CARTESIAN_POINT ( 'NONE',  ( 2.917004591651660927, -0.1773711190117404635, 1.760840049638369154 ) ) ;
#131874 = CARTESIAN_POINT ( 'NONE',  ( 8.238550898598388628, 12.76339314834017102, 0.7998128361456462443 ) ) ;
#131875 = CARTESIAN_POINT ( 'NONE',  ( 6.545939543708723107, 0.8506627741289953804, -2.036432556493542823 ) ) ;
#131876 = CARTESIAN_POINT ( 'NONE',  ( 1.364683531250000303, 8.755208333674731946, -0.7879004041258355073 ) ) ;
#131877 = ORIENTED_EDGE ( 'NONE', *, *, #10916, .F. ) ;
#131878 = CARTESIAN_POINT ( 'NONE',  ( -7.123883369337781879, 7.275895117174344229, 0.7998128361456341429 ) ) ;
#131879 = CARTESIAN_POINT ( 'NONE',  ( 5.677361293727043901, 1.528752376640944100, 1.314985542479940817 ) ) ;
#131880 = ORIENTED_EDGE ( 'NONE', *, *, #93674, .T. ) ;
#131881 = CARTESIAN_POINT ( 'NONE',  ( 2.799504582125960095, -0.5885537693137884441, 1.775713401224961574 ) ) ;
#131882 = CARTESIAN_POINT ( 'NONE',  ( 3.625891163443736076, 2.020865133175090644, -0.4488579359705275329 ) ) ;
#131883 = CIRCLE ( 'NONE', #52380, 0.08000000000000020983 ) ;
#131884 = CARTESIAN_POINT ( 'NONE',  ( -7.390603132780795725, 8.755363422066633206, -1.082531754730549967 ) ) ;
#131885 = CARTESIAN_POINT ( 'NONE',  ( 1.916128293556786044, -1.911906470838855343, 0.05044092668918254141 ) ) ;
#131886 = CARTESIAN_POINT ( 'NONE',  ( -10.97030176249251276, 11.29999999999998117, 1.695215491223428739 ) ) ;
#131887 = CARTESIAN_POINT ( 'NONE',  ( -10.19200560444942560, 4.477620260464512114, -5.707107691925500603 ) ) ;
#131888 = CARTESIAN_POINT ( 'NONE',  ( -4.446850669412495627, 7.248452911037940538, 1.092318573022862616 ) ) ;
#131889 = CARTESIAN_POINT ( 'NONE',  ( 1.364683531249990311, 4.676041667008083103, 0.7879004041258500513 ) ) ;
#131890 = CARTESIAN_POINT ( 'NONE',  ( 1.230557176020011134, 1.282188879665364656, -1.419081615486268433 ) ) ;
#131891 = CARTESIAN_POINT ( 'NONE',  ( 2.840232074097197579, -1.010955899468408248, 1.681206195012739046 ) ) ;
#131892 = CARTESIAN_POINT ( 'NONE',  ( 7.097136523687877840, -8.233137084989836652, -6.434831245971841973 ) ) ;
#131893 = CARTESIAN_POINT ( 'NONE',  ( -3.461074353238556167, 7.259946855412102273, 0.000000000000000000 ) ) ;
#131895 = DIRECTION ( 'NONE',  ( 0.000000000000000000, 1.000000000000000000, 0.000000000000000000 ) ) ;
#131894 = CARTESIAN_POINT ( 'NONE',  ( 10.24726517383036928, 10.84956421242393887, 0.000000000000000000 ) ) ;
#131896 = CARTESIAN_POINT ( 'NONE',  ( 6.221945801152132027, -1.093087313283289230, -1.640361058829779228 ) ) ;
#131897 = CARTESIAN_POINT ( 'NONE',  ( -1.402160292154681736E-14, 2.446875000341416584, -1.575800808251660134 ) ) ;
#131898 = CARTESIAN_POINT ( 'NONE',  ( 2.109637220322407192, 1.559014694980038085, 1.273805747723085746 ) ) ;
#131899 = ADVANCED_FACE ( 'NONE', ( #35312 ), #3853, .F. ) ;
#131901 = CARTESIAN_POINT ( 'NONE',  ( 2.566138216211190759, -1.085845923642224209, 1.817437617555809792 ) ) ;
#131900 = CARTESIAN_POINT ( 'NONE',  ( -5.910991785878158211, 9.839981483592442402, -0.7216878364870278340 ) ) ;
#131902 = CARTESIAN_POINT ( 'NONE',  ( 8.628029272663843230, 13.71747347301596598, -8.342125298644845088 ) ) ;
#131903 = CARTESIAN_POINT ( 'NONE',  ( 4.299325596424930396, -1.802881993240162961, 1.017688063649782482 ) ) ;
#131904 = CARTESIAN_POINT ( 'NONE',  ( 3.627688620108284745, 6.389997935838436227, 1.199719254218452047 ) ) ;
#131906 = CARTESIAN_POINT ( 'NONE',  ( 5.529027716274630855, 5.344953845275508542, 1.040834085586084257E-14 ) ) ;
#131905 = CARTESIAN_POINT ( 'NONE',  ( 5.630836714711354496, -1.890471120482087652, 0.8929869209393003215 ) ) ;
#131908 = ORIENTED_EDGE ( 'NONE', *, *, #171344, .T. ) ;
#131907 = CARTESIAN_POINT ( 'NONE',  ( 4.682524874021861017, -1.770931954651306262, -0.4427778663074270482 ) ) ;
#131909 = CARTESIAN_POINT ( 'NONE',  ( 9.028840231696797503, 12.62106513936658203, -1.199719254218446718 ) ) ;
#131910 = CARTESIAN_POINT ( 'NONE',  ( 11.05511614931255160, 7.767163931695388435, -1.611817371847934943 ) ) ;
#131911 = CARTESIAN_POINT ( 'NONE',  ( 5.227635310461984375, -2.096914331502324647, 0.6878394029543041244 ) ) ;
#131912 = CARTESIAN_POINT ( 'NONE',  ( -0.6823417656250039265, 11.13020833367473017, -1.181850606188755259 ) ) ;
#131913 = ORIENTED_EDGE ( 'NONE', *, *, #145950, .F. ) ;
#131914 = CARTESIAN_POINT ( 'NONE',  ( 4.336511155197938727, 1.173803677898217712, -1.509565991254034678 ) ) ;
#131915 = CARTESIAN_POINT ( 'NONE',  ( -9.646789991323334590, 11.21334206375407305, 1.199719254218462483 ) ) ;
#131916 = CARTESIAN_POINT ( 'NONE',  ( 6.272618624616828953, 10.46980549536166016, 1.040834085586084257E-14 ) ) ;
#131917 = B_SPLINE_CURVE_WITH_KNOTS ( 'NONE', 3,
 ( #57741, #142224, #191982, #109764, #107623, #173654 ),
 .UNSPECIFIED., .F., .F.,
 ( 4, 2, 4 ),
 ( 0.000000000000000000, 0.0003157158648874024685, 0.0006314317297748052622 ),
 .UNSPECIFIED. ) ;
#131918 = CARTESIAN_POINT ( 'NONE',  ( -1.360316468750021768, 1.421875000341424222, -4.510281037539698445E-14 ) ) ;
#131919 = CARTESIAN_POINT ( 'NONE',  ( 5.300874872818843286, 5.286701561151180506, 0.7216878364870317197 ) ) ;
#131920 = CARTESIAN_POINT ( 'NONE',  ( 0.000000000000000000, 1.000000000000000888, 0.000000000000000000 ) ) ;
#131921 = CARTESIAN_POINT ( 'NONE',  ( 8.207694362149334566, 14.14762995341124707, -8.754715811281320370 ) ) ;
#131922 = CARTESIAN_POINT ( 'NONE',  ( 0.1691535571452691677, 1.059206136818511501, 1.505872603892892458 ) ) ;
#131923 = EDGE_LOOP ( 'NONE', ( #165510, #175850, #70452, #168529 ) ) ;
#131924 = ORIENTED_EDGE ( 'NONE', *, *, #113521, .T. ) ;
#131925 = VECTOR ( 'NONE', #4743, 1000.000000000000000 ) ;
#131926 = CARTESIAN_POINT ( 'NONE',  ( 0.000000000000000000, -5.199999999999996625, 0.000000000000000000 ) ) ;
#131927 = CARTESIAN_POINT ( 'NONE',  ( 4.464026755505964950, 0.8799173153972823513, 1.650629236088823282 ) ) ;
#131928 = CARTESIAN_POINT ( 'NONE',  ( 7.856023664475727308, 8.130058794835305136, -0.7998128361456341429 ) ) ;
#131929 = CARTESIAN_POINT ( 'NONE',  ( -11.04536101718726293, 13.50581159806359643, -1.100000000000000311 ) ) ;
#131930 = CARTESIAN_POINT ( 'NONE',  ( -6.968527767744110868, 9.153035033833367251, 1.443375672974078761 ) ) ;
#131931 = CARTESIAN_POINT ( 'NONE',  ( 4.690231075323689325, 7.559354456931247412, 1.199719254218462483 ) ) ;
#131932 = CARTESIAN_POINT ( 'NONE',  ( 1.639439270303972851, 1.821716124042528584, -0.7488776562727271768 ) ) ;
#131933 = CARTESIAN_POINT ( 'NONE',  ( 2.372672929649359386, -0.3474902101525711440, -1.986097784353996643 ) ) ;
#131934 = CARTESIAN_POINT ( 'NONE',  ( -8.857554428429624593, 9.228235009456373206, 0.7998128361456462443 ) ) ;
#131935 = CARTESIAN_POINT ( 'NONE',  ( 7.042534447655770080, 7.180988041878682004, -0.7998128361456341429 ) ) ;
#131936 = CARTESIAN_POINT ( 'NONE',  ( 6.773846765317334651, -7.246166700180801001, 6.773846765317318663 ) ) ;
#131937 = CARTESIAN_POINT ( 'NONE',  ( 2.045129345224237394, -1.761195505111545989, -1.303888621850733509 ) ) ;
#131938 = CARTESIAN_POINT ( 'NONE',  ( 2.370092853298483959, 0.1904551827020779520, -0.4476525039842664810 ) ) ;
#131939 = CARTESIAN_POINT ( 'NONE',  ( -9.378489572351046633, 11.96465713920816043, -1.599625672291263179 ) ) ;
#131940 = DIRECTION ( 'NONE',  ( -1.207943261119674327E-30, -2.168404344971008079E-15, -1.000000000000000000 ) ) ;
#131941 = DIRECTION ( 'NONE',  ( 0.000000000000000000, 0.08676576675288256990, 0.9962287396576072762 ) ) ;
#131942 = CARTESIAN_POINT ( 'NONE',  ( 4.095971805104285934, 6.832365301713403838, 1.082531754730549078 ) ) ;
#131943 = CARTESIAN_POINT ( 'NONE',  ( 9.094822116668764167, 9.505047312402055582, 0.7998128361456462443 ) ) ;
#131944 = CARTESIAN_POINT ( 'NONE',  ( -2.065088895208611941, 8.523968132013475696, -2.459875961809982137 ) ) ;
#131945 = CARTESIAN_POINT ( 'NONE',  ( 6.048345925472178308, 9.110135108809304327, 1.082531754730549967 ) ) ;
#131946 = ORIENTED_EDGE ( 'NONE', *, *, #84582, .F. ) ;
#131948 = CARTESIAN_POINT ( 'NONE',  ( 1.313140557769366890, 1.644527964066449632, -1.160800818697106163 ) ) ;
#131947 = CARTESIAN_POINT ( 'NONE',  ( 4.968220237687512864, -1.735557695065930606, -0.6152675618510683453 ) ) ;
#131949 = CARTESIAN_POINT ( 'NONE',  ( 3.181363629901075463, -1.130666556857576444, -2.000962643106804606 ) ) ;
#131951 = CARTESIAN_POINT ( 'NONE',  ( 1.252544054828262476, -0.4453625992760417707, -1.806759803163625167 ) ) ;
#131950 = CARTESIAN_POINT ( 'NONE',  ( -3.104453987849326690, 4.644948957289396496, 1.040834085586084257E-14 ) ) ;
#131952 = CARTESIAN_POINT ( 'NONE',  ( -1.642778471875000035, -3.317708332855374476, -2.845375778867859751 ) ) ;
#131953 = SURFACE_STYLE_USAGE ( .BOTH. , #180659 ) ;
#131954 = CARTESIAN_POINT ( 'NONE',  ( 5.853752780977106163, -1.389761788226477002, -1.313969904969368496 ) ) ;
#131955 = CARTESIAN_POINT ( 'NONE',  ( -9.806625181386236179, 10.33548422123910449, -0.7998128361456291469 ) ) ;
#131956 = CARTESIAN_POINT ( 'NONE',  ( -4.963693636378939011, 8.805076652501815815, 0.7216878364870267237 ) ) ;
#131958 = CARTESIAN_POINT ( 'NONE',  ( 2.781945002432617997, -0.9632652739061451364, 1.603442845774772474 ) ) ;
#131957 = CARTESIAN_POINT ( 'NONE',  ( 3.614856758894122724, -0.1514882961727741506, 2.085299387778175806 ) ) ;
#131959 = CARTESIAN_POINT ( 'NONE',  ( 7.293923454472087897, 8.572294120714675003, 1.082531754730558626 ) ) ;
#131960 = CARTESIAN_POINT ( 'NONE',  ( 0.6823417656249899377, 4.988541667008086655, -1.181850606188754593 ) ) ;
#131961 = CARTESIAN_POINT ( 'NONE',  ( 6.339398910184078417, 0.6979989802004606947, -1.704029730133400866 ) ) ;
#131962 = CARTESIAN_POINT ( 'NONE',  ( 3.928111819657337911, 5.605883094398769195, 1.599625672291267398 ) ) ;
#131963 = CARTESIAN_POINT ( 'NONE',  ( 1.224999999999995204, 1.125000000000000888, -2.949029909160572061E-14 ) ) ;
#131964 = CARTESIAN_POINT ( 'NONE',  ( 4.547283022377748729, -1.335744037758682667, -1.091317429222604884 ) ) ;
#131965 = CARTESIAN_POINT ( 'NONE',  ( -6.470265622219711688, 8.571729197388226140, -1.599625672291263179 ) ) ;
#131966 = CARTESIAN_POINT ( 'NONE',  ( 0.3340423123194468658, 0.5469568729883391711, -1.645723886551814452 ) ) ;
#131967 = SURFACE_STYLE_FILL_AREA ( #211023 ) ;
#131968 = CYLINDRICAL_SURFACE ( 'NONE', #77851, 1.224999999999996980 ) ;
#131969 = CARTESIAN_POINT ( 'NONE',  ( 11.07131242353766254, 11.29999999999999893, -0.8043462106219256835 ) ) ;
#131970 = AXIS2_PLACEMENT_3D ( 'NONE', #197681, #181434, #33063 ) ;
#131971 = CARTESIAN_POINT ( 'NONE',  ( 3.863710590214593399, 7.451486755318259547, 1.040834085586084257E-14 ) ) ;
#131972 = CARTESIAN_POINT ( 'NONE',  ( 4.241221290925122567, -0.2070989531138747453, -2.161143177887809852 ) ) ;
#131973 = CARTESIAN_POINT ( 'NONE',  ( 3.017977635683791071, -0.9002817137206723386, -1.588204215665294461 ) ) ;
#131974 = CARTESIAN_POINT ( 'NONE',  ( 0.8484012048698870156, -1.946262134508335739, -0.2457884297097159831 ) ) ;
#131975 = CARTESIAN_POINT ( 'NONE',  ( 5.594942764039734229, 1.868482245966827326, 0.9958698414167986845 ) ) ;
#131976 = AXIS2_PLACEMENT_3D ( 'NONE', #162797, #129313, #180103 ) ;
#131977 = EDGE_CURVE ( 'NONE', #175932, #210028, #201496, .T. ) ;
#131979 = CARTESIAN_POINT ( 'NONE',  ( 1.364683531249990311, 3.696875000341416584, 1.214306433183764966E-14 ) ) ;
#131978 = CARTESIAN_POINT ( 'NONE',  ( 6.356980026238091774, 0.3966049396831958229, -2.257653707126358267 ) ) ;
#131980 = CARTESIAN_POINT ( 'NONE',  ( 6.471393748265540147, 5.229711127717882491, 2.500000000000011102 ) ) ;
#131981 = CARTESIAN_POINT ( 'NONE',  ( 8.106885785967500979, 11.54545161934907682, 1.199719254218460707 ) ) ;
#131982 = CARTESIAN_POINT ( 'NONE',  ( 1.313308151137903224, 1.731519532738003297, -1.223779428986125462 ) ) ;
#131983 = CARTESIAN_POINT ( 'NONE',  ( -4.473827502829599290, 4.321812962830357208, 0.7216878364870317197 ) ) ;
#131984 = EDGE_CURVE ( 'NONE', #56213, #67059, #146422, .T. ) ;
#131985 = CARTESIAN_POINT ( 'NONE',  ( -2.449742653233043743, 3.949999999999981526, -0.4500000000000354272 ) ) ;
#131986 = CARTESIAN_POINT ( 'NONE',  ( -5.070386261386537363, 5.017798181146802428, 1.214306433183764966E-14 ) ) ;
#131987 = CARTESIAN_POINT ( 'NONE',  ( 6.473493066963706966, -0.2743099562094972743, 2.153646047958713172 ) ) ;
#131989 = CARTESIAN_POINT ( 'NONE',  ( -1.500000000000001110, 12.30208333401612641, 0.8660254037844419273 ) ) ;
#131988 = CARTESIAN_POINT ( 'NONE',  ( 6.883263157960358924, 7.052235917045241997, 2.651962373728885325 ) ) ;
#131991 = VERTEX_POINT ( 'NONE', #4916 ) ;
#131990 = CARTESIAN_POINT ( 'NONE',  ( 2.631719755377628811, -0.2151721393647449687, 2.210840341435269973 ) ) ;
#131992 = CARTESIAN_POINT ( 'NONE',  ( 6.082657761774013849, -0.6767167302549759178, 1.899617564980569995 ) ) ;
#131994 = CARTESIAN_POINT ( 'NONE',  ( 4.381722380181817478, -1.975297276180818296, 0.5937428812356324581 ) ) ;
#131993 = CARTESIAN_POINT ( 'NONE',  ( 4.521807925357579805, 5.234196320127330715, -1.199719254218452047 ) ) ;
#131996 = CARTESIAN_POINT ( 'NONE',  ( -0.2409995289980246258, 2.020898751655671788, -2.415740196953279462 ) ) ;
#131995 = CARTESIAN_POINT ( 'NONE',  ( 5.123001941117305336, 7.070197912760590064, 1.599625672291268286 ) ) ;
#131997 = CARTESIAN_POINT ( 'NONE',  ( 6.333594036239346359, 7.418223126147930557, 1.199719254218453823 ) ) ;
#131998 = CARTESIAN_POINT ( 'NONE',  ( 3.285556943749998737, -3.842708332855377051, -1.896917185911906500 ) ) ;
#131999 = CARTESIAN_POINT ( 'NONE',  ( 1.177073619093315759, 2.949321498342245995, 0.7750000000000100142 ) ) ;
#132000 = CARTESIAN_POINT ( 'NONE',  ( 4.440845869443198701, -1.426288408191313639, -1.164454570719307469 ) ) ;
#132001 = CARTESIAN_POINT ( 'NONE',  ( 4.656335691289526402, 7.519809842224722374, -1.199719254218452047 ) ) ;
#132002 = DIRECTION ( 'NONE',  ( 0.000000000000000000, 0.000000000000000000, 1.000000000000000000 ) ) ;
#132003 = CARTESIAN_POINT ( 'NONE',  ( 1.324769809204975557, -0.04781147349866912699, 1.724288685672677568 ) ) ;
#132004 = DIRECTION ( 'NONE',  ( 0.3321398189114310173, 0.9432301631592798774, 0.000000000000000000 ) ) ;
#132005 = CARTESIAN_POINT ( 'NONE',  ( 2.057686432631794293, -1.410295276735703540, 1.815187820423395992 ) ) ;
#132006 = CARTESIAN_POINT ( 'NONE',  ( -0.6823417656250212460, 4.363541667008085767, 1.181850606188767472 ) ) ;
#132007 = CARTESIAN_POINT ( 'NONE',  ( 0.7732102150014728004, -2.130643883221981838, -0.7610950190743612787 ) ) ;
#132008 = CARTESIAN_POINT ( 'NONE',  ( 3.791714260247856849, 1.525338472785308097, 1.452445685796518227 ) ) ;
#132009 = CARTESIAN_POINT ( 'NONE',  ( -7.756673280794142755, 8.222076047114187602, -0.7216878364870338292 ) ) ;
#132010 = CARTESIAN_POINT ( 'NONE',  ( 3.022431051408695613, 1.665045927894950095, 0.5999815234925524043 ) ) ;
#132011 = CARTESIAN_POINT ( 'NONE',  ( 6.154511665599609493, 9.267681812253174556, 1.199719254218462483 ) ) ;
#132012 = CARTESIAN_POINT ( 'NONE',  ( 4.543390873910903238, 7.354354215321133204, 1.082531754730548412 ) ) ;
#132013 = CARTESIAN_POINT ( 'NONE',  ( -4.415151579544611238, 8.302760609444034046, -0.7998128361456281477 ) ) ;
#132014 = B_SPLINE_CURVE_WITH_KNOTS ( 'NONE', 3,
 ( #111564, #191656, #25968, #178643, #175446, #93139, #76851, #94206, #110501, #28112 ),
 .UNSPECIFIED., .F., .F.,
 ( 4, 3, 3, 4 ),
 ( 5.442583568837955947E-16, 3.125183826620649906E-05, 6.400261867760048467E-05, 9.676915533390859927E-05 ),
 .UNSPECIFIED. ) ;
#132015 = CARTESIAN_POINT ( 'NONE',  ( 1.499999999999989120, 1.775000000000019673, 0.000000000000000000 ) ) ;
#132016 = CARTESIAN_POINT ( 'NONE',  ( -3.086452525405351643, 6.752611712948207057, 0.7998128361456341429 ) ) ;
#132017 = CARTESIAN_POINT ( 'NONE',  ( 4.939773707303276140, -2.109081064246129067, 0.6975513078685476875 ) ) ;
#132018 = CARTESIAN_POINT ( 'NONE',  ( 3.205210054081304438, -0.4271916898582402422, 2.149238826137919389 ) ) ;
#132019 = CARTESIAN_POINT ( 'NONE',  ( -4.249591082879585535, 7.045274465746411252, 1.199719254218464037 ) ) ;
#132020 = CARTESIAN_POINT ( 'NONE',  ( -11.88234649872613602, 9.843392170832489185, 0.9090484974825225883 ) ) ;
#132021 = DIRECTION ( 'NONE',  ( 0.000000000000000000, -1.301042606982654316E-17, -1.000000000000000000 ) ) ;
#132022 = CARTESIAN_POINT ( 'NONE',  ( 1.364683531249988535, 3.613541667008086211, 0.7879004041258500513 ) ) ;
#132023 = CARTESIAN_POINT ( 'NONE',  ( 6.890000000000007674, 6.036127733823692054, 2.594896729422516923 ) ) ;
#132024 = CARTESIAN_POINT ( 'NONE',  ( -4.121315508874269007, 5.831287398485176077, -1.443375672974053447 ) ) ;
#132025 = CARTESIAN_POINT ( 'NONE',  ( 6.187751663909415001, 2.028806014889028120, -0.6170373231123224000 ) ) ;
#132026 = CARTESIAN_POINT ( 'NONE',  ( -5.804299160426229953, 8.825413882922319431, -1.082531754730549967 ) ) ;
#132027 = ORIENTED_EDGE ( 'NONE', *, *, #157816, .F. ) ;
#132029 = DIRECTION ( 'NONE',  ( 0.000000000000000000, 1.000000000000000000, 0.000000000000000000 ) ) ;
#132028 = CARTESIAN_POINT ( 'NONE',  ( -5.478903473698260029, 6.525047153136981137, -1.082531754730549967 ) ) ;
#132030 = CARTESIAN_POINT ( 'NONE',  ( 5.840865249388943248, 5.708764300575555062, 0.7998128361456341429 ) ) ;
#132031 = CARTESIAN_POINT ( 'NONE',  ( 5.935073298327618652, -1.338256116417003927, -1.264887592264056559 ) ) ;
#132032 =( NAMED_UNIT ( * ) SI_UNIT ( $, .STERADIAN. ) SOLID_ANGLE_UNIT ( ) );
#132033 = CARTESIAN_POINT ( 'NONE',  ( -1.364683531250012516, 3.051041667008083547, -0.7879004041258289570 ) ) ;
#132034 = CARTESIAN_POINT ( 'NONE',  ( 1.592878374036447164, -0.5866614404700842833, 1.638733785964431755 ) ) ;
#132035 = CARTESIAN_POINT ( 'NONE',  ( 4.033714395265605823, 4.664753868353354704, -1.199719254218446718 ) ) ;
#132036 = CARTESIAN_POINT ( 'NONE',  ( 0.3265133270617843753, -1.284392789319420913, 1.483054880892265892 ) ) ;
#132037 = CARTESIAN_POINT ( 'NONE',  ( 0.6823417656249882723, -0.5947916663252492686, 1.181850606188755259 ) ) ;
#132038 = CARTESIAN_POINT ( 'NONE',  ( 4.750933126423753095, -1.738186171353903742, 1.284983810367075208 ) ) ;
#132039 = CARTESIAN_POINT ( 'NONE',  ( -2.449219305563052895, 6.009172956465517856, 1.040834085586084257E-14 ) ) ;
#132040 = PRESENTATION_LAYER_ASSIGNMENT (  '', '', ( #114901 ) ) ;
#132041 = CARTESIAN_POINT ( 'NONE',  ( -6.412643469139482910, 7.544134137826577380, 1.082531754730549967 ) ) ;
#132042 = CARTESIAN_POINT ( 'NONE',  ( 4.452137864729129646, 2.161286467946467837, -0.05003489268536746859 ) ) ;
#132044 = ORIENTED_EDGE ( 'NONE', *, *, #11497, .T. ) ;
#132043 = LINE ( 'NONE', #48631, #67220 ) ;
#132045 = CARTESIAN_POINT ( 'NONE',  ( 0.6823417656249899377, 3.426041667008085323, -1.181850606188754593 ) ) ;
#132046 = CARTESIAN_POINT ( 'NONE',  ( 5.536387714897482049, 1.941722972556509053, 0.3397322875919612795 ) ) ;
#132047 = CARTESIAN_POINT ( 'NONE',  ( 5.307816166741994302, -1.486200299559970128, 0.8926388968444918248 ) ) ;
#132049 = CARTESIAN_POINT ( 'NONE',  ( 2.033021410476544943, -1.955939774129427988, 0.9887309579383956049 ) ) ;
#132048 = CARTESIAN_POINT ( 'NONE',  ( -1.360316468750002894, -0.6302083329919370147, -0.7853790794158941324 ) ) ;
#132050 = CARTESIAN_POINT ( 'NONE',  ( 2.854834436329793057, 0.7764391075696615019, 2.173172238055173455 ) ) ;
#132051 = CARTESIAN_POINT ( 'NONE',  ( 4.235659074092642307, -1.418359850100110009, -1.495269491646352256 ) ) ;
#132052 = CARTESIAN_POINT ( 'NONE',  ( 0.4627034902389154936, 0.1913720229725413835, -1.932491135362510715 ) ) ;
#132053 = CARTESIAN_POINT ( 'NONE',  ( -5.694061327615147050, 9.586895948952255608, 0.000000000000000000 ) ) ;
#132054 = CARTESIAN_POINT ( 'NONE',  ( -4.305596300791617814, 7.180890229968955651, 1.199719254218452935 ) ) ;
#132055 = DIRECTION ( 'NONE',  ( 0.000000000000000000, -1.000000000000000000, 0.000000000000000000 ) ) ;
#132056 = EDGE_CURVE ( 'NONE', #101997, #114731, #122362, .T. ) ;
#132057 = CARTESIAN_POINT ( 'NONE',  ( 3.551138032611600437, 0.3147205237276836653, 2.097014573754731881 ) ) ;
#132058 = SURFACE_STYLE_FILL_AREA ( #183955 ) ;
#132059 = CARTESIAN_POINT ( 'NONE',  ( 1.670546294658280084, 1.392546765991018454, 1.458555661489918442 ) ) ;
#132060 = CARTESIAN_POINT ( 'NONE',  ( -7.348156068482412095, 7.675196289425353591, 1.040834085586084257E-14 ) ) ;
#132061 = CARTESIAN_POINT ( 'NONE',  ( 4.665167916288286420, -1.969490514480085164, -0.9956290437203789701 ) ) ;
#132062 = CARTESIAN_POINT ( 'NONE',  ( 0.000000000000000000, -0.9843749995220403282, -3.793834371823813001 ) ) ;
#132063 = CARTESIAN_POINT ( 'NONE',  ( 1.455271222711090884, 3.352338309680428896, 0.3949897977301484731 ) ) ;
#132064 = CARTESIAN_POINT ( 'NONE',  ( 2.854315967138055132, 6.433244981884085334, -0.2941531795266367211 ) ) ;
#132065 = CARTESIAN_POINT ( 'NONE',  ( 1.813555757143400893, 2.470689410283006371, -2.499999999999999556 ) ) ;
#132067 = CARTESIAN_POINT ( 'NONE',  ( -11.29517787156874853, -8.030538574678853792, 0.1971580631239607251 ) ) ;
#132066 = CARTESIAN_POINT ( 'NONE',  ( -5.830795741961422252, 7.309361553235873998, -1.292907557591252088 ) ) ;
#132068 = CARTESIAN_POINT ( 'NONE',  ( 11.01135777277262306, 12.69999999999999929, -1.400000000000001910 ) ) ;
#132069 = ORIENTED_EDGE ( 'NONE', *, *, #186635, .F. ) ;
#132070 = CARTESIAN_POINT ( 'NONE',  ( 4.504794318429003575, 1.594258339665870938, -1.305997064384886830 ) ) ;
#132071 = CARTESIAN_POINT ( 'NONE',  ( -3.755786496842897795E-14, 1.703125000341434214, 1.570758158831776052 ) ) ;
#132072 = CARTESIAN_POINT ( 'NONE',  ( -3.716906668440817185, 7.488141546489591072, 0.7998128361456341429 ) ) ;
#132073 = CARTESIAN_POINT ( 'NONE',  ( 3.123699121837515413, -0.3918110498563053268, 1.981120561552232262 ) ) ;
#132074 = CARTESIAN_POINT ( 'NONE',  ( -1.500000000000015099, -0.8708333333333129200, -0.8660254037844383745 ) ) ;
#132075 = CARTESIAN_POINT ( 'NONE',  ( 2.846322183865124700, 5.408127416896231665, -1.199719254218446718 ) ) ;
#132076 = CIRCLE ( 'NONE', #80238, 11.89429233241351902 ) ;
#132077 = CARTESIAN_POINT ( 'NONE',  ( 3.467699783257427004, 2.010999201309400686, -0.4499753609362132090 ) ) ;
#132078 = EDGE_CURVE ( 'NONE', #60775, #158934, #22241, .T. ) ;
#132079 = CARTESIAN_POINT ( 'NONE',  ( 3.968218245261731170, 4.000131783038177957, 0.6440902300205559872 ) ) ;
#132080 = CARTESIAN_POINT ( 'NONE',  ( 6.193377243344257543, 6.120028293523423812, -0.7998128361456281477 ) ) ;
#132081 = CARTESIAN_POINT ( 'NONE',  ( -0.1408020194050354501, 2.869306972054268989, -2.588546047063750688 ) ) ;
#132082 = CARTESIAN_POINT ( 'NONE',  ( 1.007454599746326895, -0.8259622865525710900, -1.645551850779983116 ) ) ;
#132083 = CARTESIAN_POINT ( 'NONE',  ( 6.358075476802443227, 2.201304964888863402, -0.1578768562689457922 ) ) ;
#132084 = CARTESIAN_POINT ( 'NONE',  ( 6.886615681098613884, 6.999082814228660077, 0.000000000000000000 ) ) ;
#132085 = CARTESIAN_POINT ( 'NONE',  ( 1.159701560084012595, 0.4228694819443152286, -2.119656415666733906 ) ) ;
#132086 = CARTESIAN_POINT ( 'NONE',  ( -2.643476764984671767, 6.027880625883323518, 1.040834085586084257E-14 ) ) ;
#132087 = CARTESIAN_POINT ( 'NONE',  ( 1.551970632248239612, 1.040795554343958429, 1.727062486439542965 ) ) ;
#132088 = VECTOR ( 'NONE', #53838, 1000.000000000000000 ) ;
#132089 = DIRECTION ( 'NONE',  ( 0.000000000000000000, 1.000000000000000000, 0.000000000000000000 ) ) ;
#132090 = CARTESIAN_POINT ( 'NONE',  ( 0.1978467685152424937, -1.870139902624564865, -0.05068021481659244765 ) ) ;
#132091 = CARTESIAN_POINT ( 'NONE',  ( -5.458264003855187951, 7.602368174425948588, -1.382272695577278387 ) ) ;
#132092 = CARTESIAN_POINT ( 'NONE',  ( 4.487161871577921346, 1.761403164857084702, -0.8856326919300193667 ) ) ;
#132093 = CARTESIAN_POINT ( 'NONE',  ( 4.926970384345759513, -1.727065721694167832, 1.040790168839386798 ) ) ;
#132094 = CARTESIAN_POINT ( 'NONE',  ( 1.364683531249986537, 2.655208333674754062, -0.7879004041258239610 ) ) ;
#132096 = CARTESIAN_POINT ( 'NONE',  ( 6.727182134110234024, -0.002100931800118072384, 2.089081857379895268 ) ) ;
#132095 = CARTESIAN_POINT ( 'NONE',  ( -6.204827856548512877, 10.39071626594860476, -0.7998128361456291469 ) ) ;
#132097 = EDGE_CURVE ( 'NONE', #182295, #157478, #98018, .T. ) ;
#132098 = CARTESIAN_POINT ( 'NONE',  ( 5.248515149483167441, -2.054309126314420642, -0.2569322651706855143 ) ) ;
#132099 = CARTESIAN_POINT ( 'NONE',  ( 5.947222937888848371, 10.09017719417900416, 1.040834085586084257E-14 ) ) ;
#132100 = CARTESIAN_POINT ( 'NONE',  ( -4.889686956022917919, 8.856385215335397021, 1.214306433183764966E-14 ) ) ;
#132101 = CARTESIAN_POINT ( 'NONE',  ( 1.859587702710796542, 3.245828361968115860, -0.4000000000000271672 ) ) ;
#132102 = CARTESIAN_POINT ( 'NONE',  ( 5.168225562285083896, 2.017301038980311656, -0.1031631561184200713 ) ) ;
#132103 = CARTESIAN_POINT ( 'NONE',  ( -1.500000000000015099, -1.297916665983847029, 0.8660254037844403729 ) ) ;
#132104 = CARTESIAN_POINT ( 'NONE',  ( 3.352467919438668620, 2.307868970251240714, 0.0003179301051748489328 ) ) ;
#132105 = ADVANCED_FACE ( 'NONE', ( #190100, #88351 ), #101390, .T. ) ;
#132106 = CARTESIAN_POINT ( 'NONE',  ( 1.288015978462764277, -1.305315335096700613, -1.597021576285734268 ) ) ;
#132107 = CARTESIAN_POINT ( 'NONE',  ( 7.619319141200057821, 10.87266085050000974, 1.082531754730557072 ) ) ;
#132108 = CARTESIAN_POINT ( 'NONE',  ( 6.261886844665240481, 8.398896966899865646, 1.599625672291268286 ) ) ;
#132109 = CARTESIAN_POINT ( 'NONE',  ( 6.900173834712277632, 7.014900660111269559, -0.7998128361456341429 ) ) ;
#132110 = CARTESIAN_POINT ( 'NONE',  ( 1.364683531249986537, 0.2177083336747502595, -0.7879004041258309554 ) ) ;
#132111 = CARTESIAN_POINT ( 'NONE',  ( 4.095444919779759552, 6.935713618788495793, 1.199719254218451159 ) ) ;
#132112 = CARTESIAN_POINT ( 'NONE',  ( 5.788968402910795064, 9.697620870130524651, 0.7216878364870438212 ) ) ;
#132113 = CARTESIAN_POINT ( 'NONE',  ( 4.158752335142390955, -0.6773029245935069387, -2.062915381819859562 ) ) ;
#132115 = CARTESIAN_POINT ( 'NONE',  ( 3.140019216317342376, 0.4501627324021878485, 1.785233193441162491 ) ) ;
#132114 = CARTESIAN_POINT ( 'NONE',  ( -4.446711195602252253, 6.210915699667823198, -1.443375672974053447 ) ) ;
#132116 = CARTESIAN_POINT ( 'NONE',  ( -1.364683531250010295, 4.780208333674755394, 0.7879004041258379498 ) ) ;
#132117 = CARTESIAN_POINT ( 'NONE',  ( 4.511385190476093321, -2.149204750630455241, 0.4279282578087198474 ) ) ;
#132118 = CARTESIAN_POINT ( 'NONE',  ( 6.827626583076773947, -7.154544010627095219, 6.720112740279239105 ) ) ;
#132119 = CARTESIAN_POINT ( 'NONE',  ( 5.295900185863533061, -0.8195587353489269811, 2.109036902066116603 ) ) ;
#132120 = CARTESIAN_POINT ( 'NONE',  ( -4.816275411463948330, 6.948951914485960835, -1.437501944199247372 ) ) ;
#132121 = CARTESIAN_POINT ( 'NONE',  ( 4.890561790263044273, 8.149264200713410844, -1.004099907704804950 ) ) ;
#132122 = CARTESIAN_POINT ( 'NONE',  ( -6.577113915960849155, 6.845923454808663600, -0.7216878364870338292 ) ) ;
#132123 = CARTESIAN_POINT ( 'NONE',  ( 5.424670859243587273, 5.501406555305196733, -0.7216878364870458196 ) ) ;
#132124 =( BOUNDED_SURFACE ( )  B_SPLINE_SURFACE ( 3, 2, ( 
 ( #114958, #195088, #46726 ),
 ( #112838, #213438, #32581 ),
 ( #80266, #96550, #162597 ),
 ( #64020, #98657, #130167 ),
 ( #164713, #196159, #16301 ),
 ( #170031, #85586, #168971 ),
 ( #87726, #21618, #2173 ),
 ( #20573, #84524, #102911 ) ),
 .UNSPECIFIED., .F., .F., .T. ) 
 B_SPLINE_SURFACE_WITH_KNOTS ( ( 4, 2, 2, 4 ),
 ( 3, 3 ),
 ( 0.000000000000000000, 0.0004912655988793406025, 0.0007368983983190109579, 0.0009825311977586812049 ),
 ( 0.000000000000000000, 1.000000000000000000 ),
 .UNSPECIFIED. ) 
 GEOMETRIC_REPRESENTATION_ITEM ( )  RATIONAL_B_SPLINE_SURFACE ( (
 ( 1.000000000000000000, 0.7100530722026821007, 1.000000000000000000),
 ( 1.000000000000000000, 0.6561915434216080145, 1.000000000000000000),
 ( 1.000000000000000000, 0.5915413786744014857, 1.000000000000000000),
 ( 1.000000000000000000, 0.4908282809847615002, 1.000000000000000000),
 ( 1.000000000000000000, 0.4560392263211024977, 1.000000000000000000),
 ( 1.000000000000000000, 0.3997350557757124445, 1.000000000000000000),
 ( 1.000000000000000000, 0.3799210206804777279, 1.000000000000000000),
 ( 1.000000000000000000, 0.3826834323650904479, 1.000000000000000000) ) ) 
 REPRESENTATION_ITEM ( '' )  SURFACE ( )  );
#132125 = CARTESIAN_POINT ( 'NONE',  ( 6.397684210179588327, -0.5939413028648796722, 1.667199339893215448 ) ) ;
#132126 = AXIS2_PLACEMENT_3D ( 'NONE', #36861, #2205, #102945 ) ;
#132127 = CARTESIAN_POINT ( 'NONE',  ( 4.143230477514478594, 0.1011454402246019235, 2.010680395766785811 ) ) ;
#132128 = CARTESIAN_POINT ( 'NONE',  ( 5.621827251160867789, 9.710548892996357040, 1.040834085586084257E-14 ) ) ;
#132129 = CARTESIAN_POINT ( 'NONE',  ( 2.854625263381281641, 0.7083305855763160075, 1.983406512126543841 ) ) ;
#132130 = CARTESIAN_POINT ( 'NONE',  ( 2.583477129321013255, -0.5985834622587657972, 1.819768813671450935 ) ) ;
#132131 = STYLED_ITEM ( 'NONE', ( #125846 ), #48566 ) ;
#132132 = CARTESIAN_POINT ( 'NONE',  ( 2.998324526916512411, 6.649795714711241423, 0.000000000000000000 ) ) ;
#132133 = CARTESIAN_POINT ( 'NONE',  ( 3.051173608728700248, 1.690664904776484789, -1.010063219348409813 ) ) ;
#132134 = CARTESIAN_POINT ( 'NONE',  ( 1.041631754505952134, 0.7616270086890539748, -1.708776438048253077 ) ) ;
#132135 = CARTESIAN_POINT ( 'NONE',  ( 1.258172656280614365, -1.962046632281065461, -0.003472340283867945618 ) ) ;
#132137 = ORIENTED_EDGE ( 'NONE', *, *, #99758, .T. ) ;
#132136 = CARTESIAN_POINT ( 'NONE',  ( 0.2988868148526523938, -0.2362956723594503705, -1.897694653714178781 ) ) ;
#132138 = CARTESIAN_POINT ( 'NONE',  ( 6.317736394288147039, 6.473040002865377396, 0.7216878364870317197 ) ) ;
#132139 = CARTESIAN_POINT ( 'NONE',  ( 1.364683531249986537, 1.176041667008082658, 0.7879004041258500513 ) ) ;
#132140 = CARTESIAN_POINT ( 'NONE',  ( 6.438356904408193415, 1.850619875698428674, 0.2722718653145329015 ) ) ;
#132141 = CARTESIAN_POINT ( 'NONE',  ( 10.70146331988817323, 11.37946204949139251, 0.7998128361456341429 ) ) ;
#132142 = DIRECTION ( 'NONE',  ( -0.000000000000000000, -0.000000000000000000, -1.000000000000000000 ) ) ;
#132143 = EDGE_LOOP ( 'NONE', ( #111842, #159306, #19165, #90202 ) ) ;
#132144 = CARTESIAN_POINT ( 'NONE',  ( 6.209843387784003355, 0.6066176463192971546, -1.979359621541395553 ) ) ;
#132145 = CARTESIAN_POINT ( 'NONE',  ( 0.000000000000000000, 1.000000000000002665, 6.329999999999995630 ) ) ;
#132146 = CARTESIAN_POINT ( 'NONE',  ( 1.398975865466948632, 0.4019745351953528112, 2.030794141931663521 ) ) ;
#132147 = CARTESIAN_POINT ( 'NONE',  ( -1.201851678989727383E-14, 2.212500000000021672, 1.732050807568877637 ) ) ;
#132148 = CARTESIAN_POINT ( 'NONE',  ( 6.287230548435207567, 8.358188277972981695, -1.599625672291262513 ) ) ;
#132149 = CARTESIAN_POINT ( 'NONE',  ( -8.799405390469187793, 10.22472669609091689, -1.199719254218446718 ) ) ;
#132150 = CARTESIAN_POINT ( 'NONE',  ( 5.123001941117305336, 7.070197912760590064, 1.599625672291268286 ) ) ;
#132151 = CARTESIAN_POINT ( 'NONE',  ( 5.602226918196428151, -0.9533447246646039597, 1.894147766696724799 ) ) ;
#132152 = CARTESIAN_POINT ( 'NONE',  ( 5.598591087800349086, 5.496387455380669529, -0.7998128361456481317 ) ) ;
#132153 = CARTESIAN_POINT ( 'NONE',  ( 0.6823417656249882723, 1.176041667008083325, -1.181850606188749264 ) ) ;
#132154 = VERTEX_POINT ( 'NONE', #8152 ) ;
#132155 = CARTESIAN_POINT ( 'NONE',  ( -1.201851678989727383E-14, 2.837500000000024780, -1.732050807568863648 ) ) ;
#132157 = CARTESIAN_POINT ( 'NONE',  ( 3.822509244049070887, 6.547012320444182798, -1.199719254218452047 ) ) ;
#132156 = CARTESIAN_POINT ( 'NONE',  ( 6.338335788673861160, -1.050647824335379399, 1.656640365463659670 ) ) ;
#132158 = CARTESIAN_POINT ( 'NONE',  ( 2.882185300971401798, -0.2004049647258976941, 2.006138917898095730 ) ) ;
#132159 = CARTESIAN_POINT ( 'NONE',  ( 3.133901338358492161, 1.915903397621956383, -0.005105665024216290114 ) ) ;
#132160 = CARTESIAN_POINT ( 'NONE',  ( -1.902112725515572755, 3.289212146679091120, -0.4096023912812309375 ) ) ;
#132161 = CARTESIAN_POINT ( 'NONE',  ( 1.769323484426460480, 2.095969018468134770, -0.6401429536977767398 ) ) ;
#132162 = CARTESIAN_POINT ( 'NONE',  ( 0.2331713839410966271, 5.723577825403736163, -2.547423061495857954 ) ) ;
#132163 = CARTESIAN_POINT ( 'NONE',  ( 3.198369223161025676, -0.5396142385952484855, -1.791042426047453784 ) ) ;
#132164 = CARTESIAN_POINT ( 'NONE',  ( 1.499999999999987566, -0.9437499993171851731, 0.000000000000000000 ) ) ;
#132165 = CARTESIAN_POINT ( 'NONE',  ( -6.008234629150358330, 10.16135750065076060, 0.000000000000000000 ) ) ;
#132167 = CARTESIAN_POINT ( 'NONE',  ( 5.835599761872579450, 0.6139674163637841575, -2.026275392342128612 ) ) ;
#132166 = CARTESIAN_POINT ( 'NONE',  ( -5.273758566035884776, 5.255065869904374409, 0.000000000000000000 ) ) ;
#132168 = DIRECTION ( 'NONE',  ( 3.706092522800016599E-15, 0.000000000000000000, 1.000000000000000000 ) ) ;
#132169 = CARTESIAN_POINT ( 'NONE',  ( 6.689897370947560873, -1.349224794794257720, -1.570457413003906177 ) ) ;
#132171 = CARTESIAN_POINT ( 'NONE',  ( 1.734723475976807094E-15, 0.2401923788623722134, 11.09999999999960885 ) ) ;
#132170 = CARTESIAN_POINT ( 'NONE',  ( 1.769195444908505888, 1.999712852614519143, -0.6101556835421716452 ) ) ;
#132173 = VERTEX_POINT ( 'NONE', #40678 ) ;
#132172 = CARTESIAN_POINT ( 'NONE',  ( 0.6742806677700216023, -1.621663110835226629, -0.5878086553270861492 ) ) ;
#132174 = CARTESIAN_POINT ( 'NONE',  ( 6.368579470117202490, 8.453095353268645695, 1.599625672291281386 ) ) ;
#132176 = AXIS2_PLACEMENT_3D ( 'NONE', #51951, #36742, #187265 ) ;
#132175 = FACE_OUTER_BOUND ( 'NONE', #167289, .T. ) ;
#132177 = CARTESIAN_POINT ( 'NONE',  ( 0.000000000000000000, 2.817530495244580102, 1.214306433183764966E-14 ) ) ;
#132178 = CARTESIAN_POINT ( 'NONE',  ( 7.876924059415351564, 12.13356913605253240, -0.7216878364870267237 ) ) ;
#132179 = DIRECTION ( 'NONE',  ( 0.000000000000000000, 1.000000000000000000, 0.000000000000000000 ) ) ;
#132181 = CARTESIAN_POINT ( 'NONE',  ( 1.418313031307829153, -0.6519236697288594007, -1.690267533947023892 ) ) ;
#132180 = CARTESIAN_POINT ( 'NONE',  ( 5.071631979963703962, 8.074598522336444262, 1.199719254218451159 ) ) ;
#132182 = CARTESIAN_POINT ( 'NONE',  ( -6.021792782764022078, 10.17717534653336209, -0.7998128361456291469 ) ) ;
#132183 = CARTESIAN_POINT ( 'NONE',  ( 3.005103603723342953, 6.657704637652544832, -0.7998128361456291469 ) ) ;
#132184 = CARTESIAN_POINT ( 'NONE',  ( -6.108552962726611746, 7.019250575032890183, 0.9758408306729206005 ) ) ;
#132185 = CARTESIAN_POINT ( 'NONE',  ( 6.496291879603339758, 7.608037276739255006, 1.199719254218452935 ) ) ;
#132186 = CARTESIAN_POINT ( 'NONE',  ( 6.539320575229256249, 6.039323383297771741, 2.391644441267444687 ) ) ;
#132187 = CARTESIAN_POINT ( 'NONE',  ( 9.327646496521982300, 11.90534021740758064, -1.443375672974057666 ) ) ;
#132188 = ORIENTED_EDGE ( 'NONE', *, *, #168648, .F. ) ;
#132189 = CARTESIAN_POINT ( 'NONE',  ( 2.769781630715903997, -1.841240947949342788, 0.2698520108674675733 ) ) ;
#132190 = CARTESIAN_POINT ( 'NONE',  ( 0.7553224350208649351, 1.845776580612036533, -0.5121453728616427448 ) ) ;
#132191 = CARTESIAN_POINT ( 'NONE',  ( 6.774445256934315651, -1.184694399318196201, 1.519801669933226407 ) ) ;
#132192 = CARTESIAN_POINT ( 'NONE',  ( -1.872868072690844432, 8.979822391611987698, 0.7750000000000013545 ) ) ;
#132193 = VECTOR ( 'NONE', #130002, 1000.000000000000000 ) ;
#132194 = CARTESIAN_POINT ( 'NONE',  ( 4.594747986498664005, 8.374059380672374431, -0.03693212167796278145 ) ) ;
#132195 = CARTESIAN_POINT ( 'NONE',  ( 0.000000000000000000, 0.9200000000000041478, 0.000000000000000000 ) ) ;
#132196 = CARTESIAN_POINT ( 'NONE',  ( -3.416291520963659512, 5.969128626890772615, 1.082531754730560403 ) ) ;
#132197 = CARTESIAN_POINT ( 'NONE',  ( 7.768458830950378591, 12.00702636951006497, 1.040834085586084257E-14 ) ) ;
#132198 = CARTESIAN_POINT ( 'NONE',  ( 4.645333151331359822, 1.761124666023382579, -0.8816396696852289994 ) ) ;
#132199 = CARTESIAN_POINT ( 'NONE',  ( 1.963691422110905638, -1.704870618661393999, -1.260721693921822428 ) ) ;
#132200 = CARTESIAN_POINT ( 'NONE',  ( -6.891622154448065807, 6.934647356477856128, 1.040834085586084257E-14 ) ) ;
#132201 = CARTESIAN_POINT ( 'NONE',  ( -11.86145016429273014, 10.19999999999999929, -1.100000000000000533 ) ) ;
#132202 = CARTESIAN_POINT ( 'NONE',  ( 5.718738293430368991, -0.05686238728638653983, 2.190873718245327506 ) ) ;
#132203 = CARTESIAN_POINT ( 'NONE',  ( -1.500000000000015099, 10.01041666734946745, -0.8660254037844309360 ) ) ;
#132204 = CARTESIAN_POINT ( 'NONE',  ( 4.594702886556338406, -0.4214696541114425488, -1.879573207023744974 ) ) ;
#132205 = CARTESIAN_POINT ( 'NONE',  ( -7.867809214632013770, 8.073532260025807261, 1.040834085586084257E-14 ) ) ;
#132206 = CARTESIAN_POINT ( 'NONE',  ( 0.3053143536290472970, -0.4923201697357786899, 1.757875871163571802 ) ) ;
#132207 = CARTESIAN_POINT ( 'NONE',  ( 1.278255639411193245, 1.316999024263129092, 1.770685722221450709 ) ) ;
#132208 = VERTEX_POINT ( 'NONE', #120924 ) ;
#132209 = DIRECTION ( 'NONE',  ( -0.000000000000000000, 1.000000000000000000, -0.000000000000000000 ) ) ;
#132210 = EDGE_LOOP ( 'NONE', ( #143260, #131242, #92187, #160284 ) ) ;
#132211 = CARTESIAN_POINT ( 'NONE',  ( 6.578958714233388072, 1.836342173298356917, 0.7121609383471518839 ) ) ;
#132212 = CARTESIAN_POINT ( 'NONE',  ( 1.944774020950320592, -1.561091384877069554, -1.155077030050962295 ) ) ;
#132213 = CARTESIAN_POINT ( 'NONE',  ( 6.538407551539116902, 2.202477839928073333, -0.6571292610791487077 ) ) ;
#132215 = CARTESIAN_POINT ( 'NONE',  ( 4.012436097835626825, 0.6663421089948203813, 1.737758261286206807 ) ) ;
#132214 = CARTESIAN_POINT ( 'NONE',  ( -5.433785704026946384, 9.561443431331920095, 0.000000000000000000 ) ) ;
#132216 = CARTESIAN_POINT ( 'NONE',  ( 4.389807875774629942, 8.343469298370917997, 0.7998128361456271485 ) ) ;
#132217 = CARTESIAN_POINT ( 'NONE',  ( -6.966220764712148572, 6.002124920821316323, 2.500000000000000444 ) ) ;
#132218 = CARTESIAN_POINT ( 'NONE',  ( -4.557512192488103686, 8.468847991211438497, -0.7998128361456281477 ) ) ;
#132219 = CARTESIAN_POINT ( 'NONE',  ( -4.855228407469635243, 4.837057028235559386, 0.7216878364870257245 ) ) ;
#132220 = CARTESIAN_POINT ( 'NONE',  ( -0.005964567173097347699, -2.191213315851054944, -0.04726126812268362232 ) ) ;
#132221 = CARTESIAN_POINT ( 'NONE',  ( 5.341549334104194635, 6.294524313618772737, 1.082531754730558626 ) ) ;
#132223 = EDGE_CURVE ( 'NONE', #87474, #57507, #104606, .T. ) ;
#132222 = TOROIDAL_SURFACE ( 'NONE', #204826, 9.580000000000001847, 0.08000000000000000167 ) ;
#132224 = CARTESIAN_POINT ( 'NONE',  ( 10.99180900346484968, -6.701306620465910413, -0.4265819271707739779 ) ) ;
#132225 = CARTESIAN_POINT ( 'NONE',  ( 3.719872605471085336, 6.605953636083950364, 2.420000000000000373 ) ) ;
#132226 = CARTESIAN_POINT ( 'NONE',  ( 1.611646134362737959, -1.812087876328593916, 0.2219229778191167957 ) ) ;
#132227 = CARTESIAN_POINT ( 'NONE',  ( -5.298539104842322267, 5.076050465271134016, 0.7998128361456341429 ) ) ;
#132228 = CARTESIAN_POINT ( 'NONE',  ( 3.533592999799278989, -1.415137147236225079, 1.001973916141611687 ) ) ;
#132229 = CARTESIAN_POINT ( 'NONE',  ( -11.97929049433705373, 13.88000000000000078, 0.7046979865771783036 ) ) ;
#132230 = CARTESIAN_POINT ( 'NONE',  ( 6.508999999999979025, 4.693190036150777011, 2.662629399390674667 ) ) ;
#132231 = CARTESIAN_POINT ( 'NONE',  ( 4.559605246071182449, 3.300000000000025135, -0.7749999999999944711 ) ) ;
#132232 = CARTESIAN_POINT ( 'NONE',  ( 0.2582596107527914131, 0.7359740259155130859, 1.780569212123730871 ) ) ;
#132233 = CARTESIAN_POINT ( 'NONE',  ( 4.627759936859944467, 1.903863570041373077, -0.4726564843360381851 ) ) ;
#132234 = EDGE_CURVE ( 'NONE', #139750, #76889, #73135, .T. ) ;
#132235 = CARTESIAN_POINT ( 'NONE',  ( -8.636707547105197946, 10.03491254549959777, -1.199719254218446718 ) ) ;
#132236 = CARTESIAN_POINT ( 'NONE',  ( 6.796715079152391148, 6.823922435299587974, 0.7998128361456341429 ) ) ;
#132237 = CARTESIAN_POINT ( 'NONE',  ( 4.494861206476631565, -2.057060146276223023, -0.5143016718046622415 ) ) ;
#132238 = CARTESIAN_POINT ( 'NONE',  ( -7.160677686311960777, 11.50587440067263678, -0.7998128361456291469 ) ) ;
#132239 = CARTESIAN_POINT ( 'NONE',  ( 5.983225862332436584, 5.874851682342960402, 0.7998128361456341429 ) ) ;
#132240 = CARTESIAN_POINT ( 'NONE',  ( 2.483334644719075168, -0.004358110040847408898, 2.070434559716929357 ) ) ;
#132242 = CARTESIAN_POINT ( 'NONE',  ( -1.364683531250014514, -0.4072916663252447167, 0.7879004041258379498 ) ) ;
#132241 = CARTESIAN_POINT ( 'NONE',  ( 0.000000000000000000, 8.999999999999998224, 0.000000000000000000 ) ) ;
#132243 = ORIENTED_EDGE ( 'NONE', *, *, #120497, .T. ) ;
#132244 = CARTESIAN_POINT ( 'NONE',  ( 2.637635294750583004, 0.7773225462509441019, 2.163377341885423188 ) ) ;
#132245 = CARTESIAN_POINT ( 'NONE',  ( 9.408995418203975447, 10.07950886410055524, 0.7216878364870438212 ) ) ;
#132247 = CARTESIAN_POINT ( 'NONE',  ( -3.285556943750000070, -2.559374999522041172, 0.000000000000000000 ) ) ;
#132246 = CARTESIAN_POINT ( 'NONE',  ( 5.343321937561575474, 8.287607122913563273, -1.082531754730548412 ) ) ;
#132248 = SURFACE_SIDE_STYLE ('',( #36827 ) ) ;
#132249 = SURFACE_STYLE_USAGE ( .BOTH. , #54162 ) ;
#132250 = ORIENTED_EDGE ( 'NONE', *, *, #189331, .T. ) ;
#132251 = CARTESIAN_POINT ( 'NONE',  ( 10.66990370383054731, 11.55056853066490952, 0.7216878364870317197 ) ) ;
#132252 = CARTESIAN_POINT ( 'NONE',  ( 4.095896644567202038, 1.253117935160457552, 1.444681106026260320 ) ) ;
#132253 = DIRECTION ( 'NONE',  ( 1.000000000000000000, -1.250471828332824404E-35, -1.561251128379126077E-17 ) ) ;
#132254 = CARTESIAN_POINT ( 'NONE',  ( 4.893404818765360709, 1.279633041931761639, 1.156618277182480892 ) ) ;
#132255 = CARTESIAN_POINT ( 'NONE',  ( 3.696500153570709379, 1.422608671726926177, -1.429447704489300364 ) ) ;
#132256 = CARTESIAN_POINT ( 'NONE',  ( 5.116020035227313301, 0.1674390183682184785, 2.292669612833755810 ) ) ;
#132257 = CARTESIAN_POINT ( 'NONE',  ( 0.3282377607281153908, 1.238835450998194920, -1.225000000000006972 ) ) ;
#132258 = CARTESIAN_POINT ( 'NONE',  ( 0.8564375766340023288, 2.204168734417511821, -0.1118928034387969561 ) ) ;
#132259 = CARTESIAN_POINT ( 'NONE',  ( -5.478903473698268023, 5.564677938835638216, -0.7216878364870338292 ) ) ;
#132260 = CARTESIAN_POINT ( 'NONE',  ( 5.413276439055476175, -0.2588944790761596448, 1.750576072867173316 ) ) ;
#132262 = CARTESIAN_POINT ( 'NONE',  ( 1.869451396563295065, 2.192715141705191773, -0.6681815460085840375 ) ) ;
#132261 = CARTESIAN_POINT ( 'NONE',  ( 6.723917837734620484, 6.809268663637336516, 0.000000000000000000 ) ) ;
#132263 = CARTESIAN_POINT ( 'NONE',  ( 6.210883717528068892, -0.2205035313364057392, 1.827825250963102111 ) ) ;
#132264 = DIRECTION ( 'NONE',  ( -1.000000000000000000, 0.000000000000000000, 2.168404344971007685E-15 ) ) ;
#132265 = DIRECTION ( 'NONE',  ( -0.4999999999999999445, 0.000000000000000000, 0.8660254037844387076 ) ) ;
#132266 = CARTESIAN_POINT ( 'NONE',  ( -7.533490631048818109, 8.818102486758951031, -1.199719254218452047 ) ) ;
#132267 = CARTESIAN_POINT ( 'NONE',  ( -0.6801582343750091075, -1.036458332991943454, 1.178068619123817218 ) ) ;
#132268 = CARTESIAN_POINT ( 'NONE',  ( -11.94105722165071093, 13.52582762082958823, -1.187919369849417484 ) ) ;
#132269 = CARTESIAN_POINT ( 'NONE',  ( 6.549288556030710140, 1.803345607721940524, -1.016871928424132099 ) ) ;
#132270 = CARTESIAN_POINT ( 'NONE',  ( 2.518767860054324625, 0.2516336668320385828, 2.000731427934741902 ) ) ;
#132271 = VECTOR ( 'NONE', #185864, 1000.000000000000000 ) ;
#132272 = CARTESIAN_POINT ( 'NONE',  ( -1.402160292154681736E-14, -0.006249999317184824418, 1.732050807568877637 ) ) ;
#132273 = CARTESIAN_POINT ( 'NONE',  ( 5.426370213035293766, 1.145732239094964466, -1.548636736622555299 ) ) ;
#132274 = CARTESIAN_POINT ( 'NONE',  ( 0.6823417656249969321, 12.02604166700806054, -1.181850606188757036 ) ) ;
#132275 = CARTESIAN_POINT ( 'NONE',  ( 2.496574912728947382, -1.137965521849234607, 1.907653428263719864 ) ) ;
#132276 = EDGE_LOOP ( 'NONE', ( #199, #178059, #85880, #134118 ) ) ;
#132278 = AXIS2_PLACEMENT_3D ( 'NONE', #117260, #171276, #3421 ) ;
#132277 = CARTESIAN_POINT ( 'NONE',  ( 0.2802162696002897246, 8.153957901067531822, -2.020850277443529741 ) ) ;
#132279 = DIRECTION ( 'NONE',  ( -1.000000000000000000, 0.000000000000000000, 0.000000000000000000 ) ) ;
#132280 = CARTESIAN_POINT ( 'NONE',  ( 8.920375002787457319, 12.49452237230570084, 1.199719254218450271 ) ) ;
#132281 = DIRECTION ( 'NONE',  ( -5.578564026256490882E-16, -1.000000000000000000, -9.066213480720158442E-32 ) ) ;
#132282 = CARTESIAN_POINT ( 'NONE',  ( 10.91132967064556070, -5.166862915010145052, -0.4350687514514655629 ) ) ;
#132283 = CARTESIAN_POINT ( 'NONE',  ( 5.425286103790146974, -1.110369212591550747, -1.340227399214832360 ) ) ;
#132284 = CARTESIAN_POINT ( 'NONE',  ( 3.016010921186715432, 1.952665002612500533, -0.1895750030070641190 ) ) ;
#132286 = CARTESIAN_POINT ( 'NONE',  ( -6.724481002698120768, 9.828683022247721723, -1.082531754730538864 ) ) ;
#132285 = CARTESIAN_POINT ( 'NONE',  ( 5.007038802148489509, 4.735966778795008381, 0.7998128361456341429 ) ) ;
#132287 = SURFACE_STYLE_USAGE ( .BOTH. , #185244 ) ;
#132288 = CARTESIAN_POINT ( 'NONE',  ( 4.921284695982240720, -0.1178685990214298068, 2.259476483347002240 ) ) ;
#132289 = CARTESIAN_POINT ( 'NONE',  ( 0.8364713509731898089, -1.147405136530167624, 1.713900253247694350 ) ) ;
#132290 = CARTESIAN_POINT ( 'NONE',  ( -6.333630315878337136, 10.54098580183340772, 0.000000000000000000 ) ) ;
#132291 = CARTESIAN_POINT ( 'NONE',  ( -4.595850884908229794, 4.464173575255435011, 0.7216878364870317197 ) ) ;
#132292 = CARTESIAN_POINT ( 'NONE',  ( 1.850798253084064537, 0.7104643512030085484, 2.148151574381700790 ) ) ;
#132293 = ORIENTED_EDGE ( 'NONE', *, *, #6240, .F. ) ;
#132294 = CARTESIAN_POINT ( 'NONE',  ( -1.402160292154681736E-14, -0.3812499993171785673, -1.732050807568870754 ) ) ;
#132295 = CARTESIAN_POINT ( 'NONE',  ( 2.618241971997347317, 1.224968108320439342, -1.413705424714882586 ) ) ;
#132296 = CARTESIAN_POINT ( 'NONE',  ( 1.652526702274889514, 0.8913305402388423948, 1.487382274443969754 ) ) ;
#132297 = CARTESIAN_POINT ( 'NONE',  ( 5.583573808894983337, -0.9862700065477579825, 1.957137920222583372 ) ) ;
#132298 = CARTESIAN_POINT ( 'NONE',  ( 6.370204010553460527, 1.178711257604664109, 1.983722394024198143 ) ) ;
#132299 = CARTESIAN_POINT ( 'NONE',  ( 1.252885565054340011, -1.625093837591420787, 1.267311679704327121 ) ) ;
#132300 = CARTESIAN_POINT ( 'NONE',  ( 4.540924088961058480, -1.502189473471927439, -1.230693300551897185 ) ) ;
#132301 = CARTESIAN_POINT ( 'NONE',  ( -4.568734577680894304, 5.392907097791561633, -1.082531754730543971 ) ) ;
#132302 = CARTESIAN_POINT ( 'NONE',  ( 5.483624757375023862, 1.255567903217995829, 1.386730702750748945 ) ) ;
#132303 = CARTESIAN_POINT ( 'NONE',  ( 1.625000000000001554, -2.052068128417951165, 9.007296548519099900E-14 ) ) ;
#132304 = LINE ( 'NONE', #164769, #123316 ) ;
#132305 = CARTESIAN_POINT ( 'NONE',  ( 6.327499943094792023, -1.427716970705223520, 1.423745300580002482 ) ) ;
#132306 = EDGE_CURVE ( 'NONE', #99531, #18446, #55841, .T. ) ;
#132307 = CARTESIAN_POINT ( 'NONE',  ( 4.312902262922978736, 5.164712407232485702, -1.082531754730548412 ) ) ;
#132308 = CARTESIAN_POINT ( 'NONE',  ( -1.360316468750030650, 0.8697916670080860779, -0.7853790794159041244 ) ) ;
#132309 = CARTESIAN_POINT ( 'NONE',  ( 4.342422763466713853, 0.4390309838058319425, -1.967887491402267486 ) ) ;
#132310 = CARTESIAN_POINT ( 'NONE',  ( -2.290964770585000920, 5.616616632417037458, -0.7216878364870257245 ) ) ;
#132311 =( BOUNDED_CURVE ( )  B_SPLINE_CURVE ( 2, ( #29380, #92278, #161523 ),
 .UNSPECIFIED., .F., .T. ) 
 B_SPLINE_CURVE_WITH_KNOTS ( ( 3, 3 ),
 ( 0.000000000000000000, 0.002781257751169560668 ),
 .UNSPECIFIED. ) 
 CURVE ( )  GEOMETRIC_REPRESENTATION_ITEM ( )  RATIONAL_B_SPLINE_CURVE ( ( 1.000000000000000000, 0.9105717077957579120, 0.9405305184076300229 ) ) 
 REPRESENTATION_ITEM ( '' )  );
#132312 = CARTESIAN_POINT ( 'NONE',  ( 6.611572464958476836, 10.86525164242692298, 0.7998128361456462443 ) ) ;
#132313 = APPLICATION_CONTEXT ( 'automotive_design' ) ;
#132314 = CARTESIAN_POINT ( 'NONE',  ( 3.555981428534177091, 7.370671776590375757, 0.7998128361456271485 ) ) ;
#132316 = CARTESIAN_POINT ( 'NONE',  ( 6.670655732516626912, 7.629137130509076492, 2.426260288887295502 ) ) ;
#132315 = CARTESIAN_POINT ( 'NONE',  ( 2.121465551170404140, -1.771062468586531047, 0.4427346646293239818 ) ) ;
#132317 = CARTESIAN_POINT ( 'NONE',  ( 6.922231005658577629, -8.202869699938531767, -6.506745451169505756 ) ) ;
#132318 = ORIENTED_EDGE ( 'NONE', *, *, #32535, .F. ) ;
#132319 = CARTESIAN_POINT ( 'NONE',  ( -6.916067756302494374, 7.241369601873926420, 0.000000000000000000 ) ) ;
#132320 = CARTESIAN_POINT ( 'NONE',  ( 11.84668730067608600, 10.19999999999998153, 1.399999999999998579 ) ) ;
#132321 = CARTESIAN_POINT ( 'NONE',  ( -9.484092147959342967, 11.02352791316275216, 1.199719254218462483 ) ) ;
#132322 = CARTESIAN_POINT ( 'NONE',  ( -0.1930879795662324705, -0.4444491470046680326, -1.977061965688177825 ) ) ;
#132323 = CARTESIAN_POINT ( 'NONE',  ( 0.04773460823432121303, -1.936894771697717621, 0.8635138731061947626 ) ) ;
#132324 = ORIENTED_EDGE ( 'NONE', *, *, #102521, .T. ) ;
#132325 = CARTESIAN_POINT ( 'NONE',  ( -5.101610940492132151, 9.173906207207963348, -0.7998128361456362523 ) ) ;
#132326 = COLOUR_RGB ( '', 0.72549020, 0.75294118, 0.79215686) ;
#132327 = CARTESIAN_POINT ( 'NONE',  ( 6.342516933094585418, 6.294024598232139667, 1.040834085586084257E-14 ) ) ;
#132328 = CARTESIAN_POINT ( 'NONE',  ( 6.034070662188514511, 1.017841854155163706, -1.791927558475673754 ) ) ;
#132329 = CARTESIAN_POINT ( 'NONE',  ( 5.291638762709002464, 1.525045427759319727, -1.319226660814104335 ) ) ;
#132330 = ORIENTED_EDGE ( 'NONE', *, *, #128510, .F. ) ;
#132331 = EDGE_LOOP ( 'NONE', ( #104070, #184082, #37687, #56079 ) ) ;
#132332 = PLANE ( 'NONE',  #136264 ) ;
#132333 = CARTESIAN_POINT ( 'NONE',  ( 8.167861197590044142, 8.493869250135347215, 0.000000000000000000 ) ) ;
#132336 = VERTEX_POINT ( 'NONE', #170653 ) ;
#132335 = CARTESIAN_POINT ( 'NONE',  ( 0.2331563151865738703, 7.629137130509052511, -2.545728013813946866 ) ) ;
#132334 = CARTESIAN_POINT ( 'NONE',  ( -6.479871072688648148, 6.524547437750345402, 0.000000000000000000 ) ) ;
#132337 = CARTESIAN_POINT ( 'NONE',  ( 5.371503168974233411, 7.687194297833679357, 1.321221623412481394 ) ) ;
#132338 = CARTESIAN_POINT ( 'NONE',  ( 5.606796008369615336, 0.8196459417171353401, -1.842166028910074527 ) ) ;
#132339 = CARTESIAN_POINT ( 'NONE',  ( 4.277188459880359339, 1.204364621523913437, 1.392669941884729035 ) ) ;
#132340 = FACE_OUTER_BOUND ( 'NONE', #106192, .T. ) ;
#132341 = CARTESIAN_POINT ( 'NONE',  ( 3.370030522709596355, 2.251568201494443588, -0.5052104078027676026 ) ) ;
#132342 = CARTESIAN_POINT ( 'NONE',  ( 6.373214726875630731, 9.593111727067046957, 1.199719254218452047 ) ) ;
#132343 = CARTESIAN_POINT ( 'NONE',  ( 4.341216920475977403, -1.883070171734081200, 1.061215411333437109 ) ) ;
#132345 = CARTESIAN_POINT ( 'NONE',  ( 8.444030743212801227, 8.745790710036752458, 0.7998128361456462443 ) ) ;
#132344 = CARTESIAN_POINT ( 'NONE',  ( 3.380092458137720968, -2.014432998692190058, -0.09411721906785883163 ) ) ;
#132346 = CARTESIAN_POINT ( 'NONE',  ( 0.9076408456279178028, -0.8746481411591797706, -1.734042483418346547 ) ) ;
#132347 = CARTESIAN_POINT ( 'NONE',  ( -5.447678794592645701, 5.250046769979851646, 0.000000000000000000 ) ) ;
#132348 = CARTESIAN_POINT ( 'NONE',  ( 2.680963302754415079, 0.4788041664859938318, -0.1016165050511480955 ) ) ;
#132349 = CARTESIAN_POINT ( 'NONE',  ( -4.359828915246279024, 7.244161613499399799, -1.199719254218455378 ) ) ;
#132350 = AXIS2_PLACEMENT_3D ( 'NONE', #152629, #3149, #115927 ) ;
#132351 = CARTESIAN_POINT ( 'NONE',  ( 3.045614982896325262, 0.6747646648952825288, -1.744891315567910439 ) ) ;
#132352 = AXIS2_PLACEMENT_3D ( 'NONE', #181149, #113028, #14365 ) ;
#132353 = B_SPLINE_CURVE_WITH_KNOTS ( 'NONE', 3,
 ( #114174, #162861, #97868, #15504, #81591, #12310, #195353, #78391, #144511, #210519 ),
 .UNSPECIFIED., .F., .F.,
 ( 4, 2, 2, 2, 4 ),
 ( 0.000000000000000000, 0.0002216178067634652128, 0.0004432356135269304256, 0.0006648534202903956655, 0.0008864712270538608512 ),
 .UNSPECIFIED. ) ;
#132356 = CARTESIAN_POINT ( 'NONE',  ( -5.074494633264801990, 9.142270515442742607, 0.7998128361456291469 ) ) ;
#132355 = CARTESIAN_POINT ( 'NONE',  ( -0.6823417656249969321, 5.717708333674756283, -1.181850606188749264 ) ) ;
#132354 = CARTESIAN_POINT ( 'NONE',  ( 1.089939655121434203, 1.141396045679959004, 1.534244836814010693 ) ) ;
#132357 = CARTESIAN_POINT ( 'NONE',  ( 3.053566222061272040, -1.804402116661915967, -1.270350324234905903 ) ) ;
#132358 = EDGE_CURVE ( 'NONE', #20115, #73634, #163720, .T. ) ;
#132359 = CARTESIAN_POINT ( 'NONE',  ( 4.977251789548238214, 7.860525283564661514, -1.082531754730548412 ) ) ;
#132360 = CARTESIAN_POINT ( 'NONE',  ( 2.205172540517054802, 5.724451730578533848, 1.040834085586084257E-14 ) ) ;
#132361 = CARTESIAN_POINT ( 'NONE',  ( 7.160114521348466710, 7.526090827760914870, 0.000000000000000000 ) ) ;
#132362 = CARTESIAN_POINT ( 'NONE',  ( -2.598358995313378550, 6.183169261174235487, 0.7998128361456341429 ) ) ;
#132363 = CARTESIAN_POINT ( 'NONE',  ( -5.736508391913536897, 9.706693867292189637, 0.7216878364870267237 ) ) ;
#132364 = CARTESIAN_POINT ( 'NONE',  ( 0.9835902346791641770, 1.320712255264442803, 1.463733941802777716 ) ) ;
#132365 = CARTESIAN_POINT ( 'NONE',  ( 6.621674845842873580, -2.240319515690874397, 0.5532079777821105049 ) ) ;
#132366 = CARTESIAN_POINT ( 'NONE',  ( 1.521847698614446687, 1.933392594956625521, -0.3320675068423510345 ) ) ;
#132367 = CARTESIAN_POINT ( 'NONE',  ( 5.383662037909134668, -1.960299721042932930, 0.6417261926762083402 ) ) ;
#132368 = CARTESIAN_POINT ( 'NONE',  ( 5.856759171423504107, 5.935233242856626568, -0.7216878364870257245 ) ) ;
#132369 = CARTESIAN_POINT ( 'NONE',  ( 6.530187263637528439, 7.647581891445782709, -1.199719254218452047 ) ) ;
#132370 = ORIENTED_EDGE ( 'NONE', *, *, #165324, .T. ) ;
#132371 = CARTESIAN_POINT ( 'NONE',  ( 1.364683531249990311, 4.696875000341417916, 1.214306433183764966E-14 ) ) ;
#132372 = LINE ( 'NONE', #4424, #163094 ) ;
#132373 = CARTESIAN_POINT ( 'NONE',  ( 2.684151225381301575, 6.075334163012737321, 0.000000000000000000 ) ) ;
#132374 = CARTESIAN_POINT ( 'NONE',  ( 0.7784788067067629491, -1.160020112895485456, -1.834993543685500939 ) ) ;
#132376 = CARTESIAN_POINT ( 'NONE',  ( 5.899929530298204661, -0.6689130865737795695, -1.715630562827724637 ) ) ;
#132375 = LINE ( 'NONE', #118279, #18169 ) ;
#132377 = ADVANCED_FACE ( 'NONE', ( #24381 ), #13978, .T. ) ;
#132378 = CARTESIAN_POINT ( 'NONE',  ( 11.84104725192634966, 12.49016462548580542, 1.443823348526939165 ) ) ;
#132379 = CARTESIAN_POINT ( 'NONE',  ( 0.3000000000000016542, 4.000000000000003553, -1.007084189318387502 ) ) ;
#132380 = CARTESIAN_POINT ( 'NONE',  ( 1.352582913587907942, -1.478046865151939393, 1.146363905606573086 ) ) ;
#132381 = CARTESIAN_POINT ( 'NONE',  ( 5.905597126736788383, -0.5315564325061740147, 2.095088507090197893 ) ) ;
#132383 = CARTESIAN_POINT ( 'NONE',  ( -5.867374215541069304, 6.167859493020809047, 0.9100554989533160555 ) ) ;
#132382 = AXIS2_PLACEMENT_3D ( 'NONE', #182038, #81362, #179937 ) ;
#132384 = CARTESIAN_POINT ( 'NONE',  ( 1.500000000000065503, 7.750000000000000000, -10.99818166789400919 ) ) ;
#132385 = CARTESIAN_POINT ( 'NONE',  ( 5.696489930276292135, 7.416392257432566026, -1.320530921439456273 ) ) ;
#132386 = CARTESIAN_POINT ( 'NONE',  ( 1.364683531249992088, 5.696875000341418804, 1.214306433183764966E-14 ) ) ;
#132387 = CARTESIAN_POINT ( 'NONE',  ( 0.9789966485893276671, -1.729064073676725544, -0.8170501332188941923 ) ) ;
#132388 = CARTESIAN_POINT ( 'NONE',  ( 2.570886989259568267, 0.08925172825972882418, -1.767725737713058631 ) ) ;
#132389 = CARTESIAN_POINT ( 'NONE',  ( 1.260255548581414642, 1.910129771108992625, 0.09294656408432439010 ) ) ;
#132391 = CARTESIAN_POINT ( 'NONE',  ( 4.939036846723444008, -1.620647644904899654, -1.020970555301304206 ) ) ;
#132390 = CARTESIAN_POINT ( 'NONE',  ( 2.287227787140717172, -3.222749323649096720, 2.379012648498802118 ) ) ;
#132392 = CARTESIAN_POINT ( 'NONE',  ( 6.021921669442146907, 1.940670798679052123, -0.3350140356708011802 ) ) ;
#132393 = CARTESIAN_POINT ( 'NONE',  ( -1.001543065824772872E-14, 4.962500000000019007, 1.732050807568877637 ) ) ;
#132394 = CARTESIAN_POINT ( 'NONE',  ( 1.476976393720278002, -1.495863523836362896, 1.503369785937097136 ) ) ;
#132395 = CARTESIAN_POINT ( 'NONE',  ( -1.734299959503179353E-15, -8.332912386296857932, -10.92578969873748740 ) ) ;
#132396 = CARTESIAN_POINT ( 'NONE',  ( 4.047608660086319254, 0.6306619223146043840, -1.761260876548931709 ) ) ;
#132398 = ORIENTED_EDGE ( 'NONE', *, *, #168226, .T. ) ;
#132397 = CARTESIAN_POINT ( 'NONE',  ( 0.2053145577999641036, -0.4904175937916722128, 1.758528939493007481 ) ) ;
#132400 = CARTESIAN_POINT ( 'NONE',  ( 4.768187943840554333, 8.164982483533503199, -0.7738548252242994918 ) ) ;
#132399 = CARTESIAN_POINT ( 'NONE',  ( 4.881566871873391555, 2.059980941486462047, -0.7921658822237286346 ) ) ;
#132401 = CARTESIAN_POINT ( 'NONE',  ( 1.364683531249988535, 4.717708333674756283, -0.7879004041258300672 ) ) ;
#132402 = CARTESIAN_POINT ( 'NONE',  ( 1.662626038903247228, -0.7403543059694576156, -1.925410787417888958 ) ) ;
#132403 = CARTESIAN_POINT ( 'NONE',  ( 5.099838337034727331, 9.101561826515851550, -0.7998128361456281477 ) ) ;
#132404 = CARTESIAN_POINT ( 'NONE',  ( -8.642432853707342488, 12.17025653171218558, 1.199719254218462483 ) ) ;
#132405 = CARTESIAN_POINT ( 'NONE',  ( 0.000000000000000000, 0.02011834319527033843, -6.938893903907228378E-15 ) ) ;
#132406 = DIRECTION ( 'NONE',  ( -0.000000000000000000, -1.000000000000000000, -0.000000000000000000 ) ) ;
#132407 = EDGE_CURVE ( 'NONE', #123409, #79803, #177218, .T. ) ;
#132408 = CARTESIAN_POINT ( 'NONE',  ( 6.486579876843340919, -1.171037552013409089, 1.512559164390047561 ) ) ;
#132409 = VERTEX_POINT ( 'NONE', #155818 ) ;
#132410 = CARTESIAN_POINT ( 'NONE',  ( 4.457524453155742528, 1.660904245173303373, 1.235824716467534889 ) ) ;
#132411 = CARTESIAN_POINT ( 'NONE',  ( -1.402160292154681736E-14, -0.9906249996585834161, -1.575800808251665908 ) ) ;
#132412 = CARTESIAN_POINT ( 'NONE',  ( 1.774925396934714295, -2.051924176137665423, -0.6798970441593693570 ) ) ;
#132413 = CARTESIAN_POINT ( 'NONE',  ( -5.355672060655169098, 7.601107163255693244, -1.239215230201977436 ) ) ;
#132414 = CARTESIAN_POINT ( 'NONE',  ( 1.611979286579327431, -0.6784349324776539625, 1.902464779174169562 ) ) ;
#132415 = CARTESIAN_POINT ( 'NONE',  ( -9.578206935422265644, -9.825744180092243596, 0.1671882239536719994 ) ) ;
#132416 = VERTEX_POINT ( 'NONE', #71328 ) ;
#132417 = ORIENTED_EDGE ( 'NONE', *, *, #143084, .T. ) ;
#132419 = CARTESIAN_POINT ( 'NONE',  ( 6.778713617152772208, 10.85232362007950258, -0.7216878364870267237 ) ) ;
#132418 = CARTESIAN_POINT ( 'NONE',  ( 1.001543065824772753E-15, -2.712499999999999911, 4.012584370867899430 ) ) ;
#132420 = CARTESIAN_POINT ( 'NONE',  ( 0.08269815893116483352, -5.360092950639683274, 10.99976946526262900 ) ) ;
#132421 = CARTESIAN_POINT ( 'NONE',  ( 0.1808755166769344669, 1.673851406602990366, -1.124249698880399162 ) ) ;
#132422 = CYLINDRICAL_SURFACE ( 'NONE', #62130, 1.250000000000000000 ) ;
#132423 = CARTESIAN_POINT ( 'NONE',  ( 5.214472588068230330, 2.024700573814151028, 0.8392323156421463981 ) ) ;
#132424 = CARTESIAN_POINT ( 'NONE',  ( 1.499999999999987121, 3.077083334016149863, -0.8660254037844262731 ) ) ;
#132425 = CARTESIAN_POINT ( 'NONE',  ( 3.832203377193269755, -0.9874410831685247469, -1.637625244210038300 ) ) ;
#132426 = CARTESIAN_POINT ( 'NONE',  ( -6.064574784014443942, 5.969758757638621738, -0.7998128361456291469 ) ) ;
#132427 = CARTESIAN_POINT ( 'NONE',  ( 4.867013957181530515, 5.740899707208986236, -1.082531754730548412 ) ) ;
#132429 = CARTESIAN_POINT ( 'NONE',  ( 2.513296185832504470, -1.880429104915388727, 0.7283969491318904588 ) ) ;
#132428 = DIRECTION ( 'NONE',  ( 0.05872483221476467591, -7.952201780260630618E-17, -0.9982742078614211811 ) ) ;
#132430 = CARTESIAN_POINT ( 'NONE',  ( -0.6823417656250003738, 12.21354166700806765, 1.181850606188754593 ) ) ;
#132432 = CARTESIAN_POINT ( 'NONE',  ( -4.359828915246279024, 7.244161613499399799, -1.199719254218455378 ) ) ;
#132431 = CARTESIAN_POINT ( 'NONE',  ( 0.5040057298127769148, -2.280580521882575429, 0.2324455964911649464 ) ) ;
#132433 = CARTESIAN_POINT ( 'NONE',  ( 4.418794198169028853, 1.577559062085803765, 0.6976772398503274797 ) ) ;
#132434 = CARTESIAN_POINT ( 'NONE',  ( 7.526711554241970248, 8.810193563817646734, -1.199719254218452047 ) ) ;
#132435 = CARTESIAN_POINT ( 'NONE',  ( 3.171717870593107058, 5.787755718078879674, -1.199719254218446718 ) ) ;
#132436 = FACE_OUTER_BOUND ( 'NONE', #4385, .T. ) ;
#132437 = CARTESIAN_POINT ( 'NONE',  ( 0.7484013653801385724, -1.946605496936428370, -0.2438083268051088881 ) ) ;
#132438 = CARTESIAN_POINT ( 'NONE',  ( -10.55819884875827697, -6.268611901546719878, 1.734723475976807094E-15 ) ) ;
#132439 = CARTESIAN_POINT ( 'NONE',  ( 2.855963913973019963, 6.483708332943829866, 0.000000000000000000 ) ) ;
#132440 = CARTESIAN_POINT ( 'NONE',  ( 0.1753634416057740786, 1.334841368177059895, -2.397339160348281428 ) ) ;
#132441 = EDGE_LOOP ( 'NONE', ( #105017, #198037, #56991, #94624 ) ) ;
#132443 = AXIS2_PLACEMENT_3D ( 'NONE', #4190, #155817, #37792 ) ;
#132442 = DIRECTION ( 'NONE',  ( 1.000000000000000000, -0.000000000000000000, -0.000000000000000000 ) ) ;
#132444 = ADVANCED_FACE ( 'NONE', ( #37793 ), #88690, .F. ) ;
#132445 = EDGE_LOOP ( 'NONE', ( #42154, #43415, #106967, #82154, #213937, #28381, #146685 ) ) ;
#132446 = CARTESIAN_POINT ( 'NONE',  ( 5.145072886348948771, 0.1388508722429954989, 1.806219837558323826 ) ) ;
#132447 = ORIENTED_EDGE ( 'NONE', *, *, #159943, .T. ) ;
#132449 = CARTESIAN_POINT ( 'NONE',  ( 6.540882763950133238, 6.595727744222092959, 0.000000000000000000 ) ) ;
#132448 = CIRCLE ( 'NONE', #42444, 0.07999999999999968248 ) ;
#132450 = CARTESIAN_POINT ( 'NONE',  ( 7.721398836998367265, -6.134628647623499909, -7.721398836998390358 ) ) ;
#132451 = CARTESIAN_POINT ( 'NONE',  ( 5.971335983229998590, -1.557292021941504734, -0.9250951156042800383 ) ) ;
#132452 = CARTESIAN_POINT ( 'NONE',  ( 6.089020385868848528, 8.197219431637373432, -1.443375672974078761 ) ) ;
#132453 = DIRECTION ( 'NONE',  ( 3.347138415753902517E-16, 0.6000000000000019762, 0.7999999999999986011 ) ) ;
#132454 = CARTESIAN_POINT ( 'NONE',  ( 5.678179657697552507, 6.109196432984326464, -0.7486794562398890740 ) ) ;
#132456 = CARTESIAN_POINT ( 'NONE',  ( 10.55232363013785246, 11.20546574478267132, 0.000000000000000000 ) ) ;
#132455 = CARTESIAN_POINT ( 'NONE',  ( 6.408657378324259746, 0.5850815967071677504, 1.766781856238110127 ) ) ;
#132457 = CARTESIAN_POINT ( 'NONE',  ( 3.286649939900693429, 1.508079230315559016, -1.181058552281685659 ) ) ;
#132458 = CARTESIAN_POINT ( 'NONE',  ( 0.000000000000000000, 19.00000000000000000, 0.000000000000000000 ) ) ;
#132459 = CARTESIAN_POINT ( 'NONE',  ( 5.829642864196162400, 7.824335979694092558, 1.443375672974062551 ) ) ;
#132461 = CARTESIAN_POINT ( 'NONE',  ( 5.770749444886737578, -0.3132382886438951908, -2.093953712743265694 ) ) ;
#132460 = CARTESIAN_POINT ( 'NONE',  ( -8.663296969452339624, 13.05100419776235299, 1.040834085586084257E-14 ) ) ;
#132462 = CARTESIAN_POINT ( 'NONE',  ( 0.2159880523044250267, -2.119658899406823505, 0.4233941889316418239 ) ) ;
#132463 = CARTESIAN_POINT ( 'NONE',  ( -5.448397627845328550, 7.449826213943242514, 1.599625672291263179 ) ) ;
#132464 = CARTESIAN_POINT ( 'NONE',  ( 4.716257332707354699, 6.595662536282280719, -1.599625672291269396 ) ) ;
#132465 = CARTESIAN_POINT ( 'NONE',  ( 1.395219695971817941, 1.379742824092672349, 1.195523663710513995 ) ) ;
#132466 = CARTESIAN_POINT ( 'NONE',  ( -4.172158584703340445, 5.890604320285754980, -1.599625672291256295 ) ) ;
#132467 = CARTESIAN_POINT ( 'NONE',  ( 3.750846114953470867, -1.492790808496821775, 1.050590184284278861 ) ) ;
#132468 = CARTESIAN_POINT ( 'NONE',  ( 8.366200769982176766, 13.06116137083107098, 8.526426475962127327 ) ) ;
#132469 = CARTESIAN_POINT ( 'NONE',  ( 2.513799616133075343, -0.5961229146635020903, 1.817204401178821760 ) ) ;
#132470 = ORIENTED_EDGE ( 'NONE', *, *, #164748, .F. ) ;
#132471 = CARTESIAN_POINT ( 'NONE',  ( 3.174220446822792141, -0.9683065041741106826, -1.714983525329449421 ) ) ;
#132472 = CARTESIAN_POINT ( 'NONE',  ( 4.792492878049551486, 1.612589784423448025, -1.081918670939057137 ) ) ;
#132473 = CARTESIAN_POINT ( 'NONE',  ( -7.075376061485238566, 9.347967719856493218, 1.599625672291269396 ) ) ;
#132475 = CARTESIAN_POINT ( 'NONE',  ( 5.660427296577901224, 2.118236611397010805, 0.1021076702828054988 ) ) ;
#132474 = CARTESIAN_POINT ( 'NONE',  ( 7.666209513884374438, 7.908608952478760834, 0.7998128361456281477 ) ) ;
#132476 = CARTESIAN_POINT ( 'NONE',  ( 4.726684935852882852, 4.891486930089099516, -0.8194250277325196841 ) ) ;
#132477 = CARTESIAN_POINT ( 'NONE',  ( 2.736851483355093873, 1.801321139115559244, 0.6423184003811268639 ) ) ;
#132478 = CARTESIAN_POINT ( 'NONE',  ( 6.110807642276722795, 6.018297815386236316, -0.1222484578899986352 ) ) ;
#132479 = B_SPLINE_CURVE_WITH_KNOTS ( 'NONE', 3,
 ( #206978, #140968, #186462, #203764, #124763, #105246, #107424, #38098, #205912, #73786 ),
 .UNSPECIFIED., .F., .F.,
 ( 4, 2, 2, 2, 4 ),
 ( 0.000000000000000000, 0.0005407846995530511116, 0.001081569399106102223, 0.001622354098659153226, 0.002163138798212204447 ),
 .UNSPECIFIED. ) ;
#132480 = CARTESIAN_POINT ( 'NONE',  ( -4.650083499807243115, 5.295740330745369207, -1.052294140492322283 ) ) ;
#132481 = CARTESIAN_POINT ( 'NONE',  ( 4.309512724297349884, 6.121127159803966933, 1.599625672291261402 ) ) ;
#132482 = CIRCLE ( 'NONE', #11360, 0.08000000000000025147 ) ;
#132483 = CARTESIAN_POINT ( 'NONE',  ( 0.08367765422324577318, -9.912493506416723221, 9.499631469177300502 ) ) ;
#132484 = CARTESIAN_POINT ( 'NONE',  ( 4.582524934692378871, -1.771534430979417429, -0.4408631061849078714 ) ) ;
#132485 = CARTESIAN_POINT ( 'NONE',  ( 0.8013346216862862192, -1.776568573310655985, 1.062853015585236482 ) ) ;
#132486 = CARTESIAN_POINT ( 'NONE',  ( -8.297226821883391779, 11.66355314463053006, 1.082531754730549967 ) ) ;
#132487 = CARTESIAN_POINT ( 'NONE',  ( -6.126043159632901691, 7.090966632250176538, 1.117993467579528222 ) ) ;
#132488 = CARTESIAN_POINT ( 'NONE',  ( 1.203907071533380613, 2.868479746939697872, -0.7749999999999910294 ) ) ;
#132489 = CARTESIAN_POINT ( 'NONE',  ( 5.401189721097995111, 1.529905263132097071, 1.076157610686766075 ) ) ;
#132490 = CARTESIAN_POINT ( 'NONE',  ( 8.776205506747620788, 9.133327934160710981, -0.7998128361456221525 ) ) ;
#132491 = CARTESIAN_POINT ( 'NONE',  ( -4.924636110261798372, 6.768494766770632332, 1.599625672291267175 ) ) ;
#132492 = EDGE_CURVE ( 'NONE', #129260, #42950, #149951, .T. ) ;
#132493 = CARTESIAN_POINT ( 'NONE',  ( 3.083589872104280705, 5.684939719841914929, 1.199719254218450271 ) ) ;
#132494 = CARTESIAN_POINT ( 'NONE',  ( -0.6823417656250039265, 10.88020833367472839, -1.181850606188755259 ) ) ;
#132495 = CARTESIAN_POINT ( 'NONE',  ( -4.550733115681270036, 8.460939068270139529, 0.7998128361456481317 ) ) ;
#132496 = CARTESIAN_POINT ( 'NONE',  ( 2.686486993802192913, 6.285985259411197568, 0.7998128361456362523 ) ) ;
#132497 = CARTESIAN_POINT ( 'NONE',  ( -7.608060475923978494, 8.905100639113307182, 1.199719254218452047 ) ) ;
#132498 = CIRCLE ( 'NONE', #80673, 6.249999999999995559 ) ;
#132499 = CARTESIAN_POINT ( 'NONE',  ( -4.367698041896780126, 8.247398148854895084, 0.7998128361456481317 ) ) ;
#132500 = PRESENTATION_LAYER_ASSIGNMENT (  '', '', ( #104800 ) ) ;
#132501 = CARTESIAN_POINT ( 'NONE',  ( 6.719587830005472995, 0.3798626643731088937, -2.137457590422507714 ) ) ;
#132502 = CARTESIAN_POINT ( 'NONE',  ( 2.689187139871064502, 1.790190400678292715, 1.130151903539077463 ) ) ;
#132503 = CARTESIAN_POINT ( 'NONE',  ( 8.565000355531088516, 11.01558638625153286, -1.599625672291257406 ) ) ;
#132504 = CARTESIAN_POINT ( 'NONE',  ( 0.5056851195614943117, 6.800201140161028945, 3.700268186881439547 ) ) ;
#132505 = CARTESIAN_POINT ( 'NONE',  ( 6.614133338355735248, 2.065126723422955557, -0.1462301744803648496 ) ) ;
#132506 = CARTESIAN_POINT ( 'NONE',  ( 4.420695050690802930, 7.093836324768183488, -1.099706215833176515 ) ) ;
#132507 = CARTESIAN_POINT ( 'NONE',  ( 6.493992391265805075, 6.678671999339316656, 1.040834085586084257E-14 ) ) ;
#132509 =( LENGTH_UNIT ( ) NAMED_UNIT ( * ) SI_UNIT ( .MILLI., .METRE. ) );
#132508 = CARTESIAN_POINT ( 'NONE',  ( 3.475000000000000533, -3.004166666666665542, 2.006292185433948827 ) ) ;
#132510 = CARTESIAN_POINT ( 'NONE',  ( 2.326505592738498329, 2.223965110380062615, 0.5549310701656160472 ) ) ;
#132512 = CARTESIAN_POINT ( 'NONE',  ( 0.2333690889706726279, 7.629137130509075604, -2.653349640194931247 ) ) ;
#132511 = CARTESIAN_POINT ( 'NONE',  ( 0.01192831195480706721, -0.7772932952810689411, -1.650495136788888040 ) ) ;
#132513 = CARTESIAN_POINT ( 'NONE',  ( 2.496234081663367022, -0.9796988711565941532, 1.642222327643327873 ) ) ;
#132514 = VERTEX_POINT ( 'NONE', #7402 ) ;
#132515 = CARTESIAN_POINT ( 'NONE',  ( 8.066738210006686671, 9.473911335505048825, 1.082531754730558626 ) ) ;
#132516 = AXIS2_PLACEMENT_3D ( 'NONE', #65684, #119865, #181585 ) ;
#132517 = CARTESIAN_POINT ( 'NONE',  ( 0.1760394598168211200, 1.990691791301450575, -0.2996127288820998325 ) ) ;
#132518 = CARTESIAN_POINT ( 'NONE',  ( 0.8484012048698870156, -1.946262134508335739, -0.2457884297097159831 ) ) ;
#132519 = CARTESIAN_POINT ( 'NONE',  ( -8.611400122974211868, 13.19838391011195888, 1.040834085586084257E-14 ) ) ;
#132520 = CARTESIAN_POINT ( 'NONE',  ( -7.446452682403657874, 9.710614100936176385, -1.599625672291263179 ) ) ;
#132521 = CARTESIAN_POINT ( 'NONE',  ( 0.000000000000000000, -0.6343749995220417937, -3.793834371823813001 ) ) ;
#132523 = CARTESIAN_POINT ( 'NONE',  ( 2.887294646099856532, 1.250245360129684791, 1.252957939402859600 ) ) ;
#132522 = CARTESIAN_POINT ( 'NONE',  ( 3.521503319566265944, -1.245636697800769355, -1.678868242315070258 ) ) ;
#132524 = CARTESIAN_POINT ( 'NONE',  ( 3.988012250146443449, 7.596505358572088085, 0.1212705993496351053 ) ) ;
#132526 = CARTESIAN_POINT ( 'NONE',  ( 5.437530556340149701, 0.9332327497303912756, -2.093863557220442484 ) ) ;
#132525 = CARTESIAN_POINT ( 'NONE',  ( 11.94105721237523277, 12.69999999999999929, -1.187919463087249827 ) ) ;
#132527 = CARTESIAN_POINT ( 'NONE',  ( 3.696946667989671642, -0.5033324012985186391, 1.665945954428204923 ) ) ;
#132528 = AXIS2_PLACEMENT_3D ( 'NONE', #193166, #178002, #48020 ) ;
#132529 = CARTESIAN_POINT ( 'NONE',  ( 3.460355519985863548, 5.060167411448709629, 1.599625672291267398 ) ) ;
#132530 = DIRECTION ( 'NONE',  ( -0.5994789404140901112, 2.055006554627987857E-15, 0.8003905296791060664 ) ) ;
#132531 = CARTESIAN_POINT ( 'NONE',  ( 2.899396954618923772, 0.2085115220819243054, 1.721149687620449953 ) ) ;
#132532 = CARTESIAN_POINT ( 'NONE',  ( 3.297511149327167601, -1.916070068265750992, 1.021083071776592410 ) ) ;
#132533 = CARTESIAN_POINT ( 'NONE',  ( 2.347533153460546806, 5.890539112345938300, 0.000000000000000000 ) ) ;
#132534 = CARTESIAN_POINT ( 'NONE',  ( 5.823453932400854960, -1.463924103857511039, -1.387103351090559711 ) ) ;
#132535 = CARTESIAN_POINT ( 'NONE',  ( 0.6875000000000004441, -1.451031289061094132, 1.451031289061148755 ) ) ;
#132536 = CARTESIAN_POINT ( 'NONE',  ( -0.7500000000000215383, 4.472916667349482012, 1.299038105676671107 ) ) ;
#132537 = CARTESIAN_POINT ( 'NONE',  ( 2.186434445367648749, -1.888794084208703206, -0.3779312967549207092 ) ) ;
#132538 = CARTESIAN_POINT ( 'NONE',  ( -1.500000000000015099, 9.260416667349463893, -0.8660254037844309360 ) ) ;
#132539 = CARTESIAN_POINT ( 'NONE',  ( 5.625276811391259457, 1.958927336128764241, 1.047432077188856780 ) ) ;
#132540 = ORIENTED_EDGE ( 'NONE', *, *, #98818, .F. ) ;
#132541 = CARTESIAN_POINT ( 'NONE',  ( 6.883263157960391787, 1.249388486322531078, 2.158948101847418144 ) ) ;
#132542 = CARTESIAN_POINT ( 'NONE',  ( -1.201851678989727383E-14, 2.212500000000021672, 1.732050807568877637 ) ) ;
#132543 = CARTESIAN_POINT ( 'NONE',  ( 5.750629710490689384, 9.860818428881154674, -0.7998128361456291469 ) ) ;
#132544 = CARTESIAN_POINT ( 'NONE',  ( 5.639828713160493834, 5.682147708216442439, 1.040834085586084257E-14 ) ) ;
#132545 = CARTESIAN_POINT ( 'NONE',  ( 1.629831963231648029, -0.2677717415913836718, 2.205032603725831652 ) ) ;
#132546 = CARTESIAN_POINT ( 'NONE',  ( 7.727784370109387346, 10.99920361756089093, -1.082531754730543083 ) ) ;
#132547 = FACE_OUTER_BOUND ( 'NONE', #99508, .T. ) ;
#132548 = CARTESIAN_POINT ( 'NONE',  ( 3.528865121306874464, 7.339036084825155015, -0.7998128361456362523 ) ) ;
#132549 = CARTESIAN_POINT ( 'NONE',  ( -3.797692425603673705, 6.484372692295976570, 1.082531754730549967 ) ) ;
#132550 = CARTESIAN_POINT ( 'NONE',  ( 4.545415624535277921, 1.843838458276589209, -0.9247144854665176883 ) ) ;
#132551 = CARTESIAN_POINT ( 'NONE',  ( -4.391951695823077984, 7.211361847513815704, 1.199719254218464037 ) ) ;
#132552 = CARTESIAN_POINT ( 'NONE',  ( -0.7499999999999972244, 3.889583334016149863, -1.299038105676652011 ) ) ;
#132553 = CARTESIAN_POINT ( 'NONE',  ( -1.364683531250014514, 0.2802083336747505649, 0.7879004041258379498 ) ) ;
#132554 = CARTESIAN_POINT ( 'NONE',  ( 5.852782322939767745, -1.474943281369223369, 1.150351685248012457 ) ) ;
#132555 = CARTESIAN_POINT ( 'NONE',  ( 4.764171500175623741, 1.615563337074712225, -0.6307657835151522230 ) ) ;
#132556 = CARTESIAN_POINT ( 'NONE',  ( 3.983749006537410153, -1.722186279587777369, -0.2504274415035238621 ) ) ;
#132557 = CARTESIAN_POINT ( 'NONE',  ( 3.011882680530176604, 6.665613560593854459, 0.7998128361456341429 ) ) ;
#132558 = CARTESIAN_POINT ( 'NONE',  ( 2.085838899777220590, -0.9763249575661275825, 2.074189754910108263 ) ) ;
#132559 = CARTESIAN_POINT ( 'NONE',  ( -1.364683531250010295, 5.551041667008087543, -0.7879004041258300672 ) ) ;
#132560 = CARTESIAN_POINT ( 'NONE',  ( 6.269093502906415871, 2.000459608610676288, -0.6076830679577133187 ) ) ;
#132561 = CARTESIAN_POINT ( 'NONE',  ( 1.517261703430743625, -1.021610662766696764, -1.531488883528262512 ) ) ;
#132562 = CARTESIAN_POINT ( 'NONE',  ( 1.723279953462612202, 1.994870059565261755, 0.2930690452552578429 ) ) ;
#132563 = CARTESIAN_POINT ( 'NONE',  ( 3.563261906135761770, 6.332667919118538435, 2.420000000000010587 ) ) ;
#132564 = CARTESIAN_POINT ( 'NONE',  ( 7.296230878984865775, 15.96627503840708329, -9.125506818615267690 ) ) ;
#132565 = CARTESIAN_POINT ( 'NONE',  ( -7.660520486921249983, 8.896027641951645748, -1.199719254218446718 ) ) ;
#132566 = CARTESIAN_POINT ( 'NONE',  ( 3.832150974156964818, 7.622593236491780999, 1.040834085586084257E-14 ) ) ;
#132567 = CARTESIAN_POINT ( 'NONE',  ( -0.6801582343750004478, 2.598958333674746157, -1.178068619123848526 ) ) ;
#132568 = CARTESIAN_POINT ( 'NONE',  ( 3.264422710156249963, 2.120667954687505574, -0.001943060928578931989 ) ) ;
#132569 = CARTESIAN_POINT ( 'NONE',  ( -1.364683531250014514, -0.4697916663252449943, 0.7879004041258379498 ) ) ;
#132570 = CARTESIAN_POINT ( 'NONE',  ( 5.566980414702134894, -1.652319403193935887, -0.7768266693391965294 ) ) ;
#132571 = ORIENTED_EDGE ( 'NONE', *, *, #178101, .T. ) ;
#132572 = CARTESIAN_POINT ( 'NONE',  ( -4.769436176957319695, 8.786368983084006601, 0.7998128361456281477 ) ) ;
#132573 = CARTESIAN_POINT ( 'NONE',  ( 6.116136693096175136, 9.189224337703940648, -1.082531754730548412 ) ) ;
#132574 = CARTESIAN_POINT ( 'NONE',  ( -1.737499999999997824, -2.697916665710752060, 3.009438278150925683 ) ) ;
#132575 = CARTESIAN_POINT ( 'NONE',  ( -5.194745412330402878, 9.212286747694129474, 0.000000000000000000 ) ) ;
#132576 = CARTESIAN_POINT ( 'NONE',  ( 3.621357264417348620, 1.734514936435461507, 1.034602781942542515 ) ) ;
#132577 = CARTESIAN_POINT ( 'NONE',  ( 6.633804142636003931, -1.436369002829580133, -1.675418478561958802 ) ) ;
#132578 = CARTESIAN_POINT ( 'NONE',  ( -7.456058132872594335, 7.663432341298296535, 0.000000000000000000 ) ) ;
#132579 = CARTESIAN_POINT ( 'NONE',  ( -3.363304624641834106, 6.081549941127532222, -1.199719254218452047 ) ) ;
#132580 = CARTESIAN_POINT ( 'NONE',  ( 4.662867571641106323, 1.440366211568647303, -1.178370841985799888 ) ) ;
#132581 = CARTESIAN_POINT ( 'NONE',  ( 9.399880572976245574, 9.860948844760784482, 0.7998128361456462443 ) ) ;
#132582 = CARTESIAN_POINT ( 'NONE',  ( -10.04321860110356468, 4.586749146271848154, -6.488091244683950265 ) ) ;
#132583 = CARTESIAN_POINT ( 'NONE',  ( -3.307299406729781399, 5.945934176904983381, -1.199719254218452935 ) ) ;
#132584 = CARTESIAN_POINT ( 'NONE',  ( -8.518600588087975822, 8.832788862391110385, 1.040834085586084257E-14 ) ) ;
#132585 = CARTESIAN_POINT ( 'NONE',  ( 6.473517581629535833, 1.972881934646727231, -0.5958391983454867091 ) ) ;
#132586 = TOROIDAL_SURFACE ( 'NONE', #21814, 1.914481421317583587, 0.05000000000000000278 ) ;
#132588 = CARTESIAN_POINT ( 'NONE',  ( -4.243318646243602998, 7.513047557524930475, 1.036732258902311354 ) ) ;
#132587 = CARTESIAN_POINT ( 'NONE',  ( -6.557303570864871034, 7.679217583210999010, -1.199719254218452047 ) ) ;
#132589 = CARTESIAN_POINT ( 'NONE',  ( -1.364683531250014514, 0.03020833367475737191, 0.7879004041258379498 ) ) ;
#132590 = CARTESIAN_POINT ( 'NONE',  ( 1.211752002169782738, -1.362220228754877027, -1.072495211514002289 ) ) ;
#132591 = CARTESIAN_POINT ( 'NONE',  ( 0.7436347644121766853, 0.5012835123295921180, 1.666554394910790382 ) ) ;
#132593 = CARTESIAN_POINT ( 'NONE',  ( 8.107412671292035355, 10.48173408797264194, 1.443375672974076540 ) ) ;
#132592 = CARTESIAN_POINT ( 'NONE',  ( 6.533790081910475500, -1.501629927769430273, -1.752384480091616847 ) ) ;
#132594 = CARTESIAN_POINT ( 'NONE',  ( 3.984117037569365305, 5.741498858621315371, 1.599625672291261402 ) ) ;
#132595 = CARTESIAN_POINT ( 'NONE',  ( 2.161468745749118625, 0.3553341821136410950, -2.029755476197503850 ) ) ;
#132596 = CARTESIAN_POINT ( 'NONE',  ( 1.686874821769188237, -1.117660090026689979, -1.677749154088927552 ) ) ;
#132597 = CARTESIAN_POINT ( 'NONE',  ( 0.9311234436981545848, -1.503130369558482560, -3.474999999999999201 ) ) ;
#132598 = CARTESIAN_POINT ( 'NONE',  ( -6.622231685632140596, 6.690634819517756959, 0.000000000000000000 ) ) ;
#132599 = CARTESIAN_POINT ( 'NONE',  ( 0.1980364362535640133, -1.970970528886636153, -0.05095907160383715551 ) ) ;
#132601 = CARTESIAN_POINT ( 'NONE',  ( -7.444835747679825033, 7.858265591814152629, 0.000000000000000000 ) ) ;
#132600 = CARTESIAN_POINT ( 'NONE',  ( 4.939673314881130040, -1.814047719456039154, 0.6055163330952323397 ) ) ;
#132602 = CARTESIAN_POINT ( 'NONE',  ( 5.654950187766193181, -1.741821662664808867, 1.355018943897445149 ) ) ;
#132603 = CARTESIAN_POINT ( 'NONE',  ( -6.577113915960841162, 7.806292669110006521, -1.082531754730549967 ) ) ;
#132604 = CARTESIAN_POINT ( 'NONE',  ( 7.849244587668864348, 8.122149871893999062, 0.7998128361456291469 ) ) ;
#132605 = CARTESIAN_POINT ( 'NONE',  ( -3.146901051703345331, 6.685485303713597283, 0.000000000000000000 ) ) ;
#132606 = CARTESIAN_POINT ( 'NONE',  ( 6.604144390287855160, -0.9070803646254663732, 1.914764756563241965 ) ) ;
#132607 = DIRECTION ( 'NONE',  ( 0.000000000000000000, 0.000000000000000000, -1.000000000000000000 ) ) ;
#132608 = CARTESIAN_POINT ( 'NONE',  ( 3.487651025411703021, 2.087124329425969371, -0.9845696281253720761 ) ) ;
#132609 = CARTESIAN_POINT ( 'NONE',  ( 4.580490334204036174, 1.208584658811951762, -1.545285769342201965 ) ) ;
#132610 = CARTESIAN_POINT ( 'NONE',  ( 1.393326438508041942, -1.775833184744341375, 0.8338576968042878956 ) ) ;
#132611 = CARTESIAN_POINT ( 'NONE',  ( 9.856941372335116469, 11.45851867493453291, 1.199719254218450271 ) ) ;
#132612 = CARTESIAN_POINT ( 'NONE',  ( -9.342889097980298985, 15.44694756379904099, 7.460114341897615908 ) ) ;
#132613 = VERTEX_POINT ( 'NONE', #56179 ) ;
#132614 = CARTESIAN_POINT ( 'NONE',  ( -0.06503379110851194300, -1.696408147887063178, 1.266814603907985504 ) ) ;
#132615 = CARTESIAN_POINT ( 'NONE',  ( -3.276266675996675204, 6.974061555304760240, -0.7998128361456281477 ) ) ;
#132616 = CARTESIAN_POINT ( 'NONE',  ( 1.288719586054212884, 1.393062650230517674, 1.203921758438614376 ) ) ;
#132617 = CARTESIAN_POINT ( 'NONE',  ( 4.293918747171243666, -1.492831977124044363, -1.576629974643141363 ) ) ;
#132618 = CARTESIAN_POINT ( 'NONE',  ( 1.499999999999961364, 7.750000000000000000, -10.64483442802188762 ) ) ;
#132620 = EDGE_CURVE ( 'NONE', #127089, #96541, #28520, .T. ) ;
#132619 = CARTESIAN_POINT ( 'NONE',  ( 1.336355901170083849, -1.182550835430173919, -1.760063440837428272 ) ) ;
#132621 = CARTESIAN_POINT ( 'NONE',  ( -1.500000000000013101, 2.452083334016154748, 0.8660254037844403729 ) ) ;
#132622 = CARTESIAN_POINT ( 'NONE',  ( 9.725276259704228821, 10.24057714594344048, 0.7998128361456462443 ) ) ;
#132623 = CARTESIAN_POINT ( 'NONE',  ( 11.95360554405587195, 13.60444996502594428, -1.059413164304662924 ) ) ;
#132624 = CARTESIAN_POINT ( 'NONE',  ( 6.589288424369031283, 6.777081280454712697, 0.2339771526987007022 ) ) ;
#132625 = CARTESIAN_POINT ( 'NONE',  ( 2.284514177335088991, -2.020382039854185408, -0.4051362335234820478 ) ) ;
#132626 = CIRCLE ( 'NONE', #39204, 0.04999999999999883010 ) ;
#132628 = CYLINDRICAL_SURFACE ( 'NONE', #190117, 3.475000000000000089 ) ;
#132627 = CARTESIAN_POINT ( 'NONE',  ( -8.208571938070008400, 11.66408546346865016, -1.199719254218446718 ) ) ;
#132629 = CARTESIAN_POINT ( 'NONE',  ( -0.6823417656250003738, 1.967708333674753174, -1.181850606188749264 ) ) ;
#132630 = DIRECTION ( 'NONE',  ( -5.578564026256490882E-16, -1.000000000000000000, -9.066213480720158442E-32 ) ) ;
#132631 = ORIENTED_EDGE ( 'NONE', *, *, #123168, .T. ) ;
#132632 = CARTESIAN_POINT ( 'NONE',  ( 4.441997247558228779, -1.179148908705367482, -1.505365500079666852 ) ) ;
#132633 = CARTESIAN_POINT ( 'NONE',  ( 11.92619526248524586, 12.57255386085826032, -1.328859120100568170 ) ) ;
#132634 = CARTESIAN_POINT ( 'NONE',  ( 1.564152511173346749, 2.229009205740081434, -0.3863987453041685116 ) ) ;
#132635 = CARTESIAN_POINT ( 'NONE',  ( -3.789667630219657912, 4.380032642466370696, 1.199719254218462483 ) ) ;
#132636 = CARTESIAN_POINT ( 'NONE',  ( 0.9491188979427627181, -1.637284982186116400, 0.7756696494297130595 ) ) ;
#132637 = CARTESIAN_POINT ( 'NONE',  ( 2.342874207364954220, -1.669023557642179467, -0.9401844802782586275 ) ) ;
#132638 = CARTESIAN_POINT ( 'NONE',  ( 2.752462066230080495, -2.064650614848703825, -0.1547973748374023295 ) ) ;
#132639 = CARTESIAN_POINT ( 'NONE',  ( -1.364683531250000748, 1.071875000341421247, 0.000000000000000000 ) ) ;
#132640 = CARTESIAN_POINT ( 'NONE',  ( 0.9363264705049412218, 1.941902958617349961, 0.3393069938249710371 ) ) ;
#132641 = CARTESIAN_POINT ( 'NONE',  ( 5.549420396211061757, -1.520166291496179323, -1.183330462961203589 ) ) ;
#132643 = CARTESIAN_POINT ( 'NONE',  ( 5.772745519453025054, 7.247817053759448847, -1.191736586928717978 ) ) ;
#132642 = CARTESIAN_POINT ( 'NONE',  ( 1.506910664365119334, -0.8341063803433286239, -2.151852887045426765 ) ) ;
#132644 = CARTESIAN_POINT ( 'NONE',  ( -1.201851678989727383E-14, 1.321875000341419248, 1.575800808251672791 ) ) ;
#132645 = CARTESIAN_POINT ( 'NONE',  ( 5.301261097381549270, -1.770826635688247386, 1.057502194177829979 ) ) ;
#132646 = VECTOR ( 'NONE', #126170, 1000.000000000000000 ) ;
#132648 = CARTESIAN_POINT ( 'NONE',  ( -5.412729640353771465, 7.337937218544611895, 1.599625672291269396 ) ) ;
#132647 = CIRCLE ( 'NONE', #42654, 0.05000000000000002359 ) ;
#132649 = CARTESIAN_POINT ( 'NONE',  ( 1.000000000000001554, 6.468705557303653819, -4.925226524755053958 ) ) ;
#132650 = EDGE_CURVE ( 'NONE', #141262, #79190, #191150, .T. ) ;
#132652 = CARTESIAN_POINT ( 'NONE',  ( -0.7499999999999972244, 3.608333333333359150, -1.299038105676652011 ) ) ;
#132651 = CARTESIAN_POINT ( 'NONE',  ( 5.104563850188495344, -0.7068653695375884949, -1.983929190867816494 ) ) ;
#132653 = CARTESIAN_POINT ( 'NONE',  ( -1.364683531250012516, 3.301041667008084879, -0.7879004041258289570 ) ) ;
#132654 = CARTESIAN_POINT ( 'NONE',  ( 5.290363030411685763, -2.144575937485785566, -0.2703735795691122323 ) ) ;
#132655 = CARTESIAN_POINT ( 'NONE',  ( 5.777991907792089599, 1.989422559269612201, -0.3473161181037613954 ) ) ;
#132656 = FACE_OUTER_BOUND ( 'NONE', #103943, .T. ) ;
#132657 = CARTESIAN_POINT ( 'NONE',  ( -5.016153647376219382, 6.875265226737464985, 1.443375672974064550 ) ) ;
#132658 = AXIS2_PLACEMENT_3D ( 'NONE', #30215, #14997, #179669 ) ;
#132661 = CARTESIAN_POINT ( 'NONE',  ( 5.585596099150174965, 7.539614753807099667, -1.443375672974057666 ) ) ;
#132660 = CARTESIAN_POINT ( 'NONE',  ( -3.285556943749998737, -2.180208332855376518, 1.896917185911908499 ) ) ;
#132659 = CARTESIAN_POINT ( 'NONE',  ( 6.016786309414542622, 10.24161080428416426, 0.7998128361456341429 ) ) ;
#132662 = CARTESIAN_POINT ( 'NONE',  ( -6.005335696210345020, 5.970922831858983315, 0.7998128361456281477 ) ) ;
#132663 = CARTESIAN_POINT ( 'NONE',  ( 3.204314817619222211, 1.275555974797081049, -1.561881975048397209 ) ) ;
#132664 = CARTESIAN_POINT ( 'NONE',  ( -7.004758919754800139, 11.32396917302262018, 0.000000000000000000 ) ) ;
#132666 = CARTESIAN_POINT ( 'NONE',  ( 1.637338291174485510E-15, -6.530144695498204754, 11.00000000000000178 ) ) ;
#132665 = CARTESIAN_POINT ( 'NONE',  ( -3.521367211247373508, 5.131347717920458962, -1.599625672291256295 ) ) ;
#132667 = CARTESIAN_POINT ( 'NONE',  ( -1.201851678989727383E-14, 5.446875000341422357, -1.575800808251660134 ) ) ;
#132669 = CARTESIAN_POINT ( 'NONE',  ( -11.94980361058168938, 12.70000000000000107, -1.100000000000000311 ) ) ;
#132668 = CARTESIAN_POINT ( 'NONE',  ( 5.313408243115379292, -0.3210861823062813314, 2.137610926513198617 ) ) ;
#132670 = DIRECTION ( 'NONE',  ( 0.000000000000000000, 0.000000000000000000, -1.000000000000000000 ) ) ;
#132671 = CARTESIAN_POINT ( 'NONE',  ( -11.38926526437179731, 6.532335583446259086, -3.785035105474102934 ) ) ;
#132673 = CARTESIAN_POINT ( 'NONE',  ( 5.835564593388589572, 0.5826401998472263699, -1.930423629703325927 ) ) ;
#132672 = CARTESIAN_POINT ( 'NONE',  ( -6.521108698048772467, 9.591415333490143524, -1.082531754730537976 ) ) ;
#132674 = CARTESIAN_POINT ( 'NONE',  ( 0.7499999999999902300, 5.066666666666684193, -1.299038105676658228 ) ) ;
#132675 = CARTESIAN_POINT ( 'NONE',  ( 0.9434950454815290710, 0.7028112840000885209, -1.575391610592514757 ) ) ;
#132676 = CARTESIAN_POINT ( 'NONE',  ( 4.492547798081839794, 6.334668079219206049, 1.599625672291262513 ) ) ;
#132678 = CARTESIAN_POINT ( 'NONE',  ( 5.820193082016415609, 10.01225203898631655, 0.000000000000000000 ) ) ;
#132677 = CARTESIAN_POINT ( 'NONE',  ( 7.836249599018724865, 9.205007956019091608, -1.082531754730537976 ) ) ;
#132679 = DIRECTION ( 'NONE',  ( -0.9885327375000381167, 0.000000000000000000, 0.1510067114093955609 ) ) ;
#132680 = CARTESIAN_POINT ( 'NONE',  ( 6.538356921592370696, 1.850225872366149105, 0.2742375073267953045 ) ) ;
#132681 = CARTESIAN_POINT ( 'NONE',  ( 0.9615884438243198495, -1.588399402277500760, -1.236662224066273019 ) ) ;
#132683 = EDGE_CURVE ( 'NONE', #185122, #149864, #30824, .T. ) ;
#132682 = CARTESIAN_POINT ( 'NONE',  ( -7.227905289416804102, 8.565549271475310533, -1.082531754730549967 ) ) ;
#132684 = ORIENTED_EDGE ( 'NONE', *, *, #89482, .T. ) ;
#132685 = CARTESIAN_POINT ( 'NONE',  ( 10.01911233037458260, 10.79131192829960462, 0.7216878364870438212 ) ) ;
#132687 = CARTESIAN_POINT ( 'NONE',  ( 1.739861462675455828, 2.010826045486389102, -0.1511602461454417123 ) ) ;
#132686 = CARTESIAN_POINT ( 'NONE',  ( 2.561320117580662803, -1.761587792986643475, 1.180070990429403555 ) ) ;
#132688 = CARTESIAN_POINT ( 'NONE',  ( 2.443383269832733795, -1.689004019812107460, 0.6554920229192174874 ) ) ;
#132689 = CARTESIAN_POINT ( 'NONE',  ( 6.339319342841494453, 9.553567112360518365, -1.199719254218452047 ) ) ;
#132690 = CARTESIAN_POINT ( 'NONE',  ( 6.543834100630380846, 0.8322713294773576020, -1.995267709627518427 ) ) ;
#132691 = ORIENTED_EDGE ( 'NONE', *, *, #16190, .F. ) ;
#132692 = CARTESIAN_POINT ( 'NONE',  ( 5.503720292143644777, 8.508425209887878538, 1.199719254218462483 ) ) ;
#132694 = CARTESIAN_POINT ( 'NONE',  ( 0.3564614995229599681, -1.804831555932787657, -0.6427613734035338977 ) ) ;
#132693 = CARTESIAN_POINT ( 'NONE',  ( -5.687809136132860210, 6.594531066031826150, -1.199719254218446718 ) ) ;
#132695 = CARTESIAN_POINT ( 'NONE',  ( 1.879585681373342698, 8.984805382992709255, 0.7750000000000004663 ) ) ;
#132696 = CARTESIAN_POINT ( 'NONE',  ( 1.579999999999989413, 6.280000000000042881, 2.500000000000000444 ) ) ;
#132697 =( BOUNDED_CURVE ( )  B_SPLINE_CURVE ( 2, ( #168400, #100198, #99150, #1598, #82875, #67659, #524 ),
 .UNSPECIFIED., .F., .T. ) 
 B_SPLINE_CURVE_WITH_KNOTS ( ( 3, 2, 2, 3 ),
 ( 0.1249999999999998612, 0.1309523809523809035, 0.1369047619047619735, 0.1428571428571429880 ),
 .UNSPECIFIED. ) 
 CURVE ( )  GEOMETRIC_REPRESENTATION_ITEM ( )  RATIONAL_B_SPLINE_CURVE ( ( 1.000000000000003109, 0.8660254037844355990, 1.000000000000000000, 0.8660254037844387076, 1.000000000000000000, 0.8660254037844355990, 1.000000000000003109 ) ) 
 REPRESENTATION_ITEM ( '' )  );
#132698 = CARTESIAN_POINT ( 'NONE',  ( 4.636525345749193505, 8.353103970108639587, 1.040834085586084257E-14 ) ) ;
#132699 = CARTESIAN_POINT ( 'NONE',  ( 1.364683531249986537, 0.1760416670080860446, 0.7879004041258500513 ) ) ;
#132700 = CARTESIAN_POINT ( 'NONE',  ( 2.901081683644312736, 6.328419697652925002, 0.7216878364870338292 ) ) ;
#132701 = CARTESIAN_POINT ( 'NONE',  ( -7.648771216403934758, 12.07531685244661723, -0.7998128361456291469 ) ) ;
#132702 = CARTESIAN_POINT ( 'NONE',  ( 4.487301133948972343, 1.932317252032596411, -0.9692046190768678349 ) ) ;
#132703 = CARTESIAN_POINT ( 'NONE',  ( -4.651856103264620401, 8.441266197201775512, 0.000000000000000000 ) ) ;
#132704 = CARTESIAN_POINT ( 'NONE',  ( 5.912764389335563919, 6.070849007079172743, -0.7216878364870458196 ) ) ;
#132705 = CARTESIAN_POINT ( 'NONE',  ( 2.303126745213024851, -0.3670769733005624369, -2.088442229865586697 ) ) ;
#132706 = CARTESIAN_POINT ( 'NONE',  ( 1.836970198721030181E-16, 0.000000000000000000, 1.500000000000000222 ) ) ;
#132707 = CARTESIAN_POINT ( 'NONE',  ( 3.268780567936521830, -1.820120084945201500, -0.7576984602858954920 ) ) ;
#132708 = CARTESIAN_POINT ( 'NONE',  ( 5.572493885891085519, 0.7809320506734825917, 1.745880147543739325 ) ) ;
#132709 = VERTEX_POINT ( 'NONE', #186160 ) ;
#132710 = DIRECTION ( 'NONE',  ( 0.000000000000000000, -1.000000000000000000, 0.000000000000000000 ) ) ;
#132711 = CARTESIAN_POINT ( 'NONE',  ( 6.320757381585181633, -1.393903556229304730, 1.391728847557841542 ) ) ;
#132712 = CARTESIAN_POINT ( 'NONE',  ( 1.253738886202176106, 0.7867099759248905588, 1.775636482627058088 ) ) ;
#132713 = EDGE_LOOP ( 'NONE', ( #152801, #149344, #28519, #132871 ) ) ;
#132714 = CARTESIAN_POINT ( 'NONE',  ( -5.334207092333882017, 5.187939460669764635, 0.7998128361456281477 ) ) ;
#132716 = CARTESIAN_POINT ( 'NONE',  ( -2.331034670843834533E-15, -7.868711954895448280, 9.183873791909961781 ) ) ;
#132715 = CARTESIAN_POINT ( 'NONE',  ( -6.780486220610184134, 9.003929572168926754, -1.443375672974066548 ) ) ;
#132717 = CARTESIAN_POINT ( 'NONE',  ( 6.337546739384100292, 9.481222731668410120, 1.199719254218460707 ) ) ;
#132719 = CARTESIAN_POINT ( 'NONE',  ( 5.275531169048895741, 7.248148678680751189, -1.443375672974078761 ) ) ;
#132718 = CARTESIAN_POINT ( 'NONE',  ( 6.551614543901692400, 8.666636272683888365, 1.599625672291281386 ) ) ;
#132721 = ORIENTED_EDGE ( 'NONE', *, *, #134279, .T. ) ;
#132720 = CARTESIAN_POINT ( 'NONE',  ( 6.147114339676178041, 0.1922309238813116328, 1.902605946959089689 ) ) ;
#132722 = CARTESIAN_POINT ( 'NONE',  ( 4.635508124736155366, -2.018492079602551392, 0.8926152185086615454 ) ) ;
#132723 = CARTESIAN_POINT ( 'NONE',  ( 2.186817281270125424, -2.164169025584137263, -0.4306803264119417607 ) ) ;
#132724 = CARTESIAN_POINT ( 'NONE',  ( -11.91826848676304529, 12.59166292761251782, 1.400000051402190637 ) ) ;
#132725 = CARTESIAN_POINT ( 'NONE',  ( 1.102048709075389654, -0.8591247869965330519, 1.708478583560539166 ) ) ;
#132726 = CIRCLE ( 'NONE', #39312, 0.07999999999999998779 ) ;
#132727 = CARTESIAN_POINT ( 'NONE',  ( -10.62873463776380056, 13.79999999999999893, -3.200000000000001510 ) ) ;
#132728 = CARTESIAN_POINT ( 'NONE',  ( 10.73535870392234237, 11.41900666419791399, 0.000000000000000000 ) ) ;
#132729 = CARTESIAN_POINT ( 'NONE',  ( 3.666520218671379006, -0.8364210039109070127, -1.894060025281426585 ) ) ;
#132730 = CARTESIAN_POINT ( 'NONE',  ( -5.063080299699540987, 7.994345218703034384, 1.199719254218464037 ) ) ;
#132731 = MECHANICAL_DESIGN_GEOMETRIC_PRESENTATION_REPRESENTATION (  '', ( #170729 ), #84300 ) ;
#132733 = CARTESIAN_POINT ( 'NONE',  ( 1.973706723050288936, 2.068691090354588091, -0.6273066937243013674 ) ) ;
#132732 = CARTESIAN_POINT ( 'NONE',  ( -4.952806187693842510, 4.672695395264567786, 0.7998128361456341429 ) ) ;
#132734 = CARTESIAN_POINT ( 'NONE',  ( 3.632539538618652752, 0.3231117836275976818, 2.167502126216628522 ) ) ;
#132735 = CARTESIAN_POINT ( 'NONE',  ( 4.923019175537949543, 4.916146257648610352, 0.000000000000000000 ) ) ;
#132736 = LINE ( 'NONE', #81820, #26828 ) ;
#132737 = EDGE_CURVE ( 'NONE', #12149, #103805, #113747, .T. ) ;
#132738 = CARTESIAN_POINT ( 'NONE',  ( -0.6823417656250003738, 14.21354166700806232, 1.181850606188754593 ) ) ;
#132739 = CARTESIAN_POINT ( 'NONE',  ( -3.654804927335652209, 6.421633627603656080, 1.199719254218452935 ) ) ;
#132740 = PRODUCT_DEFINITION_CONTEXT ( 'detailed design', #195850, 'design' ) ;
#132741 = CARTESIAN_POINT ( 'NONE',  ( 5.731065183167076249, 1.732634240323025043, 0.07581458514279926231 ) ) ;
#132742 = VECTOR ( 'NONE', #39044, 1000.000000000000000 ) ;
#132743 = CARTESIAN_POINT ( 'NONE',  ( -2.103486388414573138, 5.605817886458954291, 1.040834085586084257E-14 ) ) ;
#132744 = CARTESIAN_POINT ( 'NONE',  ( 4.082924941702062327, 1.964217522864346810, 0.6541895251909736198 ) ) ;
#132745 = CARTESIAN_POINT ( 'NONE',  ( 5.202788454032899246, 1.956619031766251737, 0.8093448757829673212 ) ) ;
#132746 = CARTESIAN_POINT ( 'NONE',  ( 6.124532705071213279, 8.168374127381657246, -1.599625672291262513 ) ) ;
#132747 = CARTESIAN_POINT ( 'NONE',  ( -1.364683531250010740, 5.280208333674758947, 0.7879004041258379498 ) ) ;
#132748 = CARTESIAN_POINT ( 'NONE',  ( 3.063290813078624719, 1.661244007368352982, 1.057527034793050547 ) ) ;
#132749 = CARTESIAN_POINT ( 'NONE',  ( 5.419995920891611085, 1.369053228189264670, -1.838397148955115412 ) ) ;
#132750 = CARTESIAN_POINT ( 'NONE',  ( 2.455445036260803349, 0.4872311372507812655, -1.759406031448563557 ) ) ;
#132751 = CARTESIAN_POINT ( 'NONE',  ( 3.067887898442204442, 6.801229324816399746, 0.7998128361456271485 ) ) ;
#132752 = CARTESIAN_POINT ( 'NONE',  ( 4.650083499362867911, 6.448183387388563226, 1.443375672974062551 ) ) ;
#132753 = CARTESIAN_POINT ( 'NONE',  ( -5.343885102080728977, 9.386283052402845328, 0.7998128361456481317 ) ) ;
#132754 = ORIENTED_EDGE ( 'NONE', *, *, #74123, .F. ) ;
#132755 = ORIENTED_EDGE ( 'NONE', *, *, #131699, .T. ) ;
#132756 = CARTESIAN_POINT ( 'NONE',  ( 3.621343358005862267, 1.728792273982106220, 1.031380397273339078 ) ) ;
#132757 = CARTESIAN_POINT ( 'NONE',  ( 3.942202469084721272, -0.9707516781715104237, 1.704694321266352786 ) ) ;
#132758 = CARTESIAN_POINT ( 'NONE',  ( -7.694415870955439551, 8.935572256658169010, 1.199719254218462483 ) ) ;
#132759 = CARTESIAN_POINT ( 'NONE',  ( -4.436542580169821726, 6.199052314996659874, 1.599625672291267398 ) ) ;
#132760 = CARTESIAN_POINT ( 'NONE',  ( 0.07556134207193675179, -0.004209888911949499594, -2.244269416743961187 ) ) ;
#132762 = CARTESIAN_POINT ( 'NONE',  ( 5.717594842608604289, -1.725906139129701478, 0.3911541089357990497 ) ) ;
#132761 = CARTESIAN_POINT ( 'NONE',  ( 0.1344724916707736029, 0.3614680779570299540, 2.059103226732065028 ) ) ;
#132763 = CARTESIAN_POINT ( 'NONE',  ( 10.99935770452674610, -5.294776013890325039, -0.1368885365587498570 ) ) ;
#132764 = CARTESIAN_POINT ( 'NONE',  ( 2.027518650255655253, -1.432890729411402830, -1.658174735819065049 ) ) ;
#132765 = CARTESIAN_POINT ( 'NONE',  ( 0.5908509756735094154, -0.6286620326499070543, 1.623129586062905805 ) ) ;
#132766 = CARTESIAN_POINT ( 'NONE',  ( 6.799577732453452761, 7.891594428405881878, -1.199719254218446718 ) ) ;
#132767 = CARTESIAN_POINT ( 'NONE',  ( 0.2333690889706682703, 0.003390530909083006028, -2.053566628440507635 ) ) ;
#132768 = CARTESIAN_POINT ( 'NONE',  ( 0.8907089605301542479, 1.523294409195220966, -0.8092020298176191284 ) ) ;
#132769 = CARTESIAN_POINT ( 'NONE',  ( 0.5975257653535933633, 1.179397575757964001, -1.972621981072789410 ) ) ;
#132770 = CARTESIAN_POINT ( 'NONE',  ( 0.9783777488623355278, -2.139296967303818686, -0.4750931833387496694 ) ) ;
#132771 = CARTESIAN_POINT ( 'NONE',  ( 3.457846583235091753, 0.5364296187198510646, -2.140574738106671759 ) ) ;
#132772 =( BOUNDED_SURFACE ( )  B_SPLINE_SURFACE ( 3, 2, ( 
 ( #169188, #136706, #104203 ),
 ( #137776, #170249, #203794 ),
 ( #117302, #53308, #19729 ),
 ( #55440, #20780, #17577 ),
 ( #199537, #202730, #21834 ),
 ( #87942, #85808, #34905 ) ),
 .UNSPECIFIED., .F., .F., .T. ) 
 B_SPLINE_SURFACE_WITH_KNOTS ( ( 4, 2, 4 ),
 ( 3, 3 ),
 ( 0.000000000000000000, 0.002122857551078453833, 0.004245715102156907665 ),
 ( 0.000000000000000000, 1.000000000000000000 ),
 .UNSPECIFIED. ) 
 GEOMETRIC_REPRESENTATION_ITEM ( )  RATIONAL_B_SPLINE_SURFACE ( (
 ( 1.000000000000000000, 0.7806433624857550546, 1.000000000000000000),
 ( 1.000000000000000000, 0.7860453980259737294, 1.000000000000000000),
 ( 1.000000000000000000, 0.7924770197564218188, 1.000000000000000000),
 ( 1.000000000000000000, 0.8094762427233131996, 1.000000000000000000),
 ( 1.000000000000000000, 0.8200718518785200528, 1.000000000000000000),
 ( 1.000000000000000000, 0.8343063410434338190, 1.000000000000000000) ) ) 
 REPRESENTATION_ITEM ( '' )  SURFACE ( )  );
#132773 = CARTESIAN_POINT ( 'NONE',  ( 1.464000922811282468, -0.5298712919106687291, 2.105275420227727956 ) ) ;
#132774 = DIRECTION ( 'NONE',  ( -0.000000000000000000, 1.000000000000000000, -0.000000000000000000 ) ) ;
#132775 = CARTESIAN_POINT ( 'NONE',  ( 1.780608593570524034, -0.5699985197749558585, -2.039088110117696750 ) ) ;
#132776 = CARTESIAN_POINT ( 'NONE',  ( 6.663994888585881959, -7.154544010627095219, -6.770610912236887380 ) ) ;
#132777 = CARTESIAN_POINT ( 'NONE',  ( 5.702155557734973179, -1.926566265495327723, 0.0002483051060025303638 ) ) ;
#132778 = ORIENTED_EDGE ( 'NONE', *, *, #91398, .F. ) ;
#132780 = CARTESIAN_POINT ( 'NONE',  ( 0.7499999999999920064, 5.483333333333353821, 1.299038105676669330 ) ) ;
#132779 = CARTESIAN_POINT ( 'NONE',  ( 2.595625714788946770, -0.7159257691751429453, 2.177794363412302481 ) ) ;
#132781 = CARTESIAN_POINT ( 'NONE',  ( 4.253507506385319381, 5.985511395581417204, 1.599625672291267398 ) ) ;
#132782 = CARTESIAN_POINT ( 'NONE',  ( 4.656335691289526402, 7.519809842224722374, -1.199719254218452047 ) ) ;
#132783 = CARTESIAN_POINT ( 'NONE',  ( 5.004621511133813705, -2.204373672735039147, -0.2730638322096557435 ) ) ;
#132784 = CARTESIAN_POINT ( 'NONE',  ( -6.399085315970132193, 10.40942393536641397, -0.7216878364870278340 ) ) ;
#132785 = CARTESIAN_POINT ( 'NONE',  ( -2.065456695249157981, 8.523797939977241001, -2.459872958007379928 ) ) ;
#132786 = CARTESIAN_POINT ( 'NONE',  ( 4.351804120306567825, 8.020929207092235558, 1.040834085586084257E-14 ) ) ;
#132787 = CARTESIAN_POINT ( 'NONE',  ( -8.690413276235355866, 10.20153224610512943, 1.082531754730558626 ) ) ;
#132788 = CIRCLE ( 'NONE', #122348, 0.1000000000000000333 ) ;
#132789 = CARTESIAN_POINT ( 'NONE',  ( 6.211043768836185031, 6.418841616496599123, 0.7216878364870328300 ) ) ;
#132790 = ORIENTED_EDGE ( 'NONE', *, *, #109534, .F. ) ;
#132791 = CARTESIAN_POINT ( 'NONE',  ( 2.637342451166882373, 0.6819965276749391236, 1.897697610567940174 ) ) ;
#132793 = CARTESIAN_POINT ( 'NONE',  ( 1.129816159781659390, 1.988900438959967376, -0.5462022044933153575 ) ) ;
#132792 = CARTESIAN_POINT ( 'NONE',  ( 7.721532178182734185, 8.967207948423393304, 1.199719254218462483 ) ) ;
#132794 = CARTESIAN_POINT ( 'NONE',  ( -1.420000000000001039, 6.200000000000045475, -2.579999999999995630 ) ) ;
#132795 = ADVANCED_FACE ( 'NONE', ( #125531 ), #141741, .T. ) ;
#132796 = CARTESIAN_POINT ( 'NONE',  ( 5.356880090730857802, 8.303424968277756335, 1.082531754730548412 ) ) ;
#132797 = CARTESIAN_POINT ( 'NONE',  ( -2.788906526875773208E-15, 8.718750000682796042, -1.499999999999998446 ) ) ;
#132798 = CARTESIAN_POINT ( 'NONE',  ( 1.364683531249988535, 3.863541667008087543, 0.7879004041258500513 ) ) ;
#132799 = CARTESIAN_POINT ( 'NONE',  ( 3.662233025353780480, -1.472007171213615351, 1.623636439255560227 ) ) ;
#132800 = CARTESIAN_POINT ( 'NONE',  ( 0.9674229098759130618, -1.967888300253183953, -0.4390273639364171698 ) ) ;
#132801 = CARTESIAN_POINT ( 'NONE',  ( 0.9250624443557056154, -1.167992581197497604, -1.423340509374780405 ) ) ;
#132802 = CARTESIAN_POINT ( 'NONE',  ( 5.091491514903929705, -0.8269519956315901643, 2.138199492833972482 ) ) ;
#132803 = CARTESIAN_POINT ( 'NONE',  ( 4.488128036367874607, -0.4058819498431766037, -1.795677737744493019 ) ) ;
#132804 = CARTESIAN_POINT ( 'NONE',  ( 6.747154001095143627, 11.02343010125301959, -0.7998128361456291469 ) ) ;
#132805 = PRESENTATION_STYLE_ASSIGNMENT (( #592 ) ) ;
#132806 = CARTESIAN_POINT ( 'NONE',  ( 5.543921259432438298, 0.7380120197021734496, -1.669944898041133552 ) ) ;
#132807 = CARTESIAN_POINT ( 'NONE',  ( 6.399064592084179992, -0.9530083391863402031, -1.777013033299412292 ) ) ;
#132808 = CARTESIAN_POINT ( 'NONE',  ( -8.799405390469187793, 10.22472669609091689, -1.199719254218446718 ) ) ;
#132810 = CARTESIAN_POINT ( 'NONE',  ( -5.257529707049291900, 9.355811434857983500, 0.7998128361456291469 ) ) ;
#132809 = CARTESIAN_POINT ( 'NONE',  ( 5.014671263542332724, 1.563880152264264245, -1.635232377595864595 ) ) ;
#132811 = CARTESIAN_POINT ( 'NONE',  ( 6.616252143301227129, -0.9890948110137095517, -1.859226117534703571 ) ) ;
#132812 = CARTESIAN_POINT ( 'NONE',  ( 2.847613298335896675E-16, 4.500000000000002665, -1.600000000000005196 ) ) ;
#132813 = CARTESIAN_POINT ( 'NONE',  ( 4.615722581382986967, 0.4567890626981512270, -2.019179087418949692 ) ) ;
#132814 = CARTESIAN_POINT ( 'NONE',  ( 7.540305987494599016, 11.94877408538573427, -0.7998128361456291469 ) ) ;
#132815 = CARTESIAN_POINT ( 'NONE',  ( -3.096765176264313357, 6.450054161018508481, 0.6354748981389554130 ) ) ;
#132816 = B_SPLINE_CURVE_WITH_KNOTS ( 'NONE', 3,
 ( #192792, #100370, #128963, #127915 ),
 .UNSPECIFIED., .F., .F.,
 ( 4, 4 ),
 ( 0.000000000000000000, 0.0004037790303856251119 ),
 .UNSPECIFIED. ) ;
#132817 = APPLICATION_PROTOCOL_DEFINITION ( 'draft international standard', 'automotive_design', 1998, #115578 ) ;
#132819 = CARTESIAN_POINT ( 'NONE',  ( 2.578635874325632127, -1.843646926959886523, -0.5589146710999506329 ) ) ;
#132818 = CARTESIAN_POINT ( 'NONE',  ( -7.666245793523398078, 11.03137162816423356, 1.199719254218453823 ) ) ;
#132820 = CARTESIAN_POINT ( 'NONE',  ( 0.1861310709357004711, 6.361154168393027497, 3.114872224523889344 ) ) ;
#132821 = CARTESIAN_POINT ( 'NONE',  ( 4.434925645001613681, 5.307073019657559065, -1.082531754730548412 ) ) ;
#132822 = CARTESIAN_POINT ( 'NONE',  ( 5.343583877570073248, 6.330574952785890552, -1.095086179472234189 ) ) ;
#132823 = CARTESIAN_POINT ( 'NONE',  ( -4.627410500965859264, 4.293067094081919777, 0.7998128361456341429 ) ) ;
#132825 = CARTESIAN_POINT ( 'NONE',  ( 1.389269710167878369, -2.111442789942123088, -0.6905784607170639688 ) ) ;
#132824 = CARTESIAN_POINT ( 'NONE',  ( 1.037531286769650452, -0.04638328994046451298, 2.120250110247793085 ) ) ;
#132826 = CARTESIAN_POINT ( 'NONE',  ( 3.311648941680225722, -0.4124737740866398217, 2.064988983437756165 ) ) ;
#132827 = CARTESIAN_POINT ( 'NONE',  ( -7.611976899429754084, 7.845337568948314022, 0.7998128361456341429 ) ) ;
#132828 = CARTESIAN_POINT ( 'NONE',  ( 5.601490020740366838, 9.686822124172440596, 1.040834085586084257E-14 ) ) ;
#132829 = CARTESIAN_POINT ( 'NONE',  ( 3.543363863352413823, 1.774678991803163575, -0.8365776047038612218 ) ) ;
#132830 = CARTESIAN_POINT ( 'NONE',  ( 5.148345644887269756, 7.029489223833707001, -1.599625672291256295 ) ) ;
#132831 = CARTESIAN_POINT ( 'NONE',  ( -4.022774286133019572, 7.614368594009178537, 0.1926593524083572428 ) ) ;
#132832 = CARTESIAN_POINT ( 'NONE',  ( 4.202137545231717120, 6.989912005157271402, 1.199719254218462483 ) ) ;
#132833 = CARTESIAN_POINT ( 'NONE',  ( -5.804299160426237059, 7.865044668620976509, -1.443375672974066548 ) ) ;
#132834 = CARTESIAN_POINT ( 'NONE',  ( -7.917598520700757980, 9.299915031314755609, 1.082531754730558626 ) ) ;
#132835 = CARTESIAN_POINT ( 'NONE',  ( 2.162495577681341707, 2.120227376586072854, 0.04728746717985036346 ) ) ;
#132836 = CARTESIAN_POINT ( 'NONE',  ( -6.635789839245807897, 6.706452665400368218, 0.7998128361456341429 ) ) ;
#132837 = CARTESIAN_POINT ( 'NONE',  ( 4.668382477721988444, -0.8370036265390871089, -1.774476930476886594 ) ) ;
#132838 = CARTESIAN_POINT ( 'NONE',  ( 2.729541802387557059, -2.017400560480298033, 0.7770373237434913261 ) ) ;
#132839 = CARTESIAN_POINT ( 'NONE',  ( 3.315785976855676775, 1.165629053876730659, -1.425327459889616399 ) ) ;
#132840 = CARTESIAN_POINT ( 'NONE',  ( -4.022774286133019572, 7.614368594009178537, 0.1926593524083572428 ) ) ;
#132841 = CARTESIAN_POINT ( 'NONE',  ( 1.364683531249988757, -0.8031249996585804185, 0.000000000000000000 ) ) ;
#132842 = CARTESIAN_POINT ( 'NONE',  ( 4.329842768969596634, 1.707365525456190358, 0.3361313568818121156 ) ) ;
#132843 = CARTESIAN_POINT ( 'NONE',  ( 1.050790385994986309, 16.00000000000000711, -12.64745918785790835 ) ) ;
#132844 = CARTESIAN_POINT ( 'NONE',  ( 3.199361063144961825, 6.676412307070352270, -0.7216878364870267237 ) ) ;
#132845 = CARTESIAN_POINT ( 'NONE',  ( -11.21412923722849619, 8.995494058042485364, 2.499828665724475485 ) ) ;
#132846 = CARTESIAN_POINT ( 'NONE',  ( 1.727627455807039691, -2.035446057602477321, 0.7283451284763039490 ) ) ;
#132847 = CARTESIAN_POINT ( 'NONE',  ( 3.989611116449209405, 1.913510565032714883, 0.6351021849077125303 ) ) ;
#132848 = CARTESIAN_POINT ( 'NONE',  ( -8.785320351530977234, 13.19336481018743079, 1.040834085586084257E-14 ) ) ;
#132849 = CARTESIAN_POINT ( 'NONE',  ( 1.657319961134783748, -1.854130675604428902, -1.111159678259740602 ) ) ;
#132850 = CARTESIAN_POINT ( 'NONE',  ( 2.957844615808038480, 1.962099266425470390, -0.1918489139557562340 ) ) ;
#132851 = CARTESIAN_POINT ( 'NONE',  ( 6.509000000000014552, 2.959959533984284352, 2.552917358632576850 ) ) ;
#132852 = CARTESIAN_POINT ( 'NONE',  ( 3.315898775378321339, 1.229719374647167296, -1.503149361444736876 ) ) ;
#132855 = ORIENTED_EDGE ( 'NONE', *, *, #107143, .F. ) ;
#132854 = CARTESIAN_POINT ( 'NONE',  ( -3.363831509966363598, 5.978201624052440266, -1.082531754730548412 ) ) ;
#132853 = CARTESIAN_POINT ( 'NONE',  ( -10.29027540264791440, 11.10766884595181203, 0.7216878364870438212 ) ) ;
#132856 = CARTESIAN_POINT ( 'NONE',  ( -5.610041701004606196, 9.767075427805856691, -0.7998128361456362523 ) ) ;
#132857 = CARTESIAN_POINT ( 'NONE',  ( 5.086243903782109221, 5.962981304947771122, -1.199719254218452047 ) ) ;
#132859 = ORIENTED_EDGE ( 'NONE', *, *, #57116, .T. ) ;
#132858 = CARTESIAN_POINT ( 'NONE',  ( -6.656127069666307072, 6.730179434224282886, 0.7998128361456341429 ) ) ;
#132860 = CARTESIAN_POINT ( 'NONE',  ( -7.795575137733361970, 12.03866206075687018, 0.7216878364870458196 ) ) ;
#132861 = CARTESIAN_POINT ( 'NONE',  ( 0.6927435329204565395, -2.190372518412486702, -0.2681103625320201411 ) ) ;
#132862 = CARTESIAN_POINT ( 'NONE',  ( 1.001543065824772753E-15, -3.171874999522042327, 3.793834371823811669 ) ) ;
#132863 = CARTESIAN_POINT ( 'NONE',  ( 5.014483083204026137, 0.7471541359172824137, 1.814103259000845458 ) ) ;
#132864 = CARTESIAN_POINT ( 'NONE',  ( 2.496720397819631732, -1.994071314890283553, 0.2986276487200872354 ) ) ;
#132865 = ORIENTED_EDGE ( 'NONE', *, *, #59183, .T. ) ;
#132866 = CARTESIAN_POINT ( 'NONE',  ( 3.046228577489984879, 0.9562745863303960814, 1.889201325992972080 ) ) ;
#132867 = CARTESIAN_POINT ( 'NONE',  ( 1.499999999999987121, 2.327083334016154303, -0.8660254037844262731 ) ) ;
#132869 = CARTESIAN_POINT ( 'NONE',  ( -6.403528624356093601, 6.365204904703887223, 1.040834085586084257E-14 ) ) ;
#132868 = CARTESIAN_POINT ( 'NONE',  ( 4.786522169170392971, 5.141580351323885800, 0.8077998227834035649 ) ) ;
#132870 = CARTESIAN_POINT ( 'NONE',  ( 3.925598083870453614, 0.9833751987384667936, -1.556331266066004027 ) ) ;
#132871 = ORIENTED_EDGE ( 'NONE', *, *, #123262, .F. ) ;
#132872 = UNCERTAINTY_MEASURE_WITH_UNIT (LENGTH_MEASURE( 1.000000000000000082E-05 ), #140026, 'distance_accuracy_value', 'NONE');
#132873 = CARTESIAN_POINT ( 'NONE',  ( -7.808606406466886973, 11.19745900993164511, 1.199719254218453823 ) ) ;
#132874 = FACE_OUTER_BOUND ( 'NONE', #147528, .T. ) ;
#132876 = EDGE_CURVE ( 'NONE', #190431, #137219, #149742, .T. ) ;
#132875 = CARTESIAN_POINT ( 'NONE',  ( 5.695592476053609410, 1.958610405324921588, -0.8133567297157192622 ) ) ;
#132877 = DIRECTION ( 'NONE',  ( -1.000000000000000000, 0.000000000000000000, 0.000000000000000000 ) ) ;
#132878 = CARTESIAN_POINT ( 'NONE',  ( 5.126954644262057492, 9.133197518281081173, 0.7998128361456462443 ) ) ;
#132879 = CARTESIAN_POINT ( 'NONE',  ( 5.343066995996487378, -1.769704953023493399, 1.055641863377870138 ) ) ;
#132882 = CARTESIAN_POINT ( 'NONE',  ( 1.962219809069129184, -1.683971100191889336, -0.7449956418128443891 ) ) ;
#132881 = CARTESIAN_POINT ( 'NONE',  ( 0.4845113730182957767, 1.779151863920569232, 0.5459849130424464514 ) ) ;
#132880 = CARTESIAN_POINT ( 'NONE',  ( 10.50000000000000000, 12.59290055818100562, 3.599999999999996536 ) ) ;
#132883 = CARTESIAN_POINT ( 'NONE',  ( 8.633844893804129228, 8.967240552393299424, -0.7998128361456211532 ) ) ;
#132884 = CARTESIAN_POINT ( 'NONE',  ( 0.9399888277777949108, 7.435091042679344397, 4.383624543540939555 ) ) ;
#132885 = DIRECTION ( 'NONE',  ( 0.7592566023652995710, -0.6507913734559652719, 0.000000000000000000 ) ) ;
#132886 = CARTESIAN_POINT ( 'NONE',  ( 1.700138637298425737, -0.7412910010123253679, 2.078789392164873906 ) ) ;
#132887 = CARTESIAN_POINT ( 'NONE',  ( 5.360715614582075794, -1.643942929158914268, 1.554587190974612732 ) ) ;
#132888 = CARTESIAN_POINT ( 'NONE',  ( -6.561783159334130922, 9.638868871656395498, -1.082531754730538864 ) ) ;
#132889 = CARTESIAN_POINT ( 'NONE',  ( 4.904484127313208042, -1.798792703336571375, -0.2141664767603863595 ) ) ;
#132890 = CARTESIAN_POINT ( 'NONE',  ( 4.979654327277899917, -0.6834858053395581612, 1.789849564252174119 ) ) ;
#132891 = CYLINDRICAL_SURFACE ( 'NONE', #171914, 0.08000000000000020983 ) ;
#132892 = CARTESIAN_POINT ( 'NONE',  ( 4.838664814796108438, 0.3202261158844340594, 1.842872994462002367 ) ) ;
#132893 = CARTESIAN_POINT ( 'NONE',  ( 5.213276571848306951, -1.572085989900060765, -0.9957144527335654027 ) ) ;
#132894 = CARTESIAN_POINT ( 'NONE',  ( -1.364683531250010295, 5.030208333674757171, 0.7879004041258379498 ) ) ;
#132895 = CARTESIAN_POINT ( 'NONE',  ( 6.368005316177769437, 0.9137572655052300652, 1.515547905889617519 ) ) ;
#132896 = CARTESIAN_POINT ( 'NONE',  ( 0.6730650033222317363, 1.776164188848127878, -0.9548607967814757291 ) ) ;
#132898 = CARTESIAN_POINT ( 'NONE',  ( 2.332770561069871462, 2.043027141408111813, 0.5109185277013729154 ) ) ;
#132897 = CARTESIAN_POINT ( 'NONE',  ( -3.267151830768959098, 4.834763107362302748, -1.443375672974058777 ) ) ;
#132899 = CARTESIAN_POINT ( 'NONE',  ( 8.238550898598388628, 12.76339314834017102, 0.7998128361456462443 ) ) ;
#132901 = CARTESIAN_POINT ( 'NONE',  ( -8.859363311525973117, 12.42334206583395328, -1.199719254218446718 ) ) ;
#132900 = CARTESIAN_POINT ( 'NONE',  ( 1.499999999999822586, 7.268077025657071033, 4.207854987878929975 ) ) ;
#132902 = SURFACE_STYLE_FILL_AREA ( #50552 ) ;
#132903 = CARTESIAN_POINT ( 'NONE',  ( 1.547134890100225535, 0.2020692043026971751, 2.009678023649637879 ) ) ;
#132904 = CARTESIAN_POINT ( 'NONE',  ( -1.364683531250000748, 2.259375000341422357, 1.214306433183764966E-14 ) ) ;
#132905 = CARTESIAN_POINT ( 'NONE',  ( 6.720655732516650716, 1.307757891114844417, 1.844004982043083940 ) ) ;
#132906 = CARTESIAN_POINT ( 'NONE',  ( 4.684505768721569652, 5.424010470718658716, -1.199719254218452047 ) ) ;
#132907 = ORIENTED_EDGE ( 'NONE', *, *, #153405, .F. ) ;
#132908 = CARTESIAN_POINT ( 'NONE',  ( 1.950665695202157046, 0.6760947502928333908, 2.053231632317173538 ) ) ;
#132909 = CARTESIAN_POINT ( 'NONE',  ( 6.610000000000002096, 6.034162285353575683, 2.874900418788868262 ) ) ;
#132912 = CARTESIAN_POINT ( 'NONE',  ( 2.796816994357219865, 2.968434822912331850, -2.452793345967703154 ) ) ;
#132911 = CARTESIAN_POINT ( 'NONE',  ( -3.028993686180011746, 2.741750000184231428, -2.499999999999996003 ) ) ;
#132910 = CARTESIAN_POINT ( 'NONE',  ( 4.923546060418115822, 5.773167154356443120, -1.199719254218452047 ) ) ;
#132913 = CARTESIAN_POINT ( 'NONE',  ( 8.961576348508637935, 11.47825837805867799, -1.443375672974052559 ) ) ;
#132914 = CARTESIAN_POINT ( 'NONE',  ( -8.103009739377982967, -6.893137084989842123, 7.439168848974024861 ) ) ;
#132915 = CARTESIAN_POINT ( 'NONE',  ( -6.887178846062116833, 9.058127958537705027, -1.443375672974059665 ) ) ;
#132916 = CARTESIAN_POINT ( 'NONE',  ( 0.8553300576445364012, 0.4222666777726029608, -2.150330908352434012 ) ) ;
#132917 = CARTESIAN_POINT ( 'NONE',  ( 0.3421332810201426211, 7.155223633118597881, 1.971148363701352269 ) ) ;
#132918 = CARTESIAN_POINT ( 'NONE',  ( 1.868429791336771340, 1.163878172895687069, 1.940057763798187951 ) ) ;
#132919 = CARTESIAN_POINT ( 'NONE',  ( -8.158255747121117452, 10.54105100977322174, 1.599625672291295375 ) ) ;
#132920 = CARTESIAN_POINT ( 'NONE',  ( -4.622967192135580383, 5.456178481322002227, 1.082531754730558626 ) ) ;
#132921 = CARTESIAN_POINT ( 'NONE',  ( -1.201851678989727383E-14, 3.884375000341423689, 1.575800808251672791 ) ) ;
#132922 = CARTESIAN_POINT ( 'NONE',  ( 4.629651883607522223, 8.329987488807731211, -0.3686744245932921937 ) ) ;
#132923 = CARTESIAN_POINT ( 'NONE',  ( 0.7500000000000006661, 10.83333333333333393, 1.299038105676657340 ) ) ;
#132924 = CARTESIAN_POINT ( 'NONE',  ( 5.076602173674213070, 4.887400388900169368, 0.000000000000000000 ) ) ;
#132925 = CARTESIAN_POINT ( 'NONE',  ( 3.479546766767865673, 1.120508650343427171, 1.369845563140754230 ) ) ;
#132926 = CARTESIAN_POINT ( 'NONE',  ( 8.778014389843965759, 12.32843499053828928, 1.199719254218450271 ) ) ;
#132927 = CARTESIAN_POINT ( 'NONE',  ( 0.08314155087942810829, -0.1569203414564980525, -2.071771216027401774 ) ) ;
#132928 = CARTESIAN_POINT ( 'NONE',  ( 1.364683531249997417, 15.04687500034139447, 2.602085213965210642E-15 ) ) ;
#132929 = ORIENTED_EDGE ( 'NONE', *, *, #185077, .T. ) ;
#132930 = CARTESIAN_POINT ( 'NONE',  ( -5.586841817283045408, 8.675676665875643678, 1.199719254218454489 ) ) ;
#132931 = CARTESIAN_POINT ( 'NONE',  ( 5.694935465533643715, 1.779635825068434984, 0.9480254120717497290 ) ) ;
#132932 = ORIENTED_EDGE ( 'NONE', *, *, #13361, .T. ) ;
#132933 = CARTESIAN_POINT ( 'NONE',  ( 2.623731232481395725, -1.075365945362505293, -1.530472918023266571 ) ) ;
#132934 = CARTESIAN_POINT ( 'NONE',  ( 2.483334644719074724, -0.004358110040847408898, 2.070434559716929357 ) ) ;
#132935 = AXIS2_PLACEMENT_3D ( 'NONE', #28086, #44353, #62705 ) ;
#132936 = CARTESIAN_POINT ( 'NONE',  ( -6.034787771414192648, 9.094317262408276648, 1.082531754730549967 ) ) ;
#132937 = CARTESIAN_POINT ( 'NONE',  ( 2.285291272251275707, 0.09004542135446562401, -1.910373438827176251 ) ) ;
#132938 = PLANE ( 'NONE',  #1639 ) ;
#132939 = DIRECTION ( 'NONE',  ( -3.491481338843133750E-15, -0.000000000000000000, -1.000000000000000000 ) ) ;
#132940 = CARTESIAN_POINT ( 'NONE',  ( -6.773846765317318663, -7.246166700180828535, 6.773846765317342644 ) ) ;
#132941 = CIRCLE ( 'NONE', #122666, 0.07999999999999946043 ) ;
#132942 = CARTESIAN_POINT ( 'NONE',  ( 1.364683531249990311, 3.946875000341417028, 1.214306433183764966E-14 ) ) ;
#132943 = CARTESIAN_POINT ( 'NONE',  ( 0.2461629937395051482, 0.9812432698282258503, -1.641294572782559635 ) ) ;
#132944 = B_SPLINE_CURVE_WITH_KNOTS ( 'NONE', 3,
 ( #13456, #178112, #194347, #212714 ),
 .UNSPECIFIED., .F., .F.,
 ( 4, 4 ),
 ( 8.673617379883660879E-19, 0.0006776115001627299730 ),
 .UNSPECIFIED. ) ;
#132945 = CARTESIAN_POINT ( 'NONE',  ( 5.207740401424913124, 9.089797878388800711, -0.7216878364870458196 ) ) ;
#132946 = CARTESIAN_POINT ( 'NONE',  ( 2.453501617077270769, 1.514643136537169310, 1.246875331876770243 ) ) ;
#132947 = CARTESIAN_POINT ( 'NONE',  ( -3.189213936345670852, 2.817530495244580102, -2.450448857954567572 ) ) ;
#132948 = CARTESIAN_POINT ( 'NONE',  ( -4.122561227007127016, 6.967349310553715647, 1.199719254218452935 ) ) ;
#132949 = CARTESIAN_POINT ( 'NONE',  ( 5.660427296577901224, 2.118236611397011249, 0.1021076702828054988 ) ) ;
#132951 = CARTESIAN_POINT ( 'NONE',  ( -2.279673327426058105, 5.603443282065057929, -0.02210016498917465738 ) ) ;
#132950 = CARTESIAN_POINT ( 'NONE',  ( 8.075853055234393452, 12.57357899774884658, 0.7998128361456462443 ) ) ;
#132952 =( BOUNDED_SURFACE ( )  B_SPLINE_SURFACE ( 3, 2, ( 
 ( #12871, #180722, #152497 ),
 ( #66939, #68008, #182851 ),
 ( #4080, #34470, #134148 ),
 ( #132020, #99483, #135203 ),
 ( #51810, #183922, #35534 ),
 ( #101610, #133081, #50725 ) ),
 .UNSPECIFIED., .F., .F., .F. ) 
 B_SPLINE_SURFACE_WITH_KNOTS ( ( 4, 2, 4 ),
 ( 3, 3 ),
 ( 0.000000000000000000, 0.0003754691837024765901, 0.0007509383674049531802 ),
 ( 0.000000000000000000, 1.000000000000000000 ),
 .UNSPECIFIED. ) 
 GEOMETRIC_REPRESENTATION_ITEM ( )  RATIONAL_B_SPLINE_SURFACE ( (
 ( 1.000000000000000000, 0.6711954675835484219, 1.000000000000000000),
 ( 1.000000000000000000, 0.6709646295267468474, 1.000000000000000000),
 ( 1.000000000000000000, 0.6771840716659200954, 1.000000000000000000),
 ( 1.000000000000000000, 0.6927481755867312962, 1.000000000000000000),
 ( 1.000000000000000000, 0.7017972101310004929, 1.000000000000000000),
 ( 1.000000000000000000, 0.7071067811865475727, 1.000000000000000000) ) ) 
 REPRESENTATION_ITEM ( '' )  SURFACE ( )  );
#132953 = CARTESIAN_POINT ( 'NONE',  ( 0.1923495491853322581, -0.4021996241703913455, -1.833441224692602844 ) ) ;
#132954 = CARTESIAN_POINT ( 'NONE',  ( -1.364683531249997417, 3.009375000341422801, 1.214306433183764966E-14 ) ) ;
#132955 = CARTESIAN_POINT ( 'NONE',  ( 2.355728993131640525, -1.494696414742059387, -1.348868867694212881 ) ) ;
#132957 = CARTESIAN_POINT ( 'NONE',  ( 1.054496592829538004, -1.339774933521440392, 1.639435421165438500 ) ) ;
#132956 = CARTESIAN_POINT ( 'NONE',  ( -5.721177635286839092, 9.618531641235897212, 0.7216878364870458196 ) ) ;
#132958 = CARTESIAN_POINT ( 'NONE',  ( 10.39592987943500724, 9.162555348756470153, 6.046252475528372194 ) ) ;
#132959 = CARTESIAN_POINT ( 'NONE',  ( 2.453653613718423276, 1.598880132357576755, 1.315258840600006085 ) ) ;
#132960 = CARTESIAN_POINT ( 'NONE',  ( 3.932747076415766596, 6.745899468197171345, 1.199719254218451159 ) ) ;
#132961 = CARTESIAN_POINT ( 'NONE',  ( 3.386504508363381571, 7.172948703057747011, -0.7998128361456362523 ) ) ;
#132962 = ORIENTED_EDGE ( 'NONE', *, *, #143867, .T. ) ;
#132964 = CARTESIAN_POINT ( 'NONE',  ( 5.190073875932979419, 4.949507698210251938, 0.7998128361456341429 ) ) ;
#132963 = CARTESIAN_POINT ( 'NONE',  ( 6.070280604649140876, -1.984772539198733865, -0.6570628365835521345 ) ) ;
#132967 = VERTEX_POINT ( 'NONE', #141232 ) ;
#132966 = CARTESIAN_POINT ( 'NONE',  ( 2.402729293200474459, -0.3110027565414590356, -1.784399550462684392 ) ) ;
#132965 = CARTESIAN_POINT ( 'NONE',  ( 3.821172736587064023, -0.1348131347885111742, 1.820669774636254346 ) ) ;
#132968 = CARTESIAN_POINT ( 'NONE',  ( 8.215351014876830504, 11.67199438640995801, -1.199719254218446718 ) ) ;
#132969 = SURFACE_STYLE_USAGE ( .BOTH. , #179562 ) ;
#132970 = CARTESIAN_POINT ( 'NONE',  ( 11.15299978643949252, 7.622798436847911141, 0.8142573934770976907 ) ) ;
#132971 = CARTESIAN_POINT ( 'NONE',  ( 5.385833121705805304, 1.478444731487274622, 1.638484004604986000 ) ) ;
#132972 = CARTESIAN_POINT ( 'NONE',  ( -1.364683531250000748, 11.17187500034139802, 0.000000000000000000 ) ) ;
#132973 = VERTEX_POINT ( 'NONE', #193130 ) ;
#132974 = CARTESIAN_POINT ( 'NONE',  ( 3.721269560815092525, 1.641568950759502377, 0.9805937191851579193 ) ) ;
#132975 = CARTESIAN_POINT ( 'NONE',  ( -8.272446282632566650, 12.80293776304669962, 0.7998128361456481317 ) ) ;
#132976 = CARTESIAN_POINT ( 'NONE',  ( 5.960781091502512119, 10.10599504006161986, 0.7998128361456462443 ) ) ;
#132977 = CARTESIAN_POINT ( 'NONE',  ( -0.6801582343750265380, 1.463541667008072533, 1.178068619123799898 ) ) ;
#132978 = CARTESIAN_POINT ( 'NONE',  ( 5.626270559546826533, 5.666329862333828515, 0.7216878364870317197 ) ) ;
#132979 = DIRECTION ( 'NONE',  ( 0.000000000000000000, 1.000000000000000000, 0.000000000000000000 ) ) ;
#132981 = EDGE_CURVE ( 'NONE', #139750, #157226, #49583, .T. ) ;
#132980 = CARTESIAN_POINT ( 'NONE',  ( 7.884034871045744630, 14.36475460829932516, -9.047442571381882459 ) ) ;
#132982 = CARTESIAN_POINT ( 'NONE',  ( 0.4855842612344652975, -1.827229208960782447, -0.2260576252584786672 ) ) ;
#132983 =( NAMED_UNIT ( * ) SI_UNIT ( $, .STERADIAN. ) SOLID_ANGLE_UNIT ( ) );
#132984 = ADVANCED_FACE ( 'NONE', ( #158508 ), #167264, .T. ) ;
#132985 = CARTESIAN_POINT ( 'NONE',  ( 4.622238261848357510, 1.152259890254858421, -1.473394524551619789 ) ) ;
#132986 = CARTESIAN_POINT ( 'NONE',  ( 7.075376061485196821, 9.347967719856493218, 1.599625672291268286 ) ) ;
#132987 = CARTESIAN_POINT ( 'NONE',  ( -11.06298660227979802, 13.75680399625266759, -0.9087478855431304625 ) ) ;
#132989 = CARTESIAN_POINT ( 'NONE',  ( -7.863365906246074566, 8.276274433482971205, -0.7216878364870278340 ) ) ;
#132988 = AXIS2_PLACEMENT_3D ( 'NONE', #202602, #171194, #21708 ) ;
#132990 = CARTESIAN_POINT ( 'NONE',  ( 3.649115900372475796, 7.409052317076538330, 1.040834085586084257E-14 ) ) ;
#132991 = CARTESIAN_POINT ( 'NONE',  ( 1.744903480705553012, -0.2836847097360816194, -1.948756091721944861 ) ) ;
#132992 = CARTESIAN_POINT ( 'NONE',  ( 2.653922917551009952, 1.081085551080329443, 1.701936510390424928 ) ) ;
#132993 = CARTESIAN_POINT ( 'NONE',  ( -8.158255747121117452, 10.54105100977322174, 1.599625672291295375 ) ) ;
#132994 = CARTESIAN_POINT ( 'NONE',  ( 5.559725510055676168, 8.644040974110419384, 1.199719254218451159 ) ) ;
#132995 = PRESENTATION_STYLE_ASSIGNMENT (( #165455 ) ) ;
#132996 = CARTESIAN_POINT ( 'NONE',  ( 2.853686581259745836, 2.180823047698337902, -0.2155538573413370296 ) ) ;
#132997 = CARTESIAN_POINT ( 'NONE',  ( 6.604126001430527637, -1.825160783932573860, 0.05055279568313279792 ) ) ;
#132998 = CARTESIAN_POINT ( 'NONE',  ( -3.327636637150278798, 5.969660945728899826, -1.199719254218452935 ) ) ;
#132999 = DIRECTION ( 'NONE',  ( 0.000000000000000000, 0.000000000000000000, -1.000000000000000000 ) ) ;
#133000 = DIRECTION ( 'NONE',  ( 0.000000000000000000, 0.000000000000000000, 1.000000000000000000 ) ) ;
#133002 = EDGE_CURVE ( 'NONE', #66184, #132154, #61885, .T. ) ;
#133001 = AXIS2_PLACEMENT_3D ( 'NONE', #69291, #135402, #201425 ) ;
#133003 = CARTESIAN_POINT ( 'NONE',  ( 5.722950238744211937, 5.849399164722627553, 0.7216878364870328300 ) ) ;
#133004 = CARTESIAN_POINT ( 'NONE',  ( 9.759171643738394408, 10.28012176064996197, 0.000000000000000000 ) ) ;
#133005 = CARTESIAN_POINT ( 'NONE',  ( 3.005103603723342953, 6.657704637652544832, -0.7998128361456291469 ) ) ;
#133006 = CARTESIAN_POINT ( 'NONE',  ( 6.617788377246179188, 8.814115421577600529, -1.443375672974078761 ) ) ;
#133007 = ORIENTED_EDGE ( 'NONE', *, *, #172864, .T. ) ;
#133009 = CARTESIAN_POINT ( 'NONE',  ( 1.225244855396601551, 1.776329837998322780, 0.9471711224926461226 ) ) ;
#133008 = CARTESIAN_POINT ( 'NONE',  ( 3.913478945735289205, -0.9499487412085620974, -1.577145280185827447 ) ) ;
#133010 = CARTESIAN_POINT ( 'NONE',  ( 3.023178501820302344, 2.287506772329782390, -0.2231754551033394429 ) ) ;
#133012 = CARTESIAN_POINT ( 'NONE',  ( 0.6900174830311635032, 0.9632304765912635958, -1.592144255797292463 ) ) ;
#133011 = CARTESIAN_POINT ( 'NONE',  ( 2.250290310188348464, 5.569163095287620990, 0.7216878364870438212 ) ) ;
#133013 = CARTESIAN_POINT ( 'NONE',  ( 3.475000000000000533, -0.1750000000000015432, 0.000000000000000000 ) ) ;
#133014 = CARTESIAN_POINT ( 'NONE',  ( -2.591579918506545344, 6.175260338232929413, 1.040834085586084257E-14 ) ) ;
#133015 = CYLINDRICAL_SURFACE ( 'NONE', #81495, 1.500000000000000222 ) ;
#133016 = CARTESIAN_POINT ( 'NONE',  ( 4.851772015791367743, -1.356534033432246211, -1.348250844427544282 ) ) ;
#133017 = CARTESIAN_POINT ( 'NONE',  ( -7.309817376062285099, 11.67987070538135264, 0.000000000000000000 ) ) ;
#133018 = CARTESIAN_POINT ( 'NONE',  ( -4.977251789992602760, 8.820894498384422633, 0.000000000000000000 ) ) ;
#133020 = CARTESIAN_POINT ( 'NONE',  ( 2.166681600665042229, -1.709288833360942617, -0.7604731621856930524 ) ) ;
#133019 = CARTESIAN_POINT ( 'NONE',  ( 3.948837864290375421, -1.739349124335771712, -1.159800787976144720 ) ) ;
#133021 = CARTESIAN_POINT ( 'NONE',  ( 5.829642864196151741, 9.745074408296771296, 0.7216878364870438212 ) ) ;
#133022 = CARTESIAN_POINT ( 'NONE',  ( -1.364683531249997417, 5.071875000341417916, 1.214306433183764966E-14 ) ) ;
#133023 = CARTESIAN_POINT ( 'NONE',  ( 5.882333747326812023, -0.2767177626767613474, -1.820229446528654371 ) ) ;
#133024 = CARTESIAN_POINT ( 'NONE',  ( 2.347533153460546806, 5.890539112345938300, 0.000000000000000000 ) ) ;
#133025 = CARTESIAN_POINT ( 'NONE',  ( 5.908755808680682620, 6.041823544852629624, 0.5163281919262531217 ) ) ;
#133026 = CARTESIAN_POINT ( 'NONE',  ( 3.773808747373870620, 0.9599976342714054978, 1.432812656881277791 ) ) ;
#133027 = CARTESIAN_POINT ( 'NONE',  ( -6.877010230629689858, 9.046264573866535486, 1.599625672291283607 ) ) ;
#133028 = CARTESIAN_POINT ( 'NONE',  ( 6.656857027519620829, -1.708965229049699053, 1.396003577074665714 ) ) ;
#133029 = CARTESIAN_POINT ( 'NONE',  ( 9.578796289606994918, -9.978085408363298825, -0.1296641399399049710 ) ) ;
#133030 = CARTESIAN_POINT ( 'NONE',  ( 4.416952212917071741, -1.612892420192946652, 1.453532087098859504 ) ) ;
#133031 = CARTESIAN_POINT ( 'NONE',  ( 3.246530741642670304, 0.4443377543969920795, 1.770662692542070538 ) ) ;
#133032 = CARTESIAN_POINT ( 'NONE',  ( 0.7956631384608278124, -1.383255022760669251, -1.391342014947574146 ) ) ;
#133033 = CARTESIAN_POINT ( 'NONE',  ( 5.243409334377605369, 0.4101777817676309223, -2.077071965933465769 ) ) ;
#133034 = EDGE_CURVE ( 'NONE', #52465, #31723, #194931, .T. ) ;
#133035 = ORIENTED_EDGE ( 'NONE', *, *, #113819, .T. ) ;
#133037 = CARTESIAN_POINT ( 'NONE',  ( -1.364683531250012516, 3.801041667008087099, -0.7879004041258300672 ) ) ;
#133036 = CARTESIAN_POINT ( 'NONE',  ( 6.233931918547526152, 2.266764885754421144, 0.3408509611897111991 ) ) ;
#133038 = CARTESIAN_POINT ( 'NONE',  ( 9.023114925094663619, 10.48572115315399245, 1.199719254218453823 ) ) ;
#133039 = CARTESIAN_POINT ( 'NONE',  ( 1.541811043186253061, -1.995513645039903361, 0.7175487213698438227 ) ) ;
#133040 = CARTESIAN_POINT ( 'NONE',  ( -4.256897045010916258, 7.910204285913967404, 0.7216878364870317197 ) ) ;
#133041 = DIRECTION ( 'NONE',  ( 0.000000000000000000, -1.000000000000000000, 0.000000000000000000 ) ) ;
#133042 = CARTESIAN_POINT ( 'NONE',  ( -4.243338890952901288, 6.934017225211593249, -1.082531754730548412 ) ) ;
#133043 = CARTESIAN_POINT ( 'NONE',  ( 6.596539238361469160, 2.146192635953731553, 0.3271905807876190897 ) ) ;
#133045 = CARTESIAN_POINT ( 'NONE',  ( -0.7500000000000179856, 13.07291666734946389, 1.299038105676658228 ) ) ;
#133044 = CARTESIAN_POINT ( 'NONE',  ( 6.983263157960365675, 7.629137130509066722, 2.553810918356711479 ) ) ;
#133047 = ORIENTED_EDGE ( 'NONE', *, *, #201142, .F. ) ;
#133046 = CARTESIAN_POINT ( 'NONE',  ( 1.981385142061100835, -2.032350350298214980, -0.8968915317347254668 ) ) ;
#133048 = CARTESIAN_POINT ( 'NONE',  ( -0.05159450770049476415, -2.057278634402651907, -1.025749021234131364 ) ) ;
#133050 = CARTESIAN_POINT ( 'NONE',  ( 4.996965725392733759, 0.3474287616172208604, 2.032942699294958633 ) ) ;
#133049 = CARTESIAN_POINT ( 'NONE',  ( 4.253507506385319381, 5.985511395581417204, 1.599625672291267398 ) ) ;
#133052 = CARTESIAN_POINT ( 'NONE',  ( 1.737499999999999378, -3.966666666666666785, -3.009438278150925683 ) ) ;
#133051 = CARTESIAN_POINT ( 'NONE',  ( 7.018280793729500644, 8.217024343219755167, -1.199719254218452047 ) ) ;
#133053 = ADVANCED_FACE ( 'NONE', ( #174779 ), #128235, .F. ) ;
#133054 = CARTESIAN_POINT ( 'NONE',  ( 5.091969210384201361, 8.098325291160362482, 1.199719254218452047 ) ) ;
#133055 = CARTESIAN_POINT ( 'NONE',  ( 1.001543065824772753E-15, -3.259374999522042682, 3.793834371823811669 ) ) ;
#133056 = CARTESIAN_POINT ( 'NONE',  ( 0.1331565106231328843, 0.003911343561965873426, -1.946049565259087455 ) ) ;
#133057 = CARTESIAN_POINT ( 'NONE',  ( 0.6563342376118604937, -1.512884991606887386, 1.443139479479842668 ) ) ;
#133058 = CARTESIAN_POINT ( 'NONE',  ( 5.168592345394213972, 1.356298078840772803, 1.492257005506092193 ) ) ;
#133059 = CARTESIAN_POINT ( 'NONE',  ( 4.493604616018744835, -1.840970053361364656, -0.04044509776383875543 ) ) ;
#133060 = ADVANCED_FACE ( 'NONE', ( #127159 ), #44779, .T. ) ;
#133062 = EDGE_LOOP ( 'NONE', ( #227, #26178, #70461, #188347 ) ) ;
#133061 = CARTESIAN_POINT ( 'NONE',  ( 6.328958779480917229, 6.278206752349526631, 0.7998128361456341429 ) ) ;
#133063 = SURFACE_STYLE_FILL_AREA ( #66921 ) ;
#133064 = CARTESIAN_POINT ( 'NONE',  ( 2.256509660847346943, -1.335373073873729943, 1.091610183656815503 ) ) ;
#133065 = CARTESIAN_POINT ( 'NONE',  ( 0.05782782957228919940, 1.164991625563294386, 1.645756161228327130 ) ) ;
#133066 = CARTESIAN_POINT ( 'NONE',  ( 1.600609022366938916, -0.2761435782051116505, 2.281986030651184993 ) ) ;
#133067 = CARTESIAN_POINT ( 'NONE',  ( -6.423865854776591000, 6.388931673527803667, 1.040834085586084257E-14 ) ) ;
#133068 = CARTESIAN_POINT ( 'NONE',  ( 1.019259390987249603, 2.090591978351970859, 0.8652678750288608223 ) ) ;
#133069 = CARTESIAN_POINT ( 'NONE',  ( 3.738982163358902877, 0.3088429966837880070, 2.083174605729753992 ) ) ;
#133070 = CARTESIAN_POINT ( 'NONE',  ( -4.111865726694519552, 8.019203457777400956, 0.000000000000000000 ) ) ;
#133071 = CARTESIAN_POINT ( 'NONE',  ( 6.693975156845185737, 8.832723654451292816, 1.599625672291281386 ) ) ;
#133072 = CARTESIAN_POINT ( 'NONE',  ( 4.353576723319599218, 8.093273587265928271, -0.7216878364870357165 ) ) ;
#133073 = CARTESIAN_POINT ( 'NONE',  ( 5.687500000000004441, -1.451031289060884077, 1.451031289061342378 ) ) ;
#133074 = B_SPLINE_CURVE_WITH_KNOTS ( 'NONE', 3,
 ( #183358, #48066, #17634, #51236, #83719, #81595, #147680, #149809, #117360, #114178, #34963, #150882, #18710, #84794, #2445, #180172, #16571, #68519, #213697, #134646, #151939, #49113, #52300, #118429, #102114, #168183, #85864, #196421 ),
 .UNSPECIFIED., .F., .F.,
 ( 4, 2, 2, 2, 2, 2, 2, 2, 2, 2, 2, 2, 2, 4 ),
 ( 8.673617379884039324E-19, 0.001589606426660063751, 0.002384409639990094001, 0.003179212853320124467, 0.003974016066650155367, 0.004768819279980185399, 0.006358425706640248067, 0.007153228919970278966, 0.007948032133300312468, 0.008742835346630343368, 0.009537638559960374268, 0.01033244177329040690, 0.01112724498662043780, 0.01271685141328049613 ),
 .UNSPECIFIED. ) ;
#133075 = CARTESIAN_POINT ( 'NONE',  ( -6.911959384868566758, 6.958374125301778790, 1.040834085586084257E-14 ) ) ;
#133076 = CARTESIAN_POINT ( 'NONE',  ( 0.7499999999999902300, 2.733333333333351600, 1.299038105676669330 ) ) ;
#133077 = CARTESIAN_POINT ( 'NONE',  ( -4.029797971759847997, 5.724516938518342535, -1.599625672291256295 ) ) ;
#133078 = CARTESIAN_POINT ( 'NONE',  ( 5.027667009318355973, -0.3252736580323810633, 2.197331836796195592 ) ) ;
#133079 = CARTESIAN_POINT ( 'NONE',  ( 3.662233025353780480, -1.472007171213615351, 1.623636439255560227 ) ) ;
#133080 = CARTESIAN_POINT ( 'NONE',  ( -3.913499895838973508, 7.717500311787445000, 1.040834085586084257E-14 ) ) ;
#133081 = CARTESIAN_POINT ( 'NONE',  ( -11.97929049433705551, 9.799999999999998934, 0.7046979865771804130 ) ) ;
#133082 = CARTESIAN_POINT ( 'NONE',  ( -1.364683531249997417, 3.009375000341422801, 1.214306433183764966E-14 ) ) ;
#133083 = CARTESIAN_POINT ( 'NONE',  ( 6.889999999999970370, 3.679256271150095792, 2.793895465809397294 ) ) ;
#133084 = CARTESIAN_POINT ( 'NONE',  ( -3.958617665510266725, 7.562211676496538360, -0.7216878364870267237 ) ) ;
#133085 = CARTESIAN_POINT ( 'NONE',  ( 5.256147377898004791, 0.8573370980917979223, -1.939729252509444279 ) ) ;
#133086 = CARTESIAN_POINT ( 'NONE',  ( -7.119440060951841787, 7.478637290631501067, 0.000000000000000000 ) ) ;
#133087 = VERTEX_POINT ( 'NONE', #78311 ) ;
#133089 = CARTESIAN_POINT ( 'NONE',  ( 6.789893189004300389, -0.9291300992274166282, 1.949920244826188309 ) ) ;
#133088 = CARTESIAN_POINT ( 'NONE',  ( -4.990809943606286048, 5.955604701363006015, -1.082531754730549967 ) ) ;
#133090 = CARTESIAN_POINT ( 'NONE',  ( 3.683011284406639607, 7.448596931783069586, 0.7998128361456321445 ) ) ;
#133091 = CARTESIAN_POINT ( 'NONE',  ( 6.022987620897008121, -1.731432113864934674, 0.6267441317700100933 ) ) ;
#133092 = SURFACE_STYLE_FILL_AREA ( #68020 ) ;
#133093 = CARTESIAN_POINT ( 'NONE',  ( -1.402160292154681736E-14, 2.259375000341416140, -1.575800808251660134 ) ) ;
#133094 = CARTESIAN_POINT ( 'NONE',  ( 0.7490575545651646516, 1.738588327661923394, -0.08332016361957059192 ) ) ;
#133095 = CARTESIAN_POINT ( 'NONE',  ( 2.496672843210871129, 6.064535417054653266, -0.7998128361456291469 ) ) ;
#133096 = CARTESIAN_POINT ( 'NONE',  ( 11.55950211276791428, 12.21999999999998288, 3.221476510067112109 ) ) ;
#133097 = CARTESIAN_POINT ( 'NONE',  ( 1.364683531249986537, 0.4260416670080872659, 0.7879004041258500513 ) ) ;
#133098 = CARTESIAN_POINT ( 'NONE',  ( -4.246261168552931231, 7.356898243746066157, -0.9190081729578998271 ) ) ;
#133099 = CARTESIAN_POINT ( 'NONE',  ( 5.243122039519461097, -1.856066598825537373, 1.107904190987746063 ) ) ;
#133100 = AXIS2_PLACEMENT_3D ( 'NONE', #82618, #199558, #31765 ) ;
#133101 = CARTESIAN_POINT ( 'NONE',  ( -2.598358995313378550, 6.183169261174235487, 0.7998128361456341429 ) ) ;
#133102 = CARTESIAN_POINT ( 'NONE',  ( -6.141480396866151992, 9.148515648777049591, 1.082531754730548412 ) ) ;
#133103 = CARTESIAN_POINT ( 'NONE',  ( 4.434552454296070145, 2.119417814153037316, 0.4246342833542292028 ) ) ;
#133104 = VERTEX_POINT ( 'NONE', #144435 ) ;
#133105 = CARTESIAN_POINT ( 'NONE',  ( -1.364683531250012516, 3.488541667008085767, -0.7879004041258300672 ) ) ;
#133106 = CARTESIAN_POINT ( 'NONE',  ( 6.344996225704436554, -1.666636976361988154, 1.052594414163325220 ) ) ;
#133107 = CARTESIAN_POINT ( 'NONE',  ( 5.044171318280882055, 1.617313383883935529, -0.6254187727454744161 ) ) ;
#133108 = STYLED_ITEM ( 'NONE', ( #213630 ), #186082 ) ;
#133110 = CARTESIAN_POINT ( 'NONE',  ( 1.540847765565691585, -1.849059859674206496, 1.176127931831471907 ) ) ;
#133109 = CARTESIAN_POINT ( 'NONE',  ( -10.56519166458664039, 11.25908454800986647, -3.404836274859124323 ) ) ;
#133111 = CARTESIAN_POINT ( 'NONE',  ( 2.046342449252246620, 0.8823731130137985046, -2.132409122670553270 ) ) ;
#133112 = CARTESIAN_POINT ( 'NONE',  ( 4.850885224688990860, -1.657504552092460504, 1.224352689660711535 ) ) ;
#133113 = CARTESIAN_POINT ( 'NONE',  ( 0.4802856102240244951, -0.2370191179813440352, -1.927374317010506877 ) ) ;
#133114 = CARTESIAN_POINT ( 'NONE',  ( -6.033015167956800262, 9.021972881716168402, -1.082531754730537976 ) ) ;
#133115 = CARTESIAN_POINT ( 'NONE',  ( -5.191846479390389568, 5.021852078902356631, 0.7998128361456281477 ) ) ;
#133116 = DIRECTION ( 'NONE',  ( -0.000000000000000000, -1.000000000000000000, 0.000000000000000000 ) ) ;
#133117 = CARTESIAN_POINT ( 'NONE',  ( 3.252298345715322281, 0.9499829135306799843, -1.895951488860507128 ) ) ;
#133118 = CARTESIAN_POINT ( 'NONE',  ( 1.424454163599726320, -1.462446849824734274, -1.388484543128357229 ) ) ;
#133119 = CARTESIAN_POINT ( 'NONE',  ( -5.978782553502159480, 8.958701498185728695, 1.082531754730548412 ) ) ;
#133120 = CARTESIAN_POINT ( 'NONE',  ( 4.524592175135637717, 1.360519573838222085, -1.737388959189074100 ) ) ;
#133121 = CARTESIAN_POINT ( 'NONE',  ( 1.001543065824772753E-15, -2.559374999522041172, 3.793834371823811669 ) ) ;
#133122 = CARTESIAN_POINT ( 'NONE',  ( 1.568971434307638857, 1.638126988201485279, 0.8830449202173286105 ) ) ;
#133123 =( GEOMETRIC_REPRESENTATION_CONTEXT ( 3 ) GLOBAL_UNCERTAINTY_ASSIGNED_CONTEXT ( ( #35321 ) ) GLOBAL_UNIT_ASSIGNED_CONTEXT ( ( #119191, #203546, #7490 ) ) REPRESENTATION_CONTEXT ( 'NONE', 'WORKASPACE' ) );
#133124 = CARTESIAN_POINT ( 'NONE',  ( 0.1399997263886038068, 6.947785072119228467, -2.594798351071639253 ) ) ;
#133125 = CARTESIAN_POINT ( 'NONE',  ( -0.08000000000000367928, 7.849261790823902629, 9.579665964948883783 ) ) ;
#133126 = CARTESIAN_POINT ( 'NONE',  ( 6.181863768892743138, 5.311700300033169952, -2.438145242048101569 ) ) ;
#133128 = CARTESIAN_POINT ( 'NONE',  ( -0.1000000000000080685, -9.919999999999998153, -10.91954211494235238 ) ) ;
#133127 = CARTESIAN_POINT ( 'NONE',  ( -5.058680321808019187, 7.974527835229765493, -1.188367278328520849 ) ) ;
#133129 = ORIENTED_EDGE ( 'NONE', *, *, #106815, .F. ) ;
#133130 = CARTESIAN_POINT ( 'NONE',  ( 3.678635468349491511, -1.985665955521208614, -0.5514216839303841544 ) ) ;
#133131 = CARTESIAN_POINT ( 'NONE',  ( -1.360316468750004448, 1.640625000341400241, -2.602085213965210642E-14 ) ) ;
#133132 = CARTESIAN_POINT ( 'NONE',  ( -7.040761844198392794, 7.108643661186573759, -0.7998128361456291469 ) ) ;
#133133 = CARTESIAN_POINT ( 'NONE',  ( 3.440107494509841768, -1.204893485711604484, -1.620726792054197452 ) ) ;
#133134 = CARTESIAN_POINT ( 'NONE',  ( -1.500000000000015099, -0.3708333333333105331, -0.8660254037844383745 ) ) ;
#133135 = CARTESIAN_POINT ( 'NONE',  ( 8.866669273657322492, 12.32790267170016207, -1.082531754730543083 ) ) ;
#133136 = CARTESIAN_POINT ( 'NONE',  ( 1.938423425814293388, 2.038317423364948588, 0.3033609537064930750 ) ) ;
#133138 = CARTESIAN_POINT ( 'NONE',  ( 1.364683531249997417, 12.98437500034139980, 2.602085213965210642E-15 ) ) ;
#133137 = CARTESIAN_POINT ( 'NONE',  ( 4.177814833339259515, 3.976464848425037779, 0.1981503615792765127 ) ) ;
#133139 = CARTESIAN_POINT ( 'NONE',  ( 4.981731378017507872, 7.899438143407371271, -1.199719254218452047 ) ) ;
#133140 = CARTESIAN_POINT ( 'NONE',  ( -0.2409995289980246258, 1.355929887833319469, -2.254219809973062816 ) ) ;
#133141 = CARTESIAN_POINT ( 'NONE',  ( 1.288719586054212884, 1.393062650230517674, 1.203921758438614376 ) ) ;
#133142 = CARTESIAN_POINT ( 'NONE',  ( 6.129534211984397629, -2.079372889712034489, 0.7396383780838566846 ) ) ;
#133143 = CARTESIAN_POINT ( 'NONE',  ( 6.561219994370630637, 6.619454513046008515, 0.000000000000000000 ) ) ;
#133144 = CARTESIAN_POINT ( 'NONE',  ( 2.003414267471514965, 1.795956895356983551, 1.202623776965026536 ) ) ;
#133145 = CARTESIAN_POINT ( 'NONE',  ( -3.850152436600983386, 4.554561266531622188, 1.082531754730560403 ) ) ;
#133146 = CARTESIAN_POINT ( 'NONE',  ( 2.325407997918966796, -1.497503195670712328, -1.350734289967000512 ) ) ;
#133147 = CARTESIAN_POINT ( 'NONE',  ( -0.1695794614869980399, 7.019966546936163176, 3.993288729248444024 ) ) ;
#133148 =( LENGTH_UNIT ( ) NAMED_UNIT ( * ) SI_UNIT ( .MILLI., .METRE. ) );
#133149 = CARTESIAN_POINT ( 'NONE',  ( 4.100430126988792168, -0.6171887515804741486, -1.872443122656509029 ) ) ;
#133150 = STYLED_ITEM ( 'NONE', ( #43323 ), #86239 ) ;
#133151 = CARTESIAN_POINT ( 'NONE',  ( 3.309780021317248355, -1.205041885261768808, -1.616693488061982098 ) ) ;
#133153 = CARTESIAN_POINT ( 'NONE',  ( 8.663296969007976855, 12.09063498294259809, -1.082531754730543083 ) ) ;
#133152 = CARTESIAN_POINT ( 'NONE',  ( 1.364683531249988757, 1.884375000341421913, 0.000000000000000000 ) ) ;
#133155 = CARTESIAN_POINT ( 'NONE',  ( 6.445935634123193481, 0.8078061350838610100, -1.945192272397469280 ) ) ;
#133154 = CARTESIAN_POINT ( 'NONE',  ( -8.389798128758148010, 8.682519326506312751, 0.7998128361456462443 ) ) ;
#133156 = B_SPLINE_CURVE_WITH_KNOTS ( 'NONE', 3,
 ( #156956, #190490, #83135, #82072 ),
 .UNSPECIFIED., .F., .F.,
 ( 4, 4 ),
 ( 0.0005910214237607931166, 0.001001414237305830969 ),
 .UNSPECIFIED. ) ;
#133157 = CARTESIAN_POINT ( 'NONE',  ( 5.723117673755029777, -1.870111591731966616, -0.8886290660751752224 ) ) ;
#133158 = CARTESIAN_POINT ( 'NONE',  ( 5.849453209292126310, 8.911780279894442103, 1.199719254218462483 ) ) ;
#133159 = CARTESIAN_POINT ( 'NONE',  ( -6.177711549321182716, 10.35908057418338402, 0.7998128361456481317 ) ) ;
#133160 = CARTESIAN_POINT ( 'NONE',  ( 1.963827086952127710, 3.753930767994603457, -0.3999999999999195310 ) ) ;
#133161 = CARTESIAN_POINT ( 'NONE',  ( 5.344012529290226965, -1.284645313656457288, -1.558556736529070674 ) ) ;
#133162 = CARTESIAN_POINT ( 'NONE',  ( 0.7499999999999867883, -0.6520833326505159899, -1.299038105676652899 ) ) ;
#133163 = PRESENTATION_LAYER_ASSIGNMENT (  '', '', ( #126407 ) ) ;
#133164 = CARTESIAN_POINT ( 'NONE',  ( 0.4091259740910870302, -1.658837074242287102, 1.225595967756993865 ) ) ;
#133165 = CARTESIAN_POINT ( 'NONE',  ( 8.622622508611357262, 9.162073802909148412, -0.7216878364870197293 ) ) ;
#133166 = CARTESIAN_POINT ( 'NONE',  ( 5.559725510055676168, 8.644040974110419384, 1.199719254218451159 ) ) ;
#133167 = CARTESIAN_POINT ( 'NONE',  ( 5.737035277238070385, 6.722237907313067140, -1.199719254218452047 ) ) ;
#133168 = CARTESIAN_POINT ( 'NONE',  ( 1.364683531249986537, 0.9677083336747538400, -0.7879004041258239610 ) ) ;
#133170 = CARTESIAN_POINT ( 'NONE',  ( 6.727182134110199385, 3.711531441867378600, 2.225637065106730095 ) ) ;
#133169 = CARTESIAN_POINT ( 'NONE',  ( 5.337069745634900997, 6.255611453776062980, 1.199719254218452047 ) ) ;
#133171 = CARTESIAN_POINT ( 'NONE',  ( 6.060131475184119765, 9.053608573481392696, -1.082531754730537976 ) ) ;
#133173 = DIRECTION ( 'NONE',  ( 0.000000000000000000, 0.000000000000000000, 1.000000000000000000 ) ) ;
#133172 = CARTESIAN_POINT ( 'NONE',  ( 2.717415358725610908, -1.887964963866497259, -1.072103292869843960 ) ) ;
#133174 = CARTESIAN_POINT ( 'NONE',  ( -3.065858701071340509, -0.8887487162373149951, -1.201087490044906669 ) ) ;
#133176 = CARTESIAN_POINT ( 'NONE',  ( 2.700538275128167687, 1.556679782967337999, 0.9830204120172959525 ) ) ;
#133175 = CARTESIAN_POINT ( 'NONE',  ( -4.067082894419624672, 6.728385229256075739, 1.082531754730560403 ) ) ;
#133177 = CARTESIAN_POINT ( 'NONE',  ( -1.364683531249997417, 4.509375000341424133, 1.214306433183764966E-14 ) ) ;
#133178 = CARTESIAN_POINT ( 'NONE',  ( 4.019203527901527018, -2.096847714747759106, 0.6372333828079318474 ) ) ;
#133179 = CARTESIAN_POINT ( 'NONE',  ( 0.09999999999999592548, -9.999999999999994671, 10.91954211494236660 ) ) ;
#133180 = CARTESIAN_POINT ( 'NONE',  ( 4.311571290614625518, -0.3905533787264577894, 2.228413237907675537 ) ) ;
#133181 = CYLINDRICAL_SURFACE ( 'NONE', #31858, 0.08000000000000020983 ) ;
#133182 = CARTESIAN_POINT ( 'NONE',  ( 4.623177087595867540, 8.455029494522658950, -0.3425024339245314464 ) ) ;
#133183 = CARTESIAN_POINT ( 'NONE',  ( -5.112833325684908559, 8.018703742390766109, -1.082531754730549967 ) ) ;
#133184 = CARTESIAN_POINT ( 'NONE',  ( 3.906157654512984134, 7.571284673658201569, -0.7216878364870338292 ) ) ;
#133185 = CARTESIAN_POINT ( 'NONE',  ( 6.555894367415777246, 1.764769525206461687, -0.1329060007094622631 ) ) ;
#133186 = CARTESIAN_POINT ( 'NONE',  ( 3.826817946245956392, 1.422007987377239546, -1.425180056034919041 ) ) ;
#133187 = CARTESIAN_POINT ( 'NONE',  ( 7.983053520348166288, 8.207983950027992748, -0.7998128361456281477 ) ) ;
#133188 = CARTESIAN_POINT ( 'NONE',  ( 2.626118769021787536, -1.211593817910999293, -1.722331309457482362 ) ) ;
#133189 = CARTESIAN_POINT ( 'NONE',  ( 1.528765853866232538, -1.617345627753681514, 1.026210199876474105 ) ) ;
#133190 = CARTESIAN_POINT ( 'NONE',  ( -8.012344526598182026E-15, 11.54687500034139980, -1.575800808251669460 ) ) ;
#133191 = CARTESIAN_POINT ( 'NONE',  ( 1.574589453129974004, 1.325232347829819135, -1.457171473731319278 ) ) ;
#133192 = CARTESIAN_POINT ( 'NONE',  ( 1.076777757339364205, -0.04213119042271313425, -1.870346338061685154 ) ) ;
#133193 = CARTESIAN_POINT ( 'NONE',  ( 0.5198770262540284293, 1.941052373433370448, -0.2841105942011297736 ) ) ;
#133195 = ORIENTED_EDGE ( 'NONE', *, *, #64213, .F. ) ;
#133194 = CARTESIAN_POINT ( 'NONE',  ( 0.4219365929402639215, -1.902980170924161385, 0.1897552588234762416 ) ) ;
#133196 = CARTESIAN_POINT ( 'NONE',  ( 4.473827502829567315, 7.202920605734387749, -1.082531754730548412 ) ) ;
#133197 = CARTESIAN_POINT ( 'NONE',  ( -0.6823417656250212460, 1.363541667008083547, 1.181850606188755259 ) ) ;
#133198 = ADVANCED_FACE ( 'NONE', ( #210437 ), #62078, .T. ) ;
#133199 = CARTESIAN_POINT ( 'NONE',  ( 5.840666405660361882, 0.3664468388623157158, 1.834233659845654119 ) ) ;
#133200 = CARTESIAN_POINT ( 'NONE',  ( 9.028840231696797503, 12.62106513936658203, -1.199719254218446718 ) ) ;
#133201 = CYLINDRICAL_SURFACE ( 'NONE', #151823, 2.500000000000000888 ) ;
#133202 = CARTESIAN_POINT ( 'NONE',  ( 6.244996659533327943, -0.2978818936431072983, -2.048576297084458098 ) ) ;
#133203 = CARTESIAN_POINT ( 'NONE',  ( 0.6124999999999793943, 2.833333333333354354, 1.060881119635899816 ) ) ;
#133204 = CARTESIAN_POINT ( 'NONE',  ( -0.7500000000000006661, 0.8583333333333567072, -1.299038105676652011 ) ) ;
#133205 = CARTESIAN_POINT ( 'NONE',  ( 7.450369105909416589, 8.650851030771185890, -1.199719254218441611 ) ) ;
#133206 = CARTESIAN_POINT ( 'NONE',  ( -9.013473194986783454, 9.410140237106395134, -0.7998128361456291469 ) ) ;
#133207 = CARTESIAN_POINT ( 'NONE',  ( 3.867818961648523235, 7.734482231890414283, 1.040834085586084257E-14 ) ) ;
#133208 = CARTESIAN_POINT ( 'NONE',  ( 3.898851692381625877, 6.706354853490643642, -1.199719254218452047 ) ) ;
#133209 = CARTESIAN_POINT ( 'NONE',  ( -0.6823417656250212460, 1.551041667008083769, 1.181850606188755259 ) ) ;
#133210 = CARTESIAN_POINT ( 'NONE',  ( 1.499999999999989120, 2.254166666666685970, 0.8660254037844524744 ) ) ;
#133212 = CARTESIAN_POINT ( 'NONE',  ( 3.310162060030825248, 7.013606170011280838, -0.7998128361456291469 ) ) ;
#133211 = CARTESIAN_POINT ( 'NONE',  ( 6.426224708462171087, 1.007414738832881351, 1.683299376423300853 ) ) ;
#133213 = CARTESIAN_POINT ( 'NONE',  ( 3.268907511149142575, -2.013924394373915128, 0.09611935726179518524 ) ) ;
#133214 = CARTESIAN_POINT ( 'NONE',  ( 4.135878506090823414, 1.915180532728939289, -0.05283342432932899152 ) ) ;
#133215 = CARTESIAN_POINT ( 'NONE',  ( 11.92619526248524586, 10.07255386085825677, -1.328859120100568170 ) ) ;
#133216 = CARTESIAN_POINT ( 'NONE',  ( 1.751786407749492014, 2.185395279939935431, -0.1653414253460702699 ) ) ;
#133217 = CARTESIAN_POINT ( 'NONE',  ( 0.1333692844072559280, 6.947498546895843674, -2.648624074793118233 ) ) ;
#133218 = CARTESIAN_POINT ( 'NONE',  ( 2.987410616422137899, 1.320145714686842497, 1.325460448179466066 ) ) ;
#133219 = CARTESIAN_POINT ( 'NONE',  ( 1.499999999999989120, -0.1937499993171845625, 0.000000000000000000 ) ) ;
#133220 = CARTESIAN_POINT ( 'NONE',  ( -7.588813295347149435, 9.876701482703580837, -1.599625672291263179 ) ) ;
#133222 = CARTESIAN_POINT ( 'NONE',  ( 4.077823013788191453, -0.8085361882982607939, 1.956954002425244088 ) ) ;
#133221 = CARTESIAN_POINT ( 'NONE',  ( -3.456965981804629884, 6.976951378839947537, 1.040834085586084257E-14 ) ) ;
#133224 = VECTOR ( 'NONE', #29509, 1000.000000000000000 ) ;
#133223 = FILL_AREA_STYLE ('',( #29303 ) ) ;
#133225 = CARTESIAN_POINT ( 'NONE',  ( 5.916483165358986440, 0.8355632440216669288, 1.894440869009452300 ) ) ;
#133227 = CARTESIAN_POINT ( 'NONE',  ( 6.620655732516668834, 7.629137130509086262, 2.873739711112702544 ) ) ;
#133226 = CARTESIAN_POINT ( 'NONE',  ( 2.401997865216979111, -0.8028288615537516604, -1.930668023334235484 ) ) ;
#133229 = VERTEX_POINT ( 'NONE', #195278 ) ;
#133228 = CARTESIAN_POINT ( 'NONE',  ( 0.6919144707170435948, -1.710882258413017221, -0.2179282654613586834 ) ) ;
#133230 = ADVANCED_FACE ( 'NONE', ( #111963 ), #196344, .F. ) ;
#133231 = CARTESIAN_POINT ( 'NONE',  ( 6.124532705071213279, 8.168374127381657246, -1.599625672291262513 ) ) ;
#133232 = CARTESIAN_POINT ( 'NONE',  ( 9.354067518987882579, 13.88574871644472708, 7.517258212044111154 ) ) ;
#133233 = DIRECTION ( 'NONE',  ( -1.000000000000000000, 7.771561172376097755E-16, 4.440892098500627148E-16 ) ) ;
#133234 = CARTESIAN_POINT ( 'NONE',  ( -9.410012541129075814, 4.000000000000001776, 6.919867902370715917 ) ) ;
#133235 = CARTESIAN_POINT ( 'NONE',  ( 7.470179451005385829, 8.777926116670192513, -1.082531754730537976 ) ) ;
#133236 = CARTESIAN_POINT ( 'NONE',  ( 8.948250016579860855, 1.813773193624685254, 7.995571895478047253 ) ) ;
#133238 = CARTESIAN_POINT ( 'NONE',  ( 0.5217373455332212639, -1.802923944912222520, 0.1758665181858156124 ) ) ;
#133237 = CARTESIAN_POINT ( 'NONE',  ( 5.155843554946782703, 9.237177590738404831, -0.7998128361456481317 ) ) ;
#133239 = CARTESIAN_POINT ( 'NONE',  ( -6.157374318900681764, 10.33535380535947290, 0.7998128361456481317 ) ) ;
#133240 = CARTESIAN_POINT ( 'NONE',  ( 4.976006071415387311, 5.764094157194782575, 1.199719254218462483 ) ) ;
#133241 = CARTESIAN_POINT ( 'NONE',  ( -6.184982820901517186, 6.966600618058066630, 0.8941503475990535410 ) ) ;
#133242 = CARTESIAN_POINT ( 'NONE',  ( 5.580062740476173566, 8.667767742934335828, 1.199719254218451159 ) ) ;
#133243 = CARTESIAN_POINT ( 'NONE',  ( 1.387358672533593129, 7.315968950352074174, -4.254625267140469624 ) ) ;
#133244 = CARTESIAN_POINT ( 'NONE',  ( -6.773846765307970585, -7.473374494058216300, 6.773846765307992790 ) ) ;
#133245 = CARTESIAN_POINT ( 'NONE',  ( 4.041346116833469893, 7.538066791021210022, -0.4365389052301202333 ) ) ;
#133246 = CARTESIAN_POINT ( 'NONE',  ( 7.917598520700710019, 12.18102267421877727, -0.7216878364870328300 ) ) ;
#133247 = ORIENTED_EDGE ( 'NONE', *, *, #17877, .T. ) ;
#133248 = CARTESIAN_POINT ( 'NONE',  ( 2.523689441098162511, 1.825779920793478839, -0.3596660026494375995 ) ) ;
#133249 = CARTESIAN_POINT ( 'NONE',  ( 0.5795164177304649167, -0.6885740665637375413, 1.787764417203549172 ) ) ;
#133250 = CARTESIAN_POINT ( 'NONE',  ( 0.7332529803791461021, 1.960763319057107879, 0.8078710241638600298 ) ) ;
#133251 = PRESENTATION_LAYER_ASSIGNMENT (  '', '', ( #12153 ) ) ;
#133252 = FILL_AREA_STYLE ('',( #99652 ) ) ;
#133253 = CARTESIAN_POINT ( 'NONE',  ( -0.1399997263889611598, 2.874570648431204578, -2.488748559936367233 ) ) ;
#133254 = CARTESIAN_POINT ( 'NONE',  ( -1.525860493984666055, 8.693043820721571890, -2.521102513734311046 ) ) ;
#133255 = CARTESIAN_POINT ( 'NONE',  ( -4.609409038966248318, 5.440360635957812718, -1.082531754730544860 ) ) ;
#133256 = CARTESIAN_POINT ( 'NONE',  ( 7.456621297836061757, 11.64321591421002644, 0.7216878364870438212 ) ) ;
#133257 = CARTESIAN_POINT ( 'NONE',  ( 4.627768981117735159, 1.911305289405954344, -0.4745475857620209958 ) ) ;
#133258 = CARTESIAN_POINT ( 'NONE',  ( 1.137531110418067204, -0.04838959064331486287, 2.120096749846810624 ) ) ;
#133259 = CARTESIAN_POINT ( 'NONE',  ( -6.175902666224832416, 7.163973517805802160, -1.199719254218446718 ) ) ;
#133260 = SPHERICAL_SURFACE ( 'NONE', #207780, 0.08000000000000000167 ) ;
#133261 = CARTESIAN_POINT ( 'NONE',  ( -3.129460678718345878, 6.444905630999884671, -0.7687999843507524744 ) ) ;
#133262 = CARTESIAN_POINT ( 'NONE',  ( 5.595707529797693702, -2.191629465999441084, -0.002916574791289594515 ) ) ;
#133263 = CARTESIAN_POINT ( 'NONE',  ( 3.922244425448867311, 2.804391244181456244, 0.7750000000000135669 ) ) ;
#133264 = CARTESIAN_POINT ( 'NONE',  ( 4.506809989931632288, 1.489605450875215453, -1.221516061710873347 ) ) ;
#133265 = CARTESIAN_POINT ( 'NONE',  ( -7.049349804101573191, 10.31165964050546258, -1.199719254218440723 ) ) ;
#133266 = CARTESIAN_POINT ( 'NONE',  ( 0.1295496576057716120, -1.118478952742516297, -1.443350188048427629 ) ) ;
#133267 = CARTESIAN_POINT ( 'NONE',  ( 0.9091299924109221831, 1.668792687453458878, -1.444214864661397035 ) ) ;
#133268 = EDGE_CURVE ( 'NONE', #110438, #131570, #100616, .T. ) ;
#133269 = DIRECTION ( 'NONE',  ( 0.000000000000000000, 0.000000000000000000, -1.000000000000000000 ) ) ;
#133270 = ORIENTED_EDGE ( 'NONE', *, *, #148486, .T. ) ;
#133271 = CARTESIAN_POINT ( 'NONE',  ( 4.760321332173959696, 4.726332107057286791, 0.000000000000000000 ) ) ;
#133272 = VERTEX_POINT ( 'NONE', #114103 ) ;
#133273 = CARTESIAN_POINT ( 'NONE',  ( 5.717622241336643540, 0.3879015478767386949, -1.930678852912662391 ) ) ;
#133274 = CARTESIAN_POINT ( 'NONE',  ( 1.452572125225624955, -1.666495805118956897, -0.9969474394922008820 ) ) ;
#133275 = CARTESIAN_POINT ( 'NONE',  ( 6.731773689652298387, -2.096994807688298934, -0.9412720059410217832 ) ) ;
#133277 = CARTESIAN_POINT ( 'NONE',  ( 4.434314628233038569, -1.074157013132440275, 1.519412852752539678 ) ) ;
#133276 = CARTESIAN_POINT ( 'NONE',  ( -7.228432174741334038, 8.462200954400218578, -1.199719254218452047 ) ) ;
#133278 = CARTESIAN_POINT ( 'NONE',  ( 6.176621499477501054, 9.363752961769195693, -1.199719254218452047 ) ) ;
#133279 = FACE_OUTER_BOUND ( 'NONE', #143061, .T. ) ;
#133280 = CYLINDRICAL_SURFACE ( 'NONE', #109371, 4.500000000000000000 ) ;
#133281 = CARTESIAN_POINT ( 'NONE',  ( -5.042743069279040036, 7.970618449879118828, 1.199719254218464037 ) ) ;
#133282 = CARTESIAN_POINT ( 'NONE',  ( -3.349705649621375958, -0.9332739474907891797, 0.06918225470302911961 ) ) ;
#133283 = CARTESIAN_POINT ( 'NONE',  ( -0.07626876867936756288, -1.353788312843669406, -1.724171373301164767 ) ) ;
#133284 = CARTESIAN_POINT ( 'NONE',  ( 3.389175213736285386, 6.897862149426897460, 0.7216878364870317197 ) ) ;
#133285 = DIRECTION ( 'NONE',  ( -0.000000000000000000, -1.000000000000000000, -0.000000000000000000 ) ) ;
#133286 = CARTESIAN_POINT ( 'NONE',  ( -0.4366904681730566784, -5.787668213791788752, -10.40319425600973346 ) ) ;
#133288 = ADVANCED_FACE ( 'NONE', ( #47987 ), #197995, .F. ) ;
#133287 = CARTESIAN_POINT ( 'NONE',  ( 1.805030607383810715, 1.517133602069477893, 1.015288170653723343 ) ) ;
#133289 = CARTESIAN_POINT ( 'NONE',  ( -3.761497552787613330, 6.475832013972435242, 1.199719254218464037 ) ) ;
#133290 = CARTESIAN_POINT ( 'NONE',  ( 3.990606130280470509, -1.729166733334456030, 0.1323968765898491939 ) ) ;
#133291 = CARTESIAN_POINT ( 'NONE',  ( -6.597731880524014159, 6.769412454161013670, -0.2479414380717175903 ) ) ;
#133292 = CARTESIAN_POINT ( 'NONE',  ( -1.225000000000011857, 2.770833333333349024, 0.7072540797572636206 ) ) ;
#133293 = CARTESIAN_POINT ( 'NONE',  ( 1.292128843000315053, 8.373613470998938269, -10.90074592850030655 ) ) ;
#133294 = CARTESIAN_POINT ( 'NONE',  ( 0.4164666496747080338, 1.329428171303851824, -1.394508830869565230 ) ) ;
#133295 = CARTESIAN_POINT ( 'NONE',  ( 4.803538753074391821, -1.513872852549098091, -1.247617340562396926 ) ) ;
#133296 = CARTESIAN_POINT ( 'NONE',  ( -7.069687034522070590, 10.33538640932937724, -1.199719254218440723 ) ) ;
#133297 = CARTESIAN_POINT ( 'NONE',  ( 7.284808609244363353, 7.393364887073558656, 0.7998128361456341429 ) ) ;
#133298 = CARTESIAN_POINT ( 'NONE',  ( 4.547591073264711348, -1.938359017324686961, 0.8602097090630378418 ) ) ;
#133299 = DIRECTION ( 'NONE',  ( 1.224646799147343346E-16, 0.000000000000000000, -1.000000000000000000 ) ) ;
#133300 = CARTESIAN_POINT ( 'NONE',  ( -7.133561379084627063, 11.47423870890741782, 0.7998128361456481317 ) ) ;
#133301 = B_SPLINE_CURVE_WITH_KNOTS ( 'NONE', 3,
 ( #30972, #95981, #113345, #81829 ),
 .UNSPECIFIED., .F., .F.,
 ( 4, 4 ),
 ( 0.0005609329959280208141, 0.0008723013827243832410 ),
 .UNSPECIFIED. ) ;
#133302 = CARTESIAN_POINT ( 'NONE',  ( 4.147904930777053245, 6.926640621626830807, -1.199719254218452047 ) ) ;
#133303 = CARTESIAN_POINT ( 'NONE',  ( 3.080986915251407776, 1.947773190787219555, 0.7018234266842755531 ) ) ;
#133305 = CARTESIAN_POINT ( 'NONE',  ( 1.364683531249986537, 0.4677083336747514530, -0.7879004041258309554 ) ) ;
#133304 = FACE_OUTER_BOUND ( 'NONE', #159411, .T. ) ;
#133306 = VERTEX_POINT ( 'NONE', #17554 ) ;
#133307 = CARTESIAN_POINT ( 'NONE',  ( 2.831036414133382806, 0.8244386821347724492, -2.145926533794308533 ) ) ;
#133308 = CARTESIAN_POINT ( 'NONE',  ( 9.246297574839983824, 9.889694713509232571, 0.7216878364870438212 ) ) ;
#133310 = CARTESIAN_POINT ( 'NONE',  ( -3.285556943749998737, -1.480208332855375453, 1.896917185911908499 ) ) ;
#133309 = CARTESIAN_POINT ( 'NONE',  ( 6.319508997745523438, 9.426492026461511742, -1.082531754730548412 ) ) ;
#133311 = ADVANCED_FACE ( 'NONE', ( #164901 ), #35349, .T. ) ;
#133312 = CARTESIAN_POINT ( 'NONE',  ( -2.324088772396477673E-16, 1.562500000000000666, 1.224999999999980549 ) ) ;
#133313 = CARTESIAN_POINT ( 'NONE',  ( 6.609000000000015085, -6.653734696159079563E-05, 2.100160721423646404 ) ) ;
#133314 = VERTEX_POINT ( 'NONE', #212574 ) ;
#133316 = CARTESIAN_POINT ( 'NONE',  ( -3.283337425626721373, -0.1112512837626866702, -0.1207467602163218856 ) ) ;
#133315 = AXIS2_PLACEMENT_3D ( 'NONE', #108021, #155637, #207573 ) ;
#133317 = ADVANCED_FACE ( 'NONE', ( #82575 ), #163853, .F. ) ;
#133318 = CARTESIAN_POINT ( 'NONE',  ( 3.867365959033176814, -1.592763314076732106, -1.058159689705892692 ) ) ;
#133319 = CARTESIAN_POINT ( 'NONE',  ( -0.2309780072035732823, 7.005396854623739067, -3.973862472851087624 ) ) ;
#133320 = CARTESIAN_POINT ( 'NONE',  ( 5.139545982361763521, -1.221863454424999329, -1.217595815693907957 ) ) ;
#133321 = CARTESIAN_POINT ( 'NONE',  ( 3.204314817619222211, 1.275555974797081049, -1.561881975048397209 ) ) ;
#133322 = CARTESIAN_POINT ( 'NONE',  ( 5.326872488440856479, 0.9340183262317149904, -2.100526973934746522 ) ) ;
#133323 = DIRECTION ( 'NONE',  ( 0.7592566023653005702, 0.6507913734559639396, 0.000000000000000000 ) ) ;
#133324 = CARTESIAN_POINT ( 'NONE',  ( 0.6982365061397632910, -0.7907169553198112322, 2.060542492664858560 ) ) ;
#133325 = CARTESIAN_POINT ( 'NONE',  ( -5.506019780925599960, 5.596313630600862510, 0.7216878364870257245 ) ) ;
#133326 = CARTESIAN_POINT ( 'NONE',  ( 5.571497546025357295, 1.705283197966761310, -0.4730582879079441305 ) ) ;
#133328 = CARTESIAN_POINT ( 'NONE',  ( 1.746416057278064482, 0.7220573502318957670, 2.175635376676859689 ) ) ;
#133327 = CARTESIAN_POINT ( 'NONE',  ( 4.701645408888975197, 8.707279753670952971, 0.000000000000000000 ) ) ;
#133329 = CARTESIAN_POINT ( 'NONE',  ( 6.720655732516648939, 0.005566325962592238129, 1.826293863978686538 ) ) ;
#133330 = CARTESIAN_POINT ( 'NONE',  ( -2.785310492603665367, 5.336947110424484109, 1.199719254218462483 ) ) ;
#133331 = CARTESIAN_POINT ( 'NONE',  ( 6.471393748265519719, 5.229711127717882491, -2.419999999999995044 ) ) ;
#133332 = CARTESIAN_POINT ( 'NONE',  ( -5.113360211009450040, 5.994616996712990975, -1.199719254218453823 ) ) ;
#133333 = CARTESIAN_POINT ( 'NONE',  ( -1.360316468750024876, -0.8072916663252578395, 0.7853790794158560518 ) ) ;
#133334 = CARTESIAN_POINT ( 'NONE',  ( -8.158842082463221956, 15.47018964179058287, 8.845107385697343005 ) ) ;
#133335 = CARTESIAN_POINT ( 'NONE',  ( 6.478973898625433492, 1.930320082341809629, 0.7489585856828018251 ) ) ;
#133336 = CARTESIAN_POINT ( 'NONE',  ( 0.7082206942033396624, 1.197301205363930254, -1.622488844446705381 ) ) ;
#133337 = CARTESIAN_POINT ( 'NONE',  ( -0.7500000000000249800, -0.2770833326505156569, 1.299038105676659116 ) ) ;
#133338 = CARTESIAN_POINT ( 'NONE',  ( 5.109954983015153829, -1.917020813385891254, 0.1909056391717136592 ) ) ;
#133339 = CARTESIAN_POINT ( 'NONE',  ( -1.364683531250000748, 11.35937500034139802, 0.000000000000000000 ) ) ;
#133340 = CARTESIAN_POINT ( 'NONE',  ( 2.285647630545981190, 0.1040316455800850692, -2.219075330209609120 ) ) ;
#133341 = ORIENTED_EDGE ( 'NONE', *, *, #200423, .T. ) ;
#133343 = DIRECTION ( 'NONE',  ( 0.000000000000000000, -1.000000000000000000, 0.000000000000000000 ) ) ;
#133342 = CYLINDRICAL_SURFACE ( 'NONE', #120050, 1.250000000000000000 ) ;
#133344 = CARTESIAN_POINT ( 'NONE',  ( 8.432281472695482449, 11.92507992053172572, 1.199719254218450271 ) ) ;
#133345 = CARTESIAN_POINT ( 'NONE',  ( 6.170369307550806148, 10.21286493553572328, 0.7216878364870317197 ) ) ;
#133346 = CARTESIAN_POINT ( 'NONE',  ( 4.669343813871559945, 1.007284801977660349, 1.419122490755047705 ) ) ;
#133347 = CARTESIAN_POINT ( 'NONE',  ( 2.383191274269541360, -0.003000794896521400724, 1.962046632024143866 ) ) ;
#133349 = CARTESIAN_POINT ( 'NONE',  ( -7.565086526745425033, 7.928281824065535055, 0.7216878364870317197 ) ) ;
#133348 = CARTESIAN_POINT ( 'NONE',  ( 5.332434488876471868, 5.115595079977664383, 0.7998128361456341429 ) ) ;
#133350 = CARTESIAN_POINT ( 'NONE',  ( -5.788012183699196456, 6.074875824575221017, 0.5810633148162994699 ) ) ;
#133351 = CARTESIAN_POINT ( 'NONE',  ( -2.981281212289682792, 6.492261378021210838, -0.0003813922843012157449 ) ) ;
#133352 = CIRCLE ( 'NONE', #147093, 0.7499999999999997780 ) ;
#133353 = CARTESIAN_POINT ( 'NONE',  ( 1.522013433763437895, 2.032506561856410876, -0.3506121680386958261 ) ) ;
#133354 = CARTESIAN_POINT ( 'NONE',  ( -7.694415870955439551, 8.935572256658169010, 1.199719254218462483 ) ) ;
#133355 = CARTESIAN_POINT ( 'NONE',  ( -4.080641047588918546, 4.823464646017586510, -1.082531754730548412 ) ) ;
#133356 = CARTESIAN_POINT ( 'NONE',  ( 1.200488511320395579, -2.262689073810118412, 0.002107776778791786276 ) ) ;
#133357 = ORIENTED_EDGE ( 'NONE', *, *, #98548, .T. ) ;
#133358 = CARTESIAN_POINT ( 'NONE',  ( -1.500000000000015099, -0.3395833326505143801, -0.8660254037844383745 ) ) ;
#133359 = CARTESIAN_POINT ( 'NONE',  ( 2.126040175964475143, 1.080828230516362121, -1.526477596812993553 ) ) ;
#133360 = CARTESIAN_POINT ( 'NONE',  ( 0.9494047574800461575, -1.567277312892487284, -0.7424874142042283687 ) ) ;
#133361 = CARTESIAN_POINT ( 'NONE',  ( 5.530878137806295669, -1.981686641427220286, 0.9361944923952856268 ) ) ;
#133362 = CARTESIAN_POINT ( 'NONE',  ( 5.614422408412740317, -1.031215703586242149, -2.064428503307714546 ) ) ;
#133363 = CARTESIAN_POINT ( 'NONE',  ( 1.112264416572866566, -0.9257652390157306010, -1.841317064699917516 ) ) ;
#133364 = CARTESIAN_POINT ( 'NONE',  ( 3.679572934066538181, -0.9564393601015194202, 1.690012426612282681 ) ) ;
#133365 = CARTESIAN_POINT ( 'NONE',  ( -3.728129053633589152, 7.293308295973741195, 0.7216878364870317197 ) ) ;
#133366 = PRODUCT_DEFINITION_SHAPE ( 'NONE', 'NONE',  #128644 ) ;
#133367 = CARTESIAN_POINT ( 'NONE',  ( 5.940666398231567058, 0.3644617591120716260, 1.834516074763043347 ) ) ;
#133368 = CARTESIAN_POINT ( 'NONE',  ( 1.562500000000001554, -1.451031289061184282, -1.451031289061057050 ) ) ;
#133369 = CARTESIAN_POINT ( 'NONE',  ( 0.3667750149253126701, 13.29281888235296094, 1.403446231478199246 ) ) ;
#133370 = CARTESIAN_POINT ( 'NONE',  ( 6.204453847213379447, -1.458334814074750740, -1.392330997281837623 ) ) ;
#133371 =( NAMED_UNIT ( * ) SI_UNIT ( $, .STERADIAN. ) SOLID_ANGLE_UNIT ( ) );
#133372 = CARTESIAN_POINT ( 'NONE',  ( -0.6801582343750143256, 1.848958333674724397, -1.178068619123862515 ) ) ;
#133373 = CARTESIAN_POINT ( 'NONE',  ( 4.360000113718985659, -0.002809843368253156070, -2.016597020062675050 ) ) ;
#133374 = CARTESIAN_POINT ( 'NONE',  ( -2.779058300676974014, 6.186059084191009916, -0.7216878364870257245 ) ) ;
#133375 = CARTESIAN_POINT ( 'NONE',  ( 7.248805684800777804, 11.60869039890961218, 1.040834085586084257E-14 ) ) ;
#133376 = CARTESIAN_POINT ( 'NONE',  ( 4.716257332707354699, 6.595662536282280719, -1.599625672291269396 ) ) ;
#133378 = FILL_AREA_STYLE_COLOUR ( '', #174788 ) ;
#133377 = CARTESIAN_POINT ( 'NONE',  ( 2.015964598666186269, -0.8597642540715648707, -1.610575774528985704 ) ) ;
#133379 = CARTESIAN_POINT ( 'NONE',  ( -5.822300622425855110, 5.757381912443740646, 0.7998128361456281477 ) ) ;
#133380 = CARTESIAN_POINT ( 'NONE',  ( -0.1296875068447882473, 5.724785194352729256, -2.420566058096422779 ) ) ;
#133381 = CARTESIAN_POINT ( 'NONE',  ( -7.404765023120893019, -6.836271202499959010, -7.949604103952373713 ) ) ;
#133382 = VERTEX_POINT ( 'NONE', #64212 ) ;
#133383 = CARTESIAN_POINT ( 'NONE',  ( -5.275531169048901958, 8.208517892982092334, -1.082531754730549967 ) ) ;
#133384 = CARTESIAN_POINT ( 'NONE',  ( -2.415323921528888196, 5.969628341758991930, 0.7998128361456341429 ) ) ;
#133385 = CARTESIAN_POINT ( 'NONE',  ( -9.267161690140662600, 10.77044237904097734, -1.199719254218441611 ) ) ;
#133386 = CARTESIAN_POINT ( 'NONE',  ( 6.428379779529339366, -0.9538188281377130151, -1.780268319267635846 ) ) ;
#133387 = CARTESIAN_POINT ( 'NONE',  ( 6.428415558115947448, -1.044286553621230240, -1.960546399981792476 ) ) ;
#133388 = CARTESIAN_POINT ( 'NONE',  ( -7.761116589180078407, 8.019333873657032541, 0.000000000000000000 ) ) ;
#133389 = CARTESIAN_POINT ( 'NONE',  ( 5.854423403002611437, 5.724582146458163656, 1.040834085586084257E-14 ) ) ;
#133390 = CARTESIAN_POINT ( 'NONE',  ( 5.436423068491611055, 2.030003055342466389, 0.3545201283375771228 ) ) ;
#133391 = CARTESIAN_POINT ( 'NONE',  ( 4.834611377684539413, 0.6298767044488964295, -1.915599524792414465 ) ) ;
#133392 = VERTEX_POINT ( 'NONE', #79386 ) ;
#133393 = VERTEX_POINT ( 'NONE', #229 ) ;
#133394 =( BOUNDED_SURFACE ( )  B_SPLINE_SURFACE ( 3, 2, ( 
 ( #163438, #15018, #147195 ),
 ( #64850, #164494, #16080 ),
 ( #82163, #34484, #18221 ),
 ( #203367, #84306, #71234 ) ),
 .UNSPECIFIED., .F., .F., .T. ) 
 B_SPLINE_SURFACE_WITH_KNOTS ( ( 4, 4 ),
 ( 3, 3 ),
 ( 8.470329472543003391E-22, 3.124390317667046857E-05 ),
 ( 0.000000000000000000, 1.000000000000000000 ),
 .UNSPECIFIED. ) 
 GEOMETRIC_REPRESENTATION_ITEM ( )  RATIONAL_B_SPLINE_SURFACE ( (
 ( 1.000000000000000000, 0.7071067811860876073, 1.000000000000000000),
 ( 1.000000000000000000, 0.7090998123827956245, 1.000000000000000000),
 ( 1.000000000000000000, 0.7100789167761989429, 1.000000000000000000),
 ( 1.000000000000000000, 0.7100530722022271313, 1.000000000000000000) ) ) 
 REPRESENTATION_ITEM ( '' )  SURFACE ( )  );
#133395 = CARTESIAN_POINT ( 'NONE',  ( 2.901707926954590899, 6.442594886792162967, 0.4081411060850581585 ) ) ;
#133397 = ADVANCED_FACE ( 'NONE', ( #83640 ), #15433, .T. ) ;
#133396 = CARTESIAN_POINT ( 'NONE',  ( -0.2108831679770961642, 2.882544375557041239, -2.385815782126239792 ) ) ;
#133400 = ORIENTED_EDGE ( 'NONE', *, *, #162616, .T. ) ;
#133399 = DIRECTION ( 'NONE',  ( 0.6507913734559641616, -0.7592566023653004592, 0.000000000000000000 ) ) ;
#133398 = CARTESIAN_POINT ( 'NONE',  ( -5.121948170912633991, 9.197632976031879792, -0.7998128361456362523 ) ) ;
#133401 = CARTESIAN_POINT ( 'NONE',  ( 4.783863686166085039, 8.265937597628173705, 0.8363946479656783062 ) ) ;
#133402 = CARTESIAN_POINT ( 'NONE',  ( 5.307970166423544356, -1.730600239375930549, 1.034008556546859969 ) ) ;
#133403 = CARTESIAN_POINT ( 'NONE',  ( 4.699059028873219468, -0.4882365319774860102, 1.775153104902137624 ) ) ;
#133404 = CARTESIAN_POINT ( 'NONE',  ( 10.34545848478754237, -8.336144560139965520, -0.6172425113790489526 ) ) ;
#133405 = CARTESIAN_POINT ( 'NONE',  ( 2.877863741784414842, 2.191074257732894548, -0.7245186886237849899 ) ) ;
#133406 = CARTESIAN_POINT ( 'NONE',  ( 7.191674137406095291, 7.354984346587396082, 0.000000000000000000 ) ) ;
#133407 = CARTESIAN_POINT ( 'NONE',  ( 5.378265110509337532, -1.205767192478784500, 1.793856531414832256 ) ) ;
#133408 = CARTESIAN_POINT ( 'NONE',  ( 5.947222937888848371, 10.09017719417900416, 1.040834085586084257E-14 ) ) ;
#133409 = CARTESIAN_POINT ( 'NONE',  ( 0.1869208759678643028, 1.439853572182720587, 1.303434232916983015 ) ) ;
#133410 = CARTESIAN_POINT ( 'NONE',  ( -3.978428010606240850, 6.728917548094202949, -1.199719254218452047 ) ) ;
#133411 = CARTESIAN_POINT ( 'NONE',  ( 3.937115517079175842, 1.273119805769900026, 1.913412639830965434 ) ) ;
#133412 = CARTESIAN_POINT ( 'NONE',  ( -9.386185638452808178, 15.51845904014325406, -7.476657895053266500 ) ) ;
#133413 = CARTESIAN_POINT ( 'NONE',  ( -4.522526758610270647, 7.433975764090723359, -1.199719254218453823 ) ) ;
#133414 = CARTESIAN_POINT ( 'NONE',  ( 3.906994808788874174, 1.604092888448312326, 0.9621832354540849064 ) ) ;
#133415 = CIRCLE ( 'NONE', #164446, 6.200000000000000178 ) ;
#133418 = CARTESIAN_POINT ( 'NONE',  ( -6.099189001301292379, 8.209082816308541197, 1.599625672291263179 ) ) ;
#133417 = CARTESIAN_POINT ( 'NONE',  ( 1.364683531249988535, 5.655208333674751842, -0.7879004041258300672 ) ) ;
#133416 = CARTESIAN_POINT ( 'NONE',  ( 1.652457426684301955, 1.892030339952909035, 0.2773405859870237133 ) ) ;
#133419 = CARTESIAN_POINT ( 'NONE',  ( 2.772332522587173997, 1.181257105606844160, 1.863944272329665086 ) ) ;
#133420 = CARTESIAN_POINT ( 'NONE',  ( -11.94105721237522921, 10.07259609010266388, 1.187919463087244720 ) ) ;
#133421 = CARTESIAN_POINT ( 'NONE',  ( 5.529027716274630855, 5.344953845275508542, 1.040834085586084257E-14 ) ) ;
#133422 = CARTESIAN_POINT ( 'NONE',  ( 6.156811153937166381, 10.19704708965311468, 0.000000000000000000 ) ) ;
#133423 = CARTESIAN_POINT ( 'NONE',  ( -4.460796234096120472, 5.163016013655583158, 1.199719254218462483 ) ) ;
#133424 = CARTESIAN_POINT ( 'NONE',  ( -7.905812970100109638, 8.396072351304486148, 0.7216878364870317197 ) ) ;
#133425 = CARTESIAN_POINT ( 'NONE',  ( 0.3859243437699639845, -0.9334011365476569955, 1.736406649063494623 ) ) ;
#133426 = CARTESIAN_POINT ( 'NONE',  ( 6.568959576340373197, -2.106780069790818555, -0.9421804820441375128 ) ) ;
#133427 = CARTESIAN_POINT ( 'NONE',  ( 1.803102349535959714, -1.659081995624330563, 1.046767247423967095 ) ) ;
#133428 = CARTESIAN_POINT ( 'NONE',  ( 4.733292769410803125, 0.005207392524877744490, -2.062741129207305235 ) ) ;
#133429 = CARTESIAN_POINT ( 'NONE',  ( 6.643132081016125845, 6.852668304048034287, 0.7216878364870317197 ) ) ;
#133430 = CARTESIAN_POINT ( 'NONE',  ( 4.857564175446106525, 8.889184981320973122, 0.7998128361456331437 ) ) ;
#133431 = ORIENTED_EDGE ( 'NONE', *, *, #6489, .T. ) ;
#133432 = CARTESIAN_POINT ( 'NONE',  ( 7.741342523278705201, 9.094283034322399928, 1.082531754730558626 ) ) ;
#133433 = CARTESIAN_POINT ( 'NONE',  ( -1.001543065824772872E-14, 4.384375000341417916, 1.575800808251672791 ) ) ;
#133434 = DIRECTION ( 'NONE',  ( 1.039099362110107450E-15, 1.000000000000000000, -4.583713267641621330E-32 ) ) ;
#133435 = CARTESIAN_POINT ( 'NONE',  ( 3.999292125906905859, 5.688926785023260102, 1.443375672974062551 ) ) ;
#133436 = CARTESIAN_POINT ( 'NONE',  ( 6.707499178395360140, -1.739742505839674047, -1.298780901186733505 ) ) ;
#133438 =( NAMED_UNIT ( * ) PLANE_ANGLE_UNIT ( ) SI_UNIT ( $, .RADIAN. ) );
#133437 = CARTESIAN_POINT ( 'NONE',  ( 9.620809655836525920, -9.180994456877186849, -0.3503521373105082937 ) ) ;
#133439 = CARTESIAN_POINT ( 'NONE',  ( 5.608800697670862867, 6.153485950588945208, -0.8468207216996347375 ) ) ;
#133440 = CARTESIAN_POINT ( 'NONE',  ( -11.86239285000045918, 12.22000000000000064, -1.812080536912753059 ) ) ;
#133441 = CARTESIAN_POINT ( 'NONE',  ( 1.000990332655056436, 1.525750722454706443, 1.081861512215509524 ) ) ;
#133443 = EDGE_CURVE ( 'NONE', #194084, #37843, #115063, .T. ) ;
#133442 = CARTESIAN_POINT ( 'NONE',  ( -6.116367690567846793, 6.009388118678342217, 0.2715307625813894177 ) ) ;
#133444 =( NAMED_UNIT ( * ) PLANE_ANGLE_UNIT ( ) SI_UNIT ( $, .RADIAN. ) );
#133445 = CARTESIAN_POINT ( 'NONE',  ( 6.127784903196001665, 7.091900248975262500, -1.102264294108054266 ) ) ;
#133446 = CARTESIAN_POINT ( 'NONE',  ( 0.6823417656249899377, 4.988541667008086655, -1.181850606188754593 ) ) ;
#133447 = CARTESIAN_POINT ( 'NONE',  ( 1.506358462150747091, -1.903157483220425883, -0.1863595701613318112 ) ) ;
#133448 = CARTESIAN_POINT ( 'NONE',  ( 2.641160111863867233, -1.309778345111691999, -1.190485388269453049 ) ) ;
#133449 = AXIS2_PLACEMENT_3D ( 'NONE', #194659, #209830, #46303 ) ;
#133450 = CARTESIAN_POINT ( 'NONE',  ( 0.5395309102857149819, -1.815710607404594557, 0.6001554849531522962 ) ) ;
#133452 = CARTESIAN_POINT ( 'NONE',  ( 4.183139505431884508, 1.540756628010631735, 1.138051695910688998 ) ) ;
#133451 = CARTESIAN_POINT ( 'NONE',  ( 1.752543019934815760, -3.157786969197629467, -2.872674334950378938 ) ) ;
#133453 = B_SPLINE_CURVE_WITH_KNOTS ( 'NONE', 3,
 ( #19781, #151938, #57637, #189754, #53359, #119493, #170303 ),
 .UNSPECIFIED., .F., .F.,
 ( 4, 3, 4 ),
 ( 0.000000000000000000, 6.254074696316652595E-05, 0.0001680160826026134415 ),
 .UNSPECIFIED. ) ;
#133454 = CARTESIAN_POINT ( 'NONE',  ( 5.072688767047404568, 1.359683132420253182, -1.425145238552152582 ) ) ;
#133456 = EDGE_CURVE ( 'NONE', #130448, #179867, #36128, .T. ) ;
#133455 = CARTESIAN_POINT ( 'NONE',  ( 0.8793290508635929204, -1.919567575575848339, -0.9014759086384205311 ) ) ;
#133457 = CYLINDRICAL_SURFACE ( 'NONE', #213949, 3.475000000000000089 ) ;
#133458 = CARTESIAN_POINT ( 'NONE',  ( 4.153091690245942047, -1.555063956268587066, -1.039456662654779207 ) ) ;
#133460 = ORIENTED_EDGE ( 'NONE', *, *, #56480, .F. ) ;
#133459 = CARTESIAN_POINT ( 'NONE',  ( 0.1174333910212103232, -1.791171220025630895, 0.3524246893974944395 ) ) ;
#133462 = CARTESIAN_POINT ( 'NONE',  ( -1.201851678989727383E-14, 4.337500000000023448, -1.732050807568863648 ) ) ;
#133461 = CARTESIAN_POINT ( 'NONE',  ( 3.950008152305323428, 0.7444041667201054535, -2.077678867657362538 ) ) ;
#133463 = CARTESIAN_POINT ( 'NONE',  ( 1.364683531249990311, 4.196875000341417028, 1.214306433183764966E-14 ) ) ;
#133464 = CARTESIAN_POINT ( 'NONE',  ( 0.8013246507756426329, -1.769997244335961284, 1.058882903378530749 ) ) ;
#133466 = EDGE_CURVE ( 'NONE', #157711, #55041, #12745, .T. ) ;
#133465 = CARTESIAN_POINT ( 'NONE',  ( 5.587931867126699537, 9.671004278289832001, -0.7998128361456291469 ) ) ;
#133467 = CARTESIAN_POINT ( 'NONE',  ( -9.341731535015849630, 10.85744053139533349, 1.199719254218462483 ) ) ;
#133468 = CARTESIAN_POINT ( 'NONE',  ( -0.4486072944944382579, 15.44705570208638967, -11.94951239051067482 ) ) ;
#133469 = CARTESIAN_POINT ( 'NONE',  ( -3.475000000000000533, 0.000000000000000000, 0.000000000000000000 ) ) ;
#133470 = VECTOR ( 'NONE', #144197, 1000.000000000000114 ) ;
#133471 = CARTESIAN_POINT ( 'NONE',  ( 0.1753634416057497925, 6.947017063990798214, -2.739087685391654148 ) ) ;
#133472 = ORIENTED_EDGE ( 'NONE', *, *, #79797, .F. ) ;
#133473 = CARTESIAN_POINT ( 'NONE',  ( 4.035645461687249913, 1.950487776689105557, -0.6946759356915442885 ) ) ;
#133474 = CARTESIAN_POINT ( 'NONE',  ( 1.499999999999989120, 5.045833333333354709, -0.8660254037844323793 ) ) ;
#133475 = CARTESIAN_POINT ( 'NONE',  ( 1.212450271513715094, -0.9707322288472040039, -1.931405299116680796 ) ) ;
#133476 = CARTESIAN_POINT ( 'NONE',  ( -6.202194133424988820, 6.954874670134298498, -0.8734430727420500196 ) ) ;
#133477 = CARTESIAN_POINT ( 'NONE',  ( 1.541671952839033688, -1.900923180158103021, 0.6826752959473363358 ) ) ;
#133478 = LINE ( 'NONE', #14336, #56328 ) ;
#133479 =( GEOMETRIC_REPRESENTATION_CONTEXT ( 3 ) GLOBAL_UNCERTAINTY_ASSIGNED_CONTEXT ( ( #152796 ) ) GLOBAL_UNIT_ASSIGNED_CONTEXT ( ( #142440, #127313, #177043 ) ) REPRESENTATION_CONTEXT ( 'NONE', 'WORKASPACE' ) );
#133481 = CARTESIAN_POINT ( 'NONE',  ( 9.097157885089661278, 9.715698408800516717, 1.040834085586084257E-14 ) ) ;
#133480 = CARTESIAN_POINT ( 'NONE',  ( 3.475000000000000533, -3.704166666666666163, 2.006292185433948827 ) ) ;
#133482 = CARTESIAN_POINT ( 'NONE',  ( 6.292342264464226176, -1.899326897351862664, 0.6766127494588560776 ) ) ;
#133483 = CARTESIAN_POINT ( 'NONE',  ( -0.08279552664090458758, -1.841734517378278424, 0.8216794407479923734 ) ) ;
#133484 = CARTESIAN_POINT ( 'NONE',  ( 6.639320575229256782, 0.5729255850590134758, 2.155858052613166986 ) ) ;
#133485 = CARTESIAN_POINT ( 'NONE',  ( 4.564136437409766600, -1.431273618155091576, 1.659743667367798103 ) ) ;
#133486 = CARTESIAN_POINT ( 'NONE',  ( -0.7500000000000215383, 2.972916667349487341, 1.299038105676671107 ) ) ;
#133487 = CARTESIAN_POINT ( 'NONE',  ( 3.884940529579200774, -1.786240503712609895, -0.6835825222790415934 ) ) ;
#133488 = CARTESIAN_POINT ( 'NONE',  ( -3.958090780185743451, 6.705190779270287393, -1.199719254218452047 ) ) ;
#133489 = CARTESIAN_POINT ( 'NONE',  ( 4.650083499362875017, 5.487814173087225633, 1.082531754730560403 ) ) ;
#133491 = CARTESIAN_POINT ( 'NONE',  ( 2.144157856786413241, 0.8647422840215597262, 1.821734841475818101 ) ) ;
#133490 = CARTESIAN_POINT ( 'NONE',  ( 0.4465194593917843902, 3.080450244942134486, 0.4155024747329351120 ) ) ;
#133492 = CARTESIAN_POINT ( 'NONE',  ( 1.364683531250000303, 11.81770833367472839, -0.7879004041258355073 ) ) ;
#133494 = CARTESIAN_POINT ( 'NONE',  ( -4.685224601974262271, 7.623789914682047808, -1.199719254218453823 ) ) ;
#133493 = CARTESIAN_POINT ( 'NONE',  ( 0.3458147113889240565, 0.7113776200376471515, -2.179290858394256070 ) ) ;
#133495 = CARTESIAN_POINT ( 'NONE',  ( 4.084733067335220902, -0.1695706708978762522, -1.716391344981627709 ) ) ;
#133496 =( NAMED_UNIT ( * ) PLANE_ANGLE_UNIT ( ) SI_UNIT ( $, .RADIAN. ) );
#133497 = CARTESIAN_POINT ( 'NONE',  ( 3.147464216666835402, 6.823792019419957278, -0.7998128361456291469 ) ) ;
#133498 = CARTESIAN_POINT ( 'NONE',  ( 0.000000000000000000, 15.51845925587262798, 0.000000000000000000 ) ) ;
#133499 = CARTESIAN_POINT ( 'NONE',  ( 1.433958818539453395, 1.165882187713672247, 1.577721859592796205 ) ) ;
#133500 = CARTESIAN_POINT ( 'NONE',  ( 0.000000000000000000, 4.500000000000003553, 0.000000000000000000 ) ) ;
#133501 = CARTESIAN_POINT ( 'NONE',  ( 5.464099601507359516, 6.333536608968757697, 1.199719254218462483 ) ) ;
#133502 = CARTESIAN_POINT ( 'NONE',  ( 0.07536363704233049743, 2.002983476668462881, -2.558365315478607904 ) ) ;
#133503 = ORIENTED_EDGE ( 'NONE', *, *, #157159, .T. ) ;
#133504 = DIRECTION ( 'NONE',  ( 0.7592566023653005702, -0.6507913734559639396, 0.000000000000000000 ) ) ;
#133505 = ORIENTED_EDGE ( 'NONE', *, *, #160202, .F. ) ;
#133506 = CARTESIAN_POINT ( 'NONE',  ( 4.248556108744420357, 1.777317977963272178, 0.3491261437693141123 ) ) ;
#133507 = ORIENTED_EDGE ( 'NONE', *, *, #13805, .T. ) ;
#133508 = CARTESIAN_POINT ( 'NONE',  ( 5.505492895601038938, 8.580769590579979678, -1.199719254218452047 ) ) ;
#133509 = DIRECTION ( 'NONE',  ( 0.000000000000000000, 1.000000000000000000, 0.000000000000000000 ) ) ;
#133510 = CARTESIAN_POINT ( 'NONE',  ( 5.004484103855499910, -1.798449698946352537, -0.2161431223286890690 ) ) ;
#133511 = CARTESIAN_POINT ( 'NONE',  ( 6.577113915960825175, 8.766661883411348555, -1.443375672974078761 ) ) ;
#133512 = CARTESIAN_POINT ( 'NONE',  ( -11.91294103507069480, 9.985399100436019637, -1.446263142085563169 ) ) ;
#133513 = CARTESIAN_POINT ( 'NONE',  ( 4.904330715672160501, 6.657863961833647259, -1.249385787368818113 ) ) ;
#133515 = CARTESIAN_POINT ( 'NONE',  ( 10.40318394038753702, 11.03146944007395724, -0.7998128361456281477 ) ) ;
#133514 = CARTESIAN_POINT ( 'NONE',  ( 6.549252741683062595, 1.618575325784047392, -0.9183544947665848168 ) ) ;
#133516 = CARTESIAN_POINT ( 'NONE',  ( 4.165583994951371771, 1.254247372560507223, 1.447964403467276506 ) ) ;
#133517 = CARTESIAN_POINT ( 'NONE',  ( -6.506163559800210550, -8.203199116536534774, -6.922777049148881368 ) ) ;
#133518 = CARTESIAN_POINT ( 'NONE',  ( -11.30310531956832776, 5.150576456239970291, 5.742040133384030298 ) ) ;
#133519 = CARTESIAN_POINT ( 'NONE',  ( 9.499656837482749694, -9.914216672575010492, -0.08076498840996278183 ) ) ;
#133520 = SURFACE_STYLE_USAGE ( .BOTH. , #67379 ) ;
#133521 = CARTESIAN_POINT ( 'NONE',  ( 5.992340707560151358, 8.014150130285418783, 1.443375672974062551 ) ) ;
#133522 = CARTESIAN_POINT ( 'NONE',  ( -3.789667630219657912, 4.380032642466370696, 1.199719254218462483 ) ) ;
#133523 = CARTESIAN_POINT ( 'NONE',  ( 1.094844843509492183, -0.5259716649698794599, -2.096624219460433647 ) ) ;
#133524 = CARTESIAN_POINT ( 'NONE',  ( -6.296835998904160014, 6.311006518335105397, 0.000000000000000000 ) ) ;
#133525 = CARTESIAN_POINT ( 'NONE',  ( 4.179656494762836516, 8.098292687190454586, -0.7998128361456362523 ) ) ;
#133526 = CARTESIAN_POINT ( 'NONE',  ( 0.7096328715897933792, -1.817275359149352676, 0.1739118742359047065 ) ) ;
#133527 = CARTESIAN_POINT ( 'NONE',  ( -2.754277761870538299, 6.365074488824250309, 1.040834085586084257E-14 ) ) ;
#133528 = CARTESIAN_POINT ( 'NONE',  ( 3.416849837094409370, 1.649954109374281996, 0.7815844185870901573 ) ) ;
#133529 = ADVANCED_FACE ( 'NONE', ( #198448 ), #161721, .T. ) ;
#133530 = FACE_OUTER_BOUND ( 'NONE', #1183, .T. ) ;
#133531 = CARTESIAN_POINT ( 'NONE',  ( 1.722773492080275748, 1.414811824084385661, -1.286832238068566392 ) ) ;
#133532 = ORIENTED_EDGE ( 'NONE', *, *, #40826, .T. ) ;
#133533 = CARTESIAN_POINT ( 'NONE',  ( 2.682036910502568539, -1.131707915740775672, -1.611748346588251168 ) ) ;
#133534 = CARTESIAN_POINT ( 'NONE',  ( 4.968278857500742163, -1.829972417919925265, -0.6506317318197059052 ) ) ;
#133535 = CARTESIAN_POINT ( 'NONE',  ( -3.383641855062333281, 6.105276709951447778, -1.199719254218452047 ) ) ;
#133537 = CARTESIAN_POINT ( 'NONE',  ( 4.078469121099765005, 1.002472831208834680, 1.868716877859360137 ) ) ;
#133536 = CARTESIAN_POINT ( 'NONE',  ( 4.947799714344386146, 4.737130853015369958, -0.7998128361456481317 ) ) ;
#133538 = CARTESIAN_POINT ( 'NONE',  ( -4.496171506534503592, 8.048216686630619066, -2.444650791391935307 ) ) ;
#133539 = CARTESIAN_POINT ( 'NONE',  ( 3.035702773332124238, -1.842316306609870891, 0.5122265333450183311 ) ) ;
#133540 = CARTESIAN_POINT ( 'NONE',  ( 5.943008360174058424, 6.124345481070006869, -0.7360307644482602107 ) ) ;
#133541 = CARTESIAN_POINT ( 'NONE',  ( 0.2331563151865730654, 0.7315591717663977311, -2.029986209603263259 ) ) ;
#133542 = ORIENTED_EDGE ( 'NONE', *, *, #38690, .T. ) ;
#133543 = CARTESIAN_POINT ( 'NONE',  ( 5.252858170651868441, 5.093032385374103299, -0.7998128361456481317 ) ) ;
#133544 = CARTESIAN_POINT ( 'NONE',  ( 3.323720213644492993, 7.029424015893889433, 1.040834085586084257E-14 ) ) ;
#133545 = CARTESIAN_POINT ( 'NONE',  ( 11.94105722165070560, 12.57417237917041142, -1.187919369849492757 ) ) ;
#133546 = CARTESIAN_POINT ( 'NONE',  ( 4.986841741376339066, -0.2268417095559888130, -1.811474396668552700 ) ) ;
#133547 = CARTESIAN_POINT ( 'NONE',  ( 0.02500845152586854067, 3.700502905159954725, -11.79962023279681560 ) ) ;
#133548 = CARTESIAN_POINT ( 'NONE',  ( -8.839552966430007430, 11.33589776563360019, -1.443375672974059665 ) ) ;
#133549 = CARTESIAN_POINT ( 'NONE',  ( -5.939261241470221719, 7.227352081167748743, 1.243796156610659454 ) ) ;
#133550 = FACE_OUTER_BOUND ( 'NONE', #137740, .T. ) ;
#133551 = CARTESIAN_POINT ( 'NONE',  ( 5.840666405660361882, 0.3664468388623157158, 1.834233659845653897 ) ) ;
#133552 = CARTESIAN_POINT ( 'NONE',  ( 6.089583550832340819, 10.25626457594641749, 1.040834085586084257E-14 ) ) ;
#133553 = CARTESIAN_POINT ( 'NONE',  ( -3.764360206088648297, 7.543504007078730922, -0.7998128361456282587 ) ) ;
#133554 = CARTESIAN_POINT ( 'NONE',  ( 3.357615597678655917, 7.068968630600412695, 0.7998128361456321445 ) ) ;
#133555 = CARTESIAN_POINT ( 'NONE',  ( -0.6823417656250003738, 10.71354166700806765, 1.181850606188754593 ) ) ;
#133556 = CARTESIAN_POINT ( 'NONE',  ( -5.656776405399756236, 7.622658444431597680, -1.599625672291256295 ) ) ;
#133557 = CARTESIAN_POINT ( 'NONE',  ( 2.683624340501134853, 5.218313266304903664, -1.199719254218446718 ) ) ;
#133558 = CARTESIAN_POINT ( 'NONE',  ( -5.126391479298592735, 5.153413945369351268, 0.000000000000000000 ) ) ;
#133559 = AXIS2_PLACEMENT_3D ( 'NONE', #91541, #170619, #121962 ) ;
#133560 = CARTESIAN_POINT ( 'NONE',  ( -4.205000198532790279, 8.057583998263570635, 0.7998128361456341429 ) ) ;
#133561 = CARTESIAN_POINT ( 'NONE',  ( 6.737192315218426764, -0.09781360997717462868, -2.168977284074862677 ) ) ;
#133562 = CARTESIAN_POINT ( 'NONE',  ( 0.7380959315415897004, 2.114583753240849795, -0.1084930780173159887 ) ) ;
#133563 = CIRCLE ( 'NONE', #157668, 9.616019636405017224 ) ;
#133564 = CARTESIAN_POINT ( 'NONE',  ( 8.646349277213076334, 11.11049346154719508, 1.599625672291281386 ) ) ;
#133565 = CARTESIAN_POINT ( 'NONE',  ( -5.293864907607930270, 4.747529046662118724, 2.500000000000000444 ) ) ;
#133566 = CARTESIAN_POINT ( 'NONE',  ( 6.543811353064236336, 1.423268159695538326, 1.503672778047180358 ) ) ;
#133568 = CARTESIAN_POINT ( 'NONE',  ( 4.031617349472986334, 7.784614636675013521, 0.3993128758026931457 ) ) ;
#133567 = CARTESIAN_POINT ( 'NONE',  ( 1.153568636672014369, 0.7464410156945017194, 1.683350060182234209 ) ) ;
#133569 = CARTESIAN_POINT ( 'NONE',  ( 4.500943810056890371, 8.194925511800951412, -0.7216878364870207285 ) ) ;
#133571 = CARTESIAN_POINT ( 'NONE',  ( 0.4019237886466884846, 9.707585450998170273, -1.499999999999994449 ) ) ;
#133570 = CYLINDRICAL_SURFACE ( 'NONE', #123328, 1.224999999999996980 ) ;
#133572 = CARTESIAN_POINT ( 'NONE',  ( 1.992491592054939531, -0.6139151001693385901, -2.208460184710277385 ) ) ;
#133575 = EDGE_CURVE ( 'NONE', #78277, #63091, #45662, .T. ) ;
#133574 = CARTESIAN_POINT ( 'NONE',  ( -11.78331023100045627, 13.88000000000000078, -1.800000000000001155 ) ) ;
#133573 = CARTESIAN_POINT ( 'NONE',  ( -1.367741837319783604, 3.300000000000193001, -0.09290545499925643991 ) ) ;
#133576 = VERTEX_POINT ( 'NONE', #45844 ) ;
#133577 = CARTESIAN_POINT ( 'NONE',  ( 7.388830529323379359, 11.56412668427855195, -0.7216878364870267237 ) ) ;
#133578 = EDGE_CURVE ( 'NONE', #121388, #166237, #201857, .T. ) ;
#133579 =( BOUNDED_SURFACE ( )  B_SPLINE_SURFACE ( 1, 2, ( 
 ( #68738, #200867, #83938, #33071, #99149, #35179, #66592, #116507, #169460, #102326, #118645, #166263, #132735, #198739, #101256, #168399, #117579, #151101, #86080, #152155, #3726, #150028, #70863, #185694, #1597, #67658, #2665, #136978, #167339, #133804, #199814, #51458, #18925, #134859, #76231, #141284, #171591, #107740, #170523, #75174, #40548, #206219, #186770, #139111, #25341, #108805, #207293, #24256, #105558, #173764, #92519, #74105, #172679, #23185, #157503, #26407, #205139, #204058, #9098, #208350, #39462, #125076, #8014, #189974, #138045, #90362, #106652, #55711, #140197, #57846, #89300, #142341, #38397, #122949, #5863, #121864, #174829, #124007, #41625, #187835, #88218, #120793, #188908, #91441, #56782, #156428, #58917, #191032, #42699, #104476, #158558, #10156, #154288, #155349, #22106, #71935, #6933, #73013, #126134, #11217, #143411, #109875, #59981, #192095, #27478, #77299, #43761, #175887, #93577, #159623, #115652, #67873, #168609, #37546, #136130, #167548, #34335, #36473, #21266, #2879, #101477, #100410, #86299, #20211, #19148, #166479, #152369, #18071, #198950, #84159, #3947, #103626, #52725, #185912, #1815, #182717, #33273, #70014, #71086, #137203, #102545, #150246, #134019, #200026, #51678, #165409, #50592, #117799, #49528, #183791, #83080, #17005, #116717, #202145, #53806, #169678, #181647, #85222, #35399, #87371, #99358, #119936, #118858, #153441, #68950, #149159, #151311, #135071, #201084, #5013, #737, #184844, #66803, #132945, #189135, #191250, #138268, #154509, #41849, #40774, #106879, #38622, #89524, #42915, #204282, #6090, #107960, #172905, #24480, #104699, #155578, #109025, #73232, #72159, #91671, #76449, #122092, #207514, #90592, #58069, #55939, #156651, #8244, #188056, #74328, #140430, #39685, #10372, #121024, #205369, #88450, #105797, #175044, #206442, #124232, #171820, #170750, #203226, #57004, #190191, #139339, #173987, #25560, #157724, #9319, #186991, #26629, #75393, #22336, #23413, #141505, #59132, #123176, #125291, #7161, #92731, #54870, #158776, #156094, #11953, #41293 ),
 ( #94310, #192829, #9824, #91107, #93244, #78026, #59645, #158233, #157168, #143077, #76952, #75900, #8760, #209070, #74841, #107401, #140941, #60707, #160351, #109545, #28217, #58584, #25005, #90035, #126871, #127952, #193905, #159278, #206955, #124739, #190698, #42359, #7679, #173423, #108471, #106319, #174494, #139858, #73763, #26071, #44487, #110604, #144150, #172343, #142004, #92183, #210142, #23931, #176605, #175549, #61786, #125803, #205889, #208019, #191766, #43421, #57522, #123680, #27138, #10877, #189642, #31422, #16195, #97498, #96445, #148371, #162496, #194977, #14068, #214370, #99608, #48739, #181901, #212273, #178745, #29286, #82276, #67071, #133207, #98546, #146260, #30358, #63908, #80155, #161429, #46613, #47689, #45553, #130064, #79089, #13012, #112735, #66000, #132150, #33536, #111669, #81226, #196057, #165674, #177676, #198156, #114852, #49789, #213334, #95380, #113801, #179803, #163555, #115915, #145207, #15138, #147308, #64959, #131111, #17263, #197098, #211213, #164610, #180852, #32474, #62838, #83339, #149424, #1007, #129000, #87626, #72419, #118058, #203474, #86556, #54062, #2071, #36725, #185098, #134275, #152620, #4207, #35660, #6347, #116983, #201343, #84421, #68142, #187248, #202407, #70275, #200283, #166746, #199211, #52983, #136391, #135329, #102811, #37807, #120197, #103882, #182983, #104960, #186173, #18340, #101739, #168867, #55128, #119119, #169930, #150510, #71343, #50858, #85486, #69209, #171001, #19407, #20470, #34600, #153697, #21514, #5266, #100668, #3139, #137459, #38875, #121273, #22599, #184043, #88706, #154764, #51934, #167808, #151572, #175290, #43168, #126603, #10618, #42097, #123423, #125540, #110342, #91918, #190437, #189385, #26876, #109281, #108212, #41027, #92979, #107137, #73497, #173161, #159025, #192565, #141751, #60445, #90843, #57261, #122353, #76693, #160086, #11688, #191502, #24742, #156906, #8495, #74577, #39952, #139598, #140680, #138520, #206696, #172081, #106059, #205621, #142809, #208813, #44220, #204544, #174235, #58324, #176345, #56192, #27953, #207758 ) ),
 .UNSPECIFIED., .F., .F., .T. ) 
 B_SPLINE_SURFACE_WITH_KNOTS ( ( 2, 2 ),
 ( 3, 2, 2, 2, 2, 2, 2, 2, 2, 2, 2, 2, 2, 2, 2, 2, 2, 2, 2, 2, 2, 2, 2, 2, 2, 2, 2, 2, 2, 2, 2, 2, 2, 2, 2, 2, 2, 2, 2, 2, 2, 2, 2, 2, 2, 2, 2, 2, 2, 2, 2, 2, 2, 2, 2, 2, 2, 2, 2, 2, 2, 2, 2, 2, 2, 2, 2, 2, 2, 2, 2, 2, 2, 2, 2, 2, 2, 2, 2, 2, 2, 2, 2, 2, 2, 2, 2, 2, 2, 2, 2, 2, 2, 2, 2, 2, 2, 2, 2, 2, 2, 2, 2, 2, 2, 2, 2, 2, 2, 2, 2, 2, 2, 2, 2, 2, 2, 2, 2, 2, 3 ),
 ( 0.000000000000000000, 1.000000000000000000 ),
 ( 0.000000000000000000, 0.008333333333333333218, 0.01666666666666666644, 0.02500000000000000139, 0.03333333333333333287, 0.04166666666666666435, 0.05000000000000000278, 0.05833333333333333426, 0.06666666666666666574, 0.07499999999999999722, 0.08333333333333332871, 0.09166666666666666019, 0.1000000000000000056, 0.1083333333333333370, 0.1166666666666666685, 0.1250000000000000000, 0.1333333333333333315, 0.1416666666666666630, 0.1499999999999999944, 0.1583333333333333259, 0.1666666666666666574, 0.1749999999999999889, 0.1833333333333333204, 0.1916666666666666796, 0.2000000000000000111, 0.2083333333333333426, 0.2166666666666666741, 0.2250000000000000056, 0.2333333333333333370, 0.2416666666666666685, 0.2500000000000000000, 0.2583333333333333592, 0.2666666666666666630, 0.2750000000000000222, 0.2833333333333333259, 0.2916666666666666852, 0.2999999999999999889, 0.3083333333333333481, 0.3166666666666666519, 0.3250000000000000111, 0.3333333333333333148, 0.3416666666666666741, 0.3499999999999999778, 0.3583333333333333370, 0.3666666666666666408, 0.3750000000000000000, 0.3833333333333333592, 0.3916666666666666630, 0.4000000000000000222, 0.4083333333333333259, 0.4166666666666666852, 0.4249999999999999889, 0.4333333333333333481, 0.4416666666666666519, 0.4500000000000000111, 0.4583333333333333148, 0.4666666666666666741, 0.4749999999999999778, 0.4833333333333333370, 0.4916666666666666408, 0.5000000000000000000, 0.5083333333333333037, 0.5166666666666667185, 0.5250000000000000222, 0.5333333333333333259, 0.5416666666666666297, 0.5500000000000000444, 0.5583333333333333481, 0.5666666666666666519, 0.5749999999999999556, 0.5833333333333333703, 0.5916666666666666741, 0.5999999999999999778, 0.6083333333333332815, 0.6166666666666666963, 0.6250000000000000000, 0.6333333333333333037, 0.6416666666666667185, 0.6500000000000000222, 0.6583333333333333259, 0.6666666666666666297, 0.6750000000000000444, 0.6833333333333333481, 0.6916666666666666519, 0.6999999999999999556, 0.7083333333333333703, 0.7166666666666666741, 0.7249999999999999778, 0.7333333333333332815, 0.7416666666666666963, 0.7500000000000000000, 0.7583333333333333037, 0.7666666666666667185, 0.7750000000000000222, 0.7833333333333333259, 0.7916666666666666297, 0.8000000000000000444, 0.8083333333333333481, 0.8166666666666666519, 0.8249999999999999556, 0.8333333333333333703, 0.8416666666666666741, 0.8499999999999999778, 0.8583333333333332815, 0.8666666666666666963, 0.8750000000000000000, 0.8833333333333333037, 0.8916666666666667185, 0.9000000000000000222, 0.9083333333333333259, 0.9166666666666666297, 0.9250000000000000444, 0.9333333333333333481, 0.9416666666666666519, 0.9499999999999999556, 0.9583333333333333703, 0.9666666666666666741, 0.9749999999999999778, 0.9833333333333332815, 0.9916666666666666963, 1.000000000000000000 ),
 .UNSPECIFIED. ) 
 GEOMETRIC_REPRESENTATION_ITEM ( )  RATIONAL_B_SPLINE_SURFACE ( (
 ( 1.000000000000000000, 0.8660254037844387076, 1.000000000000000000, 0.8660254037844387076, 1.000000000000000000, 0.8660254037844387076, 1.000000000000000000, 0.8660254037844387076, 1.000000000000000000, 0.8660254037844387076, 1.000000000000000000, 0.8660254037844387076, 1.000000000000000000, 0.8660254037844387076, 1.000000000000000000, 0.8660254037844387076, 1.000000000000000000, 0.8660254037844387076, 1.000000000000000000, 0.8660254037844387076, 1.000000000000000000, 0.8660254037844387076, 1.000000000000000000, 0.8660254037844387076, 1.000000000000000000, 0.8660254037844387076, 1.000000000000000000, 0.8660254037844387076, 1.000000000000000000, 0.8660254037844387076, 1.000000000000000000, 0.8660254037844387076, 1.000000000000000000, 0.8660254037844387076, 1.000000000000000000, 0.8660254037844387076, 1.000000000000000000, 0.8660254037844387076, 1.000000000000000000, 0.8660254037844387076, 1.000000000000000000, 0.8660254037844387076, 1.000000000000000000, 0.8660254037844387076, 1.000000000000000000, 0.8660254037844387076, 1.000000000000000000, 0.8660254037844387076, 1.000000000000000000, 0.8660254037844387076, 1.000000000000000000, 0.8660254037844387076, 1.000000000000000000, 0.8660254037844387076, 1.000000000000000000, 0.8660254037844387076, 1.000000000000000000, 0.8660254037844387076, 1.000000000000000000, 0.8660254037844387076, 1.000000000000000000, 0.8660254037844387076, 1.000000000000000000, 0.8660254037844387076, 1.000000000000000000, 0.8660254037844387076, 1.000000000000000000, 0.8660254037844387076, 1.000000000000000000, 0.8660254037844387076, 1.000000000000000000, 0.8660254037844387076, 1.000000000000000000, 0.8660254037844387076, 1.000000000000000000, 0.8660254037844387076, 1.000000000000000000, 0.8660254037844387076, 1.000000000000000000, 0.8660254037844387076, 1.000000000000000000, 0.8660254037844387076, 1.000000000000000000, 0.8660254037844387076, 1.000000000000000000, 0.8660254037844387076, 1.000000000000000000, 0.8660254037844387076, 1.000000000000000000, 0.8660254037844387076, 1.000000000000000000, 0.8660254037844387076, 1.000000000000000000, 0.8660254037844387076, 1.000000000000000000, 0.8660254037844387076, 1.000000000000000000, 0.8660254037844387076, 1.000000000000000000, 0.8660254037844387076, 1.000000000000000000, 0.8660254037844387076, 1.000000000000000000, 0.8660254037844387076, 1.000000000000000000, 0.8660254037844387076, 1.000000000000000000, 0.8660254037844387076, 1.000000000000000000, 0.8660254037844387076, 1.000000000000000000, 0.8660254037844387076, 1.000000000000000000, 0.8660254037844387076, 1.000000000000000000, 0.8660254037844387076, 1.000000000000000000, 0.8660254037844387076, 1.000000000000000000, 0.8660254037844387076, 1.000000000000000000, 0.8660254037844387076, 1.000000000000000000, 0.8660254037844387076, 1.000000000000000000, 0.8660254037844387076, 1.000000000000000000, 0.8660254037844387076, 1.000000000000000000, 0.8660254037844387076, 1.000000000000000000, 0.8660254037844387076, 1.000000000000000000, 0.8660254037844387076, 1.000000000000000000, 0.8660254037844387076, 1.000000000000000000, 0.8660254037844387076, 1.000000000000000000, 0.8660254037844387076, 1.000000000000000000, 0.8660254037844387076, 1.000000000000000000, 0.8660254037844387076, 1.000000000000000000, 0.8660254037844387076, 1.000000000000000000, 0.8660254037844387076, 1.000000000000000000, 0.8660254037844387076, 1.000000000000000000, 0.8660254037844387076, 1.000000000000000000, 0.8660254037844387076, 1.000000000000000000, 0.8660254037844387076, 1.000000000000000000, 0.8660254037844387076, 1.000000000000000000, 0.8660254037844387076, 1.000000000000000000, 0.8660254037844387076, 1.000000000000000000, 0.8660254037844387076, 1.000000000000000000, 0.8660254037844387076, 1.000000000000000000, 0.8660254037844387076, 1.000000000000000000, 0.8660254037844387076, 1.000000000000000000, 0.8660254037844387076, 1.000000000000000000, 0.8660254037844387076, 1.000000000000000000, 0.8660254037844387076, 1.000000000000000000, 0.8660254037844387076, 1.000000000000000000, 0.8660254037844387076, 1.000000000000000000, 0.8660254037844387076, 1.000000000000000000, 0.8660254037844387076, 1.000000000000000000, 0.8660254037844387076, 1.000000000000000000, 0.8660254037844387076, 1.000000000000000000, 0.8660254037844387076, 1.000000000000000000, 0.8660254037844387076, 1.000000000000000000, 0.8660254037844387076, 1.000000000000000000, 0.8660254037844387076, 1.000000000000000000, 0.8660254037844387076, 1.000000000000000000, 0.8660254037844387076, 1.000000000000000000, 0.8660254037844387076, 1.000000000000000000, 0.8660254037844387076, 1.000000000000000000, 0.8660254037844387076, 1.000000000000000000, 0.8660254037844387076, 1.000000000000000000, 0.8660254037844387076, 1.000000000000000000, 0.8660254037844387076, 1.000000000000000000, 0.8660254037844387076, 1.000000000000000000, 0.8660254037844387076, 1.000000000000000000, 0.8660254037844387076, 1.000000000000000000, 0.8660254037844387076, 1.000000000000000000, 0.8660254037844387076, 1.000000000000000000, 0.8660254037844387076, 1.000000000000000000, 0.8660254037844387076, 1.000000000000000000, 0.8660254037844387076, 1.000000000000000000, 0.8660254037844387076, 1.000000000000000000, 0.8660254037844387076, 1.000000000000000000, 0.8660254037844387076, 1.000000000000000000, 0.8660254037844387076, 1.000000000000000000, 0.8660254037844387076, 1.000000000000000000, 0.8660254037844387076, 1.000000000000000000),
 ( 1.000000000000000000, 0.8660254037844387076, 1.000000000000000000, 0.8660254037844387076, 1.000000000000000000, 0.8660254037844387076, 1.000000000000000000, 0.8660254037844387076, 1.000000000000000000, 0.8660254037844387076, 1.000000000000000000, 0.8660254037844387076, 1.000000000000000000, 0.8660254037844387076, 1.000000000000000000, 0.8660254037844387076, 1.000000000000000000, 0.8660254037844387076, 1.000000000000000000, 0.8660254037844387076, 1.000000000000000000, 0.8660254037844387076, 1.000000000000000000, 0.8660254037844387076, 1.000000000000000000, 0.8660254037844387076, 1.000000000000000000, 0.8660254037844387076, 1.000000000000000000, 0.8660254037844387076, 1.000000000000000000, 0.8660254037844387076, 1.000000000000000000, 0.8660254037844387076, 1.000000000000000000, 0.8660254037844387076, 1.000000000000000000, 0.8660254037844387076, 1.000000000000000000, 0.8660254037844387076, 1.000000000000000000, 0.8660254037844387076, 1.000000000000000000, 0.8660254037844387076, 1.000000000000000000, 0.8660254037844387076, 1.000000000000000000, 0.8660254037844387076, 1.000000000000000000, 0.8660254037844387076, 1.000000000000000000, 0.8660254037844387076, 1.000000000000000000, 0.8660254037844387076, 1.000000000000000000, 0.8660254037844387076, 1.000000000000000000, 0.8660254037844387076, 1.000000000000000000, 0.8660254037844387076, 1.000000000000000000, 0.8660254037844387076, 1.000000000000000000, 0.8660254037844387076, 1.000000000000000000, 0.8660254037844387076, 1.000000000000000000, 0.8660254037844387076, 1.000000000000000000, 0.8660254037844387076, 1.000000000000000000, 0.8660254037844387076, 1.000000000000000000, 0.8660254037844387076, 1.000000000000000000, 0.8660254037844387076, 1.000000000000000000, 0.8660254037844387076, 1.000000000000000000, 0.8660254037844387076, 1.000000000000000000, 0.8660254037844387076, 1.000000000000000000, 0.8660254037844387076, 1.000000000000000000, 0.8660254037844387076, 1.000000000000000000, 0.8660254037844387076, 1.000000000000000000, 0.8660254037844387076, 1.000000000000000000, 0.8660254037844387076, 1.000000000000000000, 0.8660254037844387076, 1.000000000000000000, 0.8660254037844387076, 1.000000000000000000, 0.8660254037844387076, 1.000000000000000000, 0.8660254037844387076, 1.000000000000000000, 0.8660254037844387076, 1.000000000000000000, 0.8660254037844387076, 1.000000000000000000, 0.8660254037844387076, 1.000000000000000000, 0.8660254037844387076, 1.000000000000000000, 0.8660254037844387076, 1.000000000000000000, 0.8660254037844387076, 1.000000000000000000, 0.8660254037844387076, 1.000000000000000000, 0.8660254037844387076, 1.000000000000000000, 0.8660254037844387076, 1.000000000000000000, 0.8660254037844387076, 1.000000000000000000, 0.8660254037844387076, 1.000000000000000000, 0.8660254037844387076, 1.000000000000000000, 0.8660254037844387076, 1.000000000000000000, 0.8660254037844387076, 1.000000000000000000, 0.8660254037844387076, 1.000000000000000000, 0.8660254037844387076, 1.000000000000000000, 0.8660254037844387076, 1.000000000000000000, 0.8660254037844387076, 1.000000000000000000, 0.8660254037844387076, 1.000000000000000000, 0.8660254037844387076, 1.000000000000000000, 0.8660254037844387076, 1.000000000000000000, 0.8660254037844387076, 1.000000000000000000, 0.8660254037844387076, 1.000000000000000000, 0.8660254037844387076, 1.000000000000000000, 0.8660254037844387076, 1.000000000000000000, 0.8660254037844387076, 1.000000000000000000, 0.8660254037844387076, 1.000000000000000000, 0.8660254037844387076, 1.000000000000000000, 0.8660254037844387076, 1.000000000000000000, 0.8660254037844387076, 1.000000000000000000, 0.8660254037844387076, 1.000000000000000000, 0.8660254037844387076, 1.000000000000000000, 0.8660254037844387076, 1.000000000000000000, 0.8660254037844387076, 1.000000000000000000, 0.8660254037844387076, 1.000000000000000000, 0.8660254037844387076, 1.000000000000000000, 0.8660254037844387076, 1.000000000000000000, 0.8660254037844387076, 1.000000000000000000, 0.8660254037844387076, 1.000000000000000000, 0.8660254037844387076, 1.000000000000000000, 0.8660254037844387076, 1.000000000000000000, 0.8660254037844387076, 1.000000000000000000, 0.8660254037844387076, 1.000000000000000000, 0.8660254037844387076, 1.000000000000000000, 0.8660254037844387076, 1.000000000000000000, 0.8660254037844387076, 1.000000000000000000, 0.8660254037844387076, 1.000000000000000000, 0.8660254037844387076, 1.000000000000000000, 0.8660254037844387076, 1.000000000000000000, 0.8660254037844387076, 1.000000000000000000, 0.8660254037844387076, 1.000000000000000000, 0.8660254037844387076, 1.000000000000000000, 0.8660254037844387076, 1.000000000000000000, 0.8660254037844387076, 1.000000000000000000, 0.8660254037844387076, 1.000000000000000000, 0.8660254037844387076, 1.000000000000000000, 0.8660254037844387076, 1.000000000000000000, 0.8660254037844387076, 1.000000000000000000, 0.8660254037844387076, 1.000000000000000000, 0.8660254037844387076, 1.000000000000000000, 0.8660254037844387076, 1.000000000000000000, 0.8660254037844387076, 1.000000000000000000, 0.8660254037844387076, 1.000000000000000000, 0.8660254037844387076, 1.000000000000000000, 0.8660254037844387076, 1.000000000000000000, 0.8660254037844387076, 1.000000000000000000, 0.8660254037844387076, 1.000000000000000000, 0.8660254037844387076, 1.000000000000000000, 0.8660254037844387076, 1.000000000000000000, 0.8660254037844387076, 1.000000000000000000) ) ) 
 REPRESENTATION_ITEM ( '' )  SURFACE ( )  );
#133580 = CARTESIAN_POINT ( 'NONE',  ( 0.7561087546162044148, 0.8121304633340595824, -1.842289638184602341 ) ) ;
#133581 = CARTESIAN_POINT ( 'NONE',  ( 1.569116724355507975, 1.727593668635756918, 0.9295332132536607839 ) ) ;
#133582 = CARTESIAN_POINT ( 'NONE',  ( -6.014495906177975471, 7.161312607523874441, -1.265080238494860509 ) ) ;
#133584 = CARTESIAN_POINT ( 'NONE',  ( -10.87107728089202752, 4.495199002972934288, -4.557510466808897043 ) ) ;
#133583 = CARTESIAN_POINT ( 'NONE',  ( -8.688077508258798431, 9.030511935923748013, -0.7998128361456291469 ) ) ;
#133585 = CARTESIAN_POINT ( 'NONE',  ( -3.285556943750000070, -0.5468749995220407722, 0.000000000000000000 ) ) ;
#133587 = CARTESIAN_POINT ( 'NONE',  ( 1.920411955722916453, 1.650032497218676397, 0.6405850872945593188 ) ) ;
#133586 = CARTESIAN_POINT ( 'NONE',  ( 3.943374907373353278, 0.7044166278388838132, -1.968527102906494575 ) ) ;
#133588 = CARTESIAN_POINT ( 'NONE',  ( -10.91255906795571562, 3.426985321572576737, 3.952372590954746023 ) ) ;
#133590 = CARTESIAN_POINT ( 'NONE',  ( 5.209026396049201146, -0.3404489335739938061, 2.266724491853837620 ) ) ;
#133589 = CARTESIAN_POINT ( 'NONE',  ( 2.280903940472752467, 5.594607745005274246, -0.6109567437776646237 ) ) ;
#133591 = CARTESIAN_POINT ( 'NONE',  ( 3.732115773437282513, 0.2573812008909857618, 1.721053547986243215 ) ) ;
#133592 = CARTESIAN_POINT ( 'NONE',  ( 10.53876547652418338, 11.18964789890005918, 0.7998128361456462443 ) ) ;
#133593 = CARTESIAN_POINT ( 'NONE',  ( 2.829097238278361459, -1.198370081129100262, 1.253277946039689450 ) ) ;
#133594 = CARTESIAN_POINT ( 'NONE',  ( 3.244746832269917558, -2.138594630188391132, -0.3739374351436116073 ) ) ;
#133595 = CARTESIAN_POINT ( 'NONE',  ( 3.486418057008484617, 7.219238166485217434, 1.040834085586084257E-14 ) ) ;
#133596 = CARTESIAN_POINT ( 'NONE',  ( 6.016814611094169152, 0.2024578496369993375, 2.006372135924570088 ) ) ;
#133598 = VECTOR ( 'NONE', #78771, 1000.000000000000000 ) ;
#133597 = CARTESIAN_POINT ( 'NONE',  ( 0.01034996896555614825, -0.2601230917365888740, -1.999999999999999556 ) ) ;
#133599 = CARTESIAN_POINT ( 'NONE',  ( -1.001543065824772872E-14, 4.243750000682819490, 1.732050807568877637 ) ) ;
#133600 = CARTESIAN_POINT ( 'NONE',  ( 2.080962409574789174, -0.09239518442967499523, -1.924287757472051164 ) ) ;
#133601 = CARTESIAN_POINT ( 'NONE',  ( -1.500000000000015099, 9.010416667349463893, -0.8660254037844309360 ) ) ;
#133602 = CARTESIAN_POINT ( 'NONE',  ( 5.185853984360066171, 2.140751028750527141, -0.5928278168529849124 ) ) ;
#133603 = ORIENTED_EDGE ( 'NONE', *, *, #8484, .T. ) ;
#133604 = CARTESIAN_POINT ( 'NONE',  ( -0.2106854629475244378, 6.948332279000682732, -2.592197477433130448 ) ) ;
#133605 = CARTESIAN_POINT ( 'NONE',  ( -1.500000000000013101, 2.379166666666686414, -0.8660254037844313801 ) ) ;
#133606 = CARTESIAN_POINT ( 'NONE',  ( 5.774883364416965037, 8.824782127540085952, -1.199719254218440723 ) ) ;
#133607 = CARTESIAN_POINT ( 'NONE',  ( 5.300874872818840622, 6.247070775452521652, 1.082531754730560403 ) ) ;
#133608 = CARTESIAN_POINT ( 'NONE',  ( 3.285556943750000070, -2.034374999522043481, 0.000000000000000000 ) ) ;
#133610 = CARTESIAN_POINT ( 'NONE',  ( -1.499999999999990896, 4.879166666666689522, -0.8660254037844429265 ) ) ;
#133609 = CIRCLE ( 'NONE', #178733, 2.025000000000006573 ) ;
#133611 = CARTESIAN_POINT ( 'NONE',  ( 7.443063144222396232, 11.62739806832741785, 1.040834085586084257E-14 ) ) ;
#133612 = FILL_AREA_STYLE_COLOUR ( '', #104215 ) ;
#133613 = CARTESIAN_POINT ( 'NONE',  ( 6.696538538688765918, -0.5935452916538739299, -2.183133895321730744 ) ) ;
#133615 = EDGE_CURVE ( 'NONE', #179285, #51499, #146089, .T. ) ;
#133614 = CIRCLE ( 'NONE', #19299, 0.07999999999999975187 ) ;
#133616 = CARTESIAN_POINT ( 'NONE',  ( 5.890091390494168522, 5.836471141856793388, 0.000000000000000000 ) ) ;
#133617 = CARTESIAN_POINT ( 'NONE',  ( -0.1399997263889594112, -0.002789056014654289761, -2.000146600338557956 ) ) ;
#133618 = CARTESIAN_POINT ( 'NONE',  ( 3.982923569253065121, 1.957725435881779941, 0.6497275974019289801 ) ) ;
#133619 = CARTESIAN_POINT ( 'NONE',  ( -5.066996723205291708, 6.934582148538044777, 1.599625672291267398 ) ) ;
#133620 = CARTESIAN_POINT ( 'NONE',  ( -1.500000000000011324, 4.452083334016148086, 0.8660254037844403729 ) ) ;
#133621 = CARTESIAN_POINT ( 'NONE',  ( -0.6823417656250003738, 0.2177083336747515085, -1.181850606188749264 ) ) ;
#133622 = CARTESIAN_POINT ( 'NONE',  ( 5.395714598229544023, -0.6742385858747660388, 1.744967798948720228 ) ) ;
#133623 = CARTESIAN_POINT ( 'NONE',  ( 5.203642376314169482, 1.605325691485876671, 0.6564576239363513199 ) ) ;
#133624 = CARTESIAN_POINT ( 'NONE',  ( 4.634162599488286460, 0.3036646131651790093, 1.713576892981442557 ) ) ;
#133625 = CARTESIAN_POINT ( 'NONE',  ( 4.467575310902914154, 5.170924936596891008, 1.199719254218464037 ) ) ;
#133626 = CARTESIAN_POINT ( 'NONE',  ( 1.347684858569838440, 0.6597076516901092536, -2.195415608770342253 ) ) ;
#133627 = CARTESIAN_POINT ( 'NONE',  ( -1.364683531250010295, 5.092708333674757171, 0.7879004041258379498 ) ) ;
#133628 = CARTESIAN_POINT ( 'NONE',  ( 5.794497793856321799, 1.708647746284063684, -1.204582154990775811 ) ) ;
#133629 = CARTESIAN_POINT ( 'NONE',  ( 0.1461044202776436429, -1.480667811789614596, 1.094048858351577724 ) ) ;
#133630 = CIRCLE ( 'NONE', #188927, 1.250000000000000222 ) ;
#133631 = DIRECTION ( 'NONE',  ( 0.000000000000000000, 1.000000000000000000, -0.000000000000000000 ) ) ;
#133632 = CARTESIAN_POINT ( 'NONE',  ( 1.652970434142877920, 1.038994816082598804, 1.728001345923817267 ) ) ;
#133633 = CARTESIAN_POINT ( 'NONE',  ( 0.6213436022244858137, -2.079703760468250451, 0.6910661131078954522 ) ) ;
#133634 = CARTESIAN_POINT ( 'NONE',  ( 7.440075190158704110, 14.00000000000000000, -10.26883734974634166 ) ) ;
#133635 = CARTESIAN_POINT ( 'NONE',  ( -7.609150525767646833, 9.900428251527500834, -1.599625672291263179 ) ) ;
#133636 = CARTESIAN_POINT ( 'NONE',  ( 5.656776405399742025, 7.622658444431597680, -1.599625672291262513 ) ) ;
#133637 = CARTESIAN_POINT ( 'NONE',  ( -1.360316468750013108, 1.390625000341414008, -3.469446951953614189E-15 ) ) ;
#133638 = CARTESIAN_POINT ( 'NONE',  ( 3.598385148150527346, -1.043669326629501848, 1.845773325594574077 ) ) ;
#133639 = CARTESIAN_POINT ( 'NONE',  ( -0.6823417656250246877, -0.6989583329919113464, 1.181850606188755259 ) ) ;
#133640 = CARTESIAN_POINT ( 'NONE',  ( 5.426323838365306074, 1.084245000580752238, -1.468710674947353967 ) ) ;
#133641 = VERTEX_POINT ( 'NONE', #22889 ) ;
#133642 = CARTESIAN_POINT ( 'NONE',  ( -6.526270840131767059, 8.707344961610770540, -1.599625672291271394 ) ) ;
#133643 = CARTESIAN_POINT ( 'NONE',  ( 1.467871227757891193E-11, -3.138498625356828775, -3.379301813585260383 ) ) ;
#133645 = EDGE_CURVE ( 'NONE', #151754, #5447, #167045, .T. ) ;
#133644 = CARTESIAN_POINT ( 'NONE',  ( 6.658462837642791676, 8.861568958707010779, 1.443375672974063439 ) ) ;
#133646 = CARTESIAN_POINT ( 'NONE',  ( -3.474999999999998312, -2.377083332377420088, 2.006292185433951047 ) ) ;
#133647 = CARTESIAN_POINT ( 'NONE',  ( -6.501298352952815662, 7.543601818988450169, -1.199719254218446718 ) ) ;
#133648 = CARTESIAN_POINT ( 'NONE',  ( 2.900653795123844692, -1.990604234199357281, -0.3410580241900613707 ) ) ;
#133649 = CARTESIAN_POINT ( 'NONE',  ( 6.528370574810466564, 1.275976099532463381, -1.800301716031265764 ) ) ;
#133650 = CARTESIAN_POINT ( 'NONE',  ( 10.21336978979620191, 10.81001959771741205, 0.7998128361456462443 ) ) ;
#133651 = CARTESIAN_POINT ( 'NONE',  ( 3.713571355222999415, 0.4562380391235145161, -1.803994140785330602 ) ) ;
#133652 = CARTESIAN_POINT ( 'NONE',  ( 10.24048609702354717, 10.84165528948263457, -0.7998128361456281477 ) ) ;
#133653 = CARTESIAN_POINT ( 'NONE',  ( 3.146123468421266001, 6.442327133617253843, 0.5169845646841256803 ) ) ;
#133654 = CARTESIAN_POINT ( 'NONE',  ( -3.684065054611367351, 5.321161868511784299, -1.599625672291256295 ) ) ;
#133655 = CARTESIAN_POINT ( 'NONE',  ( -8.355902744723985975, 8.642974711799791265, 1.040834085586084257E-14 ) ) ;
#133657 = CARTESIAN_POINT ( 'NONE',  ( -4.712061673757400371, 7.041017223283659199, 1.411098259540758182 ) ) ;
#133656 = CARTESIAN_POINT ( 'NONE',  ( -6.668631453075260396, 8.873432343378178544, -1.599625672291271394 ) ) ;
#133658 = CARTESIAN_POINT ( 'NONE',  ( 0.6823417656249882723, -0.4072916663252490466, 1.181850606188755259 ) ) ;
#133659 = CARTESIAN_POINT ( 'NONE',  ( 1.739138385086140159, -1.644397438216003593, -0.5498640316261136363 ) ) ;
#133660 = CARTESIAN_POINT ( 'NONE',  ( 0.9721243863554385189, -0.03892262269361351779, -1.740072766964487316 ) ) ;
#133662 = CARTESIAN_POINT ( 'NONE',  ( 7.537970219518073556, 9.817384560903001045, -1.443375672974057666 ) ) ;
#133661 = CARTESIAN_POINT ( 'NONE',  ( 0.07775346131144458828, -0.005211914751935413023, -2.288974916015192651 ) ) ;
#133663 = CARTESIAN_POINT ( 'NONE',  ( 4.913904330310220558, 4.697586238308844919, 0.000000000000000000 ) ) ;
#133664 = CARTESIAN_POINT ( 'NONE',  ( 0.9485937975238111219, 0.5957422345228384764, 1.972812641012058776 ) ) ;
#133665 = CARTESIAN_POINT ( 'NONE',  ( 5.331380718671758778, 7.243030143248949670, -1.599625672291256295 ) ) ;
#133666 = CARTESIAN_POINT ( 'NONE',  ( 6.573571087534610058, 1.710132712828818402, -1.535791079811721360 ) ) ;
#133667 = CARTESIAN_POINT ( 'NONE',  ( 0.000000000000000000, -1.500000000000001332, 0.000000000000000000 ) ) ;
#133668 = CARTESIAN_POINT ( 'NONE',  ( -3.935609729716867289, 7.813571461303467913, 0.7998128361456352531 ) ) ;
#133669 = CARTESIAN_POINT ( 'NONE',  ( 0.3562423511419475775, 0.7522458758148011793, 1.822497947957350428 ) ) ;
#133671 = CARTESIAN_POINT ( 'NONE',  ( -5.790741006812557323, 9.769965251341050205, 0.000000000000000000 ) ) ;
#133670 = CARTESIAN_POINT ( 'NONE',  ( 4.341997288149157086, -1.180789491531178292, -1.504210074635865757 ) ) ;
#133672 = CARTESIAN_POINT ( 'NONE',  ( 6.182275136424624229, -1.184133725572718676, 1.862117674348878760 ) ) ;
#133673 = CARTESIAN_POINT ( 'NONE',  ( -0.3000000000000241918, 4.000000000000003553, -1.007084189318394385 ) ) ;
#133674 = CARTESIAN_POINT ( 'NONE',  ( 3.065552130021340194, 6.590578228417936835, 0.000000000000000000 ) ) ;
#133675 = CARTESIAN_POINT ( 'NONE',  ( -8.120407659942227241, 8.438506789546210030, 0.7998128361456341429 ) ) ;
#133676 = CARTESIAN_POINT ( 'NONE',  ( -0.005205762187880831615, -1.959593580757122089, -0.4885912094437401820 ) ) ;
#133677 = ORIENTED_EDGE ( 'NONE', *, *, #173872, .F. ) ;
#133678 = CARTESIAN_POINT ( 'NONE',  ( 3.206425952641503319, -2.304998342715250281, 0.1115464655990650450 ) ) ;
#133679 = CARTESIAN_POINT ( 'NONE',  ( 5.178158156489047315, -1.047961880893449882, -1.658324637040713867 ) ) ;
#133680 = CARTESIAN_POINT ( 'NONE',  ( 0.8308171121041010299, -1.845250773774274267, -0.6662997747023179373 ) ) ;
#133681 = DIRECTION ( 'NONE',  ( -1.000000000000000000, 0.000000000000000000, 1.224646799147353207E-16 ) ) ;
#133682 = CARTESIAN_POINT ( 'NONE',  ( -9.417400626923768669, 15.36186642319061413, 7.338645109549106316 ) ) ;
#133683 = ORIENTED_EDGE ( 'NONE', *, *, #52222, .F. ) ;
#133684 = CARTESIAN_POINT ( 'NONE',  ( -0.2408018239684434625, -0.007136184528846663787, -2.100252307185761058 ) ) ;
#133686 = CARTESIAN_POINT ( 'NONE',  ( -7.160677686311960777, 11.50587440067263678, -0.7998128361456291469 ) ) ;
#133685 = CARTESIAN_POINT ( 'NONE',  ( -5.220052836461385404, 6.048815383081766583, -1.199719254218446718 ) ) ;
#133687 = FACE_OUTER_BOUND ( 'NONE', #118418, .T. ) ;
#133689 =( GEOMETRIC_REPRESENTATION_CONTEXT ( 3 ) GLOBAL_UNCERTAINTY_ASSIGNED_CONTEXT ( ( #164225 ) ) GLOBAL_UNIT_ASSIGNED_CONTEXT ( ( #31959, #15678, #65485 ) ) REPRESENTATION_CONTEXT ( 'NONE', 'WORKASPACE' ) );
#133688 = CARTESIAN_POINT ( 'NONE',  ( 4.610331778354775700, 2.170709972759849116, -0.04705437256473897489 ) ) ;
#133690 = CARTESIAN_POINT ( 'NONE',  ( -0.001447835942344739097, 2.586556732995649366, 2.083545908858529749 ) ) ;
#133691 = CARTESIAN_POINT ( 'NONE',  ( 1.512141599020993432, -0.7094941370262074498, 1.998545949238240027 ) ) ;
#133692 = CARTESIAN_POINT ( 'NONE',  ( -1.201851678989727383E-14, 3.118750000682814161, -1.732050807568863648 ) ) ;
#133693 = CARTESIAN_POINT ( 'NONE',  ( 7.865701674222579598, 12.32840238656838139, -0.7998128361456352531 ) ) ;
#133694 = CARTESIAN_POINT ( 'NONE',  ( 0.1054570145121072472, 2.614151819895196738, -2.076146791065091701 ) ) ;
#133695 = CARTESIAN_POINT ( 'NONE',  ( 6.246047416222394233, 7.008439898793222156, -0.9866338212708870570 ) ) ;
#133696 = CARTESIAN_POINT ( 'NONE',  ( 1.932957488262206480, 0.1987776095667900533, 2.051143708757536821 ) ) ;
#133698 = CARTESIAN_POINT ( 'NONE',  ( 6.609000000000038177, 0.002801690667396730672, 2.000160786441218530 ) ) ;
#133697 = CARTESIAN_POINT ( 'NONE',  ( -9.124801077197171040, 10.60435499727357289, -1.199719254218441611 ) ) ;
#133699 = CARTESIAN_POINT ( 'NONE',  ( -0.6823417656250003738, 2.217708333674753174, -1.181850606188749264 ) ) ;
#133700 = CARTESIAN_POINT ( 'NONE',  ( -1.500000000000015099, 9.229166666666667851, -0.8660254037844309360 ) ) ;
#133701 = CARTESIAN_POINT ( 'NONE',  ( 5.558836782162523527, 7.518240855878357110, -1.384758111419038817 ) ) ;
#133702 = ORIENTED_EDGE ( 'NONE', *, *, #193910, .F. ) ;
#133703 = CARTESIAN_POINT ( 'NONE',  ( 4.143145976665215002, 0.09703654569752531711, 1.909951782607082427 ) ) ;
#133704 = CARTESIAN_POINT ( 'NONE',  ( 11.84668730067608600, 10.19999999999998153, 1.399999999999998579 ) ) ;
#133705 = CARTESIAN_POINT ( 'NONE',  ( 1.300488321244117618, -2.262578820359177012, 9.798025588786393801E-05 ) ) ;
#133706 = CARTESIAN_POINT ( 'NONE',  ( -2.764973262183167968, 5.313220341600567664, 1.199719254218462483 ) ) ;
#133707 = CARTESIAN_POINT ( 'NONE',  ( 1.705023097204850346, 1.575028893885391579, -0.8949447657340557916 ) ) ;
#133708 = CARTESIAN_POINT ( 'NONE',  ( 0.4795166263942132745, -0.6867406401212177158, 1.788596380544268616 ) ) ;
#133709 = CARTESIAN_POINT ( 'NONE',  ( 2.049362625460974030, 1.802418521853879962, -1.018503948505583789 ) ) ;
#133710 = CARTESIAN_POINT ( 'NONE',  ( -1.402160292154681736E-14, 1.259375000341419248, -1.575800808251659024 ) ) ;
#133711 = ADVANCED_FACE ( 'NONE', ( #100955 ), #19707, .T. ) ;
#133712 = CARTESIAN_POINT ( 'NONE',  ( 0.1804621682222322943, -1.911711055282316662, -0.4813082943134691094 ) ) ;
#133713 = CARTESIAN_POINT ( 'NONE',  ( 5.461526653864938297, 0.3736970969714300539, -1.889748759083320406 ) ) ;
#133715 = CARTESIAN_POINT ( 'NONE',  ( 5.441225816562971218, 7.512442699629209741, -1.249814574298679926 ) ) ;
#133714 = CARTESIAN_POINT ( 'NONE',  ( 6.428370569364434850, 1.274405893209800356, -1.801548588985131039 ) ) ;
#133716 = CARTESIAN_POINT ( 'NONE',  ( 1.364683531249988535, 2.113541667008087099, 0.7879004041258500513 ) ) ;
#133717 = AXIS2_PLACEMENT_3D ( 'NONE', #66257, #17515, #83602 ) ;
#133718 = CARTESIAN_POINT ( 'NONE',  ( 4.791499389596598490, -1.887151845835168817, 0.8330235203531827226 ) ) ;
#133719 = CARTESIAN_POINT ( 'NONE',  ( -6.901263884555985051, 8.010228272525461435, 1.199719254218450271 ) ) ;
#133720 = CARTESIAN_POINT ( 'NONE',  ( 7.564559641420864899, 10.91273778404466199, -1.199719254218446718 ) ) ;
#133721 = CARTESIAN_POINT ( 'NONE',  ( -1.177110729581227089, 2.870878374463987193, 0.7750000000000083489 ) ) ;
#133723 = CARTESIAN_POINT ( 'NONE',  ( -1.499999999999997780, 3.400000000000021227, 1.214306433183764966E-14 ) ) ;
#133722 = CARTESIAN_POINT ( 'NONE',  ( 5.280345248378272238, -1.172444710293341963, 1.749198092158671614 ) ) ;
#133724 = CARTESIAN_POINT ( 'NONE',  ( 1.065148145857688577, 1.644283457976392748, -1.417989991454001730 ) ) ;
#133725 = CARTESIAN_POINT ( 'NONE',  ( -1.201851678989727383E-14, 2.134375000341423689, 1.575800808251672791 ) ) ;
#133726 = CARTESIAN_POINT ( 'NONE',  ( 5.149776166300943814, 0.6834882490109328579, -2.050742609271530181 ) ) ;
#133727 = CARTESIAN_POINT ( 'NONE',  ( 4.881513094923572105, 0.1956549798781386795, -2.010156034525738988 ) ) ;
#133728 = LINE ( 'NONE', #101174, #184335 ) ;
#133729 = ADVANCED_FACE ( 'NONE', ( #54361 ), #102039, .F. ) ;
#133732 = CARTESIAN_POINT ( 'NONE',  ( 6.182154858151487353, 6.314861544039274577, -0.7216878364870257245 ) ) ;
#133731 = CARTESIAN_POINT ( 'NONE',  ( 3.285556943749998737, -1.655208332855374609, -1.896917185911906500 ) ) ;
#133730 = CARTESIAN_POINT ( 'NONE',  ( 7.472478939787284169, 8.746922180287201698, 1.199719254218452935 ) ) ;
#133733 = CARTESIAN_POINT ( 'NONE',  ( -5.010620288702242853, 8.003418215864698482, -1.199719254218453823 ) ) ;
#133734 = CARTESIAN_POINT ( 'NONE',  ( 3.063685658700274761, 1.282989771343697294, 1.555699169480361022 ) ) ;
#133735 = CARTESIAN_POINT ( 'NONE',  ( -9.528683032306089373, 10.01121838064558744, 0.7998128361456462443 ) ) ;
#133737 = SURFACE_STYLE_USAGE ( .BOTH. , #115382 ) ;
#133736 = CARTESIAN_POINT ( 'NONE',  ( -8.500599126088349777, 12.86119004717103209, 1.040834085586084257E-14 ) ) ;
#133739 = CARTESIAN_POINT ( 'NONE',  ( -0.6823417656250003738, 8.401041667008064096, 1.181850606188754593 ) ) ;
#133738 = CARTESIAN_POINT ( 'NONE',  ( 5.260679775997886054, -1.568431141927080219, 1.487858469166832176 ) ) ;
#133740 = LINE ( 'NONE', #34060, #214106 ) ;
#133741 = LINE ( 'NONE', #2603, #129128 ) ;
#133743 = CARTESIAN_POINT ( 'NONE',  ( 5.097279880301520905, -0.2930512725940071506, 1.994873791649566463 ) ) ;
#133742 = CARTESIAN_POINT ( 'NONE',  ( -7.714226216051410567, 9.062647342557177410, 1.082531754730558626 ) ) ;
#133744 = CARTESIAN_POINT ( 'NONE',  ( 0.7499999999999902300, 5.816666666666685082, -1.299038105676658228 ) ) ;
#133745 = CARTESIAN_POINT ( 'NONE',  ( 1.031410063161166013, -1.091267733730487466, -1.335775140220570201 ) ) ;
#133746 = CARTESIAN_POINT ( 'NONE',  ( 5.896870467300973750, 5.844380064798101237, 0.7998128361456352531 ) ) ;
#133748 = CARTESIAN_POINT ( 'NONE',  ( 7.828907357248368726, 8.098423103070084395, 0.7998128361456281477 ) ) ;
#133747 = CARTESIAN_POINT ( 'NONE',  ( 8.487040972474689582, 9.964264558384387627, -1.082531754730543083 ) ) ;
#133749 = CARTESIAN_POINT ( 'NONE',  ( -10.63162544082345917, 5.889931872887933295, 5.474679228419857324 ) ) ;
#133750 = CARTESIAN_POINT ( 'NONE',  ( 5.958239543830243790, 0.7576973323653664050, 1.710380810381225913 ) ) ;
#133751 = CARTESIAN_POINT ( 'NONE',  ( 5.853776559028295523, -1.461190594579380608, -1.385140169207878413 ) ) ;
#133752 = CIRCLE ( 'NONE', #57497, 0.5000000000000013323 ) ;
#133753 = CARTESIAN_POINT ( 'NONE',  ( -6.956742217143487395, 8.249192353823097790, 1.082531754730549078 ) ) ;
#133754 = ORIENTED_EDGE ( 'NONE', *, *, #104548, .T. ) ;
#133756 = CARTESIAN_POINT ( 'NONE',  ( 1.230092461119953517, 2.014234866427236259, 0.09611455020034495589 ) ) ;
#133755 = CARTESIAN_POINT ( 'NONE',  ( 2.614065066921432479, -0.6628553294307990562, 2.014303955012682223 ) ) ;
#133757 = CARTESIAN_POINT ( 'NONE',  ( 0.9667389835759466754, -1.427192611269219924, 1.115597691851821116 ) ) ;
#133758 = CARTESIAN_POINT ( 'NONE',  ( 8.039058738260216330, 8.343599714250547805, -0.7998128361456341429 ) ) ;
#133759 = CARTESIAN_POINT ( 'NONE',  ( 6.526263005029545816, 1.249015235541932167, -1.764162671312206498 ) ) ;
#133760 = MECHANICAL_DESIGN_GEOMETRIC_PRESENTATION_REPRESENTATION (  '', ( #19612 ), #36927 ) ;
#133761 = CARTESIAN_POINT ( 'NONE',  ( 6.100279051144945619, 9.204410428722734849, -1.199719254218440723 ) ) ;
#133763 = CARTESIAN_POINT ( 'NONE',  ( -0.06540554862877968889, -1.536972603800386361, 1.143280314369120587 ) ) ;
#133762 = CARTESIAN_POINT ( 'NONE',  ( -4.069418662396130593, 7.899405539437467816, -0.7998128361456281477 ) ) ;
#133764 = CARTESIAN_POINT ( 'NONE',  ( 1.865749732055407728, 8.973930515401084662, 0.7750000000000004663 ) ) ;
#133765 = CARTESIAN_POINT ( 'NONE',  ( 1.220146605508150803E-14, 9.687500000000000000, -1.499999999999998446 ) ) ;
#133766 = CARTESIAN_POINT ( 'NONE',  ( 4.311129659021211147, 7.973475668925984472, 1.040834085586084257E-14 ) ) ;
#133767 = CARTESIAN_POINT ( 'NONE',  ( -1.364683531250000748, 0.5718750003414208027, 0.000000000000000000 ) ) ;
#133768 = CARTESIAN_POINT ( 'NONE',  ( 4.039966587192267866, 4.776011108888172707, 1.082531754730560403 ) ) ;
#133769 = CARTESIAN_POINT ( 'NONE',  ( -2.286521462199063492, 5.819358805874190743, 1.040834085586084257E-14 ) ) ;
#133770 = AXIS2_PLACEMENT_3D ( 'NONE', #58976, #56841, #74167 ) ;
#133771 = CARTESIAN_POINT ( 'NONE',  ( 4.258765444007106105, -1.603684720688375975, 1.449730421305382544 ) ) ;
#133772 = CARTESIAN_POINT ( 'NONE',  ( -5.478903473698247595, 8.445785581739666981, -1.082531754730549967 ) ) ;
#133773 = CARTESIAN_POINT ( 'NONE',  ( 6.400857919427532572, 6.640291458853147866, -0.7216878364870458196 ) ) ;
#133774 = CARTESIAN_POINT ( 'NONE',  ( 1.951583061186522583, -1.892041120407188304, 0.9578705467366486204 ) ) ;
#133775 = CARTESIAN_POINT ( 'NONE',  ( 6.528339890195162809, 1.048227956652090009, -1.494441373796271399 ) ) ;
#133776 = EDGE_CURVE ( 'NONE', #128754, #128826, #134432, .T. ) ;
#133777 = CARTESIAN_POINT ( 'NONE',  ( 2.741432468550320412, -1.458365196291089072, -1.326584384502631719 ) ) ;
#133778 = CARTESIAN_POINT ( 'NONE',  ( 5.027564050633359649, -0.2746679736120913318, 1.892429487827557599 ) ) ;
#133779 = EDGE_LOOP ( 'NONE', ( #197521, #159312, #51354, #48869 ) ) ;
#133780 = CARTESIAN_POINT ( 'NONE',  ( -0.4000000000000357714, 3.949999999999981526, -0.5000000000000299760 ) ) ;
#133781 = CARTESIAN_POINT ( 'NONE',  ( 5.934039001034627780, 1.171926208273272207, 1.582800714458313385 ) ) ;
#133782 = CARTESIAN_POINT ( 'NONE',  ( 1.517416608934060385, -1.078585517578967368, -1.614684294522166663 ) ) ;
#133783 = ORIENTED_EDGE ( 'NONE', *, *, #10768, .F. ) ;
#133784 = CARTESIAN_POINT ( 'NONE',  ( -5.093022980588950865, 5.970890227889075419, -1.199719254218453823 ) ) ;
#133786 = CARTESIAN_POINT ( 'NONE',  ( 1.836270655118562800, 2.510430850797893410, -2.497621424930284384 ) ) ;
#133785 = CARTESIAN_POINT ( 'NONE',  ( -5.465345320084574965, 9.390336950158399532, 0.000000000000000000 ) ) ;
#133787 = CARTESIAN_POINT ( 'NONE',  ( 7.121056995675668411, 9.330985799753529264, -1.599625672291262513 ) ) ;
#133789 = CARTESIAN_POINT ( 'NONE',  ( 5.519577934094861860, 6.572500690266394940, 1.082531754730549078 ) ) ;
#133788 = CARTESIAN_POINT ( 'NONE',  ( 5.309989718046547402, 9.346738437696316737, 0.7998128361456462443 ) ) ;
#133791 = ORIENTED_EDGE ( 'NONE', *, *, #199073, .F. ) ;
#133790 = CARTESIAN_POINT ( 'NONE',  ( 6.287759715630294011, 1.828497742151834027, -0.5598019499635784602 ) ) ;
#133792 = CARTESIAN_POINT ( 'NONE',  ( 3.299657469156279888, 1.739734091921738557, 1.357710657151039779 ) ) ;
#133793 = CARTESIAN_POINT ( 'NONE',  ( 1.782535857997105566, -1.180187651135233384, 1.864495428577646274 ) ) ;
#133794 = CARTESIAN_POINT ( 'NONE',  ( 0.2582720099171370021, 1.907150531373353664, 0.1405958444523764117 ) ) ;
#133795 = CARTESIAN_POINT ( 'NONE',  ( -0.07968943112122245376, 15.51761980755981973, 11.99973206010910864 ) ) ;
#133796 = CARTESIAN_POINT ( 'NONE',  ( -8.673617379884035472E-15, 3.507114751586604129, -11.99288524841337455 ) ) ;
#133797 = CARTESIAN_POINT ( 'NONE',  ( 3.156751980976373329, -0.5984545454679365273, -1.982000093670479135 ) ) ;
#133798 = CARTESIAN_POINT ( 'NONE',  ( -6.423865854776591000, 6.388931673527803667, 1.040834085586084257E-14 ) ) ;
#133799 = CARTESIAN_POINT ( 'NONE',  ( -5.288707357724018898, 7.660230058424141397, 1.223219983389673748 ) ) ;
#133801 = CARTESIAN_POINT ( 'NONE',  ( 1.710078970767275885, -2.145365142986368934, 0.2646356489638818088 ) ) ;
#133800 = CARTESIAN_POINT ( 'NONE',  ( -2.591579918506545344, 6.175260338232929413, 1.040834085586084257E-14 ) ) ;
#133802 = CARTESIAN_POINT ( 'NONE',  ( 3.737968522918270864, 2.181131050170285857, 0.2133239450496857148 ) ) ;
#133803 = DIRECTION ( 'NONE',  ( 0.000000000000000000, 0.000000000000000000, 1.000000000000000000 ) ) ;
#133804 = CARTESIAN_POINT ( 'NONE',  ( 3.255366281057017197, 6.812028071292901998, -0.7216878364870338292 ) ) ;
#133805 = CARTESIAN_POINT ( 'NONE',  ( -1.364683531250000748, 14.42187500034139447, 0.000000000000000000 ) ) ;
#133806 = CARTESIAN_POINT ( 'NONE',  ( -6.303615075710993665, 6.318915441276411471, -0.7998128361456362523 ) ) ;
#133807 = CARTESIAN_POINT ( 'NONE',  ( 5.572856105055380205, -0.7716597722284452843, 1.553080519226685885 ) ) ;
#133808 = CARTESIAN_POINT ( 'NONE',  ( -8.459924665247381625, 11.85336729522185806, 1.082531754730560403 ) ) ;
#133809 = CARTESIAN_POINT ( 'NONE',  ( 3.977443466873982203, -0.1572589350618114057, 2.064370724987254047 ) ) ;
#133810 = CARTESIAN_POINT ( 'NONE',  ( 4.552435263133931542, -1.381712717965150938, 1.604331009294196031 ) ) ;
#133811 = CARTESIAN_POINT ( 'NONE',  ( 6.810273232766058449, 6.839740281182199233, 1.040834085586084257E-14 ) ) ;
#133812 = CARTESIAN_POINT ( 'NONE',  ( -0.6823417656249969321, 4.967708333674755394, -1.181850606188749264 ) ) ;
#133813 = CARTESIAN_POINT ( 'NONE',  ( 2.746873616242023086, -0.3318220265390697254, -1.941108330032844664 ) ) ;
#133814 = CARTESIAN_POINT ( 'NONE',  ( 0.7031954830387620037, 1.685401770928725007, -0.9037484838233383888 ) ) ;
#133815 = CARTESIAN_POINT ( 'NONE',  ( 4.611445210273608986, -2.248620548832699573, 0.4443846451570551692 ) ) ;
#133817 = ADVANCED_FACE ( 'NONE', ( #119418 ), #73459, .T. ) ;
#133816 = CARTESIAN_POINT ( 'NONE',  ( 3.088313589057069208, -1.798746773638896457, -0.3115406389907551810 ) ) ;
#133818 = CARTESIAN_POINT ( 'NONE',  ( 4.686278372178935392, 5.496354851410763409, 1.199719254218452047 ) ) ;
#133819 = CARTESIAN_POINT ( 'NONE',  ( 5.477130869796502211, 5.492333557625114437, 1.040834085586084257E-14 ) ) ;
#133820 = CARTESIAN_POINT ( 'NONE',  ( -8.044065211609668253, 8.279164256499745633, 0.7998128361456602331 ) ) ;
#133821 = VERTEX_POINT ( 'NONE', #191013 ) ;
#133822 = EDGE_LOOP ( 'NONE', ( #103141, #180628, #96475, #22316 ) ) ;
#133823 = CARTESIAN_POINT ( 'NONE',  ( 3.515888537569244132, -0.5802020150980004010, 1.927815774739343180 ) ) ;
#133824 = CARTESIAN_POINT ( 'NONE',  ( 4.627759936859944467, 1.903863570041373077, -0.4726564843360381851 ) ) ;
#133825 = CARTESIAN_POINT ( 'NONE',  ( -8.179646747746328828, 8.437342715325849341, -0.7998128361456291469 ) ) ;
#133826 = AXIS2_PLACEMENT_3D ( 'NONE', #59924, #126079, #110879 ) ;
#133827 = CARTESIAN_POINT ( 'NONE',  ( -6.423865854776591000, 6.388931673527803667, 1.040834085586084257E-14 ) ) ;
#133829 = EDGE_CURVE ( 'NONE', #184855, #154238, #184086, .T. ) ;
#133828 = CARTESIAN_POINT ( 'NONE',  ( 0.07556134207194721564, 2.859159929750184848, -2.732257853551669946 ) ) ;
#133831 = CARTESIAN_POINT ( 'NONE',  ( 5.207753166488873653, -1.761066459785052274, 0.1758167199723305041 ) ) ;
#133830 = CARTESIAN_POINT ( 'NONE',  ( 0.6442209307526406414, 0.6107738465899931191, 1.999526160293135568 ) ) ;
#133832 = CARTESIAN_POINT ( 'NONE',  ( 3.024201889537345700, 6.315044714278881699, 0.6036835607809933890 ) ) ;
#133833 = CARTESIAN_POINT ( 'NONE',  ( 2.273600812266802773, 1.349468827467028120, 1.726581335083368085 ) ) ;
#133834 = CARTESIAN_POINT ( 'NONE',  ( 6.333937804992649134, 1.722499169431927601, 0.2476611369811829999 ) ) ;
#133835 = CARTESIAN_POINT ( 'NONE',  ( 8.288111976655649471, 8.563885482386732306, -0.7998128361456291469 ) ) ;
#133836 =( NAMED_UNIT ( * ) SI_UNIT ( $, .STERADIAN. ) SOLID_ANGLE_UNIT ( ) );
#133837 = CARTESIAN_POINT ( 'NONE',  ( 0.9610595616070281011, 0.3405255003954327786, -1.690740162648683320 ) ) ;
#133838 = CARTESIAN_POINT ( 'NONE',  ( 0.7557052203445973060, -2.281327611594321958, -0.2792575881873406440 ) ) ;
#133839 = CARTESIAN_POINT ( 'NONE',  ( 0.9080814035550346386, -0.9900877184637231210, -1.955254813705724404 ) ) ;
#133840 = CARTESIAN_POINT ( 'NONE',  ( 6.731818218530718489, -1.587343137472529309, -0.6980196547925822115 ) ) ;
#133841 = CARTESIAN_POINT ( 'NONE',  ( 2.561379550486083012, -1.920685204893451292, -1.086737900330703166 ) ) ;
#133842 = CARTESIAN_POINT ( 'NONE',  ( 6.760228240101231023, -2.170840268647770799, 0.04637219581851703687 ) ) ;
#133843 = CARTESIAN_POINT ( 'NONE',  ( 0.000000000000000000, 8.500000000000000000, 0.000000000000000000 ) ) ;
#133844 = CARTESIAN_POINT ( 'NONE',  ( 2.237658791021436056, 0.5595254372263277487, -2.042044324946710621 ) ) ;
#133845 = CARTESIAN_POINT ( 'NONE',  ( 6.827182134110192813, 7.051736335826703339, 2.787205296604370108 ) ) ;
#133846 = CARTESIAN_POINT ( 'NONE',  ( 5.122061974917812677, -1.030465543002171858, -1.627433240741954723 ) ) ;
#133847 = ORIENTED_EDGE ( 'NONE', *, *, #5366, .F. ) ;
#133849 = CARTESIAN_POINT ( 'NONE',  ( -1.201851678989727383E-14, 5.587500000000021672, -1.732050807568863648 ) ) ;
#133848 = CARTESIAN_POINT ( 'NONE',  ( 2.015536172832455897, -2.222481616396556170, 0.5612588729206613447 ) ) ;
#133850 = CARTESIAN_POINT ( 'NONE',  ( 3.846762897975340767, 5.510976019103107859, -1.599625672291256295 ) ) ;
#133851 = B_SPLINE_CURVE_WITH_KNOTS ( 'NONE', 3,
 ( #174047, #125349, #109090, #73296, #106945, #189199, #92794, #123234 ),
 .UNSPECIFIED., .F., .F.,
 ( 4, 2, 2, 4 ),
 ( 0.000000000000000000, 0.0001985720215089283687, 0.0003971440430178567373, 0.0007942880860357131494 ),
 .UNSPECIFIED. ) ;
#133852 = CARTESIAN_POINT ( 'NONE',  ( 5.469824908109481854, 8.468880595181346393, -1.199719254218446718 ) ) ;
#133853 = CARTESIAN_POINT ( 'NONE',  ( 4.371885135981863790, 0.4866971690204218159, -2.167184880714991824 ) ) ;
#133854 = CARTESIAN_POINT ( 'NONE',  ( -8.188761592974058701, 8.655902734665618325, -0.7216878364870278340 ) ) ;
#133855 = CARTESIAN_POINT ( 'NONE',  ( -0.2903707658989356788, -5.254568858751054172, -10.97058181929407716 ) ) ;
#133856 = AXIS2_PLACEMENT_3D ( 'NONE', #187388, #27014, #22734 ) ;
#133857 = CARTESIAN_POINT ( 'NONE',  ( 5.002595493762530765, 8.780185809457538681, 1.040834085586084257E-14 ) ) ;
#133858 = CARTESIAN_POINT ( 'NONE',  ( -7.904040366642703930, 10.24446639921506552, 1.443375672974090751 ) ) ;
#133859 = ADVANCED_FACE ( 'NONE', ( #65276 ), #170333, .F. ) ;
#133860 = CARTESIAN_POINT ( 'NONE',  ( 4.584065335196252811, 8.362176967788721882, 0.7216878364870328300 ) ) ;
#133862 = ORIENTED_EDGE ( 'NONE', *, *, #127587, .F. ) ;
#133861 = TOROIDAL_SURFACE ( 'NONE', #5776, 5.799999999999999822, 0.4000000000000000222 ) ;
#133863 = CARTESIAN_POINT ( 'NONE',  ( 2.514296259408643319, -1.880434619097739013, 0.7283795345095490648 ) ) ;
#133865 = CARTESIAN_POINT ( 'NONE',  ( 0.9013244701963195604, -1.770926582075180944, 1.057100273733258433 ) ) ;
#133864 = CARTESIAN_POINT ( 'NONE',  ( 8.288111976655649471, 8.563885482386732306, -0.7998128361456291469 ) ) ;
#133866 = CARTESIAN_POINT ( 'NONE',  ( -10.99970480893081337, -6.134628647623513231, -0.08058608058607207025 ) ) ;
#133867 = CARTESIAN_POINT ( 'NONE',  ( 6.170369307550823912, 7.331757292631694511, 1.082531754730549967 ) ) ;
#133868 = CARTESIAN_POINT ( 'NONE',  ( -11.01135777277262129, 13.40000000000000036, -1.400000000000001910 ) ) ;
#133869 = CARTESIAN_POINT ( 'NONE',  ( -1.364683531250012516, 3.238541667008084879, -0.7879004041258289570 ) ) ;
#133870 = CARTESIAN_POINT ( 'NONE',  ( 4.382901342696458258, 1.958101449220098988, -0.9841704303943515919 ) ) ;
#133871 = CARTESIAN_POINT ( 'NONE',  ( 1.424454163599726320, -1.462446849824734274, -1.388484543128357229 ) ) ;
#133872 = CARTESIAN_POINT ( 'NONE',  ( 1.505144418776669601, -1.827259764946763454, 0.2261131901925839127 ) ) ;
#133873 = CARTESIAN_POINT ( 'NONE',  ( 4.792671637142519536, 1.906707348304257366, -1.272296631038958070 ) ) ;
#133874 = CARTESIAN_POINT ( 'NONE',  ( 3.081803158279991628, -1.813988701161291628, -0.3140598505507880556 ) ) ;
#133875 = CARTESIAN_POINT ( 'NONE',  ( 6.923409998072794558, 11.22906209772695618, 1.040834085586084257E-14 ) ) ;
#133876 = CARTESIAN_POINT ( 'NONE',  ( 3.873894609034499670, 1.013791609252197690, 1.518000939925366000 ) ) ;
#133877 = CARTESIAN_POINT ( 'NONE',  ( 5.485000066852382616, -2.016597020608828839, 0.002808655738886777897 ) ) ;
#133878 = CARTESIAN_POINT ( 'NONE',  ( -7.181014916732457287, 11.52960116949655678, -0.7998128361456291469 ) ) ;
#133880 = DIRECTION ( 'NONE',  ( -1.000000000000000000, 4.984021416236792516E-16, 0.000000000000000000 ) ) ;
#133879 = CARTESIAN_POINT ( 'NONE',  ( 4.452213415057678425, 2.262087339288323840, -0.05152095106783493444 ) ) ;
#133881 = CARTESIAN_POINT ( 'NONE',  ( 6.827182134110199030, -0.004087946457608306570, 2.088967824442849341 ) ) ;
#133882 = CARTESIAN_POINT ( 'NONE',  ( 3.982925052038261526, 1.964963782255540359, 0.6523228965355857278 ) ) ;
#133883 = CARTESIAN_POINT ( 'NONE',  ( 9.215791728987056786, 11.77484298861683598, -1.599625672291262513 ) ) ;
#133884 = CARTESIAN_POINT ( 'NONE',  ( 1.360316468749961816, 2.026041667008099179, 0.7853790794158520550 ) ) ;
#133885 = APPLICATION_PROTOCOL_DEFINITION ( 'draft international standard', 'automotive_design', 1998, #126667 ) ;
#133887 = CARTESIAN_POINT ( 'NONE',  ( 1.893070592381540740, 1.676246824859698892, -0.9494106994061870530 ) ) ;
#133886 = CARTESIAN_POINT ( 'NONE',  ( -8.311311860377216476, 9.655284244316948872, -1.199719254218446718 ) ) ;
#133888 = UNCERTAINTY_MEASURE_WITH_UNIT (LENGTH_MEASURE( 1.000000000000000082E-05 ), #81990, 'distance_accuracy_value', 'NONE');
#133889 = CARTESIAN_POINT ( 'NONE',  ( 4.831368594223144797, 5.066186338679537826, -0.7556405859116925861 ) ) ;
#133890 = CARTESIAN_POINT ( 'NONE',  ( 6.350452388456855779, -1.959648489363738699, -0.1964464578135850514 ) ) ;
#133891 = CARTESIAN_POINT ( 'NONE',  ( 5.221298554594243413, 5.264138866547622975, -0.7216878364870458196 ) ) ;
#133892 = CARTESIAN_POINT ( 'NONE',  ( 5.811422509517683466, 6.026224704000590293, 0.4751317933852049480 ) ) ;
#133893 = CARTESIAN_POINT ( 'NONE',  ( -4.302014814237876017, 3.913438792899272212, 0.7998128361456341429 ) ) ;
#133895 = CARTESIAN_POINT ( 'NONE',  ( 2.022025532713614737, -0.4812968563913700981, 2.168513943247989850 ) ) ;
#133894 = CARTESIAN_POINT ( 'NONE',  ( 0.7914572142167939361, -0.05789999323873443182, -2.119991495365561640 ) ) ;
#133896 = CARTESIAN_POINT ( 'NONE',  ( 3.135867587238525100, -1.413284743790550468, -1.561492743641406999 ) ) ;
#133897 = CARTESIAN_POINT ( 'NONE',  ( -5.966470118465691641, 9.118576350588734059, -1.199719254218452047 ) ) ;
#133898 = CARTESIAN_POINT ( 'NONE',  ( 5.991813822235618758, 9.077867661661846554, 1.199719254218462483 ) ) ;
#133899 = CARTESIAN_POINT ( 'NONE',  ( 6.912964126797830566, -1.438640208141970245, 1.180240733875538517 ) ) ;
#133900 = CARTESIAN_POINT ( 'NONE',  ( 4.950698647284403009, 8.927565521807144577, 1.040834085586084257E-14 ) ) ;
#133901 = CARTESIAN_POINT ( 'NONE',  ( -4.236586233130071655, 7.334480220043515075, -0.8772045297030308664 ) ) ;
#133902 = CARTESIAN_POINT ( 'NONE',  ( 4.364835388595708743, 7.179726155748598515, 1.199719254218462483 ) ) ;
#133903 = CARTESIAN_POINT ( 'NONE',  ( -4.489158259900630554, 8.251452046610447510, 0.000000000000000000 ) ) ;
#133905 = CARTESIAN_POINT ( 'NONE',  ( -7.212574532790092974, 10.39812547402169862, -1.082531754730543971 ) ) ;
#133904 = AXIS2_PLACEMENT_3D ( 'NONE', #102572, #104724, #103651 ) ;
#133906 = CARTESIAN_POINT ( 'NONE',  ( 1.564851893998190135, 0.6701894319398638000, 2.011955567234039677 ) ) ;
#133907 = CARTESIAN_POINT ( 'NONE',  ( -5.261446130555064826, 8.296048364692991228, 1.199719254218452935 ) ) ;
#133909 = CARTESIAN_POINT ( 'NONE',  ( 4.316819842036943911, -1.455217238560998272, 1.315978175897666080 ) ) ;
#133908 = CARTESIAN_POINT ( 'NONE',  ( 1.224999999999982991, 0.8749999999999937828, -4.163336342344337027E-14 ) ) ;
#133910 = CARTESIAN_POINT ( 'NONE',  ( 3.045950098598048328, 0.7793912989166664751, -2.016482303682599841 ) ) ;
#133911 = CARTESIAN_POINT ( 'NONE',  ( 1.487592393518050837, -1.832424703912252317, -0.1798031890194173865 ) ) ;
#133912 = CARTESIAN_POINT ( 'NONE',  ( -4.047283575590383542, 7.579128156381162107, 0.3715214982176785474 ) ) ;
#133913 = FACE_OUTER_BOUND ( 'NONE', #122724, .T. ) ;
#133914 = CARTESIAN_POINT ( 'NONE',  ( 4.698987106650459822, -0.4602053158732459237, 1.678299975232977026 ) ) ;
#133915 = CARTESIAN_POINT ( 'NONE',  ( 6.639320575229280763, 7.629137130509070275, 2.496737603865983424 ) ) ;
#133916 = CARTESIAN_POINT ( 'NONE',  ( 6.656690234629796699, 6.868486149930637552, 1.040834085586084257E-14 ) ) ;
#133917 = CARTESIAN_POINT ( 'NONE',  ( -10.71026998871754721, 6.055660674263378951, 4.667787751035539223 ) ) ;
#133918 = CONICAL_SURFACE ( 'NONE', #61208, 1.000000000000000000, 0.7853981633974508325 ) ;
#133919 = CARTESIAN_POINT ( 'NONE',  ( 1.833122199354455972, 0.2117775504973731793, 2.151289291301178075 ) ) ;
#133920 = CARTESIAN_POINT ( 'NONE',  ( 3.761092154037175117, -2.013677596940225190, -0.1017350580494805479 ) ) ;
#133921 = CARTESIAN_POINT ( 'NONE',  ( -10.29027540264791440, 11.10766884595181203, 0.7216878364870438212 ) ) ;
#133922 = CARTESIAN_POINT ( 'NONE',  ( 1.059701713109785670, 0.4209238396889224965, -2.120155868012041811 ) ) ;
#133923 = CARTESIAN_POINT ( 'NONE',  ( 3.414874914781691473, 1.781649806626634858, 0.8443359948157087569 ) ) ;
#133924 = LINE ( 'NONE', #19047, #122707 ) ;
#133925 = CARTESIAN_POINT ( 'NONE',  ( 3.017060306806388148, -1.870969668351904147, 0.5203628790987256947 ) ) ;
#133928 = ORIENTED_EDGE ( 'NONE', *, *, #178431, .F. ) ;
#133927 = CARTESIAN_POINT ( 'NONE',  ( -4.340018570150318666, 6.156717313299049366, -1.443375672974066548 ) ) ;
#133926 = CARTESIAN_POINT ( 'NONE',  ( -10.27671724903424888, 11.09185100006920877, 1.040834085586084257E-14 ) ) ;
#133929 = COLOUR_RGB ( '', 0.31764706, 0.68627451, 0.89019608) ;
#133930 = CARTESIAN_POINT ( 'NONE',  ( -5.275531169048911728, 6.287779464379406491, -1.082531754730549967 ) ) ;
#133931 = CARTESIAN_POINT ( 'NONE',  ( 3.464990776744291345, 6.200183785247111778, 1.199719254218452047 ) ) ;
#133932 = CARTESIAN_POINT ( 'NONE',  ( -5.829079699232685208, 5.765290835385048496, 0.000000000000000000 ) ) ;
#133933 = CARTESIAN_POINT ( 'NONE',  ( -6.038177310039794854, 8.137902509836795417, -1.599625672291271394 ) ) ;
#133934 = CARTESIAN_POINT ( 'NONE',  ( -9.286972035236626510, 11.85788667924133399, -1.443375672974058777 ) ) ;
#133935 = CARTESIAN_POINT ( 'NONE',  ( 0.4818276840582723652, 2.058231501447154610, -0.7964225590989246761 ) ) ;
#133936 = CARTESIAN_POINT ( 'NONE',  ( -3.285556943750000070, -3.959374999522043304, 0.000000000000000000 ) ) ;
#133937 = CARTESIAN_POINT ( 'NONE',  ( 4.979329090789969214, -0.1002203015587413149, 1.959344625532564610 ) ) ;
#133938 = CARTESIAN_POINT ( 'NONE',  ( 1.793592486599729252, 1.492254607734722072, -1.356300734917381678 ) ) ;
#133939 = EDGE_LOOP ( 'NONE', ( #167985, #69695, #121644, #115903, #185832, #17908, #60357, #23850 ) ) ;
#133940 = CARTESIAN_POINT ( 'NONE',  ( 3.661412522060889074, 1.992289893316813609, -0.7171584230975246443 ) ) ;
#133941 = CARTESIAN_POINT ( 'NONE',  ( 1.499999999999989120, 3.285416667349486897, 0.8660254037844524744 ) ) ;
#133943 = CARTESIAN_POINT ( 'NONE',  ( -5.961834861707238531, 7.978559976790334574, -1.599625672291263179 ) ) ;
#133942 = FACE_OUTER_BOUND ( 'NONE', #186990, .T. ) ;
#133944 = CARTESIAN_POINT ( 'NONE',  ( 3.468544592087896561, 0.04396668885017079864, -1.840778273432375212 ) ) ;
#133945 = ORIENTED_EDGE ( 'NONE', *, *, #81658, .T. ) ;
#133946 = CARTESIAN_POINT ( 'NONE',  ( -7.645908563102897126, 11.00764485934031889, 1.199719254218453823 ) ) ;
#133947 = LINE ( 'NONE', #68877, #23903 ) ;
#133948 = CARTESIAN_POINT ( 'NONE',  ( 4.869442314738527067, -1.792836814666173062, -1.132239877606910472 ) ) ;
#133949 = CARTESIAN_POINT ( 'NONE',  ( -5.527925976246812034, 5.968540277179252840, -0.9326450038637500439 ) ) ;
#133950 = CARTESIAN_POINT ( 'NONE',  ( 5.276094334012385367, 9.307193822989793475, 1.040834085586084257E-14 ) ) ;
#133951 = CARTESIAN_POINT ( 'NONE',  ( 5.132131416026131987, 1.062877790662479116, -1.765404227961290484 ) ) ;
#133954 = CARTESIAN_POINT ( 'NONE',  ( 2.348939331405873077, 0.4892633877765646400, -1.774999737812533063 ) ) ;
#133953 = CARTESIAN_POINT ( 'NONE',  ( 1.117373073715557164, 0.3680575366376471758, -1.824110739772739631 ) ) ;
#133952 = CARTESIAN_POINT ( 'NONE',  ( 0.9782388782688978823, 3.999999999999989786, -0.4000000000000097367 ) ) ;
#133955 = CARTESIAN_POINT ( 'NONE',  ( 8.910733272679570049, 11.41894145625809820, -1.599625672291255185 ) ) ;
#133956 = CARTESIAN_POINT ( 'NONE',  ( -11.89942855770814134, 9.799999999999998934, 0.6999999999999992895 ) ) ;
#133957 = CARTESIAN_POINT ( 'NONE',  ( -3.975497760493641675, 7.849573349659754840, -7.471960471057975262E-11 ) ) ;
#133958 = CARTESIAN_POINT ( 'NONE',  ( 1.717678464306471309, -0.2677704892378242607, 2.190511422692428045 ) ) ;
#133959 = CARTESIAN_POINT ( 'NONE',  ( 4.552213317786341307, 2.262020173471789963, -0.04951151886351152359 ) ) ;
#133960 = CARTESIAN_POINT ( 'NONE',  ( -7.863365906246074566, 8.276274433482971205, -0.7216878364870278340 ) ) ;
#133961 = CARTESIAN_POINT ( 'NONE',  ( 4.183730900115702589, 1.755568954123175596, -0.4464138967742969366 ) ) ;
#133962 = CARTESIAN_POINT ( 'NONE',  ( 4.891753643660703865, -1.905893201010636195, 0.1940691045876908327 ) ) ;
#133963 = CARTESIAN_POINT ( 'NONE',  ( -1.201851678989727383E-14, 5.509375000341415252, -1.575800808251660134 ) ) ;
#133964 = ADVANCED_FACE ( 'NONE', ( #97823 ), #15463, .F. ) ;
#133965 = CARTESIAN_POINT ( 'NONE',  ( 4.170748999387418721, -1.839122178589139178, -0.7105754535856413368 ) ) ;
#133966 = CARTESIAN_POINT ( 'NONE',  ( 4.891396039733495016, 1.386484060982313249, 1.255958711209571810 ) ) ;
#133967 = CARTESIAN_POINT ( 'NONE',  ( 4.685918305224146430, -1.144368955370359098, -1.467557204495354872 ) ) ;
#133968 = CARTESIAN_POINT ( 'NONE',  ( -0.6823417656249969321, 5.467708333674756283, -1.181850606188749264 ) ) ;
#133969 = CARTESIAN_POINT ( 'NONE',  ( 0.6379081216283178923, 2.014007883293071899, -0.1037844182863178755 ) ) ;
#133970 =( BOUNDED_SURFACE ( )  B_SPLINE_SURFACE ( 3, 2, ( 
 ( #173576, #191903, #56597 ),
 ( #5665, #207096, #104283 ),
 ( #124875, #204946, #122760 ),
 ( #188720, #137859, #105366 ),
 ( #170329, #140005, #21915 ),
 ( #25145, #203880, #55524 ),
 ( #187644, #79238, #176742 ),
 ( #109685, #196194, #113948 ),
 ( #163699, #111812, #177817 ),
 ( #128087, #47837, #213472 ),
 ( #29433, #211357, #95524 ),
 ( #127016, #44627, #179944 ),
 ( #93385, #144295, #15282 ),
 ( #192975, #146401, #131252 ),
 ( #31567, #145357, #112875 ),
 ( #161574, #13161, #110744 ),
 ( #62982, #94451, #65095 ),
 ( #45697, #129150, #209213 ) ),
 .UNSPECIFIED., .F., .F., .T. ) 
 B_SPLINE_SURFACE_WITH_KNOTS ( ( 4, 2, 2, 2, 2, 2, 2, 2, 4 ),
 ( 3, 3 ),
 ( 0.000000000000000000, 0.0002366965742690630467, 0.0004733931485381260933, 0.0007100897228071891129, 0.0009467862970762521866, 0.001183482871345315152, 0.001420179445614378226, 0.001656876019883441300, 0.001893572594152504373 ),
 ( 0.000000000000000000, 1.000000000000000000 ),
 .UNSPECIFIED. ) 
 GEOMETRIC_REPRESENTATION_ITEM ( )  RATIONAL_B_SPLINE_SURFACE ( (
 ( 1.000000000000000000, 0.5647844906712726765, 1.000000000000000000),
 ( 1.000000000000000000, 0.5466263600439149606, 1.000000000000000000),
 ( 1.000000000000000000, 0.5350732119542429555, 1.000000000000000000),
 ( 1.000000000000000000, 0.5340116227283870920, 1.000000000000000000),
 ( 1.000000000000000000, 0.5448366076419293158, 1.000000000000000000),
 ( 1.000000000000000000, 0.5794957582367121773, 1.000000000000000000),
 ( 1.000000000000000000, 0.6029004271910476387, 1.000000000000000000),
 ( 1.000000000000000000, 0.6471109807880470743, 1.000000000000000000),
 ( 1.000000000000000000, 0.6680936278988007793, 1.000000000000000000),
 ( 1.000000000000000000, 0.6979136174567561746, 1.000000000000000000),
 ( 1.000000000000000000, 0.7066420332305399787, 1.000000000000000000),
 ( 1.000000000000000000, 0.7075346919462069950, 1.000000000000000000),
 ( 1.000000000000000000, 0.6996296472763622321, 1.000000000000000000),
 ( 1.000000000000000000, 0.6710614938507052374, 1.000000000000000000),
 ( 1.000000000000000000, 0.6504127778617917466, 1.000000000000000000),
 ( 1.000000000000000000, 0.6064966788547884180, 1.000000000000000000),
 ( 1.000000000000000000, 0.5828236970731401900, 1.000000000000000000),
 ( 1.000000000000000000, 0.5649783097559288869, 1.000000000000000000) ) ) 
 REPRESENTATION_ITEM ( '' )  SURFACE ( )  );
#133972 = CARTESIAN_POINT ( 'NONE',  ( 2.156984414944181694, -1.627247350590403707, 1.336999143475733121 ) ) ;
#133971 = CARTESIAN_POINT ( 'NONE',  ( -9.022061154889962964, 12.61315621642528129, -1.199719254218446718 ) ) ;
#133973 = CARTESIAN_POINT ( 'NONE',  ( 8.940712233207955606, 12.51824914112961729, 1.199719254218450271 ) ) ;
#133975 = LINE ( 'NONE', #85179, #52755 ) ;
#133974 = CARTESIAN_POINT ( 'NONE',  ( 1.499999999999993117, 11.88541666734946034, 0.8660254037844408170 ) ) ;
#133976 = CARTESIAN_POINT ( 'NONE',  ( 3.023802379225454473, -0.4096935937694180518, 2.080477853870852378 ) ) ;
#133977 = DIRECTION ( 'NONE',  ( 1.040834085586084257E-15, 1.000000000000000000, -4.622230424712076367E-32 ) ) ;
#133978 = CARTESIAN_POINT ( 'NONE',  ( 2.004171506046021012, -0.8596719693435939114, 1.827822491074476918 ) ) ;
#133979 = CARTESIAN_POINT ( 'NONE',  ( -0.6823417656250003738, 2.717708333674753618, -1.181850606188749264 ) ) ;
#133980 = CARTESIAN_POINT ( 'NONE',  ( 6.720655732516647163, 0.5950723047917580999, 1.879543361893110109 ) ) ;
#133981 = CARTESIAN_POINT ( 'NONE',  ( 2.984766373302843778, 6.633977868828633717, -0.7998128361456291469 ) ) ;
#133982 = ORIENTED_EDGE ( 'NONE', *, *, #181883, .F. ) ;
#133983 = CARTESIAN_POINT ( 'NONE',  ( 2.407699484934812784, -0.4761397456576694776, 2.108333575599189214 ) ) ;
#133984 = CARTESIAN_POINT ( 'NONE',  ( 6.610000000000014531, 2.942932264094192174, 2.732153830519419291 ) ) ;
#133986 = CARTESIAN_POINT ( 'NONE',  ( 11.88234649872613602, 9.843392170832489185, -0.9090484974825243647 ) ) ;
#133985 = CARTESIAN_POINT ( 'NONE',  ( 5.585032934186686226, 5.480569609498057382, 0.000000000000000000 ) ) ;
#133987 = CARTESIAN_POINT ( 'NONE',  ( 1.499999999999990896, 3.306250000682818602, 1.214306433183764966E-14 ) ) ;
#133988 = DIRECTION ( 'NONE',  ( -0.000000000000000000, -1.000000000000000000, -0.000000000000000000 ) ) ;
#133989 =( BOUNDED_CURVE ( )  B_SPLINE_CURVE ( 3, ( #185768, #21117, #82950, #137052 ),
 .UNSPECIFIED., .F., .T. ) 
 B_SPLINE_CURVE_WITH_KNOTS ( ( 4, 4 ),
 ( 3.059570999471033392, 3.223614307708452031 ),
 .UNSPECIFIED. ) 
 CURVE ( )  GEOMETRIC_REPRESENTATION_ITEM ( )  RATIONAL_B_SPLINE_CURVE ( ( 1.000000000000000000, 0.9977587396908789152, 0.9977587396908789152, 1.000000000000000000 ) ) 
 REPRESENTATION_ITEM ( '' )  );
#133990 = CARTESIAN_POINT ( 'NONE',  ( -8.351459436338048548, 8.845716885256940998, -0.7216878364870278340 ) ) ;
#133991 = AXIS2_PLACEMENT_3D ( 'NONE', #149560, #167940, #18473 ) ;
#133992 = CARTESIAN_POINT ( 'NONE',  ( 1.294752383181968503, 1.788903229852260246, -1.265732775075766092 ) ) ;
#133993 = DIRECTION ( 'NONE',  ( -0.9990890794760038940, 0.000000000000000000, 0.04267330865764931702 ) ) ;
#133995 = CARTESIAN_POINT ( 'NONE',  ( 1.364683531250000748, 11.75520833367473017, -0.7879004041258355073 ) ) ;
#133994 = CARTESIAN_POINT ( 'NONE',  ( 1.639924147338491123, -1.639646335682118927, -1.559238602228057990 ) ) ;
#133996 = CARTESIAN_POINT ( 'NONE',  ( -7.621654909176601045, 12.04368116068139472, 0.7998128361456481317 ) ) ;
#133997 = CARTESIAN_POINT ( 'NONE',  ( 4.417204035549080920, -1.841734835922325120, 0.8216704330437707426 ) ) ;
#133998 = CARTESIAN_POINT ( 'NONE',  ( -3.890826896997578999, 7.483122446565064756, 0.7216878364870317197 ) ) ;
#133999 = CARTESIAN_POINT ( 'NONE',  ( -1.364683531250012516, 2.301041667008087988, -0.7879004041258289570 ) ) ;
#134000 = CARTESIAN_POINT ( 'NONE',  ( 4.768187943840554333, 8.164982483533503199, -0.7738548252242994918 ) ) ;
#134001 = CARTESIAN_POINT ( 'NONE',  ( 1.499999999999997113, 10.89583333333333215, -0.8660254037844378194 ) ) ;
#134002 = CARTESIAN_POINT ( 'NONE',  ( 4.230855031843249847, 0.08773280417345018234, 1.722775095924995004 ) ) ;
#134003 = CARTESIAN_POINT ( 'NONE',  ( 3.203469434578891661, 6.959407783642502565, -0.7998128361456362523 ) ) ;
#134004 =( BOUNDED_SURFACE ( )  B_SPLINE_SURFACE ( 3, 2, ( 
 ( #69961, #51624, #151257 ),
 ( #54816, #2827, #1763 ),
 ( #116666, #68898, #202088 ),
 ( #4952, #135017, #182664 ) ),
 .UNSPECIFIED., .F., .F., .F. ) 
 B_SPLINE_SURFACE_WITH_KNOTS ( ( 4, 4 ),
 ( 3, 3 ),
 ( 0.000000000000000000, 3.124390133962077760E-05 ),
 ( 0.000000000000000000, 1.000000000000000000 ),
 .UNSPECIFIED. ) 
 GEOMETRIC_REPRESENTATION_ITEM ( )  RATIONAL_B_SPLINE_SURFACE ( (
 ( 1.000000000000000000, 0.7100530722023767893, 1.000000000000000000),
 ( 1.000000000000000000, 0.7100778649077733595, 1.000000000000000000),
 ( 1.000000000000000000, 0.7091082185075940902, 1.000000000000000000),
 ( 1.000000000000000000, 0.7071067811862460362, 1.000000000000000000) ) ) 
 REPRESENTATION_ITEM ( '' )  SURFACE ( )  );
#134005 = CARTESIAN_POINT ( 'NONE',  ( 3.004884002558502853, 1.492965937746863148, 0.9499605963744962578 ) ) ;
#134006 = CARTESIAN_POINT ( 'NONE',  ( 5.087059579022827904, -0.2656672225294122169, -2.190654145894948890 ) ) ;
#134007 = ORIENTED_EDGE ( 'NONE', *, *, #80476, .F. ) ;
#134008 = CARTESIAN_POINT ( 'NONE',  ( -6.961185525973791144, 7.086080966583015339, 0.7998128361456341429 ) ) ;
#134009 = CARTESIAN_POINT ( 'NONE',  ( 4.816029892389546596, 1.034148959857810190, -1.730877356967218894 ) ) ;
#134010 = ORIENTED_EDGE ( 'NONE', *, *, #20246, .T. ) ;
#134011 = CARTESIAN_POINT ( 'NONE',  ( 2.711613914024712191, -1.850561042518297672, 0.2725550856255419818 ) ) ;
#134012 = CARTESIAN_POINT ( 'NONE',  ( -8.068510813464099485, 8.585886501895810596, 0.7216878364870317197 ) ) ;
#134013 = CARTESIAN_POINT ( 'NONE',  ( 1.810667312839256304, -0.5133170510521027907, -1.842115474350584980 ) ) ;
#134014 = CARTESIAN_POINT ( 'NONE',  ( -3.765305043611756552, 7.354576300424668922, -0.6638232778202641793 ) ) ;
#134015 = CARTESIAN_POINT ( 'NONE',  ( -10.33433454857960321, 4.766519530047388820, -5.444264161973041638 ) ) ;
#134016 = CARTESIAN_POINT ( 'NONE',  ( -7.550983558724425393, -6.148216694138056049, 7.550983558724451150 ) ) ;
#134017 = CARTESIAN_POINT ( 'NONE',  ( 0.6823417656249899377, 4.988541667008086655, -1.181850606188754593 ) ) ;
#134018 = CARTESIAN_POINT ( 'NONE',  ( 0.7031954830387620037, 1.685401770928725007, -0.9037484838233383888 ) ) ;
#134019 = CARTESIAN_POINT ( 'NONE',  ( 6.211043768836181478, 7.379210830797944709, 1.082531754730549967 ) ) ;
#134020 = CARTESIAN_POINT ( 'NONE',  ( 1.592165322863370980, 0.9698756732311950568, -1.705302290208744687 ) ) ;
#134021 = CARTESIAN_POINT ( 'NONE',  ( -3.797692425159308716, 7.444741906078900406, 0.000000000000000000 ) ) ;
#134022 = CARTESIAN_POINT ( 'NONE',  ( -6.310394152517827315, 6.326824364217716656, 0.7998128361456281477 ) ) ;
#134023 = CARTESIAN_POINT ( 'NONE',  ( 5.396778611113259849, -2.069399493756381769, -0.4625044129713885011 ) ) ;
#134025 = SURFACE_STYLE_FILL_AREA ( #5019 ) ;
#134024 = CARTESIAN_POINT ( 'NONE',  ( 7.750457368506414646, 12.19395069656619945, 0.7998128361456462443 ) ) ;
#134026 = CARTESIAN_POINT ( 'NONE',  ( 6.116478573505100158, 1.325718183447884169, -1.459148498715772790 ) ) ;
#134027 = CARTESIAN_POINT ( 'NONE',  ( -1.364683531250000748, 2.009375000341421913, 1.214306433183764966E-14 ) ) ;
#134028 = CARTESIAN_POINT ( 'NONE',  ( 1.968995789680173303, -1.553632997376572566, 1.280276984777522165 ) ) ;
#134029 = ORIENTED_EDGE ( 'NONE', *, *, #183780, .T. ) ;
#134031 = CARTESIAN_POINT ( 'NONE',  ( 1.001738948178192645, -2.064706785862341132, 0.4679990497924620407 ) ) ;
#134030 = CARTESIAN_POINT ( 'NONE',  ( -8.351459436338048548, 8.845716885256940998, -0.7216878364870278340 ) ) ;
#134032 = CARTESIAN_POINT ( 'NONE',  ( 10.00007831732923691, 9.861607340972970093, 6.659929834790830228 ) ) ;
#134033 = CARTESIAN_POINT ( 'NONE',  ( 2.102089431743926706, 0.7944251937819692966, -1.912079865474418439 ) ) ;
#134034 = CARTESIAN_POINT ( 'NONE',  ( 3.393283585170187688, 7.180857625999046867, 0.7998128361456271485 ) ) ;
#134035 = CARTESIAN_POINT ( 'NONE',  ( 4.980641328173811999, 6.904110530993182948, 1.599625672291269396 ) ) ;
#134036 = EDGE_LOOP ( 'NONE', ( #185814, #105206, #124892, #14967 ) ) ;
#134038 = CARTESIAN_POINT ( 'NONE',  ( 5.678167406024951624, 5.518950149984223508, 0.7998128361456341429 ) ) ;
#134037 = CARTESIAN_POINT ( 'NONE',  ( 4.980460981504991835, -0.2552229379441274815, -2.074931007936396288 ) ) ;
#134041 = ORIENTED_EDGE ( 'NONE', *, *, #68597, .T. ) ;
#134040 = CARTESIAN_POINT ( 'NONE',  ( 2.596125760314275777, -0.9296622322433767405, 1.554548433350180225 ) ) ;
#134039 = CARTESIAN_POINT ( 'NONE',  ( 2.573050890253928635, 0.09191801231544714790, -1.823395950357763695 ) ) ;
#134042 = FACE_OUTER_BOUND ( 'NONE', #141916, .T. ) ;
#134043 = CARTESIAN_POINT ( 'NONE',  ( 9.350297026732835803, 12.83744219491209293, 6.612079693597346264 ) ) ;
#134044 = CARTESIAN_POINT ( 'NONE',  ( 5.544034191846948900, 0.8990280053539388971, -2.015528879820461583 ) ) ;
#134045 = CARTESIAN_POINT ( 'NONE',  ( 1.364683531249996529, 9.776041667008064096, 0.7879004041258403923 ) ) ;
#134046 = ORIENTED_EDGE ( 'NONE', *, *, #157427, .F. ) ;
#134047 = CARTESIAN_POINT ( 'NONE',  ( 3.440010667329951310, -1.141173813254949820, -1.534285795567114974 ) ) ;
#134049 = CARTESIAN_POINT ( 'NONE',  ( -4.406563619641430840, 5.099744630125142564, -1.199719254218446718 ) ) ;
#134048 = AXIS2_PLACEMENT_3D ( 'NONE', #102753, #120138, #116923 ) ;
#134050 =( BOUNDED_CURVE ( )  B_SPLINE_CURVE ( 3, ( #34383, #66851, #198996, #210991 ),
 .UNSPECIFIED., .F., .T. ) 
 B_SPLINE_CURVE_WITH_KNOTS ( ( 4, 4 ),
 ( 4.712388980384737636, 5.276666415325541593 ),
 .UNSPECIFIED. ) 
 CURVE ( )  GEOMETRIC_REPRESENTATION_ITEM ( )  RATIONAL_B_SPLINE_CURVE ( ( 1.000000000000000000, 0.9736414627471723371, 0.9736414627471723371, 1.000000000000000000 ) ) 
 REPRESENTATION_ITEM ( '' )  );
#134051 = CARTESIAN_POINT ( 'NONE',  ( 7.039708073993665494, 9.236078724457858158, 1.599625672291281386 ) ) ;
#134052 = CARTESIAN_POINT ( 'NONE',  ( 1.360316468749945606, 0.06770833367471427999, -0.7853790794159161148 ) ) ;
#134053 = CARTESIAN_POINT ( 'NONE',  ( 3.673896439178911066, 7.230036912443299713, 0.7216878364870317197 ) ) ;
#134054 = CARTESIAN_POINT ( 'NONE',  ( 4.204437033569277560, 7.919277282557212416, 0.000000000000000000 ) ) ;
#134055 = CARTESIAN_POINT ( 'NONE',  ( 3.469446951953614189E-15, 5.167241622962441383, 1.214306433183764966E-14 ) ) ;
#134056 = CARTESIAN_POINT ( 'NONE',  ( 0.6613494997313728030, 0.9071737413179328247, 1.602200521169500957 ) ) ;
#134057 = VERTEX_POINT ( 'NONE', #164932 ) ;
#134058 = DIRECTION ( 'NONE',  ( 0.000000000000000000, 1.000000000000000000, 0.000000000000000000 ) ) ;
#134059 = CARTESIAN_POINT ( 'NONE',  ( 3.497188413392815498, 1.472618687456558551, 1.153256759092120554 ) ) ;
#134060 = CARTESIAN_POINT ( 'NONE',  ( 5.982890925380405456, 10.20206618957764100, 0.000000000000000000 ) ) ;
#134061 = CARTESIAN_POINT ( 'NONE',  ( 10.62873463776380056, 9.799999999999982947, 3.199999999999997957 ) ) ;
#134062 = CARTESIAN_POINT ( 'NONE',  ( -5.422898255786186006, 9.270539031818461950, -0.7216878364870207285 ) ) ;
#134063 = CARTESIAN_POINT ( 'NONE',  ( 3.988069740714122791, 7.804498464141805592, 0.7998128361456321445 ) ) ;
#134064 = CARTESIAN_POINT ( 'NONE',  ( 0.5320047819624426078, 1.129344350875445935, 1.613283618269464981 ) ) ;
#134065 = CARTESIAN_POINT ( 'NONE',  ( 1.792592436991577109, 1.492242793082170449, -1.356315429364700176 ) ) ;
#134066 = CARTESIAN_POINT ( 'NONE',  ( -7.486073373039941359, 11.88550270185529278, -0.7998128361456291469 ) ) ;
#134067 = CARTESIAN_POINT ( 'NONE',  ( 5.342795052237045539, 8.390955439988655229, -1.199719254218450271 ) ) ;
#134068 =( NAMED_UNIT ( * ) SI_UNIT ( $, .STERADIAN. ) SOLID_ANGLE_UNIT ( ) );
#134069 = CARTESIAN_POINT ( 'NONE',  ( 2.326364362698669641, 2.126017103801054464, 0.5310240739047759062 ) ) ;
#134070 = CARTESIAN_POINT ( 'NONE',  ( 6.445924739416000193, 0.6936395621829589686, -1.688995215704327535 ) ) ;
#134071 = CARTESIAN_POINT ( 'NONE',  ( -3.002240950422295995, 5.590032644546251817, -1.199719254218452935 ) ) ;
#134072 = CARTESIAN_POINT ( 'NONE',  ( 6.061904079085887354, 6.244845311787889486, 0.000000000000000000 ) ) ;
#134073 = CARTESIAN_POINT ( 'NONE',  ( 9.908311333488716954, 10.45411806535867782, 0.7998128361456462443 ) ) ;
#134074 = CARTESIAN_POINT ( 'NONE',  ( 4.111146893441827821, 5.819424013814004759, 1.599625672291267398 ) ) ;
#134075 = CARTESIAN_POINT ( 'NONE',  ( 7.024532985656141371, 7.367912369453226695, 0.7216878364870328300 ) ) ;
#134076 = ORIENTED_EDGE ( 'NONE', *, *, #21017, .F. ) ;
#134078 = CARTESIAN_POINT ( 'NONE',  ( 0.4518146667342719525, -1.425121331298753402, -1.422066715514385349 ) ) ;
#134077 = CARTESIAN_POINT ( 'NONE',  ( 4.071694929070113211, -1.056692140236010102, 1.507659738195665788 ) ) ;
#134079 = CARTESIAN_POINT ( 'NONE',  ( 2.583761237542493205, 1.502156065388253081, -1.739619357585840520 ) ) ;
#134081 = CARTESIAN_POINT ( 'NONE',  ( 1.340418531419234505, -1.814007083311576451, -0.4145509422008378242 ) ) ;
#134080 = CARTESIAN_POINT ( 'NONE',  ( 2.385871846325007706, 5.727341554113725586, -0.7216878364870267237 ) ) ;
#134082 = CARTESIAN_POINT ( 'NONE',  ( 1.001543065824772753E-15, -0.6125000000000012657, 4.012584370867899430 ) ) ;
#134083 = CARTESIAN_POINT ( 'NONE',  ( -4.554649539187067830, 7.401175998105142817, 1.199719254218464037 ) ) ;
#134084 = CARTESIAN_POINT ( 'NONE',  ( 4.500206361630255003, -0.8965733778899236395, 1.689174240301967389 ) ) ;
#134085 = CARTESIAN_POINT ( 'NONE',  ( -7.458957065812611198, 11.85386701009007204, 0.7998128361456481317 ) ) ;
#134087 = EDGE_CURVE ( 'NONE', #77834, #160775, #173773, .T. ) ;
#134086 = CARTESIAN_POINT ( 'NONE',  ( 6.244837129360077732, 6.910362811036335096, 0.8058565020967979331 ) ) ;
#134088 = CARTESIAN_POINT ( 'NONE',  ( -6.699137298928187434, 8.909022496873262753, 1.443375672974064550 ) ) ;
#134090 = CARTESIAN_POINT ( 'NONE',  ( 2.026040307571222332, 1.079255042350239391, -1.527726335390042767 ) ) ;
#134089 = CARTESIAN_POINT ( 'NONE',  ( 3.491813360781896858, -2.088456202509383797, -0.1002299605681444133 ) ) ;
#134091 = CARTESIAN_POINT ( 'NONE',  ( 6.317736394288131052, 9.354147645769410602, 1.082531754730558626 ) ) ;
#134092 = CARTESIAN_POINT ( 'NONE',  ( 0.6823417656249899377, 5.488541667008087543, -1.181850606188754593 ) ) ;
#134093 = CARTESIAN_POINT ( 'NONE',  ( 3.544249451937312667, -1.420498570261208959, 1.005328601869423633 ) ) ;
#134094 = CARTESIAN_POINT ( 'NONE',  ( 4.578903193113299963, 6.365139696764064325, 1.599625672291267398 ) ) ;
#134095 = DIRECTION ( 'NONE',  ( 0.000000000000000000, 0.000000000000000000, -1.000000000000000000 ) ) ;
#134096 = CARTESIAN_POINT ( 'NONE',  ( 4.019902842142981214, -0.8889698729942583366, -1.477996400630256613 ) ) ;
#134097 = CARTESIAN_POINT ( 'NONE',  ( -7.552055258011950656, 8.769484874890757453, 1.199719254218462483 ) ) ;
#134098 = CARTESIAN_POINT ( 'NONE',  ( 6.393228082638676923, 1.922373441260841087, -1.083778638264052852 ) ) ;
#134099 = CARTESIAN_POINT ( 'NONE',  ( 0.7500000000000006661, 8.666666666666669627, -1.299038105676657340 ) ) ;
#134100 = CARTESIAN_POINT ( 'NONE',  ( 9.579089671862750066, -9.990657512341117652, -0.1108584966531479393 ) ) ;
#134101 = CARTESIAN_POINT ( 'NONE',  ( 3.098652014986380543, 2.154143853245940043, 0.2703130112568508103 ) ) ;
#134102 = CARTESIAN_POINT ( 'NONE',  ( 1.980809073483770000, -0.08854697198140694392, -1.823669195971427071 ) ) ;
#134103 = CARTESIAN_POINT ( 'NONE',  ( 1.499999999999993117, 12.35416666666666607, 0.8660254037844408170 ) ) ;
#134104 = CARTESIAN_POINT ( 'NONE',  ( 5.577400755804389654, 1.605162776699980753, 1.380938528300587276 ) ) ;
#134105 = ORIENTED_EDGE ( 'NONE', *, *, #143796, .F. ) ;
#134107 = CARTESIAN_POINT ( 'NONE',  ( 0.6823417656249899377, 3.238541667008085323, -1.181850606188754593 ) ) ;
#134106 = CARTESIAN_POINT ( 'NONE',  ( 5.741781754149911876, 2.289535525127144311, 0.1160191304092756254 ) ) ;
#134108 = CARTESIAN_POINT ( 'NONE',  ( 8.041957671200231417, 12.53403438304231976, 1.040834085586084257E-14 ) ) ;
#134109 = CARTESIAN_POINT ( 'NONE',  ( 1.348456458401224412, 1.042098076042829780, -1.846665823592225975 ) ) ;
#134110 = CARTESIAN_POINT ( 'NONE',  ( -3.945059511896602089, 7.546393830613923548, 1.040834085586084257E-14 ) ) ;
#134111 = CARTESIAN_POINT ( 'NONE',  ( 2.399429999938675007, 5.743159399996332404, 0.000000000000000000 ) ) ;
#134112 = CARTESIAN_POINT ( 'NONE',  ( -6.697364695026446491, 6.915939687060050467, 1.040834085586084257E-14 ) ) ;
#134113 = EDGE_CURVE ( 'NONE', #34907, #86477, #90744, .T. ) ;
#134114 = CARTESIAN_POINT ( 'NONE',  ( 6.069212964912024333, 1.910890531626436184, 1.030632506159581352 ) ) ;
#134116 = CARTESIAN_POINT ( 'NONE',  ( -1.402160292154681736E-14, 13.09375000068280315, 1.732050807568881190 ) ) ;
#134115 = CARTESIAN_POINT ( 'NONE',  ( -1.420000000000079865, 7.204077025658377487, 4.238769367544453992 ) ) ;
#134118 = ORIENTED_EDGE ( 'NONE', *, *, #193079, .T. ) ;
#134117 = CARTESIAN_POINT ( 'NONE',  ( 1.049838644336478000, -2.005893928647552116, 0.9545428114200222858 ) ) ;
#134119 = CARTESIAN_POINT ( 'NONE',  ( -0.06910031042392690559, -1.782763753708914267, -1.450585907311294775 ) ) ;
#134121 = CARTESIAN_POINT ( 'NONE',  ( 4.575086232891404592, 1.883663672660494504, 0.8406736911329756312 ) ) ;
#134120 = CARTESIAN_POINT ( 'NONE',  ( 5.172599298813543633, 5.993452922492633839, -1.199719254218452047 ) ) ;
#134123 = CARTESIAN_POINT ( 'NONE',  ( -5.763624699140883934, 6.857221916153382502, -1.082531754730549967 ) ) ;
#134122 = CARTESIAN_POINT ( 'NONE',  ( 5.345657705538078730, 9.458627433094950021, 0.7998128361456331437 ) ) ;
#134124 = CARTESIAN_POINT ( 'NONE',  ( 6.607619761813720238, 8.802252036906432764, 1.599625672291268286 ) ) ;
#134125 = CARTESIAN_POINT ( 'NONE',  ( 3.285556943750000514, -1.713541666188707735, 1.896917185911906500 ) ) ;
#134126 = CARTESIAN_POINT ( 'NONE',  ( -1.500000000000015099, 12.72916666666666785, -0.8660254037844309360 ) ) ;
#134127 = CARTESIAN_POINT ( 'NONE',  ( 0.6914939563917784637, -0.7507456521842426067, 1.951374281879012962 ) ) ;
#134128 = CARTESIAN_POINT ( 'NONE',  ( 5.098279808040273586, -0.2930726886911338425, 1.994869512123042199 ) ) ;
#134129 = CARTESIAN_POINT ( 'NONE',  ( 3.895923546780861724, -0.5813109859279729230, -1.747131793041277970 ) ) ;
#134130 = CARTESIAN_POINT ( 'NONE',  ( 5.854423403002611437, 5.724582146458163656, 1.040834085586084257E-14 ) ) ;
#134131 = SHAPE_REPRESENTATION_RELATIONSHIP ( 'NONE' , 'NONE' ,  #11178, #210156 ) ;
#134132 = CARTESIAN_POINT ( 'NONE',  ( 0.7622199101927947806, -1.253934870956091352, 1.184532473512718509 ) ) ;
#134133 = CARTESIAN_POINT ( 'NONE',  ( -0.06521966986864842497, -1.616690375843790273, 1.205047459138554045 ) ) ;
#134134 = CARTESIAN_POINT ( 'NONE',  ( 0.3703313985920617668, -0.2899475993979240274, -2.280306813078219363 ) ) ;
#134135 = CARTESIAN_POINT ( 'NONE',  ( -4.401593425930945713, 8.286942763561420122, 1.040834085586084257E-14 ) ) ;
#134136 = CARTESIAN_POINT ( 'NONE',  ( 1.493865258296807275, 1.713033017868152763, 1.477889207592040455 ) ) ;
#134137 = CARTESIAN_POINT ( 'NONE',  ( 3.000711368280566393, -0.6119465431162304236, -2.015196771704963030 ) ) ;
#134138 = CARTESIAN_POINT ( 'NONE',  ( -5.204350862799341115, 7.165104988056252289, -1.599625672291271394 ) ) ;
#134139 = CARTESIAN_POINT ( 'NONE',  ( 6.582647274634798151, 7.638508894284114170, 1.199719254218462483 ) ) ;
#134140 = CARTESIAN_POINT ( 'NONE',  ( 5.709392084686216506, 5.833581318321598985, -0.7216878364870458196 ) ) ;
#134141 = CARTESIAN_POINT ( 'NONE',  ( 6.218749999999983125, -0.7852924748301916003, 1.895863743164212467 ) ) ;
#134142 = CARTESIAN_POINT ( 'NONE',  ( -6.247609857798938293, 6.183299677053865295, -0.7998128361456291469 ) ) ;
#134143 = CARTESIAN_POINT ( 'NONE',  ( 1.499999999999989120, 2.275000000000019895, 1.214306433183764966E-14 ) ) ;
#134144 = CARTESIAN_POINT ( 'NONE',  ( -5.461236948206312114, 5.265864615862458464, 0.7998128361456341429 ) ) ;
#134145 = CARTESIAN_POINT ( 'NONE',  ( 4.570683916498400556, 0.8515115505445168820, 2.051917206062872978 ) ) ;
#134146 = CARTESIAN_POINT ( 'NONE',  ( 4.013774469618203611, -1.125877316280783358, -1.879984707117538845 ) ) ;
#134147 = CARTESIAN_POINT ( 'NONE',  ( -6.586563698140583512, 6.578745824119123675, 1.040834085586084257E-14 ) ) ;
#134148 = CARTESIAN_POINT ( 'NONE',  ( -11.94650005372637835, 9.948972996623616893, 1.135399707157293658 ) ) ;
#134149 = CARTESIAN_POINT ( 'NONE',  ( 0.6823417656249899377, 3.092708333674754062, 1.181850606188765695 ) ) ;
#134150 = CARTESIAN_POINT ( 'NONE',  ( 6.610000000000002096, 6.034162285353575683, 2.874900418788868262 ) ) ;
#134151 = CARTESIAN_POINT ( 'NONE',  ( -4.609409038966234995, 7.361099064560491456, -1.082531754730549967 ) ) ;
#134153 = CARTESIAN_POINT ( 'NONE',  ( 5.045234882716379765, 0.1584239314957915090, 2.114765283346302205 ) ) ;
#134152 = VECTOR ( 'NONE', #2402, 1000.000000000000000 ) ;
#134154 = CARTESIAN_POINT ( 'NONE',  ( -6.861835142292179057, 9.098836647464588978, 1.443375672974064550 ) ) ;
#134155 = VERTEX_POINT ( 'NONE', #82606 ) ;
#134157 = CARTESIAN_POINT ( 'NONE',  ( 6.227428301493934448, -2.037140905555033576, 0.7235935974677574212 ) ) ;
#134156 = CARTESIAN_POINT ( 'NONE',  ( -6.617788377246204945, 6.893376992974917350, -0.7216878364870338292 ) ) ;
#134158 = CARTESIAN_POINT ( 'NONE',  ( 6.006425746053997372, 6.966250444273174303, -1.199719254218445830 ) ) ;
#134159 = CARTESIAN_POINT ( 'NONE',  ( 4.792441439910442469, 1.527937338083688923, -1.027124420945782157 ) ) ;
#134160 = CARTESIAN_POINT ( 'NONE',  ( -0.6823417656250212460, 3.363541667008085323, 1.181850606188767472 ) ) ;
#134161 = CARTESIAN_POINT ( 'NONE',  ( 0.7315135518511396429, 1.714293348657709881, 0.2994600772705089953 ) ) ;
#134162 = DIRECTION ( 'NONE',  ( 0.000000000000000000, 0.000000000000000000, 1.000000000000000000 ) ) ;
#134163 = CARTESIAN_POINT ( 'NONE',  ( -0.5160254906862650204, 7.984099418343994614, 1.935262202534214548 ) ) ;
#134164 = CARTESIAN_POINT ( 'NONE',  ( -11.55950211276791428, 12.21999999999998288, 3.221476510067114329 ) ) ;
#134165 = CARTESIAN_POINT ( 'NONE',  ( 4.997027575558514734, 1.799266821141291661, -1.197868618907194316 ) ) ;
#134166 = CARTESIAN_POINT ( 'NONE',  ( -3.002240950422295995, 5.590032644546251817, -1.199719254218452935 ) ) ;
#134167 = CARTESIAN_POINT ( 'NONE',  ( -7.822691444960713447, 9.189190109618056823, -1.082531754730543083 ) ) ;
#134169 = AXIS2_PLACEMENT_3D ( 'NONE', #178622, #128873, #130995 ) ;
#134168 = VECTOR ( 'NONE', #174023, 1000.000000000000000 ) ;
#134170 = CARTESIAN_POINT ( 'NONE',  ( 4.206063578812153203, -2.156103337031569200, 0.1562769059922017589 ) ) ;
#134171 = CARTESIAN_POINT ( 'NONE',  ( -1.402160292154681736E-14, 2.446875000341416584, -1.575800808251660134 ) ) ;
#134172 = CARTESIAN_POINT ( 'NONE',  ( 6.116478573505100158, 1.325718183447884169, -1.459148498715772790 ) ) ;
#134173 = CARTESIAN_POINT ( 'NONE',  ( 5.466046595369183692, 1.418568314722228996, 0.9965602304959333413 ) ) ;
#134174 = CARTESIAN_POINT ( 'NONE',  ( 2.314256413632868714, 1.428969747754246233, -1.661726224907192684 ) ) ;
#134175 = CARTESIAN_POINT ( 'NONE',  ( 2.099037836983450589, -0.6160640708386398989, -2.223778577795953115 ) ) ;
#134176 = CARTESIAN_POINT ( 'NONE',  ( 4.587218493272061437, 1.842632243969796413, -0.9228815313185294578 ) ) ;
#134177 = CARTESIAN_POINT ( 'NONE',  ( 0.3748122768056568743, 1.812325467826606085, -0.6980362920307162655 ) ) ;
#134178 = CARTESIAN_POINT ( 'NONE',  ( -7.171900071504745178, 9.390302721554109056, -1.443375672974058777 ) ) ;
#134179 = CARTESIAN_POINT ( 'NONE',  ( -5.340986169140711226, 5.195848383611072485, 0.000000000000000000 ) ) ;
#134180 =( NAMED_UNIT ( * ) PLANE_ANGLE_UNIT ( ) SI_UNIT ( $, .RADIAN. ) );
#134181 = CARTESIAN_POINT ( 'NONE',  ( 1.231092510272915552, 2.014232830173094513, 0.09613330637052441840 ) ) ;
#134182 = CARTESIAN_POINT ( 'NONE',  ( -5.653386866774179786, 8.579073197003079798, 1.082531754730548412 ) ) ;
#134183 = CARTESIAN_POINT ( 'NONE',  ( 3.944505925199864649, 2.195883038551619038, 0.2190369969904403802 ) ) ;
#134184 = CARTESIAN_POINT ( 'NONE',  ( 1.642778471875000035, -1.713541666188707291, -2.845375778867859751 ) ) ;
#134185 = CARTESIAN_POINT ( 'NONE',  ( 1.393147051786493673, -1.685373162331062602, 0.7893452609444310264 ) ) ;
#134186 = CARTESIAN_POINT ( 'NONE',  ( -0.1288028175207089898, 5.718623287604398087, -2.868046808693432315 ) ) ;
#134187 = CARTESIAN_POINT ( 'NONE',  ( 1.469576158976824144E-15, 0.08000000000000020983, 12.00000000000000178 ) ) ;
#134188 = FACE_OUTER_BOUND ( 'NONE', #118617, .T. ) ;
#134190 = CARTESIAN_POINT ( 'NONE',  ( 6.825078400183544503, 6.034152930826206962, 2.739236550662868197 ) ) ;
#134189 = CARTESIAN_POINT ( 'NONE',  ( -5.328968068096138211, 7.722205811214136517, -1.323081262718794893 ) ) ;
#134191 = DIRECTION ( 'NONE',  ( 0.000000000000000000, 0.000000000000000000, -1.000000000000000000 ) ) ;
#134192 = EDGE_LOOP ( 'NONE', ( #42011, #141133, #191162, #124469 ) ) ;
#134193 = CARTESIAN_POINT ( 'NONE',  ( 3.871991401782824749, 1.143396993664235417, 1.714400680826788426 ) ) ;
#134194 = CARTESIAN_POINT ( 'NONE',  ( -1.360316468750042862, 1.869791667008058988, -0.7853790794158961308 ) ) ;
#134195 = CARTESIAN_POINT ( 'NONE',  ( -6.067437437315529536, 7.037430750744921859, 1.199719254218450271 ) ) ;
#134196 = CARTESIAN_POINT ( 'NONE',  ( 2.701824437540679469, 1.429832853698081108, 1.426684077065028422 ) ) ;
#134197 = CARTESIAN_POINT ( 'NONE',  ( 0.7499999999999885647, -0.01666666666664401442, 1.299038105676657340 ) ) ;
#134198 = CARTESIAN_POINT ( 'NONE',  ( 3.195971524519376494, 4.751719416737803847, -1.599625672291262513 ) ) ;
#134199 = CARTESIAN_POINT ( 'NONE',  ( 1.815377929200719720, -0.2531822047686766441, 2.045215655110666830 ) ) ;
#134201 = CARTESIAN_POINT ( 'NONE',  ( -1.402160292154681736E-14, 12.92187500034139980, 1.575800808251682339 ) ) ;
#134200 = CARTESIAN_POINT ( 'NONE',  ( -1.458777222063855294, 0.9000000000000014655, 1.713029193092652669 ) ) ;
#134202 = CARTESIAN_POINT ( 'NONE',  ( 7.142447996300871793, 7.227277505306155092, 0.7998128361456341429 ) ) ;
#134203 = AXIS2_PLACEMENT_3D ( 'NONE', #151486, #201260, #1987 ) ;
#134204 = CARTESIAN_POINT ( 'NONE',  ( -0.2411972340275865823, -0.002466136893032512371, -1.900252416837118208 ) ) ;
#134205 = CARTESIAN_POINT ( 'NONE',  ( 0.7261896124251127072, 0.1329856088156805560, 1.836402230816103209 ) ) ;
#134206 = CARTESIAN_POINT ( 'NONE',  ( 5.215527394842717435, -0.3265260713646127022, 2.182469266582609091 ) ) ;
#134207 = CARTESIAN_POINT ( 'NONE',  ( 4.538947565524982686, 8.517465603079630299, 0.000000000000000000 ) ) ;
#134208 = CARTESIAN_POINT ( 'NONE',  ( 1.265152180075890254, -1.953616520262021039, -0.9254636565915741464 ) ) ;
#134209 = CARTESIAN_POINT ( 'NONE',  ( -5.775410249741523394, 5.840326167560965231, 0.7216878364870317197 ) ) ;
#134210 = CARTESIAN_POINT ( 'NONE',  ( 1.833220611596135363, -1.622487599052296670, -1.197302888167578683 ) ) ;
#134211 = CARTESIAN_POINT ( 'NONE',  ( 2.038793776981039141, 2.199649879376049721, -0.6664975855598854748 ) ) ;
#134212 = ADVANCED_FACE ( 'NONE', ( #64242 ), #199324, .T. ) ;
#134213 = DIRECTION ( 'NONE',  ( 1.000000000000000000, -5.578564026256504688E-16, -0.000000000000000000 ) ) ;
#134214 = CARTESIAN_POINT ( 'NONE',  ( 0.1802491246630563426, -1.813337052076903877, -0.4591185353455888296 ) ) ;
#134215 = DIRECTION ( 'NONE',  ( 1.000000000000000000, 0.000000000000000000, -1.224646799147353207E-16 ) ) ;
#134216 = CARTESIAN_POINT ( 'NONE',  ( 2.113927203836548419, -0.8795192785214582809, -1.650985937663045577 ) ) ;
#134217 = CARTESIAN_POINT ( 'NONE',  ( 3.907435596788138010, -1.928258004016227378, 0.5899861904685861358 ) ) ;
#134219 = CARTESIAN_POINT ( 'NONE',  ( 10.52076401408022299, 11.37657222595619189, 0.000000000000000000 ) ) ;
#134218 = CARTESIAN_POINT ( 'NONE',  ( -1.201851678989727383E-14, 1.571875000341420581, 1.575800808251672791 ) ) ;
#134221 = CARTESIAN_POINT ( 'NONE',  ( 4.653012138262506703, -1.691843218806210247, 1.254050867608807129 ) ) ;
#134220 = CARTESIAN_POINT ( 'NONE',  ( -6.516665389662827934, 10.75452672124865217, 0.000000000000000000 ) ) ;
#134222 = CARTESIAN_POINT ( 'NONE',  ( 7.644099680006512187, 7.812537802962739697, 1.040834085586084257E-14 ) ) ;
#134223 = CARTESIAN_POINT ( 'NONE',  ( -7.121056995675673740, 9.330985799753529264, -1.599625672291263179 ) ) ;
#134224 = CARTESIAN_POINT ( 'NONE',  ( 6.539320575229278454, 3.689604457162498630, 2.617406275049142916 ) ) ;
#134225 = CARTESIAN_POINT ( 'NONE',  ( 5.695571270406009745, 1.864622851205568699, -0.7768453975713036641 ) ) ;
#134226 = CARTESIAN_POINT ( 'NONE',  ( -1.402160292154681736E-14, -1.256249999317182953, 1.732050807568877637 ) ) ;
#134227 = EDGE_CURVE ( 'NONE', #22322, #52415, #173164, .T. ) ;
#134228 = CARTESIAN_POINT ( 'NONE',  ( 0.6903719162679988752, 1.063636609032023950, -1.767059929103020677 ) ) ;
#134229 = CARTESIAN_POINT ( 'NONE',  ( 7.117667457494414762, 11.24776976714476184, 1.040834085586084257E-14 ) ) ;
#134230 = CARTESIAN_POINT ( 'NONE',  ( 5.481239241674765950, 9.616805891921051952, -0.7998128361456481317 ) ) ;
#134231 = CARTESIAN_POINT ( 'NONE',  ( 6.062430963966053632, 7.101866208495718702, -1.199719254218452047 ) ) ;
#134232 = CARTESIAN_POINT ( 'NONE',  ( -1.364683531250000748, 0.3218750003414205807, 0.000000000000000000 ) ) ;
#134234 = CARTESIAN_POINT ( 'NONE',  ( 8.773304256324777839, 3.742896273583256939, 7.826845210040881184 ) ) ;
#134233 = CARTESIAN_POINT ( 'NONE',  ( 4.016958651398847557, 7.908478536599129249, -0.7998128361456362523 ) ) ;
#134235 =( BOUNDED_CURVE ( )  B_SPLINE_CURVE ( 2, ( #48547, #15999, #178541, #29090, #82084 ),
 .UNSPECIFIED., .F., .T. ) 
 B_SPLINE_CURVE_WITH_KNOTS ( ( 3, 2, 3 ),
 ( 0.01079486483480432586, 0.01250000000000000069, 0.01382216642637611702 ),
 .UNSPECIFIED. ) 
 CURVE ( )  GEOMETRIC_REPRESENTATION_ITEM ( )  RATIONAL_B_SPLINE_CURVE ( ( 0.9352202683046952902, 0.9451732491399892355, 1.000000000000000000, 0.9574871888551572674, 0.9419547032718726953 ) ) 
 REPRESENTATION_ITEM ( '' )  );
#134236 = CARTESIAN_POINT ( 'NONE',  ( 5.788968402910802169, 8.737251655829183505, 1.082531754730558626 ) ) ;
#134238 = CARTESIAN_POINT ( 'NONE',  ( -5.300029851643866863, 4.752152409900321395, -2.500000000000000444 ) ) ;
#134237 = CARTESIAN_POINT ( 'NONE',  ( 2.611994278460927799, 0.5808993838645438723, -2.091943403374715515 ) ) ;
#134240 = CARTESIAN_POINT ( 'NONE',  ( 2.471991059931688106, -1.762569054296094340, -0.5325411743367302053 ) ) ;
#134239 = CARTESIAN_POINT ( 'NONE',  ( -4.934804725694224459, 6.780358151441803649, -1.443375672974053447 ) ) ;
#134241 = CARTESIAN_POINT ( 'NONE',  ( -1.201851678989727383E-14, 3.571875000341422357, 1.575800808251672791 ) ) ;
#134242 = CARTESIAN_POINT ( 'NONE',  ( 3.948915171154475878, -1.822730400009948237, -1.216494452853926322 ) ) ;
#134243 = CARTESIAN_POINT ( 'NONE',  ( 8.142236001222203257, 14.23929044818452994, 8.815766320197676365 ) ) ;
#134244 = CARTESIAN_POINT ( 'NONE',  ( 5.260715670973223901, -1.642634774727338653, 1.556112085687613611 ) ) ;
#134245 = CARTESIAN_POINT ( 'NONE',  ( -4.391951695823077984, 7.211361847513815704, 1.199719254218464037 ) ) ;
#134247 = AXIS2_PLACEMENT_3D ( 'NONE', #14128, #29348, #161493 ) ;
#134246 = CARTESIAN_POINT ( 'NONE',  ( 0.1021010164683408550, 6.424493866598983693, -3.065991822131907352 ) ) ;
#134248 = CARTESIAN_POINT ( 'NONE',  ( 5.142555292688428814, 7.778213139218437711, -1.168464917166486039 ) ) ;
#134249 = CARTESIAN_POINT ( 'NONE',  ( -5.099275172071237705, 8.963255110809500437, 0.000000000000000000 ) ) ;
#134250 = CARTESIAN_POINT ( 'NONE',  ( 3.580761967785000888, 7.191656372475549119, -0.7216878364870338292 ) ) ;
#134251 = CARTESIAN_POINT ( 'NONE',  ( 6.503183016764070068, 1.472852356768614479, 0.9808112332466749628 ) ) ;
#134252 = CARTESIAN_POINT ( 'NONE',  ( 3.932292794061467589, -1.036904606752734326, -1.725386108540658103 ) ) ;
#134253 = CARTESIAN_POINT ( 'NONE',  ( 7.806797523370503811, 8.002351953554066810, 1.040834085586084257E-14 ) ) ;
#134254 = CARTESIAN_POINT ( 'NONE',  ( 2.942513229011092690, 2.089901898437613870, 0.2590637233205703716 ) ) ;
#134255 = CARTESIAN_POINT ( 'NONE',  ( 0.6674275129862971001, 1.287417287929611076, 1.418633514309353583 ) ) ;
#134258 = EDGE_CURVE ( 'NONE', #193413, #2249, #95651, .T. ) ;
#134257 = CARTESIAN_POINT ( 'NONE',  ( -1.402160292154681736E-14, 2.337500000000022560, -1.732050807568863648 ) ) ;
#134256 = CARTESIAN_POINT ( 'NONE',  ( 1.364683531249996529, 11.96354166700806765, 0.7879004041258405033 ) ) ;
#134259 = CARTESIAN_POINT ( 'NONE',  ( 2.576555279139204568, 1.288776560207754551, -1.489423508990360023 ) ) ;
#134260 = CARTESIAN_POINT ( 'NONE',  ( 0.000000000000000000, -6.893137084989842123, 0.000000000000000000 ) ) ;
#134261 = CARTESIAN_POINT ( 'NONE',  ( 0.6605093422152423788, -0.6574743052488278838, -1.848563176889833626 ) ) ;
#134263 = ORIENTED_EDGE ( 'NONE', *, *, #142048, .F. ) ;
#134262 = CARTESIAN_POINT ( 'NONE',  ( 0.5977379272000953314, 1.286164058678052946, 1.415416067018962165 ) ) ;
#134264 = CARTESIAN_POINT ( 'NONE',  ( 5.612712406377503349, 8.531619659873665995, -1.082531754730543083 ) ) ;
#134265 = CARTESIAN_POINT ( 'NONE',  ( -1.364683531250014514, 0.09270833367475767028, 0.7879004041258379498 ) ) ;
#134266 = CARTESIAN_POINT ( 'NONE',  ( 5.559403950928493821, 0.3636877230743483236, -1.834782481876767291 ) ) ;
#134267 = CYLINDRICAL_SURFACE ( 'NONE', #96489, 0.09999999999999971412 ) ;
#134268 = CARTESIAN_POINT ( 'NONE',  ( 5.840704046183605946, -2.018525344099521668, -0.4591754850708437696 ) ) ;
#134269 = CARTESIAN_POINT ( 'NONE',  ( 10.10493793804581131, 0.9691415390508739680, 6.281047173807365880 ) ) ;
#134270 = CARTESIAN_POINT ( 'NONE',  ( -3.648552735408990166, 6.310376387068841630, -1.082531754730546636 ) ) ;
#134271 = CARTESIAN_POINT ( 'NONE',  ( 0.2388460773940295212, -2.007853281042128568, -0.5044432775610437902 ) ) ;
#134272 = CARTESIAN_POINT ( 'NONE',  ( 0.7499999999999867883, 0.06666666666668707997, -1.299038105676652899 ) ) ;
#134273 = CARTESIAN_POINT ( 'NONE',  ( 7.298366762858032430, 7.409182732956175244, 1.040834085586084257E-14 ) ) ;
#134274 = CARTESIAN_POINT ( 'NONE',  ( -9.287498920561160887, 10.79416914786490089, -1.199719254218441611 ) ) ;
#134275 = CARTESIAN_POINT ( 'NONE',  ( 6.204791576909545192, 7.267953590263130259, -1.199719254218452047 ) ) ;
#134276 = ADVANCED_FACE ( 'NONE', ( #148691 ), #102554, .T. ) ;
#134277 = CARTESIAN_POINT ( 'NONE',  ( 1.364683531249986537, 1.113541667008082658, 0.7879004041258500513 ) ) ;
#134278 = ORIENTED_EDGE ( 'NONE', *, *, #150154, .T. ) ;
#134279 = EDGE_CURVE ( 'NONE', #73634, #139957, #211871, .T. ) ;
#134280 = CARTESIAN_POINT ( 'NONE',  ( 1.499999999999989120, 2.754166666666688190, 0.8660254037844524744 ) ) ;
#134282 = CARTESIAN_POINT ( 'NONE',  ( 3.472859903394816872, 7.203420320602605287, -0.7998128361456291469 ) ) ;
#134281 = CARTESIAN_POINT ( 'NONE',  ( 4.738696794244872557, -1.902450960283699199, -0.4786090228221794307 ) ) ;
#134283 = CARTESIAN_POINT ( 'NONE',  ( 2.706407486732204326, -1.492025830231600070, -1.356093404896424826 ) ) ;
#134284 = CARTESIAN_POINT ( 'NONE',  ( 2.870226655882984090, -1.888176233477338872, -0.3226071530259622677 ) ) ;
#134285 = CARTESIAN_POINT ( 'NONE',  ( -1.904329973710263246, 3.286760881231379106, -0.4119279214153201973 ) ) ;
#134286 = CARTESIAN_POINT ( 'NONE',  ( -0.07626876867936756288, -1.353788312843669406, -1.724171373301164767 ) ) ;
#134287 = CARTESIAN_POINT ( 'NONE',  ( 0.1331715793776418189, 2.029267568408019695, -2.369146612602909041 ) ) ;
#134288 = CARTESIAN_POINT ( 'NONE',  ( 3.778450875046265534, -1.801938340082277712, -0.5016190811713144848 ) ) ;
#134289 = CARTESIAN_POINT ( 'NONE',  ( -1.402160292154681736E-14, -0.2562499993171780122, 1.732050807568877637 ) ) ;
#134290 = CARTESIAN_POINT ( 'NONE',  ( -7.694415870955439551, 8.935572256658169010, 1.199719254218462483 ) ) ;
#134292 = CARTESIAN_POINT ( 'NONE',  ( 4.429392955138825805, -1.637772332673973485, -1.341807030983455773 ) ) ;
#134291 = CARTESIAN_POINT ( 'NONE',  ( -4.609409038966245653, 6.400729850259146758, -1.443375672974053447 ) ) ;
#134293 = CARTESIAN_POINT ( 'NONE',  ( 6.092251258522619395, 1.023830597077223903, -1.799436568697235783 ) ) ;
#134295 = CARTESIAN_POINT ( 'NONE',  ( 6.620655732516642189, 2.417337544263608251, 2.554705107920357321 ) ) ;
#134294 = CARTESIAN_POINT ( 'NONE',  ( 1.962552558803489555, -1.912825090402545225, -0.8444004386199343015 ) ) ;
#134297 = ORIENTED_EDGE ( 'NONE', *, *, #180525, .F. ) ;
#134296 = CARTESIAN_POINT ( 'NONE',  ( 0.6215558277854142943, -0.9165932506310509043, -1.460862699585960822 ) ) ;
#134298 = CARTESIAN_POINT ( 'NONE',  ( 5.126954644262057492, 9.133197518281081173, 0.7998128361456462443 ) ) ;
#134299 = SURFACE_SIDE_STYLE ('',( #164635 ) ) ;
#134300 = CARTESIAN_POINT ( 'NONE',  ( -0.09053139919707911543, -9.918143888366140359, -9.499568811299521798 ) ) ;
#134301 =( NAMED_UNIT ( * ) PLANE_ANGLE_UNIT ( ) SI_UNIT ( $, .RADIAN. ) );
#134302 = CARTESIAN_POINT ( 'NONE',  ( 6.277061933002777927, 8.346324893301817482, 1.443375672974076540 ) ) ;
#134303 = CARTESIAN_POINT ( 'NONE',  ( -1.907519672996887294, 3.236073672982363369, 0.4612874649729363785 ) ) ;
#134305 = CARTESIAN_POINT ( 'NONE',  ( 0.3811517019768875802, 0.1791931900220759266, -1.802556192996515705 ) ) ;
#134304 = CARTESIAN_POINT ( 'NONE',  ( 6.424584688029230328, 8.588711117491191871, 1.599625672291268286 ) ) ;
#134306 = CARTESIAN_POINT ( 'NONE',  ( -7.344766530301162000, 9.591980256816594164, 1.599625672291295375 ) ) ;
#134307 = AXIS2_PLACEMENT_3D ( 'NONE', #150324, #101557, #134095 ) ;
#134308 = CARTESIAN_POINT ( 'NONE',  ( 5.192936529234042808, 6.017179691316550283, -1.199719254218452047 ) ) ;
#134309 = CARTESIAN_POINT ( 'NONE',  ( -5.244114872543307548, 7.700386654371578210, 1.209007019071134170 ) ) ;
#134310 = CARTESIAN_POINT ( 'NONE',  ( 6.770317605177710085, 8.992066187497757213, 1.599625672291268286 ) ) ;
#134311 = CARTESIAN_POINT ( 'NONE',  ( 10.75000000000000000, 1.316495309083404618E-15, 0.000000000000000000 ) ) ;
#134312 = CARTESIAN_POINT ( 'NONE',  ( 4.128490713069958851, 7.423566268403333446, -0.7082486411538677640 ) ) ;
#134313 = CARTESIAN_POINT ( 'NONE',  ( 10.05978679165993839, 10.83876546646586014, 0.7216878364870438212 ) ) ;
#134314 = ORIENTED_EDGE ( 'NONE', *, *, #127920, .F. ) ;
#134315 = CARTESIAN_POINT ( 'NONE',  ( 0.7201576878450620667, 1.887430420354209160, 0.3262839321072578125 ) ) ;
#134316 = CARTESIAN_POINT ( 'NONE',  ( 0.01256502854718108061, -2.120115106878577294, -0.04748564598491820943 ) ) ;
#134317 =( LENGTH_UNIT ( ) NAMED_UNIT ( * ) SI_UNIT ( .MILLI., .METRE. ) );
#134319 =( GEOMETRIC_REPRESENTATION_CONTEXT ( 3 ) GLOBAL_UNCERTAINTY_ASSIGNED_CONTEXT ( ( #64590 ) ) GLOBAL_UNIT_ASSIGNED_CONTEXT ( ( #63100, #193092, #196306 ) ) REPRESENTATION_CONTEXT ( 'NONE', 'WORKASPACE' ) );
#134318 = AXIS2_PLACEMENT_3D ( 'NONE', #103986, #5368, #205726 ) ;
#134320 = CARTESIAN_POINT ( 'NONE',  ( 0.6124999999999707345, 1.395833334016133298, 1.060881119635904923 ) ) ;
#134321 = CARTESIAN_POINT ( 'NONE',  ( 1.812896364438529417, 2.514517768406685061, 2.499891510452758592 ) ) ;
#134322 = CARTESIAN_POINT ( 'NONE',  ( -5.422898255786209099, 5.429062174613087599, -0.7216878364870207285 ) ) ;
#134323 = CARTESIAN_POINT ( 'NONE',  ( 9.897088948295946764, 10.64895131587453569, 0.7216878364870438212 ) ) ;
#134324 = CARTESIAN_POINT ( 'NONE',  ( 3.784006971647640327, -1.169605039944806357, -1.584395421511639812 ) ) ;
#134325 = CARTESIAN_POINT ( 'NONE',  ( 1.260569961473339440, 2.118219532560499996, 0.1004958096475216667 ) ) ;
#134326 = CARTESIAN_POINT ( 'NONE',  ( -6.742482464697739708, 6.760651051769146491, 0.7998128361456341429 ) ) ;
#134327 = CARTESIAN_POINT ( 'NONE',  ( -1.193489751472043232E-16, 4.500000000000003553, 2.150000000000006573 ) ) ;
#134328 = CARTESIAN_POINT ( 'NONE',  ( -0.7500000000000179856, 10.29166666666667140, 1.299038105676658228 ) ) ;
#134329 = CARTESIAN_POINT ( 'NONE',  ( 5.859372887940716090, 2.159598860408561194, -0.3713886045505072064 ) ) ;
#134330 = DIRECTION ( 'NONE',  ( 0.000000000000000000, 1.000000000000000000, 0.000000000000000000 ) ) ;
#134331 = CARTESIAN_POINT ( 'NONE',  ( 3.733351708207183428, -1.780342035418970736, 0.7362343730293962052 ) ) ;
#134332 = CARTESIAN_POINT ( 'NONE',  ( -7.157815033010924921, 10.43820240756634199, 1.199719254218453823 ) ) ;
#134333 = LINE ( 'NONE', #112792, #55216 ) ;
#134334 = CARTESIAN_POINT ( 'NONE',  ( 1.489210700298746692, -0.3264265768355456565, -2.182489157894373033 ) ) ;
#134335 = CARTESIAN_POINT ( 'NONE',  ( 0.000000000000000000, -7.154544010627095219, 0.000000000000000000 ) ) ;
#134336 = ORIENTED_EDGE ( 'NONE', *, *, #162394, .F. ) ;
#134337 = CARTESIAN_POINT ( 'NONE',  ( 3.851925040058331806, 5.587274861525073355, -1.443375672974066548 ) ) ;
#134338 = ORIENTED_EDGE ( 'NONE', *, *, #15120, .T. ) ;
#134339 = CARTESIAN_POINT ( 'NONE',  ( 5.700047960291365179, 0.8015925475840814940, -1.799137058317602067 ) ) ;
#134340 = CARTESIAN_POINT ( 'NONE',  ( -0.07675543424010172755, -1.195724141806488561, -1.531021551883532172 ) ) ;
#134341 = CARTESIAN_POINT ( 'NONE',  ( 6.151801744867631427, -0.3282927394851458125, -2.274731023314037870 ) ) ;
#134343 = CARTESIAN_POINT ( 'NONE',  ( 4.188223417972539053, 0.9984873940180930552, -1.570204455898941420 ) ) ;
#134342 = CARTESIAN_POINT ( 'NONE',  ( -6.851666526859749418, 9.086973262793417661, -1.599625672291271394 ) ) ;
#134344 = CARTESIAN_POINT ( 'NONE',  ( 6.119526231721748033, 8.232809585132461194, 1.599625672291269396 ) ) ;
#134345 = DIRECTION ( 'NONE',  ( 7.610300982150707428E-15, -1.000000000000000000, -7.722633184682877167E-15 ) ) ;
#134346 = SURFACE_STYLE_FILL_AREA ( #3208 ) ;
#134347 = CARTESIAN_POINT ( 'NONE',  ( -5.032047568966410367, 9.022472597102808578, 1.214306433183764966E-14 ) ) ;
#134348 = EDGE_CURVE ( 'NONE', #149119, #197280, #170445, .T. ) ;
#134349 = CARTESIAN_POINT ( 'NONE',  ( 6.720655732516625847, 7.629137130509076492, 2.426260288887295058 ) ) ;
#134350 = CARTESIAN_POINT ( 'NONE',  ( 6.620655732516666170, 0.0004550665020433551948, 2.073887158236031425 ) ) ;
#134351 = CARTESIAN_POINT ( 'NONE',  ( 5.504247177468186258, 6.484338464210099851, 1.082531754730558626 ) ) ;
#134352 = ORIENTED_EDGE ( 'NONE', *, *, #39650, .F. ) ;
#134353 = CARTESIAN_POINT ( 'NONE',  ( 10.99374989157287885, -6.893136995915043919, -0.3811408430856385587 ) ) ;
#134354 = DIRECTION ( 'NONE',  ( 0.000000000000000000, 0.000000000000000000, -1.000000000000000000 ) ) ;
#134355 = CARTESIAN_POINT ( 'NONE',  ( 0.2229205655521030172, -0.09321834626660817358, 1.823428419517532983 ) ) ;
#134356 = CARTESIAN_POINT ( 'NONE',  ( -2.937312835655025101, 6.578615408239493867, 1.040834085586084257E-14 ) ) ;
#134357 = CARTESIAN_POINT ( 'NONE',  ( 3.129275142338799665, 0.4248101585269374869, 1.681139380183617194 ) ) ;
#134358 = FACE_OUTER_BOUND ( 'NONE', #110399, .T. ) ;
#134359 = CARTESIAN_POINT ( 'NONE',  ( -5.019912524233729911, 4.821262464552921401, 0.2549627792466685472 ) ) ;
#134360 = CARTESIAN_POINT ( 'NONE',  ( 0.4408745273426888933, 3.070687961115777131, 0.4190752896376094827 ) ) ;
#134361 = CARTESIAN_POINT ( 'NONE',  ( 6.709597972018079837, -0.3944863986210072060, 1.789098616620278470 ) ) ;
#134362 = CARTESIAN_POINT ( 'NONE',  ( 3.889464431383614862, -1.814284039448841979, 0.7467176931179178023 ) ) ;
#134363 = MECHANICAL_DESIGN_GEOMETRIC_PRESENTATION_REPRESENTATION (  '', ( #213917 ), #113682 ) ;
#134364 = CARTESIAN_POINT ( 'NONE',  ( -3.755786496842897795E-14, -0.3749999993171817536, 1.414508159514569430 ) ) ;
#134365 = CARTESIAN_POINT ( 'NONE',  ( -10.17947440576205054, 10.77047498301088346, 0.7998128361456462443 ) ) ;
#134366 = CARTESIAN_POINT ( 'NONE',  ( 6.799577732453452761, 7.891594428405881878, -1.199719254218446718 ) ) ;
#134367 = CARTESIAN_POINT ( 'NONE',  ( 5.057343377742961721, -1.818460011135439869, 1.090507627184752693 ) ) ;
#134368 = ADVANCED_FACE ( 'NONE', ( #4526 ), #185435, .T. ) ;
#134369 = CARTESIAN_POINT ( 'NONE',  ( 7.842465510862060896, 8.114240948952696542, 0.000000000000000000 ) ) ;
#134370 = CARTESIAN_POINT ( 'NONE',  ( -7.947050595904583403, 12.42330946186405249, 0.7998128361456481317 ) ) ;
#134371 = CARTESIAN_POINT ( 'NONE',  ( 2.993098612437725681, 0.2488643248897918769, 2.055149816265568585 ) ) ;
#134373 = CARTESIAN_POINT ( 'NONE',  ( -1.364683531250014514, -0.1989583329919157317, -0.7879004041258359514 ) ) ;
#134372 = CARTESIAN_POINT ( 'NONE',  ( 0.000000000000000000, 13.20000000000000284, 0.000000000000000000 ) ) ;
#134375 = ORIENTED_EDGE ( 'NONE', *, *, #5890, .F. ) ;
#134374 = CARTESIAN_POINT ( 'NONE',  ( 4.547657996348432263, -2.031006315926532135, 0.8999586162586125093 ) ) ;
#134376 = CARTESIAN_POINT ( 'NONE',  ( 2.866213343745026343, -0.1723225051825111875, -2.292302961975992037 ) ) ;
#134377 = CARTESIAN_POINT ( 'NONE',  ( 6.792271770766432404, 10.86814146596211472, 1.040834085586084257E-14 ) ) ;
#134379 = CARTESIAN_POINT ( 'NONE',  ( 3.285556943750000070, -2.734374999522042771, 0.000000000000000000 ) ) ;
#134378 = CARTESIAN_POINT ( 'NONE',  ( 7.404161286838808920, 8.771181268467660885, -1.082531754730548412 ) ) ;
#134380 = CARTESIAN_POINT ( 'NONE',  ( 7.777967379493318845, -9.999999999999994671, 7.664830294503448549 ) ) ;
#134381 = DIRECTION ( 'NONE',  ( 0.6507913734559627184, -0.7592566023653016805, 0.000000000000000000 ) ) ;
#134382 = EDGE_LOOP ( 'NONE', ( #69503, #32644, #120388, #68335 ) ) ;
#134383 = CARTESIAN_POINT ( 'NONE',  ( -5.436165250227197987, 6.300106160968032221, -1.040272029539757170 ) ) ;
#134384 = CARTESIAN_POINT ( 'NONE',  ( 3.937688585161042809, -1.828529804631402023, 0.5600222464785462595 ) ) ;
#134385 = CARTESIAN_POINT ( 'NONE',  ( -3.511198596259295535, 6.271927390929313617, -2.420000000000000373 ) ) ;
#134386 = CARTESIAN_POINT ( 'NONE',  ( 4.805503449324158183, -0.4579143662744952770, 1.662777411968613839 ) ) ;
#134387 = CARTESIAN_POINT ( 'NONE',  ( 2.958220528980559205, -1.197304571117228100, 1.622486353517027968 ) ) ;
#134388 = CARTESIAN_POINT ( 'NONE',  ( 4.237165586469007650, 2.298153656159235503, -0.05646909981197979073 ) ) ;
#134389 = FACE_OUTER_BOUND ( 'NONE', #44400, .T. ) ;
#134390 = CARTESIAN_POINT ( 'NONE',  ( 6.463511354401173747, 0.3618736704080193212, -2.074577690073164060 ) ) ;
#134391 = CARTESIAN_POINT ( 'NONE',  ( -4.773879485787619892, 7.623257595843924150, 1.082531754730549967 ) ) ;
#134392 = CARTESIAN_POINT ( 'NONE',  ( 5.870295291196549137, -1.121585077578592049, 1.368893044642209178 ) ) ;
#134394 = CARTESIAN_POINT ( 'NONE',  ( 1.658568045375780731, -1.618562549950094187, 1.623430423404078837 ) ) ;
#134393 = CARTESIAN_POINT ( 'NONE',  ( 6.170896192875352959, 7.228408975556602556, 1.199719254218453823 ) ) ;
#134395 = CARTESIAN_POINT ( 'NONE',  ( 0.1283017097272065865, -1.593451896579937355, 0.7002181395190426594 ) ) ;
#134396 = CARTESIAN_POINT ( 'NONE',  ( -8.120407659942227241, 8.438506789546210030, 0.7998128361456341429 ) ) ;
#134397 = AXIS2_PLACEMENT_3D ( 'NONE', #142768, #27910, #160046 ) ;
#134398 = CARTESIAN_POINT ( 'NONE',  ( 11.78331023100045627, 11.29999999999999893, -1.800000000000001155 ) ) ;
#134399 = CARTESIAN_POINT ( 'NONE',  ( -2.830620210203090181, 6.524417021870718258, 0.000000000000000000 ) ) ;
#134400 = CARTESIAN_POINT ( 'NONE',  ( 0.6801582343749970061, -0.1614583329919219712, -1.178068619123852079 ) ) ;
#134401 = CARTESIAN_POINT ( 'NONE',  ( 2.969872605471104876, 6.605953636086679737, -0.06813560672779371552 ) ) ;
#134402 = CARTESIAN_POINT ( 'NONE',  ( 6.637176860265922684, -0.09746846054551477900, -2.068182370504913159 ) ) ;
#134403 = CARTESIAN_POINT ( 'NONE',  ( 1.481658059775035952, -0.6748446255696785023, 1.900416712880992343 ) ) ;
#134404 = CARTESIAN_POINT ( 'NONE',  ( -1.500000000000013101, -0.04791666598384902026, 0.8660254037844403729 ) ) ;
#134405 = CARTESIAN_POINT ( 'NONE',  ( 5.619733630554700099, -1.879067156935828820, 0.4242066570522682878 ) ) ;
#134406 = CARTESIAN_POINT ( 'NONE',  ( 0.6823417656249969321, 12.27604166700806054, -1.181850606188757036 ) ) ;
#134407 = CARTESIAN_POINT ( 'NONE',  ( 2.074768627854159053, 0.9548037322763336388, 2.005906060693471993 ) ) ;
#134408 = EDGE_LOOP ( 'NONE', ( #195560, #38107, #72894, #30285 ) ) ;
#134410 = CARTESIAN_POINT ( 'NONE',  ( 0.1460981902779634745, 7.101100029736093333, -2.114500818361211287 ) ) ;
#134409 = CARTESIAN_POINT ( 'NONE',  ( 6.116136693540529912, 10.14959355252369910, 1.530808498934192557E-16 ) ) ;
#134411 = CARTESIAN_POINT ( 'NONE',  ( -3.469446951953614189E-15, 8.999999999999998224, -0.7749999999999996891 ) ) ;
#134412 = CARTESIAN_POINT ( 'NONE',  ( 8.757677159423465696, 12.30470822171437284, 1.199719254218450271 ) ) ;
#134413 = DIRECTION ( 'NONE',  ( -0.000000000000000000, 1.000000000000000000, -0.000000000000000000 ) ) ;
#134414 = AXIS2_PLACEMENT_3D ( 'NONE', #197332, #122586, #168040 ) ;
#134415 = CARTESIAN_POINT ( 'NONE',  ( 4.018918099032080526, -1.663992213871115178, 0.5101021115980988174 ) ) ;
#134416 = CARTESIAN_POINT ( 'NONE',  ( 2.646866301197240645, -0.3325320220872363675, -1.933311746529025266 ) ) ;
#134418 = CARTESIAN_POINT ( 'NONE',  ( -7.212574532790102744, 8.477387045419011002, -1.082531754730550855 ) ) ;
#134417 = CARTESIAN_POINT ( 'NONE',  ( 3.551346171775753735, 6.230655402791975384, 1.199719254218462483 ) ) ;
#134419 = EDGE_CURVE ( 'NONE', #28009, #78671, #201668, .T. ) ;
#134420 = CARTESIAN_POINT ( 'NONE',  ( -5.894595317363360287, 6.010551413984606128, 0.2245382864616944640 ) ) ;
#134421 = CARTESIAN_POINT ( 'NONE',  ( -1.737500000000000266, -2.114583332377416802, -3.009438278150923907 ) ) ;
#134422 = CARTESIAN_POINT ( 'NONE',  ( 1.117717378214663881, 0.4042816502292169711, -2.022510655824232728 ) ) ;
#134423 = CARTESIAN_POINT ( 'NONE',  ( -6.659026002606323047, 10.92061410301605662, 0.000000000000000000 ) ) ;
#134424 = CARTESIAN_POINT ( 'NONE',  ( -4.161989969270909917, 5.878740935614591656, 1.443375672974064550 ) ) ;
#134425 = CARTESIAN_POINT ( 'NONE',  ( 1.429016818436980474, 2.180957219565873295, 0.6017249355739097139 ) ) ;
#134426 = ORIENTED_EDGE ( 'NONE', *, *, #90488, .F. ) ;
#134427 = CARTESIAN_POINT ( 'NONE',  ( 1.499999999999987121, 0.5354166673494816786, 0.8660254037844524744 ) ) ;
#134428 = CARTESIAN_POINT ( 'NONE',  ( 2.846779338809723559, -1.557328454271855955, 1.035869100625155470 ) ) ;
#134429 = CARTESIAN_POINT ( 'NONE',  ( 1.371252568922965098, -0.2536805693413109464, -1.715349781374966742 ) ) ;
#134430 = CARTESIAN_POINT ( 'NONE',  ( 5.442994344319362021, -1.727133847215430729, -1.348975639928217118 ) ) ;
#134431 = CARTESIAN_POINT ( 'NONE',  ( 5.350698970897345141, 0.6634653876971875475, 2.210164229930264845 ) ) ;
#134432 = B_SPLINE_CURVE_WITH_KNOTS ( 'NONE', 3,
 ( #85786, #120502, #199513, #51158, #103107, #104181, #69508 ),
 .UNSPECIFIED., .F., .F.,
 ( 4, 3, 4 ),
 ( 6.824963372777353392E-15, 6.253410770929631051E-05, 0.0001562177157599490304 ),
 .UNSPECIFIED. ) ;
#134433 = CARTESIAN_POINT ( 'NONE',  ( 1.428666007085793277, 1.985871523383303749, 0.5506756191897729247 ) ) ;
#134434 = CARTESIAN_POINT ( 'NONE',  ( 3.732312008210575627, 0.2860496425412931143, 1.920654750396868726 ) ) ;
#134435 = CARTESIAN_POINT ( 'NONE',  ( -3.402733366905605905, 6.913679994791092298, 0.7216878364870317197 ) ) ;
#134436 = CARTESIAN_POINT ( 'NONE',  ( 5.676977070516882051, -0.04517083460114229565, -1.870152005306220611 ) ) ;
#134437 = CARTESIAN_POINT ( 'NONE',  ( 1.414375913850415278, 13.32373988190677139, 0.1231264505149970989 ) ) ;
#134438 = CARTESIAN_POINT ( 'NONE',  ( 6.766953912288387940, -2.015720078709513086, 0.04667315333419658208 ) ) ;
#134439 = CARTESIAN_POINT ( 'NONE',  ( 4.963693636378940788, 5.923969009597785274, -1.082531754730548412 ) ) ;
#134440 = CARTESIAN_POINT ( 'NONE',  ( 1.360316468749969365, 1.036458333674742827, -0.7853790794158820310 ) ) ;
#134441 = CARTESIAN_POINT ( 'NONE',  ( 4.658827374183164949, 1.163267680695536876, 1.646840100852072997 ) ) ;
#134442 = CARTESIAN_POINT ( 'NONE',  ( -2.616360457312984167, 5.996244933599686355, -0.7216878364870257245 ) ) ;
#134443 = CARTESIAN_POINT ( 'NONE',  ( 9.257519960032755790, 9.694861462993381807, 0.7998128361456462443 ) ) ;
#134444 = CARTESIAN_POINT ( 'NONE',  ( 4.146814880933355596, 5.931313009212638931, 1.599625672291261402 ) ) ;
#134446 = CARTESIAN_POINT ( 'NONE',  ( -7.008396152629729592, -6.708819892820514497, 6.400381488218093828 ) ) ;
#134445 = CARTESIAN_POINT ( 'NONE',  ( 1.752308680507021155, 0.5713779359179693706, 1.734036872924920702 ) ) ;
#134447 = CARTESIAN_POINT ( 'NONE',  ( -6.147696309153835692, 6.137010213626392208, 0.7998128361456281477 ) ) ;
#134448 = FACE_OUTER_BOUND ( 'NONE', #105216, .T. ) ;
#134449 = CARTESIAN_POINT ( 'NONE',  ( -9.348561386651960348, 5.000000000000002665, 7.001914024036568485 ) ) ;
#134450 = ORIENTED_EDGE ( 'NONE', *, *, #194571, .F. ) ;
#134451 = CARTESIAN_POINT ( 'NONE',  ( -4.950135482320918712, 7.828889591799445213, -1.082531754730549967 ) ) ;
#134452 = LINE ( 'NONE', #200455, #87403 ) ;
#134453 = CARTESIAN_POINT ( 'NONE',  ( -7.635213062790267458, 12.05949900656400686, 0.000000000000000000 ) ) ;
#134454 = CARTESIAN_POINT ( 'NONE',  ( 6.111974619354628935, -0.6785462737385530296, 1.902425049502977528 ) ) ;
#134456 = ORIENTED_EDGE ( 'NONE', *, *, #129048, .T. ) ;
#134455 = CARTESIAN_POINT ( 'NONE',  ( 0.3992906662320141464, -0.2637550127744873185, -2.103967267096308991 ) ) ;
#134457 = CARTESIAN_POINT ( 'NONE',  ( -7.286581212701773502, 7.465709267765667789, 0.7998128361456341429 ) ) ;
#134458 = CARTESIAN_POINT ( 'NONE',  ( 5.789495288235341874, 6.713164910151406595, 1.199719254218462483 ) ) ;
#134459 = CARTESIAN_POINT ( 'NONE',  ( 4.838775396685393915, 0.3501730741383273782, 2.030750449888196751 ) ) ;
#134460 = CARTESIAN_POINT ( 'NONE',  ( 5.643203987388664800, 0.8197706014990979728, 1.842448445624145226 ) ) ;
#134461 = VERTEX_POINT ( 'NONE', #200604 ) ;
#134462 = ORIENTED_EDGE ( 'NONE', *, *, #134113, .F. ) ;
#134463 = CARTESIAN_POINT ( 'NONE',  ( 4.754910920499133553, 4.886969541830044506, -0.7851691560945832649 ) ) ;
#134464 = CARTESIAN_POINT ( 'NONE',  ( -0.3282377607281344867, 0.2611645503674426827, -1.225000000000015410 ) ) ;
#134465 = VECTOR ( 'NONE', #99430, 1000.000000000000000 ) ;
#134467 = ORIENTED_EDGE ( 'NONE', *, *, #49896, .T. ) ;
#134466 = CARTESIAN_POINT ( 'NONE',  ( -4.457598643843001973, 8.422558527783969851, 0.000000000000000000 ) ) ;
#134468 = CARTESIAN_POINT ( 'NONE',  ( 4.602896574056089207, 8.480248385054199645, 0.1803159889683242367 ) ) ;
#134469 = CARTESIAN_POINT ( 'NONE',  ( 4.657577273293715514, -0.4389639308803178208, -1.967586094827819654 ) ) ;
#134470 = CARTESIAN_POINT ( 'NONE',  ( 4.312339554033173705, 1.684294245562456993, 0.7440144950455057637 ) ) ;
#134471 = CARTESIAN_POINT ( 'NONE',  ( 10.75419052074084902, -7.927673425445468602, -0.6248749548428326195 ) ) ;
#134472 = CARTESIAN_POINT ( 'NONE',  ( 2.192384427926857615, -0.9847255960707482769, 2.087179981119008598 ) ) ;
#134473 = CARTESIAN_POINT ( 'NONE',  ( 6.180537922983273091, 8.303989891604203422, -1.599625672291281386 ) ) ;
#134474 = ADVANCED_FACE ( 'NONE', ( #19736 ), #15095, .F. ) ;
#134475 = CARTESIAN_POINT ( 'NONE',  ( 5.026735257907362531, 2.066873009482797841, 0.6328083787210944111 ) ) ;
#134477 = CARTESIAN_POINT ( 'NONE',  ( 7.411503528164766763, 11.79850454950093841, 1.040834085586084257E-14 ) ) ;
#134476 = CARTESIAN_POINT ( 'NONE',  ( 3.344935638061694139, -1.780668040901035143, -0.9463001528628791625 ) ) ;
#134478 = CARTESIAN_POINT ( 'NONE',  ( 0.1517630622446651534, 0.7442075171455504456, 1.793999140845178530 ) ) ;
#134479 = CARTESIAN_POINT ( 'NONE',  ( -6.033542053281340856, 6.997886136038390603, -1.199719254218446718 ) ) ;
#134480 = CARTESIAN_POINT ( 'NONE',  ( -4.655245641445871385, 6.524482229810530498, 1.599625672291263179 ) ) ;
#134481 = CARTESIAN_POINT ( 'NONE',  ( 3.256579335763456040, -1.417408692332474462, 1.220890361658559575 ) ) ;
#134482 = VECTOR ( 'NONE', #152466, 1000.000000000000000 ) ;
#134485 = CARTESIAN_POINT ( 'NONE',  ( -6.720001414228860881, 7.869031733802326123, -1.199719254218452047 ) ) ;
#134484 = CARTESIAN_POINT ( 'NONE',  ( 0.6823417656249917140, 5.592708333674749177, 1.181850606188765695 ) ) ;
#134483 = CARTESIAN_POINT ( 'NONE',  ( 6.533470331352867255, -0.1283082721124771952, 1.781802213622991404 ) ) ;
#134486 = CARTESIAN_POINT ( 'NONE',  ( 2.315298440750997777, 1.971968782506158924, 0.9909306302095726160 ) ) ;
#134487 = CARTESIAN_POINT ( 'NONE',  ( 6.720655732516647163, -0.004400176169771369272, 2.173773060281408931 ) ) ;
#134488 = CARTESIAN_POINT ( 'NONE',  ( 4.325214697959421706, 5.004837554829479451, 1.199719254218462483 ) ) ;
#134489 = CARTESIAN_POINT ( 'NONE',  ( 8.136301581532414673, 8.664975731308866003, 0.000000000000000000 ) ) ;
#134490 = CARTESIAN_POINT ( 'NONE',  ( -5.623934791570306402, 5.455678766453782913, 0.7998128361456341429 ) ) ;
#134491 = CARTESIAN_POINT ( 'NONE',  ( -7.715998819508785189, 8.174622508947939181, -0.7216878364870338292 ) ) ;
#134492 = CARTESIAN_POINT ( 'NONE',  ( 0.2628735715076990220, -1.758816568047173234, -0.8906303152973747972 ) ) ;
#134493 = CARTESIAN_POINT ( 'NONE',  ( 0.4996044509122186672, 1.916167126895538031, -1.285522792546058390 ) ) ;
#134495 = ADVANCED_FACE ( 'NONE', ( #135645 ), #168977, .T. ) ;
#134494 = CARTESIAN_POINT ( 'NONE',  ( 1.539427311113782837, 1.813978416018032558, -0.7477436361984082236 ) ) ;
#134496 = CARTESIAN_POINT ( 'NONE',  ( 4.610253265130005218, 2.062215687086375038, -0.04552280787792003375 ) ) ;
#134497 = CARTESIAN_POINT ( 'NONE',  ( 6.371969008742804697, 7.496680600697164465, -1.082531754730543083 ) ) ;
#134498 = CARTESIAN_POINT ( 'NONE',  ( 4.830447868218803897, 8.857549289555754157, -0.7998128361456481317 ) ) ;
#134499 = VERTEX_POINT ( 'NONE', #2396 ) ;
#134500 = CARTESIAN_POINT ( 'NONE',  ( 7.578644679914702031, 10.82520731233375955, 1.082531754730558626 ) ) ;
#134501 = CARTESIAN_POINT ( 'NONE',  ( -0.6823417656249969321, 5.030208333674755394, -1.181850606188749264 ) ) ;
#134502 = CARTESIAN_POINT ( 'NONE',  ( 4.053524740361575063, 4.791828954252362216, -1.082531754730543083 ) ) ;
#134503 = CARTESIAN_POINT ( 'NONE',  ( 6.285609470618021888, -2.046568710056245965, 0.7253697862827021003 ) ) ;
#134504 = CARTESIAN_POINT ( 'NONE',  ( 6.163598723784101452, 0.9525508894225950263, 1.575581956637741587 ) ) ;
#134505 = CARTESIAN_POINT ( 'NONE',  ( 5.417385717461801420, 6.279972267429607236, -1.041140759853006026 ) ) ;
#134506 = CARTESIAN_POINT ( 'NONE',  ( -10.29780748029859616, 4.862821740736285925, -6.167739988275216412 ) ) ;
#134507 = CARTESIAN_POINT ( 'NONE',  ( 1.018573325691285003, 1.726041315240328444, 0.7214104187760681519 ) ) ;
#134508 = CARTESIAN_POINT ( 'NONE',  ( -6.131331467106510225, 6.000095466447766590, 0.1540833971661673130 ) ) ;
#134509 = CARTESIAN_POINT ( 'NONE',  ( 1.416652131158605110, 8.000043606524068096, -10.86080395187258318 ) ) ;
#134510 = CARTESIAN_POINT ( 'NONE',  ( 6.505076094845553492, 6.832456077006010098, -0.5564590407885674495 ) ) ;
#134511 = CARTESIAN_POINT ( 'NONE',  ( 1.364683531249990311, 4.676041667008083103, 0.7879004041258500513 ) ) ;
#134512 = CARTESIAN_POINT ( 'NONE',  ( 0.6274217273865911881, -0.2802014979648696502, 1.891502685196180034 ) ) ;
#134513 = CARTESIAN_POINT ( 'NONE',  ( 2.729092984789914578, -1.652188407247729529, 0.6350153418272014294 ) ) ;
#134514 = CARTESIAN_POINT ( 'NONE',  ( 0.5219363917940004205, -1.903054291476031112, 0.1877445768119419822 ) ) ;
#134516 = CARTESIAN_POINT ( 'NONE',  ( 4.798395639560619763, 1.317935440718048135, -1.390428439694970431 ) ) ;
#134515 = CARTESIAN_POINT ( 'NONE',  ( 0.1842363695348751551, -3.140514841257148859, -3.377285597684139162 ) ) ;
#134517 = LINE ( 'NONE', #4441, #25874 ) ;
#134518 = CARTESIAN_POINT ( 'NONE',  ( 4.914487397858644080, 0.7518983826605809551, 1.820584232156793769 ) ) ;
#134519 = CARTESIAN_POINT ( 'NONE',  ( 0.4574861729177078229, -1.815669959853306370, 1.095388807130371900 ) ) ;
#134520 = DIRECTION ( 'NONE',  ( 0.000000000000000000, 0.000000000000000000, -1.000000000000000000 ) ) ;
#134521 = CARTESIAN_POINT ( 'NONE',  ( 3.537841792810627606, 0.8420186812403904764, -1.670516725672297031 ) ) ;
#134523 = VERTEX_POINT ( 'NONE', #86884 ) ;
#134522 = CARTESIAN_POINT ( 'NONE',  ( 0.3283667639546791195, 1.746078182827022429, 0.5332771064449209897 ) ) ;
#134524 = CARTESIAN_POINT ( 'NONE',  ( 3.739080281021701868, 0.3231575147602770426, 2.182976880621155136 ) ) ;
#134525 = CARTESIAN_POINT ( 'NONE',  ( -1.364683531250010295, 5.092708333674757171, 0.7879004041258379498 ) ) ;
#134526 = CARTESIAN_POINT ( 'NONE',  ( 0.9770945003616584579, 1.905102050789074353, 0.7911672170514363334 ) ) ;
#134527 = CARTESIAN_POINT ( 'NONE',  ( 7.558834334818744338, 8.777393797832065303, 1.199719254218462483 ) ) ;
#134528 = CARTESIAN_POINT ( 'NONE',  ( -7.655550293210764856, 12.08322577538792331, 0.000000000000000000 ) ) ;
#134529 = CARTESIAN_POINT ( 'NONE',  ( 3.933273961740297864, 7.602920365423412541, 0.7216878364870341622 ) ) ;
#134530 = CARTESIAN_POINT ( 'NONE',  ( -3.456098937306357310, -0.009090518290199266216, -0.2650254050244002513 ) ) ;
#134531 = DIRECTION ( 'NONE',  ( -5.551115123125765446E-17, 0.000000000000000000, 1.000000000000000000 ) ) ;
#134532 = ORIENTED_EDGE ( 'NONE', *, *, #144165, .T. ) ;
#134533 = CARTESIAN_POINT ( 'NONE',  ( 3.455589482447298355, 1.630370400113918095, 1.275915752658786095 ) ) ;
#134534 = CARTESIAN_POINT ( 'NONE',  ( -1.500000000000011324, 4.670833333333353821, 0.8660254037844403729 ) ) ;
#134535 = CARTESIAN_POINT ( 'NONE',  ( 1.968271169257681752, 1.109365460190291586, 1.855047589327807778 ) ) ;
#134536 = CARTESIAN_POINT ( 'NONE',  ( -6.606676129765223671, 6.763588582595081000, -0.1820296311667093936 ) ) ;
#134538 = EDGE_CURVE ( 'NONE', #148656, #167726, #172744, .T. ) ;
#134537 = CARTESIAN_POINT ( 'NONE',  ( 0.6979228276546626253, 1.358177971483988555, 1.494960626620364552 ) ) ;
#134539 = ORIENTED_EDGE ( 'NONE', *, *, #1901, .T. ) ;
#134540 = EDGE_CURVE ( 'NONE', #17507, #81410, #59179, .T. ) ;
#134542 = CARTESIAN_POINT ( 'NONE',  ( 8.758204044748005401, 10.28062147603659504, 1.082531754730549967 ) ) ;
#134541 = CARTESIAN_POINT ( 'NONE',  ( -3.475000000000000533, -2.450000000000000622, 0.000000000000000000 ) ) ;
#134543 = CARTESIAN_POINT ( 'NONE',  ( 6.450546045330814771, 1.388275245401158431, 1.462219883709668045 ) ) ;
#134544 = CARTESIAN_POINT ( 'NONE',  ( 6.262892222096183126, -0.1014175117164286682, -1.913191589401983528 ) ) ;
#134545 = CARTESIAN_POINT ( 'NONE',  ( 6.539320575229294441, 2.949125184229839380, 2.655650464557571144 ) ) ;
#134546 = CARTESIAN_POINT ( 'NONE',  ( 4.722331747100577459, 2.097238624054961864, 0.6360808509995665716 ) ) ;
#134547 = CARTESIAN_POINT ( 'NONE',  ( 0.7499999999999885647, 2.847916667349487341, -1.299038105676658228 ) ) ;
#134548 = CARTESIAN_POINT ( 'NONE',  ( 3.058751851047710080, 0.4689117840017149041, 1.853869267190631831 ) ) ;
#134550 = CARTESIAN_POINT ( 'NONE',  ( -5.603597561149804562, 5.431951997629870910, 0.7998128361456341429 ) ) ;
#134549 = B_SPLINE_CURVE_WITH_KNOTS ( 'NONE', 3,
 ( #120604, #92330, #190840, #7819 ),
 .UNSPECIFIED., .F., .F.,
 ( 4, 4 ),
 ( 0.000000000000000000, 6.033646489354672709E-05 ),
 .UNSPECIFIED. ) ;
#134551 = CARTESIAN_POINT ( 'NONE',  ( 5.314433026432511475, 5.302519407033794430, 1.040834085586084257E-14 ) ) ;
#134553 = CARTESIAN_POINT ( 'NONE',  ( 1.388296234047466049, -0.7283980888908546669, -1.880428666220852696 ) ) ;
#134552 = CARTESIAN_POINT ( 'NONE',  ( 11.48243876534946217, 11.37999999999998302, 3.199999999999997957 ) ) ;
#134554 = CARTESIAN_POINT ( 'NONE',  ( -8.012344526598182026E-15, 11.60937500034140157, -1.575800808251669460 ) ) ;
#134555 = AXIS2_PLACEMENT_3D ( 'NONE', #133667, #153076, #4653 ) ;
#134557 = CARTESIAN_POINT ( 'NONE',  ( -5.224688093219839402, 7.188831756880171397, -1.599625672291271394 ) ) ;
#134556 = CARTESIAN_POINT ( 'NONE',  ( 0.01182134700736507844, -2.246462713633586183, 0.4557613021327082681 ) ) ;
#134558 = CARTESIAN_POINT ( 'NONE',  ( 4.278129899785966472, -0.9921777787025712891, 1.410595609005516504 ) ) ;
#134559 = CARTESIAN_POINT ( 'NONE',  ( 0.1394461523056798324, 0.009327122704651937685, -1.719853553173174232 ) ) ;
#134560 = CARTESIAN_POINT ( 'NONE',  ( 8.471147050440139381, 8.777426401801974976, -0.7998128361456281477 ) ) ;
#134561 = CARTESIAN_POINT ( 'NONE',  ( 3.928111819657337911, 5.605883094398769195, 1.599625672291267398 ) ) ;
#134562 = DIRECTION ( 'NONE',  ( -0.000000000000000000, -8.546850786086437571E-32, -1.000000000000000000 ) ) ;
#134563 = CARTESIAN_POINT ( 'NONE',  ( 1.557006721180295150, 1.605793932651664813, -1.126831546849601740 ) ) ;
#134564 = SURFACE_SIDE_STYLE ('',( #104172 ) ) ;
#134565 = CARTESIAN_POINT ( 'NONE',  ( 6.030679399980265920, 5.930214142932100252, -0.7998128361456281477 ) ) ;
#134566 = CARTESIAN_POINT ( 'NONE',  ( 0.1751657365761495888, 6.947016338497860488, -2.639079955608885975 ) ) ;
#134567 = EDGE_CURVE ( 'NONE', #94342, #119510, #163877, .T. ) ;
#134568 = ORIENTED_EDGE ( 'NONE', *, *, #76837, .F. ) ;
#134569 = SURFACE_STYLE_FILL_AREA ( #84712 ) ;
#134570 = ORIENTED_EDGE ( 'NONE', *, *, #3140, .T. ) ;
#134571 = CARTESIAN_POINT ( 'NONE',  ( 4.371601898205011771, 0.3924986647133471007, -1.768265068870542800 ) ) ;
#134572 = ORIENTED_EDGE ( 'NONE', *, *, #126259, .T. ) ;
#134573 = CARTESIAN_POINT ( 'NONE',  ( 7.018280793729500644, 8.217024343219755167, -1.199719254218452047 ) ) ;
#134574 = DIRECTION ( 'NONE',  ( 0.000000000000000000, 0.000000000000000000, 1.000000000000000000 ) ) ;
#134575 = CARTESIAN_POINT ( 'NONE',  ( 5.145072886348948771, 0.1388508722429954989, 1.806219837558323826 ) ) ;
#134576 = CARTESIAN_POINT ( 'NONE',  ( 5.506019780481205217, 9.437790487287811558, 0.000000000000000000 ) ) ;
#134577 = CIRCLE ( 'NONE', #110479, 0.04999999999999969746 ) ;
#134578 = CARTESIAN_POINT ( 'NONE',  ( 7.727873494160014900, -5.742104877864247392, -7.828177403543865154 ) ) ;
#134579 = CARTESIAN_POINT ( 'NONE',  ( 5.343583877570073248, 6.330574952785890552, -1.095086179472234189 ) ) ;
#134581 = CARTESIAN_POINT ( 'NONE',  ( 8.540746701604824409, 12.05162268759261224, -1.199719254218446718 ) ) ;
#134580 = CARTESIAN_POINT ( 'NONE',  ( 5.740631066870683696, -1.815735608131360479, -0.4073663091734185948 ) ) ;
#134582 = CARTESIAN_POINT ( 'NONE',  ( 4.200734335399162411, 1.752999579934441998, 0.7727710859696481638 ) ) ;
#134583 = DIRECTION ( 'NONE',  ( 0.000000000000000000, 0.000000000000000000, -1.000000000000000000 ) ) ;
#134584 = CARTESIAN_POINT ( 'NONE',  ( -10.83922355283164229, 5.627439893072521571, -6.488667358217314884 ) ) ;
#134585 = CARTESIAN_POINT ( 'NONE',  ( 7.446209719563365859, -5.223431457505076203, 8.064677165291195493 ) ) ;
#134586 = LINE ( 'NONE', #117293, #112050 ) ;
#134587 = CARTESIAN_POINT ( 'NONE',  ( 5.151735183512854199, 8.954182114166247430, -0.7216878364870257245 ) ) ;
#134588 = CARTESIAN_POINT ( 'NONE',  ( -8.785320351975364872, 12.23299559640450518, 1.082531754730560403 ) ) ;
#134589 = CARTESIAN_POINT ( 'NONE',  ( 1.147603855448702248, -1.704515299458901012, -1.329379018566230641 ) ) ;
#134590 = CARTESIAN_POINT ( 'NONE',  ( -6.459533842268148973, 6.500820668926428958, 0.000000000000000000 ) ) ;
#134591 = CARTESIAN_POINT ( 'NONE',  ( 5.662465432362883355, 6.635239754958710989, 1.199719254218451159 ) ) ;
#134592 = CARTESIAN_POINT ( 'NONE',  ( 0.8151338971811080691, -0.2727355552937099636, 1.804975678908596226 ) ) ;
#134593 = CARTESIAN_POINT ( 'NONE',  ( -5.742041750587549842, 6.657802449562273850, 1.199719254218450271 ) ) ;
#134594 = CARTESIAN_POINT ( 'NONE',  ( 4.067279105520240634, 0.2236234833344897255, -1.811772463268163547 ) ) ;
#134595 = CARTESIAN_POINT ( 'NONE',  ( 9.962237412473150755, 12.35880645891234408, 7.801823201411741238 ) ) ;
#134596 = CARTESIAN_POINT ( 'NONE',  ( 2.232540727315056373, 1.246330492051262784, -1.450604739030990187 ) ) ;
#134597 = CARTESIAN_POINT ( 'NONE',  ( 2.453506318599480096, 1.520516184767862100, 1.251830903418025054 ) ) ;
#134598 = CARTESIAN_POINT ( 'NONE',  ( 4.054194213510796452, -1.436945492307143635, 1.306602268835421077 ) ) ;
#134599 = ORIENTED_EDGE ( 'NONE', *, *, #72719, .F. ) ;
#134600 = CARTESIAN_POINT ( 'NONE',  ( -7.533490631048818109, 8.818102486758951031, -1.199719254218452047 ) ) ;
#134602 = CARTESIAN_POINT ( 'NONE',  ( 4.201511661969238531, 1.892856375164463367, -0.9562558712687405649 ) ) ;
#134601 = CARTESIAN_POINT ( 'NONE',  ( 4.167152111353856547, 5.955039778036558040, 1.599625672291262513 ) ) ;
#134603 = CARTESIAN_POINT ( 'NONE',  ( 7.910292558569346433, 11.31609285405122556, -1.199719254218446718 ) ) ;
#134604 = CARTESIAN_POINT ( 'NONE',  ( 6.093061176370408560, 6.029359313278345844, 0.2718797729955486631 ) ) ;
#134605 = FACE_OUTER_BOUND ( 'NONE', #91171, .T. ) ;
#134606 = ORIENTED_EDGE ( 'NONE', *, *, #146195, .F. ) ;
#134607 = CARTESIAN_POINT ( 'NONE',  ( 4.362691568547328202, 8.311833606605697256, -0.7998128361456381397 ) ) ;
#134608 = DIRECTION ( 'NONE',  ( 1.000000000000000000, 0.000000000000000000, -3.491481338843133355E-15 ) ) ;
#134609 = CARTESIAN_POINT ( 'NONE',  ( 4.160648861918358143, -1.351394993475165673, 1.227733137840483879 ) ) ;
#134610 = CARTESIAN_POINT ( 'NONE',  ( 0.1515253745957860221, 3.870538056096196833, -11.62858902121510951 ) ) ;
#134611 = CARTESIAN_POINT ( 'NONE',  ( -9.002250809794006159, 10.56534270192358704, -1.082531754730543971 ) ) ;
#134612 = AXIS2_PLACEMENT_3D ( 'NONE', #137008, #155380, #171625 ) ;
#134613 = CARTESIAN_POINT ( 'NONE',  ( -4.866517195131829787, 8.171732932056599452, 0.9908671576431731243 ) ) ;
#134614 = CARTESIAN_POINT ( 'NONE',  ( 1.214306433183764966E-14, 2.428612866367529932E-14, 1.500000000000001332 ) ) ;
#134616 = CARTESIAN_POINT ( 'NONE',  ( 4.698043743269282757, -1.870269067358639958, -0.04562963166049315705 ) ) ;
#134615 = B_SPLINE_CURVE_WITH_KNOTS ( 'NONE', 3,
 ( #66452, #101108, #169320, #148809, #102188, #99001, #136832, #165056, #51310, #168255 ),
 .UNSPECIFIED., .F., .F.,
 ( 4, 2, 2, 2, 4 ),
 ( 0.1967386737735414559, 0.2725667127094347775, 0.3483947516453281268, 0.4242227905812214206, 0.5000508295171147699 ),
 .UNSPECIFIED. ) ;
#134617 = CARTESIAN_POINT ( 'NONE',  ( 6.238723240582662477, 10.43026088065513513, -0.7998128361456291469 ) ) ;
#134618 = CARTESIAN_POINT ( 'NONE',  ( 3.826716429392281071, 1.829700617163315002, 0.6032043533580729866 ) ) ;
#134619 = CARTESIAN_POINT ( 'NONE',  ( -5.949330478298284319, 5.835307067636438916, 0.7998128361456341429 ) ) ;
#134620 = CARTESIAN_POINT ( 'NONE',  ( -8.012344526598182026E-15, 9.109375000341398021, -1.575800808251669460 ) ) ;
#134621 = CARTESIAN_POINT ( 'NONE',  ( -5.215082642750900277, 9.236013516518044142, 0.000000000000000000 ) ) ;
#134622 = CARTESIAN_POINT ( 'NONE',  ( 4.359110081993588182, 5.044382169536003602, -1.199719254218452047 ) ) ;
#134623 = CARTESIAN_POINT ( 'NONE',  ( -5.759181390754928742, 9.941071732514568993, 0.000000000000000000 ) ) ;
#134624 = CIRCLE ( 'NONE', #165194, 0.08000000000000025147 ) ;
#134625 = CARTESIAN_POINT ( 'NONE',  ( 1.546650761107182914, -1.494491507556227505, 1.499968751290579494 ) ) ;
#134626 = CARTESIAN_POINT ( 'NONE',  ( 8.106885785967500979, 11.54545161934907682, 1.199719254218460707 ) ) ;
#134627 = CARTESIAN_POINT ( 'NONE',  ( -2.728371075039041305, 2.952267909019561376, 2.500000000000000444 ) ) ;
#134628 = CARTESIAN_POINT ( 'NONE',  ( 6.772334134356085222, -0.9704686269969391432, -1.828672837219179392 ) ) ;
#134630 = CARTESIAN_POINT ( 'NONE',  ( 4.118656133465138147, 7.671478758617087834, -0.7332979114653701558 ) ) ;
#134629 = CARTESIAN_POINT ( 'NONE',  ( 1.522747961674526085, -1.733470594775164075, 0.6210259959333885860 ) ) ;
#134631 = CARTESIAN_POINT ( 'NONE',  ( 6.331294547901813452, 6.488857848747989543, 1.040834085586084257E-14 ) ) ;
#134633 = CARTESIAN_POINT ( 'NONE',  ( 0.5100945355815690307, 6.808349925817971382, 3.584950416132734130 ) ) ;
#134632 = CARTESIAN_POINT ( 'NONE',  ( 3.553645660557675612, 6.199651466408984568, -1.082531754730549967 ) ) ;
#134634 = CARTESIAN_POINT ( 'NONE',  ( 1.658568045375780731, -1.618562549950094187, 1.623430423404078837 ) ) ;
#134635 = CARTESIAN_POINT ( 'NONE',  ( 5.613211309847925712, -1.894178568204254676, 0.4274185452872342195 ) ) ;
#134636 = EDGE_LOOP ( 'NONE', ( #186194, #139505, #148752, #114697 ) ) ;
#134637 = CARTESIAN_POINT ( 'NONE',  ( 8.717529583462649612, 10.23316793787035195, 1.082531754730558626 ) ) ;
#134638 = CARTESIAN_POINT ( 'NONE',  ( 1.090090997392887173, 1.202455520763350272, 1.614487003566661638 ) ) ;
#134639 = CARTESIAN_POINT ( 'NONE',  ( -10.64723070543352712, 11.31619066596094392, 0.7998128361456462443 ) ) ;
#134641 = DIRECTION ( 'NONE',  ( -0.04267330865764863701, 0.000000000000000000, -0.9990890794760038940 ) ) ;
#134640 = CARTESIAN_POINT ( 'NONE',  ( -8.148614017013223076, 9.465470093725620870, -1.199719254218446718 ) ) ;
#134642 = CARTESIAN_POINT ( 'NONE',  ( -9.498553103985718948, -9.900000000000005684, 0.1657978611541623959 ) ) ;
#134644 = CARTESIAN_POINT ( 'NONE',  ( 1.797346856567107798, -0.6001438452145327895, 1.665118380002019283 ) ) ;
#134643 = CARTESIAN_POINT ( 'NONE',  ( 4.365234240191905535, 2.027873629061471838, -0.5078740465511691893 ) ) ;
#134645 = CARTESIAN_POINT ( 'NONE',  ( 0.4019237886466816012, 12.17633545031537068, -1.499999999999998668 ) ) ;
#134647 = CARTESIAN_POINT ( 'NONE',  ( 5.138769532551322072, -1.968056315684912683, 1.175056510511104158 ) ) ;
#134646 = CARTESIAN_POINT ( 'NONE',  ( -11.73494313955695745, 7.421333685592205853, -2.519709837933482355 ) ) ;
#134648 = CARTESIAN_POINT ( 'NONE',  ( 3.890341755399207013, 1.468866505370895137, -0.9330376088199500151 ) ) ;
#134649 = CARTESIAN_POINT ( 'NONE',  ( 8.218213668177886788, 12.73966637951625813, 0.7998128361456462443 ) ) ;
#134650 = AXIS2_PLACEMENT_3D ( 'NONE', #152292, #67798, #664 ) ;
#134651 = DIRECTION ( 'NONE',  ( -0.000000000000000000, -1.000000000000000000, -0.000000000000000000 ) ) ;
#134652 = CARTESIAN_POINT ( 'NONE',  ( 3.338897068646465627, -1.034916488738941709, 1.390885369450091336 ) ) ;
#134653 =( BOUNDED_SURFACE ( )  B_SPLINE_SURFACE ( 1, 2, ( 
 ( #88689, #70260, #7401, #169916, #73482, #87611, #123406, #90829, #5251, #203459, #71327, #22583, #170984, #137442, #172067, #139582, #154749, #152604, #187232, #120182, #205609, #206680, #20456, #121259, #38861, #6333, #72405, #122339, #189370, #138505, #188296, #74566, #41013, #39936, #107122, #173145, #156891, #8479, #140665, #58312, #124467, #174222, #27941, #44209, #175277, #109269, #210937, #75631, #96168, #43157, #13806, #112455, #26864, #11677, #125530, #25797, #193631, #128726, #129795, #63639, #159013, #94036, #9555, #10607, #62563, #76683, #194698, #209866, #178467, #79877, #160075, #177398, #29011, #30077, #191488, #77752, #141740, #211999, #143873, #176334, #61504, #161146, #142799, #208804, #92968, #60433, #157963, #126593, #192554, #110331, #127670, #45273, #111394, #95098, #195774, #12733, #47413, #78807, #91906, #46340, #207746, #145988, #144931, #59372, #162219, #151296, #179534, #85210, #83067, #114591, #200014, #2867, #164338, #166465, #48474, #18058, #67859, #725, #165393, #181632, #97226, #34322, #130840, #182703, #64695, #1802, #117788, #180582, #82009, #32203, #115636, #197887, #196833, #50581, #100396, #33261, #31153, #65731, #163279, #84145, #68937, #201071, #135059, #113527, #98279, #99344, #66791, #150231, #15926, #49516, #167535, #134008, #14863, #80952, #148099, #51665, #183777, #35388, #101464, #19133, #147043, #213066, #214102, #131878, #16989, #149145, #132930, #198936, #116703, #188039, #121006, #143349, #21249, #119921, #103608, #87356, #169664, #36458, #4993, #3930, #6074, #24464, #38605, #52713, #153424, #202129, #168596, #204266, #71070, #7145, #118846, #20196, #137187, #185896, #70000, #184828, #205354, #203209, #102534, #186973, #39668, #89509, #77230, #54855, #53790, #106862, #22318, #105779, #171804, #104683, #86284, #37531, #170732, #23396, #88431, #155563, #154495, #72144, #11153, #152355, #136114, #55919, #138254, #122077, #73217, #139323, #56988, #123161, #189121, #40756, #172889, #90577, #156637, #115139, #97780, #32755, #12226, #209344, #113015, #163840, #213606 ),
 ( #94582, #181135, #210426, #176879, #44766, #80443, #146544, #114091, #28491, #15419, #164887, #46901, #49020, #45830, #31705, #29567, #60992, #194186, #145494, #79375, #63126, #98837, #212562, #180082, #95659, #160625, #96726, #78299, #16481, #62068, #64201, #81509, #161710, #144424, #147588, #65233, #131383, #110874, #195266, #197379, #111951, #128223, #177953, #13302, #129290, #211489, #179024, #30642, #82562, #162775, #127145, #14353, #193118, #130342, #196331, #47975, #199497, #38092, #34867, #186455, #214, #120483, #118333, #149711, #20741, #104163, #51141, #201620, #83628, #53269, #103090, #35943, #200560, #2352, #132432, #69492, #165955, #3425, #99894, #37008, #152901, #1291, #117265, #67349, #150789, #18623, #17539, #85768, #135599, #68428, #66285, #100941, #198433, #119400, #170211, #21796, #148648, #50079, #133494, #134557, #102022, #185389, #183263, #116200, #182187, #169148, #33815, #167028, #84702, #86836, #4479, #70550, #136669, #54344, #202694, #52207, #184318, #168091, #19690, #151849, #92205, #41312, #205907, #87904, #156115, #172361, #88988, #22872, #124758, #203758, #9844, #171280, #142022, #26090, #155041, #139876, #39157, #153977, #107419, #42380, #43440, #191784, #72706, #7697, #137738, #138801, #190718, #204821, #108490, #123699, #158255, #208037, #73780, #91123, #157182, #75919, #105240, #57542, #55401, #125823, #189660, #90055, #173444, #74860, #56472, #122634, #6627, #188597, #71625, #109564, #175568, #40228, #25023, #121555, #106339, #174514, #23951, #59664, #8777, #5544, #187526, #140963, #206973, #58604, #31442, #192847, #95399, #76971, #64977, #211231, #29305, #161451, #14086, #78046, #144170, #44506, #210162, #10896, #94328, #160370, #110623, #13031, #28235, #11972, #61803, #197121, #127972, #131132, #193924, #48760, #63927, #114872, #147328, #45571, #27159, #111687, #93264, #159297, #213356, #62856, #177694, #113824, #143098, #79108, #80177, #176624, #146282, #196077, #129021, #145226, #194997, #209091, #162514, #46631, #96465, #112754, #130082, #97521, #178766, #30379, #212295 ) ),
 .UNSPECIFIED., .F., .F., .T. ) 
 B_SPLINE_SURFACE_WITH_KNOTS ( ( 2, 2 ),
 ( 3, 2, 2, 2, 2, 2, 2, 2, 2, 2, 2, 2, 2, 2, 2, 2, 2, 2, 2, 2, 2, 2, 2, 2, 2, 2, 2, 2, 2, 2, 2, 2, 2, 2, 2, 2, 2, 2, 2, 2, 2, 2, 2, 2, 2, 2, 2, 2, 2, 2, 2, 2, 2, 2, 2, 2, 2, 2, 2, 2, 2, 2, 2, 2, 2, 2, 2, 2, 2, 2, 2, 2, 2, 2, 2, 2, 2, 2, 2, 2, 2, 2, 2, 2, 2, 2, 2, 2, 2, 2, 2, 2, 2, 2, 2, 2, 2, 2, 2, 2, 2, 2, 2, 2, 2, 2, 2, 2, 2, 2, 2, 2, 2, 2, 2, 2, 2, 2, 2, 2, 3 ),
 ( 0.000000000000000000, 1.000000000000000000 ),
 ( 0.000000000000000000, 0.008333333333333333218, 0.01666666666666666644, 0.02500000000000000139, 0.03333333333333333287, 0.04166666666666666435, 0.05000000000000000278, 0.05833333333333333426, 0.06666666666666666574, 0.07499999999999999722, 0.08333333333333332871, 0.09166666666666666019, 0.1000000000000000056, 0.1083333333333333370, 0.1166666666666666685, 0.1250000000000000000, 0.1333333333333333315, 0.1416666666666666630, 0.1499999999999999944, 0.1583333333333333259, 0.1666666666666666574, 0.1749999999999999889, 0.1833333333333333204, 0.1916666666666666796, 0.2000000000000000111, 0.2083333333333333426, 0.2166666666666666741, 0.2250000000000000056, 0.2333333333333333370, 0.2416666666666666685, 0.2500000000000000000, 0.2583333333333333592, 0.2666666666666666630, 0.2750000000000000222, 0.2833333333333333259, 0.2916666666666666852, 0.2999999999999999889, 0.3083333333333333481, 0.3166666666666666519, 0.3250000000000000111, 0.3333333333333333148, 0.3416666666666666741, 0.3499999999999999778, 0.3583333333333333370, 0.3666666666666666408, 0.3750000000000000000, 0.3833333333333333592, 0.3916666666666666630, 0.4000000000000000222, 0.4083333333333333259, 0.4166666666666666852, 0.4249999999999999889, 0.4333333333333333481, 0.4416666666666666519, 0.4500000000000000111, 0.4583333333333333148, 0.4666666666666666741, 0.4749999999999999778, 0.4833333333333333370, 0.4916666666666666408, 0.5000000000000000000, 0.5083333333333333037, 0.5166666666666667185, 0.5250000000000000222, 0.5333333333333333259, 0.5416666666666666297, 0.5500000000000000444, 0.5583333333333333481, 0.5666666666666666519, 0.5749999999999999556, 0.5833333333333333703, 0.5916666666666666741, 0.5999999999999999778, 0.6083333333333332815, 0.6166666666666666963, 0.6250000000000000000, 0.6333333333333333037, 0.6416666666666667185, 0.6500000000000000222, 0.6583333333333333259, 0.6666666666666666297, 0.6750000000000000444, 0.6833333333333333481, 0.6916666666666666519, 0.6999999999999999556, 0.7083333333333333703, 0.7166666666666666741, 0.7249999999999999778, 0.7333333333333332815, 0.7416666666666666963, 0.7500000000000000000, 0.7583333333333333037, 0.7666666666666667185, 0.7750000000000000222, 0.7833333333333333259, 0.7916666666666666297, 0.8000000000000000444, 0.8083333333333333481, 0.8166666666666666519, 0.8249999999999999556, 0.8333333333333333703, 0.8416666666666666741, 0.8499999999999999778, 0.8583333333333332815, 0.8666666666666666963, 0.8750000000000000000, 0.8833333333333333037, 0.8916666666666667185, 0.9000000000000000222, 0.9083333333333333259, 0.9166666666666666297, 0.9250000000000000444, 0.9333333333333333481, 0.9416666666666666519, 0.9499999999999999556, 0.9583333333333333703, 0.9666666666666666741, 0.9749999999999999778, 0.9833333333333332815, 0.9916666666666666963, 1.000000000000000000 ),
 .UNSPECIFIED. ) 
 GEOMETRIC_REPRESENTATION_ITEM ( )  RATIONAL_B_SPLINE_SURFACE ( (
 ( 1.000000000000000000, 0.8660254037844387076, 1.000000000000000000, 0.8660254037844387076, 1.000000000000000000, 0.8660254037844387076, 1.000000000000000000, 0.8660254037844387076, 1.000000000000000000, 0.8660254037844387076, 1.000000000000000000, 0.8660254037844387076, 1.000000000000000000, 0.8660254037844387076, 1.000000000000000000, 0.8660254037844387076, 1.000000000000000000, 0.8660254037844387076, 1.000000000000000000, 0.8660254037844387076, 1.000000000000000000, 0.8660254037844387076, 1.000000000000000000, 0.8660254037844387076, 1.000000000000000000, 0.8660254037844387076, 1.000000000000000000, 0.8660254037844387076, 1.000000000000000000, 0.8660254037844387076, 1.000000000000000000, 0.8660254037844387076, 1.000000000000000000, 0.8660254037844387076, 1.000000000000000000, 0.8660254037844387076, 1.000000000000000000, 0.8660254037844387076, 1.000000000000000000, 0.8660254037844387076, 1.000000000000000000, 0.8660254037844387076, 1.000000000000000000, 0.8660254037844387076, 1.000000000000000000, 0.8660254037844387076, 1.000000000000000000, 0.8660254037844387076, 1.000000000000000000, 0.8660254037844387076, 1.000000000000000000, 0.8660254037844387076, 1.000000000000000000, 0.8660254037844387076, 1.000000000000000000, 0.8660254037844387076, 1.000000000000000000, 0.8660254037844387076, 1.000000000000000000, 0.8660254037844387076, 1.000000000000000000, 0.8660254037844387076, 1.000000000000000000, 0.8660254037844387076, 1.000000000000000000, 0.8660254037844387076, 1.000000000000000000, 0.8660254037844387076, 1.000000000000000000, 0.8660254037844387076, 1.000000000000000000, 0.8660254037844387076, 1.000000000000000000, 0.8660254037844387076, 1.000000000000000000, 0.8660254037844387076, 1.000000000000000000, 0.8660254037844387076, 1.000000000000000000, 0.8660254037844387076, 1.000000000000000000, 0.8660254037844387076, 1.000000000000000000, 0.8660254037844387076, 1.000000000000000000, 0.8660254037844387076, 1.000000000000000000, 0.8660254037844387076, 1.000000000000000000, 0.8660254037844387076, 1.000000000000000000, 0.8660254037844387076, 1.000000000000000000, 0.8660254037844387076, 1.000000000000000000, 0.8660254037844387076, 1.000000000000000000, 0.8660254037844387076, 1.000000000000000000, 0.8660254037844387076, 1.000000000000000000, 0.8660254037844387076, 1.000000000000000000, 0.8660254037844387076, 1.000000000000000000, 0.8660254037844387076, 1.000000000000000000, 0.8660254037844387076, 1.000000000000000000, 0.8660254037844387076, 1.000000000000000000, 0.8660254037844387076, 1.000000000000000000, 0.8660254037844387076, 1.000000000000000000, 0.8660254037844387076, 1.000000000000000000, 0.8660254037844387076, 1.000000000000000000, 0.8660254037844387076, 1.000000000000000000, 0.8660254037844387076, 1.000000000000000000, 0.8660254037844387076, 1.000000000000000000, 0.8660254037844387076, 1.000000000000000000, 0.8660254037844387076, 1.000000000000000000, 0.8660254037844387076, 1.000000000000000000, 0.8660254037844387076, 1.000000000000000000, 0.8660254037844387076, 1.000000000000000000, 0.8660254037844387076, 1.000000000000000000, 0.8660254037844387076, 1.000000000000000000, 0.8660254037844387076, 1.000000000000000000, 0.8660254037844387076, 1.000000000000000000, 0.8660254037844387076, 1.000000000000000000, 0.8660254037844387076, 1.000000000000000000, 0.8660254037844387076, 1.000000000000000000, 0.8660254037844387076, 1.000000000000000000, 0.8660254037844387076, 1.000000000000000000, 0.8660254037844387076, 1.000000000000000000, 0.8660254037844387076, 1.000000000000000000, 0.8660254037844387076, 1.000000000000000000, 0.8660254037844387076, 1.000000000000000000, 0.8660254037844387076, 1.000000000000000000, 0.8660254037844387076, 1.000000000000000000, 0.8660254037844387076, 1.000000000000000000, 0.8660254037844387076, 1.000000000000000000, 0.8660254037844387076, 1.000000000000000000, 0.8660254037844387076, 1.000000000000000000, 0.8660254037844387076, 1.000000000000000000, 0.8660254037844387076, 1.000000000000000000, 0.8660254037844387076, 1.000000000000000000, 0.8660254037844387076, 1.000000000000000000, 0.8660254037844387076, 1.000000000000000000, 0.8660254037844387076, 1.000000000000000000, 0.8660254037844387076, 1.000000000000000000, 0.8660254037844387076, 1.000000000000000000, 0.8660254037844387076, 1.000000000000000000, 0.8660254037844387076, 1.000000000000000000, 0.8660254037844387076, 1.000000000000000000, 0.8660254037844387076, 1.000000000000000000, 0.8660254037844387076, 1.000000000000000000, 0.8660254037844387076, 1.000000000000000000, 0.8660254037844387076, 1.000000000000000000, 0.8660254037844387076, 1.000000000000000000, 0.8660254037844387076, 1.000000000000000000, 0.8660254037844387076, 1.000000000000000000, 0.8660254037844387076, 1.000000000000000000, 0.8660254037844387076, 1.000000000000000000, 0.8660254037844387076, 1.000000000000000000, 0.8660254037844387076, 1.000000000000000000, 0.8660254037844387076, 1.000000000000000000, 0.8660254037844387076, 1.000000000000000000, 0.8660254037844387076, 1.000000000000000000, 0.8660254037844387076, 1.000000000000000000, 0.8660254037844387076, 1.000000000000000000, 0.8660254037844387076, 1.000000000000000000, 0.8660254037844387076, 1.000000000000000000, 0.8660254037844387076, 1.000000000000000000, 0.8660254037844387076, 1.000000000000000000, 0.8660254037844387076, 1.000000000000000000, 0.8660254037844387076, 1.000000000000000000, 0.8660254037844387076, 1.000000000000000000),
 ( 1.000000000000000000, 0.8660254037844387076, 1.000000000000000000, 0.8660254037844387076, 1.000000000000000000, 0.8660254037844387076, 1.000000000000000000, 0.8660254037844387076, 1.000000000000000000, 0.8660254037844387076, 1.000000000000000000, 0.8660254037844387076, 1.000000000000000000, 0.8660254037844387076, 1.000000000000000000, 0.8660254037844387076, 1.000000000000000000, 0.8660254037844387076, 1.000000000000000000, 0.8660254037844387076, 1.000000000000000000, 0.8660254037844387076, 1.000000000000000000, 0.8660254037844387076, 1.000000000000000000, 0.8660254037844387076, 1.000000000000000000, 0.8660254037844387076, 1.000000000000000000, 0.8660254037844387076, 1.000000000000000000, 0.8660254037844387076, 1.000000000000000000, 0.8660254037844387076, 1.000000000000000000, 0.8660254037844387076, 1.000000000000000000, 0.8660254037844387076, 1.000000000000000000, 0.8660254037844387076, 1.000000000000000000, 0.8660254037844387076, 1.000000000000000000, 0.8660254037844387076, 1.000000000000000000, 0.8660254037844387076, 1.000000000000000000, 0.8660254037844387076, 1.000000000000000000, 0.8660254037844387076, 1.000000000000000000, 0.8660254037844387076, 1.000000000000000000, 0.8660254037844387076, 1.000000000000000000, 0.8660254037844387076, 1.000000000000000000, 0.8660254037844387076, 1.000000000000000000, 0.8660254037844387076, 1.000000000000000000, 0.8660254037844387076, 1.000000000000000000, 0.8660254037844387076, 1.000000000000000000, 0.8660254037844387076, 1.000000000000000000, 0.8660254037844387076, 1.000000000000000000, 0.8660254037844387076, 1.000000000000000000, 0.8660254037844387076, 1.000000000000000000, 0.8660254037844387076, 1.000000000000000000, 0.8660254037844387076, 1.000000000000000000, 0.8660254037844387076, 1.000000000000000000, 0.8660254037844387076, 1.000000000000000000, 0.8660254037844387076, 1.000000000000000000, 0.8660254037844387076, 1.000000000000000000, 0.8660254037844387076, 1.000000000000000000, 0.8660254037844387076, 1.000000000000000000, 0.8660254037844387076, 1.000000000000000000, 0.8660254037844387076, 1.000000000000000000, 0.8660254037844387076, 1.000000000000000000, 0.8660254037844387076, 1.000000000000000000, 0.8660254037844387076, 1.000000000000000000, 0.8660254037844387076, 1.000000000000000000, 0.8660254037844387076, 1.000000000000000000, 0.8660254037844387076, 1.000000000000000000, 0.8660254037844387076, 1.000000000000000000, 0.8660254037844387076, 1.000000000000000000, 0.8660254037844387076, 1.000000000000000000, 0.8660254037844387076, 1.000000000000000000, 0.8660254037844387076, 1.000000000000000000, 0.8660254037844387076, 1.000000000000000000, 0.8660254037844387076, 1.000000000000000000, 0.8660254037844387076, 1.000000000000000000, 0.8660254037844387076, 1.000000000000000000, 0.8660254037844387076, 1.000000000000000000, 0.8660254037844387076, 1.000000000000000000, 0.8660254037844387076, 1.000000000000000000, 0.8660254037844387076, 1.000000000000000000, 0.8660254037844387076, 1.000000000000000000, 0.8660254037844387076, 1.000000000000000000, 0.8660254037844387076, 1.000000000000000000, 0.8660254037844387076, 1.000000000000000000, 0.8660254037844387076, 1.000000000000000000, 0.8660254037844387076, 1.000000000000000000, 0.8660254037844387076, 1.000000000000000000, 0.8660254037844387076, 1.000000000000000000, 0.8660254037844387076, 1.000000000000000000, 0.8660254037844387076, 1.000000000000000000, 0.8660254037844387076, 1.000000000000000000, 0.8660254037844387076, 1.000000000000000000, 0.8660254037844387076, 1.000000000000000000, 0.8660254037844387076, 1.000000000000000000, 0.8660254037844387076, 1.000000000000000000, 0.8660254037844387076, 1.000000000000000000, 0.8660254037844387076, 1.000000000000000000, 0.8660254037844387076, 1.000000000000000000, 0.8660254037844387076, 1.000000000000000000, 0.8660254037844387076, 1.000000000000000000, 0.8660254037844387076, 1.000000000000000000, 0.8660254037844387076, 1.000000000000000000, 0.8660254037844387076, 1.000000000000000000, 0.8660254037844387076, 1.000000000000000000, 0.8660254037844387076, 1.000000000000000000, 0.8660254037844387076, 1.000000000000000000, 0.8660254037844387076, 1.000000000000000000, 0.8660254037844387076, 1.000000000000000000, 0.8660254037844387076, 1.000000000000000000, 0.8660254037844387076, 1.000000000000000000, 0.8660254037844387076, 1.000000000000000000, 0.8660254037844387076, 1.000000000000000000, 0.8660254037844387076, 1.000000000000000000, 0.8660254037844387076, 1.000000000000000000, 0.8660254037844387076, 1.000000000000000000, 0.8660254037844387076, 1.000000000000000000, 0.8660254037844387076, 1.000000000000000000, 0.8660254037844387076, 1.000000000000000000, 0.8660254037844387076, 1.000000000000000000, 0.8660254037844387076, 1.000000000000000000, 0.8660254037844387076, 1.000000000000000000, 0.8660254037844387076, 1.000000000000000000, 0.8660254037844387076, 1.000000000000000000, 0.8660254037844387076, 1.000000000000000000, 0.8660254037844387076, 1.000000000000000000, 0.8660254037844387076, 1.000000000000000000, 0.8660254037844387076, 1.000000000000000000, 0.8660254037844387076, 1.000000000000000000, 0.8660254037844387076, 1.000000000000000000, 0.8660254037844387076, 1.000000000000000000, 0.8660254037844387076, 1.000000000000000000, 0.8660254037844387076, 1.000000000000000000, 0.8660254037844387076, 1.000000000000000000, 0.8660254037844387076, 1.000000000000000000, 0.8660254037844387076, 1.000000000000000000) ) ) 
 REPRESENTATION_ITEM ( '' )  SURFACE ( )  );
#134654 = CARTESIAN_POINT ( 'NONE',  ( 3.596278845262687263, 0.9791764565295042466, -1.937929667198809769 ) ) ;
#134655 = CARTESIAN_POINT ( 'NONE',  ( 4.578903193113299963, 6.365139696764064325, 1.599625672291267398 ) ) ;
#134656 = CARTESIAN_POINT ( 'NONE',  ( 4.997279897388729353, -0.2910847460899004258, 1.995267753224789997 ) ) ;
#134657 = CARTESIAN_POINT ( 'NONE',  ( 0.03128095451081137207, -0.7860540964617872550, -1.895863743164089676 ) ) ;
#134658 = CARTESIAN_POINT ( 'NONE',  ( -0.7499999999999972244, 4.389583334016150751, -1.299038105676652899 ) ) ;
#134659 = CARTESIAN_POINT ( 'NONE',  ( 2.608320942171663326, -0.7355144804263250569, -1.780640224430999563 ) ) ;
#134660 = CARTESIAN_POINT ( 'NONE',  ( -1.500000000000015099, 8.510416667349460340, -0.8660254037844309360 ) ) ;
#134661 = CARTESIAN_POINT ( 'NONE',  ( 6.170221320256972675, 2.215557125880045053, -0.1624646739342323065 ) ) ;
#134662 = ORIENTED_EDGE ( 'NONE', *, *, #99445, .F. ) ;
#134663 = CARTESIAN_POINT ( 'NONE',  ( 6.883263157960399781, 2.970623603138924818, 2.399364662246627589 ) ) ;
#134664 = CARTESIAN_POINT ( 'NONE',  ( 0.7499999999999902300, 2.233333333333351156, 1.299038105676669330 ) ) ;
#134665 = CARTESIAN_POINT ( 'NONE',  ( 6.368579470117202490, 8.453095353268645695, 1.599625672291281386 ) ) ;
#134666 = CARTESIAN_POINT ( 'NONE',  ( 4.541618270453549044, 5.361271406026338227, -1.082531754730548412 ) ) ;
#134667 = CARTESIAN_POINT ( 'NONE',  ( -3.285556943750000070, -1.159374999522042815, 0.000000000000000000 ) ) ;
#134668 = EDGE_CURVE ( 'NONE', #33058, #36899, #191109, .T. ) ;
#134669 = CARTESIAN_POINT ( 'NONE',  ( 0.3994919479695389075, -0.2781545790336605317, -2.203771652037065376 ) ) ;
#134670 = CARTESIAN_POINT ( 'NONE',  ( 6.074655751228532630, 1.318658252384183438, -1.452748870126779890 ) ) ;
#134671 = CARTESIAN_POINT ( 'NONE',  ( 8.920901888112002354, 9.510066412326583674, 0.7216878364870438212 ) ) ;
#134672 = ADVANCED_FACE ( 'NONE', ( #143149 ), #30470, .T. ) ;
#134673 = CARTESIAN_POINT ( 'NONE',  ( 6.784454189598811524, -2.216766238704069636, -0.4514476129710183194 ) ) ;
#134674 = CARTESIAN_POINT ( 'NONE',  ( 4.553559489343365740, 6.405848385690952718, -1.599625672291269396 ) ) ;
#134675 = CARTESIAN_POINT ( 'NONE',  ( -4.177320726786319049, 6.927272377009067839, -1.082531754730551743 ) ) ;
#134676 = CARTESIAN_POINT ( 'NONE',  ( 3.877431937021211361, -0.1548021625025173265, 2.056941320008953245 ) ) ;
#134677 = CARTESIAN_POINT ( 'NONE',  ( -4.446184310277715213, 7.274633231044262516, -1.199719254218452047 ) ) ;
#134678 = CARTESIAN_POINT ( 'NONE',  ( 1.499999999999989120, 3.785416667349481123, 0.8660254037844524744 ) ) ;
#134679 = CARTESIAN_POINT ( 'NONE',  ( -1.364683531250014514, -0.7614583329919104582, -0.7879004041258359514 ) ) ;
#134680 = CARTESIAN_POINT ( 'NONE',  ( 5.887941446147332947, -0.8415115861447747259, 1.670666529855535654 ) ) ;
#134681 = CARTESIAN_POINT ( 'NONE',  ( 5.150864522821732017, 0.8611363216781149355, 1.505151585408972981 ) ) ;
#134682 = CARTESIAN_POINT ( 'NONE',  ( 3.649730646487856056, 0.6304092353721781894, 1.622436561192377891 ) ) ;
#134683 = CARTESIAN_POINT ( 'NONE',  ( 9.612367721964607981, 12.23751498042398289, -1.443375672974058777 ) ) ;
#134684 = CARTESIAN_POINT ( 'NONE',  ( 1.874976642369927005, -0.1173453557595251634, -2.289501271392534676 ) ) ;
#134685 = CARTESIAN_POINT ( 'NONE',  ( -0.6823417656250212460, 3.613541667008085767, 1.181850606188767472 ) ) ;
#134686 = CARTESIAN_POINT ( 'NONE',  ( 5.636299653793654940, 0.4088526781071535887, 2.050197504659311942 ) ) ;
#134687 = CARTESIAN_POINT ( 'NONE',  ( 0.4097734724025984820, 1.271762808003698009, -1.331557029818277060 ) ) ;
#134688 = DIRECTION ( 'NONE',  ( 0.000000000000000000, 0.000000000000000000, 1.000000000000000000 ) ) ;
#134689 = CARTESIAN_POINT ( 'NONE',  ( 1.758435621656749603, 1.928751379572872571, -0.5880216644931559600 ) ) ;
#134690 = CARTESIAN_POINT ( 'NONE',  ( 0.6389542677898361056, -1.877638805159736579, 1.129783718924075364 ) ) ;
#134691 = CARTESIAN_POINT ( 'NONE',  ( 9.228631970132592954, 13.18394157654138610, -9.019657609914000673 ) ) ;
#134692 = CARTESIAN_POINT ( 'NONE',  ( -6.530223543276495235, 10.77034456713125188, -0.7998128361456291469 ) ) ;
#134693 = CARTESIAN_POINT ( 'NONE',  ( 4.957477724091233995, 8.935474444748447098, -0.7998128361456281477 ) ) ;
#134694 = CARTESIAN_POINT ( 'NONE',  ( 2.280079029133400326, 2.079044457705871096, -0.4163345062310334632 ) ) ;
#134695 = CARTESIAN_POINT ( 'NONE',  ( 0.6823417656249882723, -1.157291666325249713, 1.181850606188755259 ) ) ;
#134696 = CARTESIAN_POINT ( 'NONE',  ( 5.109893933574640279, -1.816543354971979163, 0.1824992186492402357 ) ) ;
#134697 = ORIENTED_EDGE ( 'NONE', *, *, #170700, .T. ) ;
#134698 = CARTESIAN_POINT ( 'NONE',  ( -6.981522756394290319, 7.109807735406931783, 0.7998128361456341429 ) ) ;
#134699 = SURFACE_STYLE_FILL_AREA ( #151992 ) ;
#134700 = CARTESIAN_POINT ( 'NONE',  ( 3.475000000000000533, -3.952083332377417602, -2.006292185433951047 ) ) ;
#134701 = CARTESIAN_POINT ( 'NONE',  ( -6.043183783389232566, 8.073467052085995022, 1.599625672291269396 ) ) ;
#134702 = CARTESIAN_POINT ( 'NONE',  ( 2.777608160125254688, 0.2920557517631214295, -1.998411540393054020 ) ) ;
#134703 = CARTESIAN_POINT ( 'NONE',  ( 6.299877592275240801, -0.7493655176046759570, 2.075778730795534877 ) ) ;
#134704 = CARTESIAN_POINT ( 'NONE',  ( 8.543609354905870035, 13.11929468069890525, 0.7998128361456462443 ) ) ;
#134705 = CARTESIAN_POINT ( 'NONE',  ( 4.451900780290086956, -0.7152352812324501707, 1.718214207458491849 ) ) ;
#134706 = CARTESIAN_POINT ( 'NONE',  ( 8.866142388332804103, 12.43125098877526113, -1.199719254218446718 ) ) ;
#134707 = CARTESIAN_POINT ( 'NONE',  ( 2.907633421442281207, 6.614265768316455407, -0.2557691087421434251 ) ) ;
#134708 = CARTESIAN_POINT ( 'NONE',  ( -2.916975605234527702, 6.554888639415577423, 1.040834085586084257E-14 ) ) ;
#134709 = CARTESIAN_POINT ( 'NONE',  ( -8.857554428429624593, 9.228235009456373206, 0.7998128361456462443 ) ) ;
#134711 = CARTESIAN_POINT ( 'NONE',  ( -4.172014829671058855, 7.596244486910340044, 0.9145543751994407167 ) ) ;
#134710 = CARTESIAN_POINT ( 'NONE',  ( -6.774234028683526532, 7.932303117332766718, 1.199719254218452047 ) ) ;
#134712 = CARTESIAN_POINT ( 'NONE',  ( 0.6823417656249864960, -0.5739583329919112353, -1.181850606188749264 ) ) ;
#134713 = CARTESIAN_POINT ( 'NONE',  ( 1.475528429365607019, 1.526226248090801318, 0.8227105958887138693 ) ) ;
#134714 = CARTESIAN_POINT ( 'NONE',  ( 1.517106797927396444, -0.9646358079543941866, -1.448293472534349702 ) ) ;
#134715 = PRESENTATION_LAYER_ASSIGNMENT (  '', '', ( #2753 ) ) ;
#134717 = CARTESIAN_POINT ( 'NONE',  ( 7.131225611108079399, 11.26358761302737754, 0.7216878364870438212 ) ) ;
#134716 = CARTESIAN_POINT ( 'NONE',  ( 5.356226580172758212, 2.305273348739949935, -0.1085102657557151934 ) ) ;
#134718 = CARTESIAN_POINT ( 'NONE',  ( 5.090160327287878594, 4.903218234782778850, -0.7998128361456481317 ) ) ;
#134719 = CARTESIAN_POINT ( 'NONE',  ( 1.194684731684968693, -0.4980721920408748282, -1.999570191575838818 ) ) ;
#134720 = AXIS2_PLACEMENT_3D ( 'NONE', #193367, #129530, #143601 ) ;
#134721 = CARTESIAN_POINT ( 'NONE',  ( 6.872461156203343080, -0.5239007177601956444, 2.246970456009795836 ) ) ;
#134722 = DIRECTION ( 'NONE',  ( 0.000000000000000000, -1.000000000000000000, 0.000000000000000000 ) ) ;
#134723 = CARTESIAN_POINT ( 'NONE',  ( -6.784929528996132220, 6.880448970109080520, 0.000000000000000000 ) ) ;
#134724 = CARTESIAN_POINT ( 'NONE',  ( 6.754772315933175619, -1.444328698515121800, 1.188528157999017454 ) ) ;
#134726 = CARTESIAN_POINT ( 'NONE',  ( -5.478903473698241378, 9.406154796041011679, -0.7216878364870338292 ) ) ;
#134725 = CARTESIAN_POINT ( 'NONE',  ( 4.605663860560767375, 1.420894170025093439, 1.280184534114735095 ) ) ;
#134727 = CARTESIAN_POINT ( 'NONE',  ( 6.129534211984397629, -2.079372889712034489, 0.7396383780838566846 ) ) ;
#134728 = CARTESIAN_POINT ( 'NONE',  ( -0.6125000000000053735, 2.020833334016133964, -1.060881119635941339 ) ) ;
#134729 = CARTESIAN_POINT ( 'NONE',  ( 0.7500000000000006661, 10.66666666666666430, -1.299038105676657340 ) ) ;
#134730 = CARTESIAN_POINT ( 'NONE',  ( 4.624739795592929248, 6.488892076315451618, -1.443375672974068769 ) ) ;
#134731 = CARTESIAN_POINT ( 'NONE',  ( -4.950135482320929370, 5.908151163196758482, -1.082531754730549967 ) ) ;
#134732 = CARTESIAN_POINT ( 'NONE',  ( 0.4518267731568551548, -1.429874679360541023, -1.426642250087527541 ) ) ;
#134733 = VERTEX_POINT ( 'NONE', #128019 ) ;
#134734 = CARTESIAN_POINT ( 'NONE',  ( 3.891899753260852801, 1.669126095664546838, 1.593640439619238514 ) ) ;
#134736 = EDGE_CURVE ( 'NONE', #210733, #123356, #49296, .T. ) ;
#134735 = CARTESIAN_POINT ( 'NONE',  ( 4.369553226407375313, -0.3375162941181614751, 1.932460123137308861 ) ) ;
#134737 = CARTESIAN_POINT ( 'NONE',  ( 0.4968289091572677396, 0.3296062100675010154, 1.933703066120408209 ) ) ;
#134738 = CARTESIAN_POINT ( 'NONE',  ( 3.307826292054301121, 4.882216645528547616, -1.443375672974057666 ) ) ;
#134739 = DIRECTION ( 'NONE',  ( 1.000000000000000000, 0.000000000000000000, 8.638326563840826660E-31 ) ) ;
#134740 = EDGE_LOOP ( 'NONE', ( #165396, #117470, #59861, #22725 ) ) ;
#134741 = CARTESIAN_POINT ( 'NONE',  ( 6.456263137377813877, -1.236968576560824040, 1.593241027169020052 ) ) ;
#134742 = CARTESIAN_POINT ( 'NONE',  ( -5.949330478298285207, 5.835307067636438028, 0.7998128361456341429 ) ) ;
#134743 = CARTESIAN_POINT ( 'NONE',  ( 2.676840970354518845, 1.421027823260514911, -1.641450307487320792 ) ) ;
#134744 = CARTESIAN_POINT ( 'NONE',  ( 9.348761378620913831, 13.52553930298124918, -7.449808453853659529 ) ) ;
#134745 = CARTESIAN_POINT ( 'NONE',  ( 1.072698285844303934, 0.8645715524648779349, 1.936551149067309741 ) ) ;
#134746 = CARTESIAN_POINT ( 'NONE',  ( -1.500000000000013101, 2.160416667349489561, -0.8660254037844313801 ) ) ;
#134747 = CARTESIAN_POINT ( 'NONE',  ( 10.07778825365955733, 10.65184113889131012, -0.7998128361456281477 ) ) ;
#134748 = CARTESIAN_POINT ( 'NONE',  ( 11.96535697748077709, 13.75262667064441935, -0.9148528286455174241 ) ) ;
#134749 = CARTESIAN_POINT ( 'NONE',  ( 6.440439394220377700, 6.875545743132385645, 0.7017714770480776298 ) ) ;
#134750 = CARTESIAN_POINT ( 'NONE',  ( 2.583338899891209017, 1.885494326376845775, -0.8321024974875782521 ) ) ;
#134752 = DIRECTION ( 'NONE',  ( 0.000000000000000000, 1.000000000000000000, 0.000000000000000000 ) ) ;
#134751 = CARTESIAN_POINT ( 'NONE',  ( -10.10098813738111545, 11.74323990082152491, -1.199719254218441611 ) ) ;
#134753 = CARTESIAN_POINT ( 'NONE',  ( -1.402160292154681736E-14, 1.946875000341422579, -1.575800808251660134 ) ) ;
#134754 = CARTESIAN_POINT ( 'NONE',  ( -1.499999999999997780, 4.181250000682819490, 1.214306433183764966E-14 ) ) ;
#134755 = ADVANCED_FACE ( 'NONE', ( #156167 ), #125439, .F. ) ;
#134756 = CARTESIAN_POINT ( 'NONE',  ( 5.704082950214642622, 7.400961370687027419, -1.366768684276008283 ) ) ;
#134757 = ORIENTED_EDGE ( 'NONE', *, *, #142755, .F. ) ;
#134758 = CARTESIAN_POINT ( 'NONE',  ( 4.793567869993575314, 1.782951692925707654, -0.6917526515820491273 ) ) ;
#134759 = CARTESIAN_POINT ( 'NONE',  ( -11.84104725192634966, 11.10983537451415870, 1.443823348526939165 ) ) ;
#134760 = CARTESIAN_POINT ( 'NONE',  ( 1.089599759544016999, 1.994953948513054742, -1.067007742874733545 ) ) ;
#134761 = CARTESIAN_POINT ( 'NONE',  ( -2.442440228756222353, 6.001264033524212671, -0.7998128361456281477 ) ) ;
#134762 = CARTESIAN_POINT ( 'NONE',  ( 1.581973821214562204, 0.9331543445117953528, 1.552620351220496353 ) ) ;
#134763 = CARTESIAN_POINT ( 'NONE',  ( 0.8135319083415553099, -1.217954555017298324, -1.478650609923468195 ) ) ;
#134764 = CARTESIAN_POINT ( 'NONE',  ( 1.645070734656968625, -0.3017366986639741788, -2.048123538821471801 ) ) ;
#134765 = CARTESIAN_POINT ( 'NONE',  ( -0.6823417656250003738, 0.7802083336747520637, -1.181850606188749264 ) ) ;
#134766 = CARTESIAN_POINT ( 'NONE',  ( 6.819227946136852125, -0.1326586024288610444, 1.840611662119538749 ) ) ;
#134767 = CARTESIAN_POINT ( 'NONE',  ( 5.971306315489836258, 0.1393824199819072851, -1.921517340817725961 ) ) ;
#134769 = CARTESIAN_POINT ( 'NONE',  ( 5.969043672405669909, 7.102642550806028687, -1.084880274121432064 ) ) ;
#134768 = CARTESIAN_POINT ( 'NONE',  ( 6.375609195709820654, 2.113139023092651225, -0.6363509056886568205 ) ) ;
#134770 = CARTESIAN_POINT ( 'NONE',  ( -1.364683531250014514, 1.238541667008091096, -0.7879004041258289570 ) ) ;
#134771 = CARTESIAN_POINT ( 'NONE',  ( 3.912594259961211574, 0.7396031425229695477, 1.925699983396757409 ) ) ;
#134772 = CARTESIAN_POINT ( 'NONE',  ( -7.576308911938196999, 7.733448573549685179, 0.7998128361456462443 ) ) ;
#134773 = CARTESIAN_POINT ( 'NONE',  ( 8.158255747121103241, 10.54105100977322174, 1.599625672291281386 ) ) ;
#134774 = CARTESIAN_POINT ( 'NONE',  ( -3.189213936345698830, 2.817530495244580102, 2.450448857954578230 ) ) ;
#134775 = CARTESIAN_POINT ( 'NONE',  ( 6.017121246366603060, 5.914396297049491658, 1.040834085586084257E-14 ) ) ;
#134777 = CARTESIAN_POINT ( 'NONE',  ( -1.201851678989727383E-14, 3.962500000000022116, 1.732050807568877637 ) ) ;
#134776 = CARTESIAN_POINT ( 'NONE',  ( 4.911209521004105127, 1.831006069304096373, 1.040297942642433249 ) ) ;
#134778 = CARTESIAN_POINT ( 'NONE',  ( 6.830528382861658088, -1.277203763263988101, 1.630111558092485868 ) ) ;
#134779 = CARTESIAN_POINT ( 'NONE',  ( -1.364683531250014514, 0.8010416670080889867, -0.7879004041258289570 ) ) ;
#134780 = CARTESIAN_POINT ( 'NONE',  ( 4.587301040747738590, 1.933109172225885963, -0.9673573668882374799 ) ) ;
#134782 = EDGE_CURVE ( 'NONE', #173974, #77951, #109615, .T. ) ;
#134781 = CARTESIAN_POINT ( 'NONE',  ( 5.795571226005820087, 1.865288689459403848, -0.7749498061812712946 ) ) ;
#134783 = DIRECTION ( 'NONE',  ( 0.000000000000000000, 0.000000000000000000, -1.000000000000000000 ) ) ;
#134784 = ADVANCED_FACE ( 'NONE', ( #123748 ), #135722, .T. ) ;
#134787 = CARTESIAN_POINT ( 'NONE',  ( 6.331294547901813452, 6.488857848747989543, 1.040834085586084257E-14 ) ) ;
#134786 = CARTESIAN_POINT ( 'NONE',  ( 3.285556943750000070, -2.384374999522043126, 0.000000000000000000 ) ) ;
#134785 = CARTESIAN_POINT ( 'NONE',  ( 6.526270840131753737, 8.707344961610770540, -1.599625672291283607 ) ) ;
#134788 = CARTESIAN_POINT ( 'NONE',  ( -7.144220599758281054, 7.299621885998258897, 0.7998128361456341429 ) ) ;
#134789 = CARTESIAN_POINT ( 'NONE',  ( 3.960172920142067898, -1.157100329752266621, 1.651342637023434090 ) ) ;
#134790 = CARTESIAN_POINT ( 'NONE',  ( -7.167456763118792651, 11.51378332361394818, 0.000000000000000000 ) ) ;
#134792 = FILL_AREA_STYLE_COLOUR ( '', #195445 ) ;
#134791 = CARTESIAN_POINT ( 'NONE',  ( -4.603156847039612920, 5.329103395422994716, 1.199719254218462483 ) ) ;
#134793 = CARTESIAN_POINT ( 'NONE',  ( -8.012344526598182026E-15, 8.546875000341403350, -1.575800808251669460 ) ) ;
#134794 = CARTESIAN_POINT ( 'NONE',  ( 0.000000000000000000, 6.487495393664096888, -3.100011470320000573 ) ) ;
#134795 = CARTESIAN_POINT ( 'NONE',  ( -1.453605123272271094, 13.24045051524828942, -0.3701785320580647798 ) ) ;
#134797 = CARTESIAN_POINT ( 'NONE',  ( 4.112907772398490813, 0.1017678201147946826, 2.013986186455194449 ) ) ;
#134796 = CARTESIAN_POINT ( 'NONE',  ( -6.927853306458756855, 9.105581495667113501, 1.443375672974078761 ) ) ;
#134798 = CARTESIAN_POINT ( 'NONE',  ( 1.499999999999989120, 5.795833333333350268, -0.8660254037844323793 ) ) ;
#134799 = CARTESIAN_POINT ( 'NONE',  ( 0.2930059409478984467, 1.274291793118907723, 1.162708412170476713 ) ) ;
#134800 = CARTESIAN_POINT ( 'NONE',  ( 5.550083779947807550, 7.568460058062819407, -1.599625672291283607 ) ) ;
#134802 = CARTESIAN_POINT ( 'NONE',  ( 5.982890925380405456, 10.20206618957764100, 0.000000000000000000 ) ) ;
#134801 = CARTESIAN_POINT ( 'NONE',  ( 7.131225611108079399, 11.26358761302737754, 0.7216878364870438212 ) ) ;
#134803 = MECHANICAL_DESIGN_GEOMETRIC_PRESENTATION_REPRESENTATION (  '', ( #214343 ), #55309 ) ;
#134804 = CARTESIAN_POINT ( 'NONE',  ( -10.82839673812366321, 6.397356466741112690, 5.188991974343044156 ) ) ;
#134805 = CARTESIAN_POINT ( 'NONE',  ( 5.061713478001653499, 1.850364105758989020, -0.2730526881008291662 ) ) ;
#134806 = CARTESIAN_POINT ( 'NONE',  ( 6.029547050951932441, -0.2422988993314358630, 1.998484822443524322 ) ) ;
#134807 =( LENGTH_UNIT ( ) NAMED_UNIT ( * ) SI_UNIT ( .MILLI., .METRE. ) );
#134808 = CARTESIAN_POINT ( 'NONE',  ( -6.089020385868856522, 9.157588645938716354, -1.082531754730549967 ) ) ;
#134809 = ORIENTED_EDGE ( 'NONE', *, *, #205068, .F. ) ;
#134810 = CARTESIAN_POINT ( 'NONE',  ( 8.527715432871318058, 12.89282573841782664, -0.7216878364870338292 ) ) ;
#134811 = CARTESIAN_POINT ( 'NONE',  ( 0.1754079408978586052, 1.496066871905444851, 1.352139405095334590 ) ) ;
#134812 = CARTESIAN_POINT ( 'NONE',  ( 1.388595261843462714, -1.720809334905664567, -0.5665428721913360333 ) ) ;
#134813 = CARTESIAN_POINT ( 'NONE',  ( 7.309781096423290769, 8.557108029695882578, 1.199719254218452935 ) ) ;
#134814 = CARTESIAN_POINT ( 'NONE',  ( 6.717278222822382183, -7.246166700180828535, -6.750415307812249743 ) ) ;
#134815 = MECHANICAL_DESIGN_GEOMETRIC_PRESENTATION_REPRESENTATION (  '', ( #68896 ), #207298 ) ;
#134816 = CARTESIAN_POINT ( 'NONE',  ( 7.637320603199683866, 7.804628880021436288, -0.7998128361456281477 ) ) ;
#134818 = CARTESIAN_POINT ( 'NONE',  ( 0.1279635871501626776, 1.910768599467532081, 0.1380287717926073077 ) ) ;
#134817 = CARTESIAN_POINT ( 'NONE',  ( -6.389970470742427189, 6.349387058821269747, -0.7998128361456291469 ) ) ;
#134819 = DIRECTION ( 'NONE',  ( 0.000000000000000000, 0.000000000000000000, 1.000000000000000000 ) ) ;
#134820 = FACE_OUTER_BOUND ( 'NONE', #136573, .T. ) ;
#134821 = CARTESIAN_POINT ( 'NONE',  ( 0.6823417656249864960, -0.7614583329919113464, -1.181850606188749264 ) ) ;
#134822 = CARTESIAN_POINT ( 'NONE',  ( 3.877268743828276243, 4.586196958296845594, 1.082531754730560403 ) ) ;
#134823 = CARTESIAN_POINT ( 'NONE',  ( -10.64723070543352712, 11.31619066596094392, 0.7998128361456462443 ) ) ;
#134824 = B_SPLINE_CURVE_WITH_KNOTS ( 'NONE', 3,
 ( #140933, #158225, #108465, #43412, #124732, #206947 ),
 .UNSPECIFIED., .F., .F.,
 ( 4, 2, 4 ),
 ( 0.0006378314054480060599, 0.0009584618939205532184, 0.001279092382393100377 ),
 .UNSPECIFIED. ) ;
#134825 = CARTESIAN_POINT ( 'NONE',  ( 4.276362541559985075, -1.246951984143488623, 1.765614359104182629 ) ) ;
#134826 = CARTESIAN_POINT ( 'NONE',  ( -5.126391479742927970, 8.994890803093138487, 0.7216878364870267237 ) ) ;
#134827 = CARTESIAN_POINT ( 'NONE',  ( 6.712695452541852070, 7.004101914153185504, 0.000000000000000000 ) ) ;
#134828 = CARTESIAN_POINT ( 'NONE',  ( 1.072698285844303934, 0.8645715524648778239, 1.936551149067309519 ) ) ;
#134829 = CARTESIAN_POINT ( 'NONE',  ( 0.4683205530892388113, -8.233137084989849086, 9.568546172724163412 ) ) ;
#134830 =( BOUNDED_SURFACE ( )  B_SPLINE_SURFACE ( 3, 2, ( 
 ( #14444, #210523, #160721 ),
 ( #79466, #145583, #12314 ),
 ( #123254, #146630, #211580 ),
 ( #171906, #129378, #112045 ),
 ( #74412, #73318, #205456 ),
 ( #80534, #78395, #189219 ) ),
 .UNSPECIFIED., .F., .F., .T. ) 
 B_SPLINE_SURFACE_WITH_KNOTS ( ( 4, 2, 4 ),
 ( 3, 3 ),
 ( 0.0001465838689801550747, 0.0002810652682710439903, 0.0004155466675619328516 ),
 ( 0.000000000000000000, 1.000000000000000000 ),
 .UNSPECIFIED. ) 
 GEOMETRIC_REPRESENTATION_ITEM ( )  RATIONAL_B_SPLINE_SURFACE ( (
 ( 1.000000000000000000, 0.8789000212895440312, 1.000000000000000000),
 ( 1.000000000000000000, 0.9073166784884890701, 1.000000000000000000),
 ( 1.000000000000000000, 0.9160359019619150889, 1.000000000000000000),
 ( 1.000000000000000000, 0.8858134948703313416, 1.000000000000000000),
 ( 1.000000000000000000, 0.8506312074210923280, 1.000000000000000000),
 ( 1.000000000000000000, 0.8104931255412307634, 1.000000000000000000) ) ) 
 REPRESENTATION_ITEM ( '' )  SURFACE ( )  );
#134831 = CARTESIAN_POINT ( 'NONE',  ( 2.249238725404782091, -1.581088017263340806, -1.177247449022495118 ) ) ;
#134832 = CARTESIAN_POINT ( 'NONE',  ( 4.728717205193702533, 1.314622909153417174, -1.389140896021365368 ) ) ;
#134833 = ORIENTED_EDGE ( 'NONE', *, *, #43875, .T. ) ;
#134834 = DIRECTION ( 'NONE',  ( 0.6507913734559640506, -0.7592566023653003482, 0.000000000000000000 ) ) ;
#134835 = CARTESIAN_POINT ( 'NONE',  ( 6.619592842669682398, 0.3380432134332654881, -1.940159576567195288 ) ) ;
#134836 = CARTESIAN_POINT ( 'NONE',  ( 1.868985280173897756, 1.858391233338702042, -0.5634987755925959796 ) ) ;
#134837 = ORIENTED_EDGE ( 'NONE', *, *, #54753, .F. ) ;
#134838 = CARTESIAN_POINT ( 'NONE',  ( -5.808742468812186033, 5.741564066561132940, 0.000000000000000000 ) ) ;
#134840 = CARTESIAN_POINT ( 'NONE',  ( 6.783773251375732727, -6.684699875907444522, -6.634380621478984885 ) ) ;
#134839 = CARTESIAN_POINT ( 'NONE',  ( -3.149236820124241110, 6.896136400112061970, -0.7998128361456481317 ) ) ;
#134842 = CARTESIAN_POINT ( 'NONE',  ( 3.892599500454932304, 7.555466827257172113, 0.7216878364870257245 ) ) ;
#134841 = CARTESIAN_POINT ( 'NONE',  ( 6.446011968293428041, 9.607765498729298415, -1.199719254218440723 ) ) ;
#134844 = EDGE_LOOP ( 'NONE', ( #174673, #129645, #190536, #119231 ) ) ;
#134843 = CARTESIAN_POINT ( 'NONE',  ( 4.740819843082155316, 1.831016553098392619, 0.5515768964349797576 ) ) ;
#134845 = CARTESIAN_POINT ( 'NONE',  ( 3.616033620774202983, -2.174319932014677548, 0.3768175846284789743 ) ) ;
#134846 = CARTESIAN_POINT ( 'NONE',  ( 1.764966765715753949, -1.560254191817540992, 1.560848541443552895 ) ) ;
#134847 = CARTESIAN_POINT ( 'NONE',  ( 0.4205683736966537856, 3.129384673317387122, -0.4296503687815898531 ) ) ;
#134848 = CARTESIAN_POINT ( 'NONE',  ( 0.4692111731946085884, -1.615589042895089200, -1.022764193708516789 ) ) ;
#134849 = CARTESIAN_POINT ( 'NONE',  ( 0.07680821025391955381, 1.395885924038504644, -2.068540888291516833 ) ) ;
#134850 = CARTESIAN_POINT ( 'NONE',  ( -2.279673327426077645, 5.603443282064907827, 0.1981503615792774842 ) ) ;
#134851 = CARTESIAN_POINT ( 'NONE',  ( -0.02299836291579685638, 7.070324784597906920, 4.060433046130490276 ) ) ;
#134852 = CARTESIAN_POINT ( 'NONE',  ( 3.297389726143422184, -1.827171938055579314, 0.9735347560282038293 ) ) ;
#134853 = CARTESIAN_POINT ( 'NONE',  ( -5.117312914154178216, 8.057616602233474978, -1.199719254218452047 ) ) ;
#134854 = CARTESIAN_POINT ( 'NONE',  ( -6.184982820901517186, 6.966600618058066630, 0.8941503475990535410 ) ) ;
#134856 = CARTESIAN_POINT ( 'NONE',  ( 0.5499753625364013354, 0.6768306982547143136, -2.053065283773393368 ) ) ;
#134855 = CARTESIAN_POINT ( 'NONE',  ( -4.386226389220933441, 5.076017861301227008, -1.199719254218446718 ) ) ;
#134857 = CARTESIAN_POINT ( 'NONE',  ( 3.263397454411249399, 2.137687552337414587, -0.4822058812353549606 ) ) ;
#134858 = CARTESIAN_POINT ( 'NONE',  ( -4.398886013728402489, 7.974527572605470738, 0.5967842075597221685 ) ) ;
#134859 = CARTESIAN_POINT ( 'NONE',  ( 4.258669648468281110, 6.061810238003387141, 1.443375672974058777 ) ) ;
#134860 = CARTESIAN_POINT ( 'NONE',  ( -0.6125000000000279110, 1.104166667349484765, 1.060881119635904923 ) ) ;
#134861 = STYLED_ITEM ( 'NONE', ( #173213 ), #160190 ) ;
#134862 = CARTESIAN_POINT ( 'NONE',  ( -0.6823417656250003738, 12.71354166700806942, 1.181850606188754593 ) ) ;
#134863 = CARTESIAN_POINT ( 'NONE',  ( -6.143779885648060102, 7.196773283791382703, 1.199719254218452047 ) ) ;
#134864 = UNCERTAINTY_MEASURE_WITH_UNIT (LENGTH_MEASURE( 1.000000000000000082E-05 ), #79255, 'distance_accuracy_value', 'NONE');
#134865 = CARTESIAN_POINT ( 'NONE',  ( 6.381516696256908538, -0.4728550111133908995, -1.668365442416564814 ) ) ;
#134866 = CARTESIAN_POINT ( 'NONE',  ( -9.707274797704657843, 11.38787068781932987, 1.082531754730558626 ) ) ;
#134867 = CARTESIAN_POINT ( 'NONE',  ( 3.995033623311712301, 0.2988084191791628985, 2.048438004591215389 ) ) ;
#134868 = CARTESIAN_POINT ( 'NONE',  ( 4.411780756640943046, -1.303739072956756617, -1.668109288273095014 ) ) ;
#134869 = CARTESIAN_POINT ( 'NONE',  ( 7.474622759835693131, 7.614814729430110951, -0.7998128361456281477 ) ) ;
#134870 = CARTESIAN_POINT ( 'NONE',  ( 0.6823417656249917140, 5.092708333674749177, 1.181850606188765695 ) ) ;
#134871 = CARTESIAN_POINT ( 'NONE',  ( 2.465619613223976270, -0.4363654233677862759, 1.920310867443141278 ) ) ;
#134872 = CARTESIAN_POINT ( 'NONE',  ( 1.300873410958070409, -0.2835801433653042380, -1.891145142470892715 ) ) ;
#134873 = CARTESIAN_POINT ( 'NONE',  ( 5.226663038502143088, 0.1645964690673335229, 2.286419844370500165 ) ) ;
#134874 = CARTESIAN_POINT ( 'NONE',  ( 3.316849939159485228, 1.650902842016691130, 0.7798126646740562995 ) ) ;
#134875 = CARTESIAN_POINT ( 'NONE',  ( 5.415556014015861841, 5.282846535965431300, -0.7998128361456481317 ) ) ;
#134876 = CARTESIAN_POINT ( 'NONE',  ( 6.439759776366780208, 6.615400615290456088, 0.7216878364870317197 ) ) ;
#134877 = CARTESIAN_POINT ( 'NONE',  ( -5.357443255694392725, 9.402100898285455699, 0.000000000000000000 ) ) ;
#134878 = CARTESIAN_POINT ( 'NONE',  ( 4.166274970888473206, 2.012660793657996106, -0.05373556394885727755 ) ) ;
#134879 = CARTESIAN_POINT ( 'NONE',  ( 3.836726278109466204, -1.889416792123297162, -0.5274722977551549175 ) ) ;
#134880 = CARTESIAN_POINT ( 'NONE',  ( -8.019811557683421910, 9.315200557840817908, 1.199719254218462483 ) ) ;
#134881 = CARTESIAN_POINT ( 'NONE',  ( -4.574986769607567894, 7.424902766929059261, 1.199719254218464037 ) ) ;
#134882 = CARTESIAN_POINT ( 'NONE',  ( 0.1753634416057497647, 0.2329791690731698173, -2.177930625204091086 ) ) ;
#134884 = CARTESIAN_POINT ( 'NONE',  ( 5.471497560916138703, 1.704843785431299219, -0.4750155384096472755 ) ) ;
#134883 = CARTESIAN_POINT ( 'NONE',  ( -0.1234093946873336678, -0.1598125250084568849, -2.056614676860648583 ) ) ;
#134885 = DIRECTION ( 'NONE',  ( 0.6507913734559596097, -0.7592566023653043450, 0.000000000000000000 ) ) ;
#134886 = CARTESIAN_POINT ( 'NONE',  ( 1.623246906879351581, -2.062630869249089116, 0.7406334225198917265 ) ) ;
#134887 = CARTESIAN_POINT ( 'NONE',  ( 6.263578219495629540, 0.9010232283708031753, 1.488777805958479528 ) ) ;
#134888 = CARTESIAN_POINT ( 'NONE',  ( 8.437251666405968464, 8.737881787095446384, 1.040834085586084257E-14 ) ) ;
#134889 = CARTESIAN_POINT ( 'NONE',  ( 0.1335669894368343991, 6.947499997881672940, -2.748639729795236963 ) ) ;
#134890 = CARTESIAN_POINT ( 'NONE',  ( 0.4512176508754310866, 0.5462255407458499468, -1.636193974722987221 ) ) ;
#134891 = CARTESIAN_POINT ( 'NONE',  ( 0.5800033175489105464, 1.582751930679682228, -1.666757776657208145 ) ) ;
#134892 = CARTESIAN_POINT ( 'NONE',  ( 0.5038066827526345159, -2.180447833630628107, 0.2205874978757973448 ) ) ;
#134893 = CARTESIAN_POINT ( 'NONE',  ( 6.309869086801066729, -1.462580435118435496, 0.9307709330467325293 ) ) ;
#134894 = CARTESIAN_POINT ( 'NONE',  ( 2.473496279428960776, 0.1070396533628548558, -2.204406164007084445 ) ) ;
#134895 = CARTESIAN_POINT ( 'NONE',  ( 6.514155524301521005, 2.165825943586483504, -0.1531846826740568268 ) ) ;
#134896 = FACE_OUTER_BOUND ( 'NONE', #191016, .T. ) ;
#134897 = CARTESIAN_POINT ( 'NONE',  ( 1.253280101782401124, 0.1498745247594003016, -2.112069961602327517 ) ) ;
#134898 = CARTESIAN_POINT ( 'NONE',  ( 6.827182134110223899, 2.937564492898884438, 2.740749177975018380 ) ) ;
#134899 = CARTESIAN_POINT ( 'NONE',  ( 4.981433139801599630, 1.797578344525651906, -0.6930591852608753989 ) ) ;
#134900 = ORIENTED_EDGE ( 'NONE', *, *, #202203, .F. ) ;
#134902 = CARTESIAN_POINT ( 'NONE',  ( -1.499999999999997780, 5.150000000000022560, 1.214306433183764966E-14 ) ) ;
#134901 = CARTESIAN_POINT ( 'NONE',  ( 1.224644656679523713, 2.210950556192964989, 0.6053773189644614527 ) ) ;
#134903 = CARTESIAN_POINT ( 'NONE',  ( 3.684065054611349144, 5.321161868511784299, -1.599625672291262513 ) ) ;
#134904 = CARTESIAN_POINT ( 'NONE',  ( 4.808338034340912337, 8.761478140039733020, 1.040834085586084257E-14 ) ) ;
#134905 = ADVANCED_FACE ( 'NONE', ( #108536 ), #193973, .F. ) ;
#134906 = CARTESIAN_POINT ( 'NONE',  ( 5.391355351084783365, -0.05288786341082692827, -2.220837934544753089 ) ) ;
#134907 = CARTESIAN_POINT ( 'NONE',  ( -8.039621903223732602, 8.481906429956900695, 1.040834085586084257E-14 ) ) ;
#134908 = CARTESIAN_POINT ( 'NONE',  ( 6.331294547901813452, 6.488857848747989543, 1.040834085586084257E-14 ) ) ;
#134909 = CARTESIAN_POINT ( 'NONE',  ( -7.578644679914719795, 9.864838098032418401, 1.443375672974090751 ) ) ;
#134910 = CARTESIAN_POINT ( 'NONE',  ( 5.804299160426222848, 7.865044668620976509, -1.443375672974078761 ) ) ;
#134911 = ORIENTED_EDGE ( 'NONE', *, *, #46704, .T. ) ;
#134912 = CARTESIAN_POINT ( 'NONE',  ( 1.934220422044398813, -1.621183349045727473, -1.198859219795316955 ) ) ;
#134914 = CARTESIAN_POINT ( 'NONE',  ( 1.217717225187223473, 0.4062273103370617755, -2.022011198395957887 ) ) ;
#134913 = CARTESIAN_POINT ( 'NONE',  ( 7.130698725783555680, 10.40656671580112658, 1.199719254218460707 ) ) ;
#134915 = CARTESIAN_POINT ( 'NONE',  ( -6.830415307812261361, -7.246166700180801001, -6.717278222822380407 ) ) ;
#134916 = CARTESIAN_POINT ( 'NONE',  ( 5.004368096775565711, 8.852530189631227842, -0.7216878364870458196 ) ) ;
#134917 = CARTESIAN_POINT ( 'NONE',  ( 10.67870335800436621, -6.148216694138044502, -1.725267604293023415E-15 ) ) ;
#134918 = CARTESIAN_POINT ( 'NONE',  ( -1.201851678989727383E-14, 3.821875000341423689, 1.575800808251672791 ) ) ;
#134920 = B_SPLINE_CURVE_WITH_KNOTS ( 'NONE', 3,
 ( #126536, #142737, #208746, #28953, #144877, #78752, #60373, #192498 ),
 .UNSPECIFIED., .F., .F.,
 ( 4, 2, 2, 4 ),
 ( 0.0007320770841321901784, 0.0008843033762534650366, 0.001036529668374739678, 0.001340982252617288527 ),
 .UNSPECIFIED. ) ;
#134919 = CARTESIAN_POINT ( 'NONE',  ( 3.837968455498752096, 2.180838135830205804, 0.2153102754597763235 ) ) ;
#134921 = CARTESIAN_POINT ( 'NONE',  ( 0.8092204703840089053, 1.198858234535697065, -1.621184076614573533 ) ) ;
#134922 = CARTESIAN_POINT ( 'NONE',  ( 0.8723036553972834950, -0.04505207493780280514, -1.840872848514919502 ) ) ;
#134923 = CARTESIAN_POINT ( 'NONE',  ( 5.566080547264319556, -1.456586111465259403, 1.770153815000871989 ) ) ;
#134924 = CARTESIAN_POINT ( 'NONE',  ( 3.257574473681293270, 0.8286728953739975756, 1.644182576024610265 ) ) ;
#134925 = CARTESIAN_POINT ( 'NONE',  ( 9.260382613333817403, 10.76253345609967660, -1.199719254218446718 ) ) ;
#134927 = EDGE_CURVE ( 'NONE', #165662, #194636, #42354, .T. ) ;
#134926 =( NAMED_UNIT ( * ) PLANE_ANGLE_UNIT ( ) SI_UNIT ( $, .RADIAN. ) );
#134928 = CARTESIAN_POINT ( 'NONE',  ( 4.577060434696750946, -0.0006114206978560799951, -1.825762228460731551 ) ) ;
#134929 = CARTESIAN_POINT ( 'NONE',  ( 4.641250102003463773, 0.7743139518727223392, 1.862017545363145565 ) ) ;
#134930 = CARTESIAN_POINT ( 'NONE',  ( -7.330154606482786050, 11.70359747420527619, 0.000000000000000000 ) ) ;
#134932 = CARTESIAN_POINT ( 'NONE',  ( -6.420668264523499147, 9.648474187656182366, 1.199719254218452935 ) ) ;
#134931 = CARTESIAN_POINT ( 'NONE',  ( 4.487383681424582882, 2.022794180288649990, -1.013680454646571638 ) ) ;
#134933 = CARTESIAN_POINT ( 'NONE',  ( 6.106491565043327796, -0.7546634490227432934, -1.966289716088761796 ) ) ;
#134934 = CARTESIAN_POINT ( 'NONE',  ( 3.104029480343179603, 0.7476448069429382226, -1.930825944200013966 ) ) ;
#134935 = CARTESIAN_POINT ( 'NONE',  ( 3.379006598303866848, 4.965260336153046516, -1.599625672291262513 ) ) ;
#134936 = CARTESIAN_POINT ( 'NONE',  ( -0.6801582343750177673, 1.713541667008065872, 1.178068619123799898 ) ) ;
#134937 = PRODUCT_CONTEXT ( 'NONE', #97515, 'mechanical' ) ;
#134939 = CARTESIAN_POINT ( 'NONE',  ( 1.980962579895541920, -0.09440724433935901438, -1.924309447538669060 ) ) ;
#134938 = CARTESIAN_POINT ( 'NONE',  ( -8.962103233833181193, 10.41454084668224489, -1.199719254218446718 ) ) ;
#134940 = CARTESIAN_POINT ( 'NONE',  ( -5.178288325776719603, 5.006034233019745372, 0.000000000000000000 ) ) ;
#134941 = CARTESIAN_POINT ( 'NONE',  ( 0.3265233526151562482, -1.289390354768883862, 1.488895225407897538 ) ) ;
#134942 = CARTESIAN_POINT ( 'NONE',  ( 3.567203813726949058, 7.175838526074521440, 0.7216878364870257245 ) ) ;
#134943 = CARTESIAN_POINT ( 'NONE',  ( 5.890517129559706078, 5.978185313570312687, -0.07684424279984919393 ) ) ;
#134944 = CARTESIAN_POINT ( 'NONE',  ( -1.500000000000001110, 11.05208333401613707, 0.8660254037844418162 ) ) ;
#134945 = CARTESIAN_POINT ( 'NONE',  ( -3.440018289565379028, 5.036440642624797626, 1.599625672291267398 ) ) ;
#134946 = CARTESIAN_POINT ( 'NONE',  ( 1.213460986420217047, 1.812193587075833667, -1.284517086575332367 ) ) ;
#134947 = CARTESIAN_POINT ( 'NONE',  ( 3.751088088702017487, -1.722778774704723181, 1.210957861328536112 ) ) ;
#134948 = CARTESIAN_POINT ( 'NONE',  ( -6.237633190739009237, 9.434933268240943249, 1.199719254218452047 ) ) ;
#134949 = CARTESIAN_POINT ( 'NONE',  ( 5.764187864104357573, 9.876636274763768597, 1.040834085586084257E-14 ) ) ;
#134950 = CARTESIAN_POINT ( 'NONE',  ( 1.082201983675265655, 1.112762242526295298, -1.491567265455741476 ) ) ;
#134951 = CARTESIAN_POINT ( 'NONE',  ( 5.961834861707224320, 7.978559976790334574, -1.599625672291262513 ) ) ;
#134952 = CARTESIAN_POINT ( 'NONE',  ( 3.974511587100456822, 7.788680618259193444, 1.040834085586084257E-14 ) ) ;
#134953 = CARTESIAN_POINT ( 'NONE',  ( -6.319508997745553636, 6.545384383557486530, 0.7216878364870257245 ) ) ;
#134954 = CARTESIAN_POINT ( 'NONE',  ( -8.405692050792730186, 9.869357483088723626, 1.082531754730558626 ) ) ;
#134955 = CARTESIAN_POINT ( 'NONE',  ( 1.160570123509139906, 2.118417766304943495, 0.09849428607798524360 ) ) ;
#134956 = CARTESIAN_POINT ( 'NONE',  ( -5.803772275101700906, 8.928762199997411386, -1.199719254218452047 ) ) ;
#134958 = CARTESIAN_POINT ( 'NONE',  ( 4.615648854252428102, 0.4318217149890530848, -1.913582009320368371 ) ) ;
#134957 = CARTESIAN_POINT ( 'NONE',  ( -1.225000000000026068, 1.020833333333308834, 0.7072540797572558491 ) ) ;
#134959 = CARTESIAN_POINT ( 'NONE',  ( 3.520547545725543515, 1.372905562624787024, -1.669742455111824286 ) ) ;
#134960 = CARTESIAN_POINT ( 'NONE',  ( 2.085277916773973228, -0.7859315772556186852, 1.665205719185464561 ) ) ;
#134961 = CARTESIAN_POINT ( 'NONE',  ( -4.167783244592077274, 7.418453011031667543, -0.7534271236282058526 ) ) ;
#134962 = CARTESIAN_POINT ( 'NONE',  ( 4.222827212797172436, 7.545785358913557950, -0.9571512059609885714 ) ) ;
#134963 = CARTESIAN_POINT ( 'NONE',  ( 5.191228607790203675, -0.6215644750859107281, 1.625735776773645780 ) ) ;
#134964 = CARTESIAN_POINT ( 'NONE',  ( 4.558697364098442506, 8.332581001507888274, -0.6286255394594755241 ) ) ;
#134965 = CARTESIAN_POINT ( 'NONE',  ( 5.504247177468186258, 6.484338464210099851, 1.082531754730558626 ) ) ;
#134966 = CARTESIAN_POINT ( 'NONE',  ( -10.61989522411177944, 7.619981102720494448, -4.513857952992439415 ) ) ;
#134967 = CARTESIAN_POINT ( 'NONE',  ( 1.587033755777764510, -0.3173376132806354222, -2.138153673666403964 ) ) ;
#134968 = CIRCLE ( 'NONE', #79591, 11.00000000000000000 ) ;
#134969 = CARTESIAN_POINT ( 'NONE',  ( 3.444685325028495004, 1.276847194542466646, 1.560261755768836744 ) ) ;
#134970 = CARTESIAN_POINT ( 'NONE',  ( -9.232739420781982176, 12.75498451001223010, 1.082531754730558626 ) ) ;
#134971 = CARTESIAN_POINT ( 'NONE',  ( 1.534274790466340299, 1.065227450066742687, -1.880959520452238465 ) ) ;
#134972 = CARTESIAN_POINT ( 'NONE',  ( 3.116049734078304212, -0.9705229388551097625, -1.715950581178276479 ) ) ;
#134973 = CARTESIAN_POINT ( 'NONE',  ( 6.609000000000012420, 4.697979799133416456, 2.462673521647487540 ) ) ;
#134974 = CARTESIAN_POINT ( 'NONE',  ( 3.755361975916061024, 1.927010760186953497, -0.2409419434407939486 ) ) ;
#134977 = ORIENTED_EDGE ( 'NONE', *, *, #157268, .F. ) ;
#134976 = CARTESIAN_POINT ( 'NONE',  ( -3.933273961740340496, 5.682181936820735579, 1.443375672974065660 ) ) ;
#134975 = CARTESIAN_POINT ( 'NONE',  ( -9.991996023147281747, 11.72004545083573568, 1.082531754730558626 ) ) ;
#134978 = CARTESIAN_POINT ( 'NONE',  ( -4.245111494410291897, 7.006361605903701495, 1.082531754730549967 ) ) ;
#134979 = CARTESIAN_POINT ( 'NONE',  ( 5.910428620914669473, 5.860197910680708944, 0.000000000000000000 ) ) ;
#134980 = CARTESIAN_POINT ( 'NONE',  ( -3.955946960137363799, 7.837298230127379917, 0.7998128361456352531 ) ) ;
#134981 = CARTESIAN_POINT ( 'NONE',  ( -5.468734858265826837, 7.473552982767158070, 1.599625672291263179 ) ) ;
#134982 = CARTESIAN_POINT ( 'NONE',  ( -9.951321562306267410, 10.71222269888655987, 1.040834085586084257E-14 ) ) ;
#134983 = CARTESIAN_POINT ( 'NONE',  ( 6.686558038528344738, -2.261219263861591333, -0.4595595737692282912 ) ) ;
#134985 = EDGE_CURVE ( 'NONE', #34393, #183422, #87314, .T. ) ;
#134984 = CARTESIAN_POINT ( 'NONE',  ( -1.642778471874998480, -3.201041666188710000, 2.845375778867863303 ) ) ;
#134986 = CARTESIAN_POINT ( 'NONE',  ( 4.258614474744500278, -0.6113484564182982695, -1.864166799412938502 ) ) ;
#134987 = CARTESIAN_POINT ( 'NONE',  ( 8.294891053462476904, 8.571794405328034827, 1.040834085586084257E-14 ) ) ;
#134988 = CARTESIAN_POINT ( 'NONE',  ( 2.145157927413956944, 0.8647252629472859109, 1.821741647932619390 ) ) ;
#134989 = VERTEX_POINT ( 'NONE', #41362 ) ;
#134990 = CARTESIAN_POINT ( 'NONE',  ( 3.204427616716760685, 1.339657272674670718, -1.639694800048612899 ) ) ;
#134991 = CARTESIAN_POINT ( 'NONE',  ( -1.500000000000013101, 1.702083334016151417, 0.8660254037844403729 ) ) ;
#134993 = CARTESIAN_POINT ( 'NONE',  ( -4.367698041896780126, 8.247398148854895084, 0.7998128361456481317 ) ) ;
#134992 = CARTESIAN_POINT ( 'NONE',  ( 0.07459516483345349225, 1.413926688351078154, -2.016100038618890089 ) ) ;
#134994 = CARTESIAN_POINT ( 'NONE',  ( 3.415785861374909249, 1.167101634185686576, -1.423959568491977912 ) ) ;
#134995 = ORIENTED_EDGE ( 'NONE', *, *, #13865, .T. ) ;
#134996 = CARTESIAN_POINT ( 'NONE',  ( -9.806625181386236179, 10.33548422123910449, -0.7998128361456291469 ) ) ;
#134997 = DIRECTION ( 'NONE',  ( 1.000000000000000000, -0.000000000000000000, -0.000000000000000000 ) ) ;
#134998 = CARTESIAN_POINT ( 'NONE',  ( 5.168275554957600271, 2.118074532352266282, -0.1063875075708180934 ) ) ;
#134999 = CARTESIAN_POINT ( 'NONE',  ( 7.233438648090761980, 8.397765496649418182, 1.199719254218462483 ) ) ;
#135000 = CARTESIAN_POINT ( 'NONE',  ( 5.448532837019475217, 0.5942636223626071024, 1.973259177745954718 ) ) ;
#135002 = CARTESIAN_POINT ( 'NONE',  ( 2.964219115174483665, -1.702287218311925310, -0.7022057971969236645 ) ) ;
#135001 = CARTESIAN_POINT ( 'NONE',  ( 0.4142149233586078227, 0.7067589711089922178, 1.721844540100337717 ) ) ;
#135003 = CARTESIAN_POINT ( 'NONE',  ( 7.425061681778431399, 11.81432239538354345, 0.7998128361456462443 ) ) ;
#135004 = CARTESIAN_POINT ( 'NONE',  ( 6.115103934187892776, 6.015625209457229339, 1.345820777640227805E-10 ) ) ;
#135005 = CARTESIAN_POINT ( 'NONE',  ( -11.86686399458719343, 9.990712702246623778, 1.056461745586970480 ) ) ;
#135006 = CYLINDRICAL_SURFACE ( 'NONE', #63191, 0.09999999999999990841 ) ;
#135007 = CARTESIAN_POINT ( 'NONE',  ( 2.139570144280181108, -1.970530345926827742, 0.9937953903183869286 ) ) ;
#135008 = CARTESIAN_POINT ( 'NONE',  ( 5.202513629402051976, -0.7552652112401860851, -2.132769717564055867 ) ) ;
#135009 = CARTESIAN_POINT ( 'NONE',  ( -6.060131475628484310, 10.01397778830115470, 0.000000000000000000 ) ) ;
#135010 = CARTESIAN_POINT ( 'NONE',  ( 4.570457401048643398, 0.6997940171077315918, 1.671178544893426654 ) ) ;
#135011 = CARTESIAN_POINT ( 'NONE',  ( 4.241352010100610137, 0.4139369872660918492, -1.870304626840668893 ) ) ;
#135012 = CARTESIAN_POINT ( 'NONE',  ( 1.364683531249988535, 3.717708333674750953, -0.7879004041258239610 ) ) ;
#135013 = MECHANICAL_DESIGN_GEOMETRIC_PRESENTATION_REPRESENTATION (  '', ( #180002 ), #183379 ) ;
#135014 = CARTESIAN_POINT ( 'NONE',  ( 3.450034532000289200, 1.971640592831106709, 0.001386944525654659321 ) ) ;
#135015 = CARTESIAN_POINT ( 'NONE',  ( 4.698043743269282757, -1.870269067358639958, -0.04562963166049315705 ) ) ;
#135016 = CARTESIAN_POINT ( 'NONE',  ( 5.125394178454842020, 0.1826033194989445385, -1.852086804783218188 ) ) ;
#135017 = CARTESIAN_POINT ( 'NONE',  ( 0.09916492693096318201, -10.00000000000016342, 9.499482423651661733 ) ) ;
#135018 = CARTESIAN_POINT ( 'NONE',  ( 0.3742329010679063539, -2.001858617179689492, -0.2420261300371470137 ) ) ;
#135020 = CARTESIAN_POINT ( 'NONE',  ( 1.664816323125760889, -1.488367931135538891, 1.490329786196037398 ) ) ;
#135019 = CARTESIAN_POINT ( 'NONE',  ( -3.050221372950322252, 5.542046787541873520, 1.082531754730560403 ) ) ;
#135021 = CARTESIAN_POINT ( 'NONE',  ( 10.55910270694468345, 11.21337466772398095, 0.7998128361456462443 ) ) ;
#135023 = CARTESIAN_POINT ( 'NONE',  ( -8.631737353394710155, 13.22211067893587533, 1.040834085586084257E-14 ) ) ;
#135022 = CARTESIAN_POINT ( 'NONE',  ( -1.364683531249997417, 5.571875000341417916, 1.214306433183764966E-14 ) ) ;
#135024 = CARTESIAN_POINT ( 'NONE',  ( 3.586284538990120119, 1.181046903802231984, 1.761068336431830472 ) ) ;
#135025 = CARTESIAN_POINT ( 'NONE',  ( 2.992204144738932481, 6.423898490107104564, -0.5069251535329973857 ) ) ;
#135027 = EDGE_CURVE ( 'NONE', #183550, #148587, #107472, .T. ) ;
#135026 = CARTESIAN_POINT ( 'NONE',  ( 1.863541707127059688, -1.624685865379692506, -1.199789887509305597 ) ) ;
#135028 = CARTESIAN_POINT ( 'NONE',  ( -1.201851678989727383E-14, 1.821875000341421691, 1.575800808251672791 ) ) ;
#135029 = CARTESIAN_POINT ( 'NONE',  ( -4.609409038966253647, 4.479991421656468908, -0.7216878364870207285 ) ) ;
#135030 = CARTESIAN_POINT ( 'NONE',  ( 5.359550796103802028, 5.147230771742885125, -0.7998128361456231517 ) ) ;
#135031 = ORIENTED_EDGE ( 'NONE', *, *, #54130, .T. ) ;
#135032 = CARTESIAN_POINT ( 'NONE',  ( 2.653791512158054200, 0.5793167894731532375, -2.082426382048585101 ) ) ;
#135033 = CARTESIAN_POINT ( 'NONE',  ( 6.890000000000010338, 4.693995042360769254, 2.562605081426703180 ) ) ;
#135036 = CARTESIAN_POINT ( 'NONE',  ( 2.684151225825664788, 5.114964949229812596, -1.082531754730543083 ) ) ;
#135035 = CARTESIAN_POINT ( 'NONE',  ( -3.039951802757221877, 2.724153688964683351, -2.451370731312840778 ) ) ;
#135034 = CARTESIAN_POINT ( 'NONE',  ( 5.248941747146098180, 6.152795455539095570, -1.199719254218452047 ) ) ;
#135037 = DIRECTION ( 'NONE',  ( 0.9754920898435691656, -0.1320207019938371973, -0.1760276026584480513 ) ) ;
#135038 = CARTESIAN_POINT ( 'NONE',  ( -7.796438949605438040, -6.657020681836948839, 7.586009164902152158 ) ) ;
#135039 = CARTESIAN_POINT ( 'NONE',  ( -6.385527162356466668, 10.39360608948380182, 0.000000000000000000 ) ) ;
#135040 = EDGE_CURVE ( 'NONE', #213592, #85656, #147380, .T. ) ;
#135041 = CARTESIAN_POINT ( 'NONE',  ( 0.7322823680011962821, 2.160084099745246178, 0.3691886501416344335 ) ) ;
#135042 = DIRECTION ( 'NONE',  ( 0.000000000000000000, -1.000000000000000000, 0.000000000000000000 ) ) ;
#135044 = CARTESIAN_POINT ( 'NONE',  ( -8.012344526598182026E-15, 11.79687500034140157, -1.575800808251669460 ) ) ;
#135043 = CARTESIAN_POINT ( 'NONE',  ( 1.569569324160888124, 0.1651462269399027738, -2.256556122256009100 ) ) ;
#135045 = CARTESIAN_POINT ( 'NONE',  ( -7.472515219426274946, 11.86968485597268064, 0.000000000000000000 ) ) ;
#135046 = CARTESIAN_POINT ( 'NONE',  ( -5.870317324592829067, 5.951051088220814300, -0.7216878364870197293 ) ) ;
#135047 = CARTESIAN_POINT ( 'NONE',  ( 0.6823417656249882723, 2.488541667008084435, -1.181850606188749264 ) ) ;
#135048 = CARTESIAN_POINT ( 'NONE',  ( 4.595929827128614420, 8.372548788374160722, -0.07784623617661419470 ) ) ;
#135049 = CARTESIAN_POINT ( 'NONE',  ( -6.009258394948636914E-15, 10.18750000000000000, -1.732050807568875195 ) ) ;
#135050 = CARTESIAN_POINT ( 'NONE',  ( 4.002375702155434922, -0.5437682074083802775, -1.636994321040524447 ) ) ;
#135051 = CARTESIAN_POINT ( 'NONE',  ( 3.878514461961128479, 6.682628084666728085, -1.199719254218448494 ) ) ;
#135052 = CARTESIAN_POINT ( 'NONE',  ( 1.528175773270981308, 1.703719318302211683, 0.4785495757857262666 ) ) ;
#135054 = CARTESIAN_POINT ( 'NONE',  ( 2.930340344496225935, -0.9942814366015439997, -1.750357268347104256 ) ) ;
#135053 = CIRCLE ( 'NONE', #65727, 12.00000000000000178 ) ;
#135055 = CARTESIAN_POINT ( 'NONE',  ( 9.236128959407556849, 11.79856975744075598, -1.599625672291262513 ) ) ;
#135056 = CARTESIAN_POINT ( 'NONE',  ( 5.297975422827020608, -0.7987165953184969247, 2.057335881587420534 ) ) ;
#135057 = VERTEX_POINT ( 'NONE', #99678 ) ;
#135058 = CARTESIAN_POINT ( 'NONE',  ( 4.060810560252373413, 0.5428485958907465214, 1.945370397410832730 ) ) ;
#135059 = CARTESIAN_POINT ( 'NONE',  ( -5.261446130555064826, 8.296048364692991228, 1.199719254218452935 ) ) ;
#135060 = CARTESIAN_POINT ( 'NONE',  ( 4.095327490859664188, -0.3419149367107060522, 1.987051255384481463 ) ) ;
#135061 = ORIENTED_EDGE ( 'NONE', *, *, #130401, .F. ) ;
#135062 = CARTESIAN_POINT ( 'NONE',  ( 3.063207453921251489, 0.2760179531714930246, -1.850060308400132358 ) ) ;
#135063 = ADVANCED_FACE ( 'NONE', ( #15212 ), #156438, .F. ) ;
#135064 = CARTESIAN_POINT ( 'NONE',  ( -10.42871741020803000, 1.405922845961221412, 5.936700867306084817 ) ) ;
#135065 = CARTESIAN_POINT ( 'NONE',  ( 1.529408426332915960, -0.2309274165002393187, 1.898302859121250297 ) ) ;
#135066 = DIRECTION ( 'NONE',  ( 3.491481338843133355E-15, 0.000000000000000000, 1.000000000000000000 ) ) ;
#135067 = CARTESIAN_POINT ( 'NONE',  ( -10.40063108925089885, 3.507138841238251370, -5.415724211249433040 ) ) ;
#135068 = CARTESIAN_POINT ( 'NONE',  ( 0.4370932794886464023, -5.427673425445469491, 10.76345817711984409 ) ) ;
#135069 = CARTESIAN_POINT ( 'NONE',  ( -1.364683531250012516, 3.342708333674756727, 0.7879004041258379498 ) ) ;
#135070 = CARTESIAN_POINT ( 'NONE',  ( -0.1757481403069499348, -0.8193859263425256056, -1.726394157293545062 ) ) ;
#135071 = CARTESIAN_POINT ( 'NONE',  ( 7.024532985656141371, 7.367912369453226695, 0.7216878364870328300 ) ) ;
#135072 = CARTESIAN_POINT ( 'NONE',  ( 1.715213470010600538, -1.680963409367957295, -1.011360081469035999 ) ) ;
#135073 = CARTESIAN_POINT ( 'NONE',  ( -5.786256696412555911, 6.075953140482280190, 0.5845640519336701146 ) ) ;
#135074 = CARTESIAN_POINT ( 'NONE',  ( -7.110325215724114578, 7.260077271291732082, 0.000000000000000000 ) ) ;
#135075 = CARTESIAN_POINT ( 'NONE',  ( 5.220985865760717992, 1.604251394084664550, -1.386888226476624242 ) ) ;
#135077 = CARTESIAN_POINT ( 'NONE',  ( -11.52570357830391323, 8.091488070261075194, -2.173620758456770830 ) ) ;
#135076 = CARTESIAN_POINT ( 'NONE',  ( 10.26082332744404368, 10.86538205830655279, -0.7998128361456281477 ) ) ;
#135078 = CARTESIAN_POINT ( 'NONE',  ( 5.923112194766430250, -0.05102361969991364710, 1.970867320657720301 ) ) ;
#135079 = CARTESIAN_POINT ( 'NONE',  ( -1.201851678989727383E-14, 2.946875000341419248, -1.575800808251660134 ) ) ;
#135080 = CARTESIAN_POINT ( 'NONE',  ( 1.002198536899261860, -0.9015652438304004868, 1.800089726458251826 ) ) ;
#135081 = ORIENTED_EDGE ( 'NONE', *, *, #50358, .T. ) ;
#135082 = CARTESIAN_POINT ( 'NONE',  ( 1.195080948601736859, 1.869106744463861158, 0.9945057017613133654 ) ) ;
#135083 = CARTESIAN_POINT ( 'NONE',  ( 11.95102697937679359, 6.645246171022539450, 0.4972084260056497951 ) ) ;
#135084 = CARTESIAN_POINT ( 'NONE',  ( 2.928250347896840022, 1.105370970781336837, 1.750397071514836478 ) ) ;
#135085 = CARTESIAN_POINT ( 'NONE',  ( 5.388439706788500594, 5.251210844200210559, 0.7998128361456352531 ) ) ;
#135086 = CARTESIAN_POINT ( 'NONE',  ( 6.008198349511364000, 7.038594824965278995, 1.199719254218453823 ) ) ;
#135087 = ORIENTED_EDGE ( 'NONE', *, *, #30633, .F. ) ;
#135089 = CARTESIAN_POINT ( 'NONE',  ( 3.194917754314666514, 6.879154480009089134, 0.7998128361456321445 ) ) ;
#135088 = CARTESIAN_POINT ( 'NONE',  ( 4.488279598995706721, -0.4578276946864130448, -2.039718000080573912 ) ) ;
#135092 = ORIENTED_EDGE ( 'NONE', *, *, #73625, .F. ) ;
#135091 = CARTESIAN_POINT ( 'NONE',  ( 1.365539917532717196, 0.5261944252722695614, -1.733370571883424693 ) ) ;
#135090 = CARTESIAN_POINT ( 'NONE',  ( 2.713660727937649231, -1.805999004224107418, 0.2657717501357085843 ) ) ;
#135093 = CARTESIAN_POINT ( 'NONE',  ( 9.481348452320371933, -9.006862915010128035, -0.5950054837411746789 ) ) ;
#135094 = DIRECTION ( 'NONE',  ( 0.000000000000000000, 0.000000000000000000, -1.000000000000000000 ) ) ;
#135095 = CARTESIAN_POINT ( 'NONE',  ( 9.280150959925951071, 13.43437406861168704, 6.783356236849154008 ) ) ;
#135096 = CARTESIAN_POINT ( 'NONE',  ( 5.649526978565787338, -1.736373965863503122, -1.361823127433124725 ) ) ;
#135097 = CARTESIAN_POINT ( 'NONE',  ( -1.364683531250000748, 9.421875000341396245, 0.000000000000000000 ) ) ;
#135098 = VERTEX_POINT ( 'NONE', #145279 ) ;
#135099 = CARTESIAN_POINT ( 'NONE',  ( 4.107995242876061326, -0.7289348763114507079, 1.768098669557085056 ) ) ;
#135100 = CARTESIAN_POINT ( 'NONE',  ( -2.950870989268691957, 6.594433254122103349, -0.7998128361456281477 ) ) ;
#135101 = CARTESIAN_POINT ( 'NONE',  ( 8.633844893804129228, 8.967240552393299424, -0.7998128361456211532 ) ) ;
#135102 = CARTESIAN_POINT ( 'NONE',  ( 6.144996677366851401, -0.2998803957653916052, -2.048400609436632269 ) ) ;
#135103 = CARTESIAN_POINT ( 'NONE',  ( -1.360316468750018659, 0.6927083336747492659, 0.7853790794158961308 ) ) ;
#135104 = CARTESIAN_POINT ( 'NONE',  ( 3.945059511452237100, 6.586024615794168646, -1.082531754730548412 ) ) ;
#135105 = DIRECTION ( 'NONE',  ( 0.000000000000000000, 1.000000000000000000, 0.000000000000000000 ) ) ;
#135106 = CARTESIAN_POINT ( 'NONE',  ( 8.361471489411563596, 14.02767860296625813, -8.607966671085261368 ) ) ;
#135107 = CARTESIAN_POINT ( 'NONE',  ( 3.147653791585776517, 8.920000000000001705, 2.419999999999890239 ) ) ;
#135108 = VERTEX_POINT ( 'NONE', #177744 ) ;
#135109 = DIRECTION ( 'NONE',  ( 0.000000000000000000, 0.000000000000000000, 1.000000000000000000 ) ) ;
#135110 = CARTESIAN_POINT ( 'NONE',  ( 3.251090012001829788, -1.527204365403836306, -1.079795099579644591 ) ) ;
#135111 = DIRECTION ( 'NONE',  ( -1.000000000000000000, 1.561251128379122346E-12, 0.000000000000000000 ) ) ;
#135112 = CARTESIAN_POINT ( 'NONE',  ( 6.224601922449876312, 6.434659462379210382, 0.000000000000000000 ) ) ;
#135113 = CARTESIAN_POINT ( 'NONE',  ( -6.805829924380121909, 8.963220883242035697, 1.443375672974078761 ) ) ;
#135114 = CARTESIAN_POINT ( 'NONE',  ( 2.911969131885072670, 6.619324097166378706, 0.000000000000000000 ) ) ;
#135115 = CARTESIAN_POINT ( 'NONE',  ( 4.416205349749311004, 6.175325546172740765, 1.599625672291267398 ) ) ;
#135116 = CARTESIAN_POINT ( 'NONE',  ( 6.825056245572477032, -1.890314563506745316, -0.8446596084958692963 ) ) ;
#135117 = CARTESIAN_POINT ( 'NONE',  ( 1.036732716359071604, -1.587823911754655315, 1.242746109592095527 ) ) ;
#135118 = CARTESIAN_POINT ( 'NONE',  ( -7.648771216403934758, 12.07531685244661723, -0.7998128361456291469 ) ) ;
#135119 = CARTESIAN_POINT ( 'NONE',  ( 6.475954649182838807, 7.584310507915338562, 1.199719254218452047 ) ) ;
#135120 = DIRECTION ( 'NONE',  ( 0.000000000000000000, 0.000000000000000000, -1.000000000000000000 ) ) ;
#135121 = CARTESIAN_POINT ( 'NONE',  ( 0.9377431681640016059, 0.8850447378907433382, -2.004962588275795543 ) ) ;
#135122 = CARTESIAN_POINT ( 'NONE',  ( 6.287720257080702702, 1.262826302610157381, 1.318732360701305062 ) ) ;
#135123 = CARTESIAN_POINT ( 'NONE',  ( -3.297657676621885692, 4.870353260857385180, 1.599625672291267398 ) ) ;
#135124 = CARTESIAN_POINT ( 'NONE',  ( 4.095971805104276164, 7.792734516014745871, 0.7216878364870257245 ) ) ;
#135125 = CARTESIAN_POINT ( 'NONE',  ( 10.07387183015377197, 11.71160420905630062, -1.199719254218440723 ) ) ;
#135126 = CARTESIAN_POINT ( 'NONE',  ( 3.029357257649615054, 5.621668336311468117, -1.199719254218446718 ) ) ;
#135127 = CARTESIAN_POINT ( 'NONE',  ( 5.090160327287878594, 4.903218234782778850, -0.7998128361456481317 ) ) ;
#135128 = ORIENTED_EDGE ( 'NONE', *, *, #18222, .T. ) ;
#135130 = CARTESIAN_POINT ( 'NONE',  ( 0.1178376421791422907, -0.5346926475991298222, 1.940734443874014836 ) ) ;
#135129 = CARTESIAN_POINT ( 'NONE',  ( 4.247483403459266782, 1.840758003770435414, -0.04960325993209198370 ) ) ;
#135131 = CARTESIAN_POINT ( 'NONE',  ( 2.355183240404590705, -0.9839461204387394133, 2.077256468512170162 ) ) ;
#135133 = CARTESIAN_POINT ( 'NONE',  ( 0.6372766190945264864, 1.739209566756502845, -0.6625725129940361890 ) ) ;
#135132 = CARTESIAN_POINT ( 'NONE',  ( 3.050221373394638835, 6.502416002361635528, 0.000000000000000000 ) ) ;
#135134 = CARTESIAN_POINT ( 'NONE',  ( -3.475000000000000533, -0.3791666666666649865, -2.006292185433948827 ) ) ;
#135135 = CARTESIAN_POINT ( 'NONE',  ( -5.440899717785814715, 5.242137847038546461, 0.7998128361456341429 ) ) ;
#135136 = DIRECTION ( 'NONE',  ( -5.551115123125782702E-17, 0.000000000000000000, 1.000000000000000000 ) ) ;
#135137 = CARTESIAN_POINT ( 'NONE',  ( 4.289254230599209627, -0.005406649120142519548, -1.912571728590661380 ) ) ;
#135138 = CARTESIAN_POINT ( 'NONE',  ( -8.448702279610222021, 13.00856975952063088, 1.040834085586084257E-14 ) ) ;
#135139 = CARTESIAN_POINT ( 'NONE',  ( 6.474762296362193581, 6.758873339713582062, -0.2294044474360455721 ) ) ;
#135140 = CARTESIAN_POINT ( 'NONE',  ( -7.132998214565509087, 7.494455136514109661, 0.7216878364870317197 ) ) ;
#135142 = CARTESIAN_POINT ( 'NONE',  ( 1.779943879855113709, -1.003247456797161652, 1.578688272967261996 ) ) ;
#135141 = CARTESIAN_POINT ( 'NONE',  ( 3.368770691598612643, 0.04892471221396628434, -2.090337739860036681 ) ) ;
#135143 = CARTESIAN_POINT ( 'NONE',  ( 7.700668062882064291, 10.00719871149432549, -1.443375672974057666 ) ) ;
#135144 = CARTESIAN_POINT ( 'NONE',  ( -1.201851678989727383E-14, 5.259375000341422357, -1.575800808251660134 ) ) ;
#135145 = CARTESIAN_POINT ( 'NONE',  ( 3.667295640872432649, 0.9703414817801876424, 1.444613691174992720 ) ) ;
#135146 = CARTESIAN_POINT ( 'NONE',  ( 5.508690485854129903, 5.321227076451600091, 1.040834085586084257E-14 ) ) ;
#135148 = CARTESIAN_POINT ( 'NONE',  ( 5.867981556616276073, 5.740399992340775803, -0.7998128361456281477 ) ) ;
#135147 = CARTESIAN_POINT ( 'NONE',  ( 0.3999999999999923617, 0.6284510210556870646, 1.086836331270357281 ) ) ;
#135149 = CARTESIAN_POINT ( 'NONE',  ( 3.791373243616827704, 1.250846937323921715, 1.187934608979845708 ) ) ;
#135150 = CARTESIAN_POINT ( 'NONE',  ( -8.050844288416501016, 8.287073179441051707, 1.040834085586084257E-14 ) ) ;
#135151 = CARTESIAN_POINT ( 'NONE',  ( 3.544632465004614374, -1.790652189326558563, 1.263247045326252094 ) ) ;
#135152 = CARTESIAN_POINT ( 'NONE',  ( 6.217417563691929772, -0.2743312036321900460, 2.189694890431858276 ) ) ;
#135153 = DIRECTION ( 'NONE',  ( 0.1674078377060222722, 0.000000000000000000, 0.9858877298529452604 ) ) ;
#135154 = CARTESIAN_POINT ( 'NONE',  ( 4.030270078087188068, 1.201442806954319487, 1.808153907555063000 ) ) ;
#135155 = CARTESIAN_POINT ( 'NONE',  ( 1.892912435568369744, 1.589020553905008626, -0.8988452475950716725 ) ) ;
#135156 = CARTESIAN_POINT ( 'NONE',  ( 4.927025384238821637, -1.814351377589568548, 1.091279385997992568 ) ) ;
#135157 = ORIENTED_EDGE ( 'NONE', *, *, #125035, .F. ) ;
#135159 = CARTESIAN_POINT ( 'NONE',  ( -1.364683531250012516, 2.592708333674753174, 0.7879004041258379498 ) ) ;
#135158 = CARTESIAN_POINT ( 'NONE',  ( 5.003627799853592073, -2.281530862488420297, 0.2229171871234881530 ) ) ;
#135160 = CARTESIAN_POINT ( 'NONE',  ( 6.720655732516649827, 2.453385726714229609, 2.309856631140958960 ) ) ;
#135161 = CARTESIAN_POINT ( 'NONE',  ( 3.297657676621871925, 4.870353260857385180, 1.599625672291267398 ) ) ;
#135163 = EDGE_CURVE ( 'NONE', #18033, #195316, #214114, .T. ) ;
#135162 = CIRCLE ( 'NONE', #10651, 0.2000000000000005107 ) ;
#135164 = CARTESIAN_POINT ( 'NONE',  ( 1.102369588802411426, -0.9501182663193027400, 1.895776817140030213 ) ) ;
#135165 = PRODUCT_DEFINITION ( 'UNKNOWN', '', #83370, #33075 ) ;
#135166 = CARTESIAN_POINT ( 'NONE',  ( -4.609409038966234995, 7.361099064560491456, -1.082531754730549967 ) ) ;
#135167 = CARTESIAN_POINT ( 'NONE',  ( 3.714570900464285064, 4.396382807705524698, 1.082531754730560403 ) ) ;
#135168 = B_SPLINE_CURVE_WITH_KNOTS ( 'NONE', 3,
 ( #106821, #125238, #140369, #191197, #42863, #108971, #4954, #71032, #113243, #30871 ),
 .UNSPECIFIED., .F., .F.,
 ( 4, 2, 2, 2, 4 ),
 ( 7.684844577824277550E-18, 0.0002021113321160356176, 0.0004042226642320635374, 0.0006063339963480915114, 0.0008084453284641193770 ),
 .UNSPECIFIED. ) ;
#135169 = CARTESIAN_POINT ( 'NONE',  ( -6.195713011320807873, 6.330679389403470303, -0.7216878364870267237 ) ) ;
#135171 = CARTESIAN_POINT ( 'NONE',  ( 1.499999999999993117, 13.13541666734946745, 0.8660254037844409281 ) ) ;
#135170 = CARTESIAN_POINT ( 'NONE',  ( 6.883263157960364254, 2.038911835798001171, 2.358809022084580764 ) ) ;
#135172 = ORIENTED_EDGE ( 'NONE', *, *, #147855, .F. ) ;
#135173 = CARTESIAN_POINT ( 'NONE',  ( 6.188124994278807023, 1.678003296889327034, 1.117835524071027598 ) ) ;
#135175 = CARTESIAN_POINT ( 'NONE',  ( 4.873915701820059176, -2.023805994998853830, 0.3972042427494940076 ) ) ;
#135174 = CARTESIAN_POINT ( 'NONE',  ( 3.662674053986138656, 7.424870162959149589, 0.7998128361456321445 ) ) ;
#135177 = CARTESIAN_POINT ( 'NONE',  ( -4.787437638956927977, 7.639075441208117212, -1.082531754730549967 ) ) ;
#135176 = CARTESIAN_POINT ( 'NONE',  ( 6.879836604291781121, 6.991173891287354003, -0.7998128361456341429 ) ) ;
#135178 = CARTESIAN_POINT ( 'NONE',  ( 6.230854113932139171, 9.427024345299638952, 1.199719254218452047 ) ) ;
#135179 = CARTESIAN_POINT ( 'NONE',  ( -3.285556943749998737, -0.4302083328553760744, 1.896917185911908499 ) ) ;
#135180 = CARTESIAN_POINT ( 'NONE',  ( 1.150196859685079342, 2.935958678954801115, 0.7750000000000065725 ) ) ;
#135181 = CARTESIAN_POINT ( 'NONE',  ( 0.3926704732973253509, 1.736993494895492152, -1.163127744158433119 ) ) ;
#135182 = CARTESIAN_POINT ( 'NONE',  ( 4.570935502227962743, -0.9480417383296577682, 1.779625852769652905 ) ) ;
#135183 = CARTESIAN_POINT ( 'NONE',  ( 4.704558828624370470, 1.604442792107749760, 0.9031527321438773681 ) ) ;
#135184 = CARTESIAN_POINT ( 'NONE',  ( 6.144869935491714230, 8.192100896205568361, -1.599625672291262513 ) ) ;
#135185 = ADVANCED_FACE ( 'NONE', ( #133279 ), #198226, .F. ) ;
#135186 = CARTESIAN_POINT ( 'NONE',  ( 0.2875850076352819973, -0.8198804995633873771, 1.517450437728053325 ) ) ;
#135187 = CARTESIAN_POINT ( 'NONE',  ( 0.2863426850727782136, -0.6839425765656822476, -1.897108587135355684 ) ) ;
#135188 = CARTESIAN_POINT ( 'NONE',  ( 0.9679111143040418641, -2.244285626452859450, -0.4966636800145701747 ) ) ;
#135189 = CARTESIAN_POINT ( 'NONE',  ( -6.087774667736030487, 7.061157519568837415, 1.199719254218450271 ) ) ;
#135190 = CARTESIAN_POINT ( 'NONE',  ( 0.8962371694669484246, -0.8134219682564158838, 2.111273946446708738 ) ) ;
#135191 = CARTESIAN_POINT ( 'NONE',  ( 3.158910222468692908, -1.594458197781272846, 1.376041720736504992 ) ) ;
#135192 = CARTESIAN_POINT ( 'NONE',  ( -4.447956913735107598, 7.346977611736363656, 1.199719254218452935 ) ) ;
#135193 = CARTESIAN_POINT ( 'NONE',  ( 6.103141704446003679, 10.27208242182903142, 0.7998128361456462443 ) ) ;
#135194 = CARTESIAN_POINT ( 'NONE',  ( 7.309254211098767051, 7.700087132469628948, 0.7216878364870267237 ) ) ;
#135195 = FILL_AREA_STYLE ('',( #69075 ) ) ;
#135196 = CARTESIAN_POINT ( 'NONE',  ( -4.900382456335551140, 7.804531068111707270, 1.199719254218464037 ) ) ;
#135197 = CARTESIAN_POINT ( 'NONE',  ( 6.277061933002777927, 8.346324893301817482, 1.443375672974076540 ) ) ;
#135198 = CARTESIAN_POINT ( 'NONE',  ( 4.526804827544169463, 7.221866427374837194, 1.292974732014543271 ) ) ;
#135199 = CARTESIAN_POINT ( 'NONE',  ( -4.973143418114339021, 4.696422164088486895, 0.7998128361456341429 ) ) ;
#135200 = CARTESIAN_POINT ( 'NONE',  ( 4.764059104694277735, 0.6956466834483631123, -2.109775416031458128 ) ) ;
#135201 = CARTESIAN_POINT ( 'NONE',  ( 1.957222284144799929, 0.3726435881295562247, -2.159377063894574622 ) ) ;
#135202 = CARTESIAN_POINT ( 'NONE',  ( -4.062639585589296942, 7.891496616496157301, 0.7998128361456341429 ) ) ;
#135203 = CARTESIAN_POINT ( 'NONE',  ( -11.96209379583854293, 9.772070594057634452, 0.9572398070798600056 ) ) ;
#135204 = CARTESIAN_POINT ( 'NONE',  ( 5.055110333045015558, 1.632132345252810035, -1.088295032039228172 ) ) ;
#135205 =( GEOMETRIC_REPRESENTATION_CONTEXT ( 3 ) GLOBAL_UNCERTAINTY_ASSIGNED_CONTEXT ( ( #150032 ) ) GLOBAL_UNIT_ASSIGNED_CONTEXT ( ( #177834, #195145, #43580 ) ) REPRESENTATION_CONTEXT ( 'NONE', 'WORKASPACE' ) );
#135206 = CARTESIAN_POINT ( 'NONE',  ( -0.6823417656250003738, 1.467708333674752730, -1.181850606188749264 ) ) ;
#135207 = CARTESIAN_POINT ( 'NONE',  ( 6.889999999999970370, 7.053389210336755255, 2.318152334880723142 ) ) ;
#135209 = VERTEX_POINT ( 'NONE', #129078 ) ;
#135208 = CARTESIAN_POINT ( 'NONE',  ( -5.151735183512911043, 6.073074471262228435, 1.082531754730548412 ) ) ;
#135210 = CARTESIAN_POINT ( 'NONE',  ( 4.254221937059123881, 0.9039275175388861161, -1.918405034562712830 ) ) ;
#135211 = CARTESIAN_POINT ( 'NONE',  ( -7.458393901293492334, 7.874083437696761223, 0.7216878364870317197 ) ) ;
#135212 = ORIENTED_EDGE ( 'NONE', *, *, #213029, .T. ) ;
#135214 = CARTESIAN_POINT ( 'NONE',  ( -0.006158830626153827259, 7.078243236992583398, 2.121324627965421872 ) ) ;
#135213 = CARTESIAN_POINT ( 'NONE',  ( -6.794044374223859428, 7.099008989448849505, 0.000000000000000000 ) ) ;
#135215 = CARTESIAN_POINT ( 'NONE',  ( 6.169123589417988995, 7.156064594864501416, -1.199719254218445830 ) ) ;
#135216 = CARTESIAN_POINT ( 'NONE',  ( 5.020983453748395497, -1.746657797055195305, 0.5827527221545365510 ) ) ;
#135217 = UNCERTAINTY_MEASURE_WITH_UNIT (LENGTH_MEASURE( 1.000000000000000082E-05 ), #89600, 'distance_accuracy_value', 'NONE');
#135218 = VECTOR ( 'NONE', #123905, 1000.000000000000000 ) ;
#135219 = CARTESIAN_POINT ( 'NONE',  ( 1.734723475976807094E-15, -3.469446951953614189E-15, 0.2936757779752607878 ) ) ;
#135220 = CARTESIAN_POINT ( 'NONE',  ( 1.364683531249988535, 3.217708333674748289, -0.7879004041258239610 ) ) ;
#135221 = CARTESIAN_POINT ( 'NONE',  ( 0.8018505195637380956, 1.319035621562004934, -1.135522575981460003 ) ) ;
#135222 = DIRECTION ( 'NONE',  ( 0.000000000000000000, 1.000000000000000000, 0.000000000000000000 ) ) ;
#135223 = CARTESIAN_POINT ( 'NONE',  ( -1.364683531250014514, -0.9489583329919112353, -0.7879004041258359514 ) ) ;
#135224 = CARTESIAN_POINT ( 'NONE',  ( -1.225000000000044276, 1.729166666666672292, -0.7072540797572957061 ) ) ;
#135225 = CARTESIAN_POINT ( 'NONE',  ( 5.225516498768126183, -2.053876642077703707, 0.6744380372525200507 ) ) ;
#135226 = CARTESIAN_POINT ( 'NONE',  ( -2.761056838677368397, 6.372983411765559048, 0.7998128361456341429 ) ) ;
#135227 = CARTESIAN_POINT ( 'NONE',  ( -6.466876083594135238, 9.528143949959703818, 1.082531754730548412 ) ) ;
#135228 = CARTESIAN_POINT ( 'NONE',  ( 5.014612968065254250, 1.493337269798940881, -1.563205770552501761 ) ) ;
#135229 = CARTESIAN_POINT ( 'NONE',  ( -1.364683531250012516, 2.738541667008090208, -0.7879004041258289570 ) ) ;
#135230 = CARTESIAN_POINT ( 'NONE',  ( 5.395764264914824970, -0.7120431519804657494, 1.838431125455505688 ) ) ;
#135231 = CARTESIAN_POINT ( 'NONE',  ( 4.235468066436924417, -1.617573843961607416, -0.6246848730444684028 ) ) ;
#135232 = CARTESIAN_POINT ( 'NONE',  ( 1.347511689332027807, 0.6317163119916607839, -2.098556723903362009 ) ) ;
#135233 = CARTESIAN_POINT ( 'NONE',  ( 2.257223126251302947, -1.783628160338263768, 1.464130300071916135 ) ) ;
#135234 = CARTESIAN_POINT ( 'NONE',  ( 4.411438286107774331, -0.3560947707623678959, 2.029623144953551339 ) ) ;
#135235 = CARTESIAN_POINT ( 'NONE',  ( 6.356980358691139088, 0.3275572002108660952, -1.914087848568704731 ) ) ;
#135236 = CARTESIAN_POINT ( 'NONE',  ( -6.521108698048772467, 9.591415333490143524, -1.082531754730537976 ) ) ;
#135237 = CARTESIAN_POINT ( 'NONE',  ( -5.981082042284069367, 7.006959133200059142, 1.199719254218452935 ) ) ;
#135238 = PRESENTATION_STYLE_ASSIGNMENT (( #38783 ) ) ;
#135239 = CARTESIAN_POINT ( 'NONE',  ( 1.037732671793228700, -1.587836052788630603, 1.242728777923551409 ) ) ;
#135240 = CARTESIAN_POINT ( 'NONE',  ( -7.388830529323428209, 8.683019041374528513, 1.082531754730549967 ) ) ;
#135241 = CARTESIAN_POINT ( 'NONE',  ( 3.276612781706738087, -1.315965827422488132, 1.771305981150771647 ) ) ;
#135242 = CARTESIAN_POINT ( 'NONE',  ( -3.285556943750000514, -1.276041666188709511, -1.896917185911906500 ) ) ;
#135243 = CARTESIAN_POINT ( 'NONE',  ( 0.4614603993745093891, -0.5041695895235782654, 1.791261842318598863 ) ) ;
#135244 =( BOUNDED_SURFACE ( )  B_SPLINE_SURFACE ( 3, 2, ( 
 ( #201018, #138200, #6020 ),
 ( #167487, #85162, #120951 ),
 ( #7087, #105716, #204211 ),
 ( #153369, #89452, #20145 ),
 ( #155505, #19082, #88373 ),
 ( #23342, #169614, #55863 ),
 ( #38552, #186922, #22264 ),
 ( #104630, #122020, #68887 ) ),
 .UNSPECIFIED., .F., .F., .F. ) 
 B_SPLINE_SURFACE_WITH_KNOTS ( ( 4, 2, 2, 4 ),
 ( 3, 3 ),
 ( -4.065758146820641628E-19, 0.0002475938981900014865, 0.0004951877963800034067, 0.0009903755927600072471 ),
 ( 0.000000000000000000, 1.000000000000000000 ),
 .UNSPECIFIED. ) 
 GEOMETRIC_REPRESENTATION_ITEM ( )  RATIONAL_B_SPLINE_SURFACE ( (
 ( 1.000000000000000000, 0.9238795325112891810, 1.000000000000000000),
 ( 1.000000000000000000, 0.9248499699752523728, 1.000000000000000000),
 ( 1.000000000000000000, 0.9171047238584710826, 1.000000000000000000),
 ( 1.000000000000000000, 0.8907236462368126606, 1.000000000000000000),
 ( 1.000000000000000000, 0.8725411758596960388, 1.000000000000000000),
 ( 1.000000000000000000, 0.8105159241138063519, 1.000000000000000000),
 ( 1.000000000000000000, 0.7599483315144157647, 1.000000000000000000),
 ( 1.000000000000000000, 0.7045118851637699464, 1.000000000000000000) ) ) 
 REPRESENTATION_ITEM ( '' )  SURFACE ( )  );
#135245 = CARTESIAN_POINT ( 'NONE',  ( 0.9311234436981545848, -1.809380368602567346, -3.474999999999999201 ) ) ;
#135246 = DIRECTION ( 'NONE',  ( 0.000000000000000000, -1.000000000000000000, 0.000000000000000000 ) ) ;
#135247 = CARTESIAN_POINT ( 'NONE',  ( 5.351240958524983604, 4.712734197347588250, -2.500000000000000888 ) ) ;
#135249 = CARTESIAN_POINT ( 'NONE',  ( 6.825078400183511640, 3.690008145721306310, 2.558400262806997283 ) ) ;
#135248 = CARTESIAN_POINT ( 'NONE',  ( -5.880564528862151974, 7.271459349814712425, -1.272365726499018246 ) ) ;
#135250 = CARTESIAN_POINT ( 'NONE',  ( 6.316338248019476964, 1.719745045379994064, 0.6579504788090040357 ) ) ;
#135251 = VERTEX_POINT ( 'NONE', #66075 ) ;
#135252 = CARTESIAN_POINT ( 'NONE',  ( 3.116143102785688068, -1.014332071340098285, -1.793896330205650980 ) ) ;
#135253 = CARTESIAN_POINT ( 'NONE',  ( -1.360316468750062846, 1.619791667008073643, -0.7853790794159301036 ) ) ;
#135254 = CARTESIAN_POINT ( 'NONE',  ( -7.203459687562382641, 7.298457811777897319, -0.7998128361456291469 ) ) ;
#135255 = CARTESIAN_POINT ( 'NONE',  ( 1.998700280430569576, -1.981126291604264233, -0.3917822458236255301 ) ) ;
#135256 = CARTESIAN_POINT ( 'NONE',  ( 1.499999999999985123, 0.04583333333335545129, -0.8660254037844323793 ) ) ;
#135257 = CARTESIAN_POINT ( 'NONE',  ( 2.672928840188529609, 6.270167413528593414, 0.000000000000000000 ) ) ;
#135258 = CARTESIAN_POINT ( 'NONE',  ( 2.272404554480491168, -1.268947053487592846, 1.623793324639089874 ) ) ;
#135259 =( BOUNDED_SURFACE ( )  B_SPLINE_SURFACE ( 3, 2, ( 
 ( #73586, #41115, #131980 ),
 ( #13898, #79980, #146083 ),
 ( #164436, #48569, #81054 ),
 ( #115741, #95193, #212095 ),
 ( #63731, #97326, #196931 ),
 ( #163382, #178563, #45374 ),
 ( #162313, #47513, #129890 ),
 ( #49616, #197988, #112552 ) ),
 .UNSPECIFIED., .F., .F., .T. ) 
 B_SPLINE_SURFACE_WITH_KNOTS ( ( 4, 2, 2, 4 ),
 ( 3, 3 ),
 ( 0.000000000000000000, 0.003001918495469456383, 0.004502877743204184574, 0.006003836990938912765 ),
 ( 0.000000000000000000, 1.000000000000000000 ),
 .UNSPECIFIED. ) 
 GEOMETRIC_REPRESENTATION_ITEM ( )  RATIONAL_B_SPLINE_SURFACE ( (
 ( 1.000000000000000000, 0.7835651598521251593, 1.000000000000000000),
 ( 1.000000000000000000, 0.7913519369905593903, 1.000000000000000000),
 ( 1.000000000000000000, 0.8009496234844375451, 1.000000000000000000),
 ( 1.000000000000000000, 0.8230981486283348580, 1.000000000000000000),
 ( 1.000000000000000000, 0.8318333311017230836, 1.000000000000000000),
 ( 1.000000000000000000, 0.8529518727575170489, 1.000000000000000000),
 ( 1.000000000000000000, 0.8654984584225912103, 1.000000000000000000),
 ( 1.000000000000000000, 0.8789000212895414776, 1.000000000000000000) ) ) 
 REPRESENTATION_ITEM ( '' )  SURFACE ( )  );
#135261 = CARTESIAN_POINT ( 'NONE',  ( -1.364683531250014514, 13.33854166700806587, -0.7879004041258335089 ) ) ;
#135260 = DIRECTION ( 'NONE',  ( -1.276756478318932585E-15, 1.000000000000000000, -1.665334536937738262E-16 ) ) ;
#135262 = CARTESIAN_POINT ( 'NONE',  ( 4.821896187954575197, 8.777295985922343391, 0.7998128361456462443 ) ) ;
#135263 = CARTESIAN_POINT ( 'NONE',  ( 0.000000000000000000, 4.006659545634088992, 0.000000000000000000 ) ) ;
#135264 = CARTESIAN_POINT ( 'NONE',  ( 6.059228469117068805, -1.890744221452178353, -1.137928576693452820 ) ) ;
#135265 = CARTESIAN_POINT ( 'NONE',  ( 1.634274655659254005, 1.066924998833935989, -1.879885089102695250 ) ) ;
#135266 = CARTESIAN_POINT ( 'NONE',  ( -3.768803514918943609, 7.340761834139994058, 0.7216878364870317197 ) ) ;
#135267 = CARTESIAN_POINT ( 'NONE',  ( 0.4797043241997685503, -0.7212876333932433104, 1.883314553594167107 ) ) ;
#135268 = CARTESIAN_POINT ( 'NONE',  ( -0.2172799280667317978, 6.446489533111720682, 3.228652710814125193 ) ) ;
#135269 = CARTESIAN_POINT ( 'NONE',  ( 3.215772567386471437, 6.427315425527130088, -0.8732430475888955934 ) ) ;
#135270 = CIRCLE ( 'NONE', #166317, 0.5000000000000004441 ) ;
#135271 = CARTESIAN_POINT ( 'NONE',  ( 1.692057038649401601, -1.861345348035767344, -0.1864469194169729449 ) ) ;
#135272 = CARTESIAN_POINT ( 'NONE',  ( 3.925017756809038527, -1.752140073516525565, 0.9981236898717813499 ) ) ;
#135274 = CARTESIAN_POINT ( 'NONE',  ( 11.43195036480941340, 13.65524496285255829, 3.649565797774438458 ) ) ;
#135273 = CARTESIAN_POINT ( 'NONE',  ( -0.6823417656250003738, 1.467708333674752730, -1.181850606188749264 ) ) ;
#135275 = EDGE_CURVE ( 'NONE', #33711, #29614, #213247, .T. ) ;
#135277 = CARTESIAN_POINT ( 'NONE',  ( 5.215496775961459441, -0.3099510095366068696, 2.083004237123146307 ) ) ;
#135276 = CARTESIAN_POINT ( 'NONE',  ( -8.199983978166823562, 8.461069484149769337, -0.7998128361456291469 ) ) ;
#135278 = CARTESIAN_POINT ( 'NONE',  ( 5.445571254183207088, 9.504916896522420444, -0.7998128361456281477 ) ) ;
#135279 = CARTESIAN_POINT ( 'NONE',  ( -6.714312387265696458, 8.856450423275211037, 1.599625672291283607 ) ) ;
#135280 = CARTESIAN_POINT ( 'NONE',  ( 1.406470046317633615, 3.337112123497550265, 0.01120553378792966959 ) ) ;
#135281 = CARTESIAN_POINT ( 'NONE',  ( 5.484630696634174463, -1.278254659592213516, 1.563874148425943078 ) ) ;
#135282 = CARTESIAN_POINT ( 'NONE',  ( -1.500000000000015099, -0.8395833326505166561, -0.8660254037844383745 ) ) ;
#135283 = CARTESIAN_POINT ( 'NONE',  ( 0.7782751772977951621, -1.100228457372550261, -1.744432094316533677 ) ) ;
#135284 = CARTESIAN_POINT ( 'NONE',  ( 7.293923454472069245, 11.45340176361870199, 0.7216878364870438212 ) ) ;
#135285 = CARTESIAN_POINT ( 'NONE',  ( 4.844006021832467646, 8.873367135438366304, 0.000000000000000000 ) ) ;
#135286 = CARTESIAN_POINT ( 'NONE',  ( 6.235824307642648279, 6.239826211863360506, 0.000000000000000000 ) ) ;
#135287 = CARTESIAN_POINT ( 'NONE',  ( -1.402160292154681736E-14, 1.009375000341417916, -1.575800808251659024 ) ) ;
#135289 = DIRECTION ( 'NONE',  ( 0.000000000000000000, 1.000000000000000000, 0.000000000000000000 ) ) ;
#135288 = CARTESIAN_POINT ( 'NONE',  ( 4.206772801990143584, 8.129928378955675328, 0.7998128361456271485 ) ) ;
#135290 = CARTESIAN_POINT ( 'NONE',  ( 7.199016378732056687, 10.38230762762066384, -1.082531754730537976 ) ) ;
#135291 = CARTESIAN_POINT ( 'NONE',  ( 3.473242058572806990, 1.961495611989271248, 0.9311941066344242568 ) ) ;
#135293 = CARTESIAN_POINT ( 'NONE',  ( 1.346931166825489967, 0.5339940059071214273, -1.762130705996706181 ) ) ;
#135292 = CARTESIAN_POINT ( 'NONE',  ( -3.294268138440636928, 6.787137228248626641, 1.040834085586084257E-14 ) ) ;
#135294 = EDGE_CURVE ( 'NONE', #45181, #63797, #212344, .T. ) ;
#135295 = CARTESIAN_POINT ( 'NONE',  ( 1.364683531249988535, 3.405208333674749621, -0.7879004041258239610 ) ) ;
#135296 = CARTESIAN_POINT ( 'NONE',  ( 4.704715985517350596, 1.906866092115505840, 1.080010033982371498 ) ) ;
#135297 = CARTESIAN_POINT ( 'NONE',  ( 6.983263157960370116, 1.251666756963093041, 2.167287073222202931 ) ) ;
#135298 = CARTESIAN_POINT ( 'NONE',  ( 4.786124093267453361, -1.070777880904892232, 1.993102913963458400 ) ) ;
#135299 = CARTESIAN_POINT ( 'NONE',  ( -5.096975683733680818, 8.033889833409558534, -1.199719254218452047 ) ) ;
#135300 = CARTESIAN_POINT ( 'NONE',  ( -1.387778780781445676E-14, 3.949999999999946443, -1.007084189318404821 ) ) ;
#135301 = CARTESIAN_POINT ( 'NONE',  ( 5.865087380380676230, 7.178575736046542310, -1.148900262672468475 ) ) ;
#135302 = AXIS2_PLACEMENT_3D ( 'NONE', #31977, #46107, #94856 ) ;
#135303 = CARTESIAN_POINT ( 'NONE',  ( -0.7500000000000179856, 14.04166666666666785, 1.299038105676658228 ) ) ;
#135304 = CARTESIAN_POINT ( 'NONE',  ( -5.763624699140882157, 7.817591130454727200, -1.443375672974066548 ) ) ;
#135305 = CARTESIAN_POINT ( 'NONE',  ( 4.665414256878284149, 6.536345614481700927, -1.443375672974068769 ) ) ;
#135306 = CARTESIAN_POINT ( 'NONE',  ( 5.764868906847371299, -1.600580677892119441, -0.7553990054774415430 ) ) ;
#135307 =( BOUNDED_SURFACE ( )  B_SPLINE_SURFACE ( 3, 2, ( 
 ( #157767, #89574, #14680 ),
 ( #12550, #196652, #80777 ),
 ( #146865, #195593, #160960 ),
 ( #99158, #194511, #15744 ),
 ( #177210, #163100, #180403 ),
 ( #45098, #178286, #162033 ),
 ( #210761, #181453, #46159 ),
 ( #147912, #65550, #32022 ),
 ( #94910, #213927, #78625 ),
 ( #47227, #112272, #129608 ) ),
 .UNSPECIFIED., .F., .F., .T. ) 
 B_SPLINE_SURFACE_WITH_KNOTS ( ( 4, 2, 2, 2, 4 ),
 ( 3, 3 ),
 ( 2.466559942404522587E-18, 0.0004030251014121731448, 0.0008060502028243437958, 0.001209075304236514447, 0.001612100405648685206 ),
 ( 0.000000000000000000, 1.000000000000000000 ),
 .UNSPECIFIED. ) 
 GEOMETRIC_REPRESENTATION_ITEM ( )  RATIONAL_B_SPLINE_SURFACE ( (
 ( 1.000000000000000000, 0.8509629433967630385, 1.000000000000000000),
 ( 1.000000000000000000, 0.8510310118808805946, 1.000000000000000000),
 ( 1.000000000000000000, 0.8495812529563545601, 1.000000000000000000),
 ( 1.000000000000000000, 0.8465918360525764852, 1.000000000000000000),
 ( 1.000000000000000000, 0.8452340365386274978, 1.000000000000000000),
 ( 1.000000000000000000, 0.8452309425927184705, 1.000000000000000000),
 ( 1.000000000000000000, 0.8465710739603050650, 1.000000000000000000),
 ( 1.000000000000000000, 0.8495952187152687740, 1.000000000000000000),
 ( 1.000000000000000000, 0.8510135196387145218, 1.000000000000000000),
 ( 1.000000000000000000, 0.8509629433966235945, 1.000000000000000000) ) ) 
 REPRESENTATION_ITEM ( '' )  SURFACE ( )  );
#135308 = CARTESIAN_POINT ( 'NONE',  ( 6.934105498385400246, 10.17720795050327354, -1.199719254218441611 ) ) ;
#135309 = CARTESIAN_POINT ( 'NONE',  ( 2.239418434904976607, -1.881632620311970649, 0.9459126739295388164 ) ) ;
#135311 = CARTESIAN_POINT ( 'NONE',  ( 0.7499999999999902300, 1.983333333333357817, 1.299038105676669330 ) ) ;
#135310 = CARTESIAN_POINT ( 'NONE',  ( -1.402160292154681736E-14, 12.17187500034140335, 1.575800808251682339 ) ) ;
#135312 = CARTESIAN_POINT ( 'NONE',  ( 1.767950473188628857, -1.955055593144053194, 0.2378005183036585035 ) ) ;
#135313 = CARTESIAN_POINT ( 'NONE',  ( 1.059204734455133412, 0.3686402435371800013, -1.833797362824276078 ) ) ;
#135314 = CARTESIAN_POINT ( 'NONE',  ( 1.433958818539453395, 1.165882187713672247, 1.577721859592796205 ) ) ;
#135316 = ORIENTED_EDGE ( 'NONE', *, *, #63078, .F. ) ;
#135315 = CARTESIAN_POINT ( 'NONE',  ( 5.467019156909919353, -1.422831870918849217, 1.121200454338074692 ) ) ;
#135317 = CARTESIAN_POINT ( 'NONE',  ( 6.371969008742804697, 7.496680600697164465, -1.082531754730543083 ) ) ;
#135318 = CARTESIAN_POINT ( 'NONE',  ( -0.6823417656250246877, -0.3864583329919110688, 1.181850606188755259 ) ) ;
#135319 = CARTESIAN_POINT ( 'NONE',  ( 6.104356062600288624, -0.6750377415852754082, -1.744797942764392706 ) ) ;
#135320 = ORIENTED_EDGE ( 'NONE', *, *, #183389, .T. ) ;
#135321 = CARTESIAN_POINT ( 'NONE',  ( 5.629760504653214426, 1.996728726787128538, -0.5467053113129491937 ) ) ;
#135322 =( NAMED_UNIT ( * ) PLANE_ANGLE_UNIT ( ) SI_UNIT ( $, .RADIAN. ) );
#135323 = EDGE_CURVE ( 'NONE', #29771, #121694, #38463, .T. ) ;
#135324 = CARTESIAN_POINT ( 'NONE',  ( -4.950135482320918712, 7.828889591799445213, -1.082531754730549967 ) ) ;
#135325 = DIRECTION ( 'NONE',  ( -3.330669073875485398E-16, 1.665334536937734071E-16, 1.000000000000000000 ) ) ;
#135326 = CARTESIAN_POINT ( 'NONE',  ( 1.499999999999987566, 0.02500000000001806333, 0.000000000000000000 ) ) ;
#135327 = CARTESIAN_POINT ( 'NONE',  ( 6.103141704446003679, 10.27208242182903142, 0.7998128361456462443 ) ) ;
#135328 = CARTESIAN_POINT ( 'NONE',  ( -9.365985188942097750, 9.821404230054264772, 0.7998128361456462443 ) ) ;
#135329 = CARTESIAN_POINT ( 'NONE',  ( 4.857564175446106525, 8.889184981320973122, 0.7998128361456331437 ) ) ;
#135330 = CARTESIAN_POINT ( 'NONE',  ( -1.402160292154681736E-14, -0.3031249996585801965, -1.575800808251665908 ) ) ;
#135331 = CARTESIAN_POINT ( 'NONE',  ( -0.7500000000000006661, 1.858333333333357595, -1.299038105676652011 ) ) ;
#135333 = CARTESIAN_POINT ( 'NONE',  ( 4.497554271431305040, 6.270232621468402989, -1.599625672291256295 ) ) ;
#135332 = CARTESIAN_POINT ( 'NONE',  ( 4.984793487045196869, 1.876812866478014596, 0.5713181500588762063 ) ) ;
#135334 = CARTESIAN_POINT ( 'NONE',  ( 3.216172551982798833, -1.646586737935524125, -1.163091166099708529 ) ) ;
#135335 = CARTESIAN_POINT ( 'NONE',  ( 2.325271742496349159, -1.422496398144998508, -1.283381434195222326 ) ) ;
#135336 = CARTESIAN_POINT ( 'NONE',  ( 0.7499999999999920064, 4.514583334016150751, 1.299038105676669330 ) ) ;
#135337 = CARTESIAN_POINT ( 'NONE',  ( 0.5038066827526346270, -2.180447833630628107, 0.2205874978757973448 ) ) ;
#135338 = CARTESIAN_POINT ( 'NONE',  ( 0.2333690889706925564, 0.2409277441041447754, -2.087868073146467829 ) ) ;
#135339 = CARTESIAN_POINT ( 'NONE',  ( 2.776451973220807279, -1.788819259240326698, -0.5467896145717602296 ) ) ;
#135340 = CARTESIAN_POINT ( 'NONE',  ( 1.499999999999985123, -0.6729166659838520248, -0.8660254037844323793 ) ) ;
#135341 = CARTESIAN_POINT ( 'NONE',  ( 3.955341514648374357, -1.749461739742008470, 0.9961098753780948112 ) ) ;
#135342 = CARTESIAN_POINT ( 'NONE',  ( -6.659026002606323047, 10.92061410301605662, 0.000000000000000000 ) ) ;
#135344 = CARTESIAN_POINT ( 'NONE',  ( 4.517270869736185190, -1.935087425045402654, 0.8595401143802297028 ) ) ;
#135343 = CARTESIAN_POINT ( 'NONE',  ( -4.853455804012230423, 6.685451076146141425, 1.443375672974064550 ) ) ;
#135345 = FACE_OUTER_BOUND ( 'NONE', #189954, .T. ) ;
#135346 = CARTESIAN_POINT ( 'NONE',  ( 5.512195382060368409, 2.068158883198469855, -0.09793725168850964113 ) ) ;
#135348 = CARTESIAN_POINT ( 'NONE',  ( 6.620655732516647518, 3.684600858287550906, 2.687722323901103660 ) ) ;
#135347 = CARTESIAN_POINT ( 'NONE',  ( 1.382492367555522295, -0.3100735531622924035, -2.067509394536557021 ) ) ;
#135350 = ORIENTED_EDGE ( 'NONE', *, *, #175445, .F. ) ;
#135349 = CARTESIAN_POINT ( 'NONE',  ( 6.528339890195161921, 1.048227956652090231, -1.494441373796271622 ) ) ;
#135351 = CARTESIAN_POINT ( 'NONE',  ( 8.586391356156291010, 8.911878091804165791, 0.7998128361456481317 ) ) ;
#135352 = DIRECTION ( 'NONE',  ( 0.000000000000000000, 0.000000000000000000, -1.000000000000000000 ) ) ;
#135353 = CARTESIAN_POINT ( 'NONE',  ( 6.195713011320782115, 8.251417818006149929, -1.443375672974057666 ) ) ;
#135354 = AXIS2_PLACEMENT_3D ( 'NONE', #212951, #64588, #96050 ) ;
#135356 = CARTESIAN_POINT ( 'NONE',  ( 0.6975727754284127835, 1.215713746931287753, 1.343078931132860587 ) ) ;
#135355 = CARTESIAN_POINT ( 'NONE',  ( 7.452141709366786770, 8.723195411463290583, 1.199719254218452047 ) ) ;
#135357 = CARTESIAN_POINT ( 'NONE',  ( -7.537443334193545397, 10.88110209227943770, -1.199719254218446718 ) ) ;
#135358 = PRESENTATION_LAYER_ASSIGNMENT (  '', '', ( #86792 ) ) ;
#135359 = CARTESIAN_POINT ( 'NONE',  ( 5.250031796989762967, 7.148123067953287446, 1.599625672291267398 ) ) ;
#135360 = TOROIDAL_SURFACE ( 'NONE', #131976, 2.080000000000000071, 0.08000000000000000167 ) ;
#135361 = CARTESIAN_POINT ( 'NONE',  ( -7.142181811248260459E-15, -6.291672674598642878, 10.90688615205475465 ) ) ;
#135362 = CARTESIAN_POINT ( 'NONE',  ( -11.44800751630026880, 11.29999999999998117, 3.302956944461236777 ) ) ;
#135363 = CARTESIAN_POINT ( 'NONE',  ( 3.765413976293345844, 5.416068943807445635, 1.599625672291267398 ) ) ;
#135364 = ORIENTED_EDGE ( 'NONE', *, *, #31576, .F. ) ;
#135365 = CARTESIAN_POINT ( 'NONE',  ( 5.958611281643053204, -1.915606116362132072, -0.6298603123368745615 ) ) ;
#135366 = CARTESIAN_POINT ( 'NONE',  ( 0.5398874254142792539, -2.012210497580559476, 0.6691108114003360141 ) ) ;
#135367 = CARTESIAN_POINT ( 'NONE',  ( -3.011287625495571607, 6.360174617139689346, -0.7852620323503290978 ) ) ;
#135368 = FACE_OUTER_BOUND ( 'NONE', #178712, .T. ) ;
#135369 = PLANE ( 'NONE',  #150711 ) ;
#135370 = CARTESIAN_POINT ( 'NONE',  ( -5.273758566035884776, 5.255065869904374409, 0.000000000000000000 ) ) ;
#135371 = CARTESIAN_POINT ( 'NONE',  ( 8.920901888111997025, 10.47043562662792304, 1.082531754730549967 ) ) ;
#135372 = CARTESIAN_POINT ( 'NONE',  ( 3.362113288959746704, -1.967404159762261795, 0.09189030742163574461 ) ) ;
#135373 = CARTESIAN_POINT ( 'NONE',  ( 4.692982559244565088, 1.755779632255444422, 0.9913831279167032440 ) ) ;
#135374 = CARTESIAN_POINT ( 'NONE',  ( -5.747767057189642870, 8.793146435774861658, -1.199719254218440723 ) ) ;
#135375 = CARTESIAN_POINT ( 'NONE',  ( -0.7500000000000006661, 10.20833333333333393, -1.299038105676657340 ) ) ;
#135376 = CARTESIAN_POINT ( 'NONE',  ( 4.330150130892728377, 2.148942519667027984, 0.4286813238914553570 ) ) ;
#135377 = CARTESIAN_POINT ( 'NONE',  ( 3.904598122329021148, 2.800000000000017586, 0.7750000000000135669 ) ) ;
#135378 = CARTESIAN_POINT ( 'NONE',  ( 4.805647293689061961, -0.5139743781695116365, 1.856484447351488765 ) ) ;
#135379 = CARTESIAN_POINT ( 'NONE',  ( -6.561256274009600986, 9.742217188731485678, -1.199719254218440723 ) ) ;
#135380 = CARTESIAN_POINT ( 'NONE',  ( -0.1294898018151837138, 2.036186877494918335, -2.343407025977122693 ) ) ;
#135381 = VERTEX_POINT ( 'NONE', #46688 ) ;
#135382 = CARTESIAN_POINT ( 'NONE',  ( 5.234856708652233515, 6.240325927249993576, 1.082531754730549078 ) ) ;
#135383 = CARTESIAN_POINT ( 'NONE',  ( 5.576995328841173105, 1.818227641914264225, 0.7572995901278417596 ) ) ;
#135385 = CARTESIAN_POINT ( 'NONE',  ( 4.565094110769337910, -1.615551665759178412, 1.200850101804177283 ) ) ;
#135384 = CARTESIAN_POINT ( 'NONE',  ( 0.6088030852571654217, -0.2837962540496056785, 1.921085339388538982 ) ) ;
#135386 = CARTESIAN_POINT ( 'NONE',  ( 5.975955848901470802, 2.022625890308630048, 1.091648031176053468 ) ) ;
#135388 = CARTESIAN_POINT ( 'NONE',  ( 4.293699386915854177, -1.280875055806574236, -1.350249269484518955 ) ) ;
#135387 = CARTESIAN_POINT ( 'NONE',  ( -7.442499979258930587, 7.647614495415686164, -0.7998128361456362523 ) ) ;
#135389 = CARTESIAN_POINT ( 'NONE',  ( 7.849244587668864348, 8.122149871893999062, 0.7998128361456291469 ) ) ;
#135390 = DIRECTION ( 'NONE',  ( -1.000000000000000000, 0.000000000000000000, 0.000000000000000000 ) ) ;
#135391 = CARTESIAN_POINT ( 'NONE',  ( -5.506582945444718824, 9.576097202994168001, 0.7998128361456481317 ) ) ;
#135392 = CARTESIAN_POINT ( 'NONE',  ( -3.372896589461368055, -0.9467711724014528096, 0.1326515144533354784 ) ) ;
#135393 = CARTESIAN_POINT ( 'NONE',  ( 0.6268464039562298140, 0.1668571106153530770, 2.185281662807083691 ) ) ;
#135394 = CARTESIAN_POINT ( 'NONE',  ( 3.375617060122621194, 6.882044303544283537, 1.040834085586084257E-14 ) ) ;
#135395 = EDGE_LOOP ( 'NONE', ( #157090, #74492, #155181, #120383, #130241, #60205 ) ) ;
#135396 = DIRECTION ( 'NONE',  ( -0.9512177852344306794, 0.3085202182251672864, 0.000000000000000000 ) ) ;
#135397 = CARTESIAN_POINT ( 'NONE',  ( 0.7502976729042536430, 0.5272139720400963459, 1.747899773703022408 ) ) ;
#135398 = CARTESIAN_POINT ( 'NONE',  ( -4.086893239515592136, 6.855460315155083251, 1.199719254218464037 ) ) ;
#135399 = CARTESIAN_POINT ( 'NONE',  ( 2.619397310362530096, 0.2141275842034353338, 1.720801833696316008 ) ) ;
#135400 = CARTESIAN_POINT ( 'NONE',  ( -1.499999999999997780, 5.400000000000022560, 1.214306433183764966E-14 ) ) ;
#135401 = CARTESIAN_POINT ( 'NONE',  ( -0.4500000000000198286, 3.950000000000009059, 0.8338124244295502807 ) ) ;
#135402 = DIRECTION ( 'NONE',  ( -5.578564026256490882E-16, -1.000000000000000000, -9.066213480720158442E-32 ) ) ;
#135403 = CARTESIAN_POINT ( 'NONE',  ( 5.057177669875371429, -1.544152220135000420, -0.9737345633797565014 ) ) ;
#135404 = CARTESIAN_POINT ( 'NONE',  ( 3.291801117278610800, -1.314073873198824627, -1.456807609480186061 ) ) ;
#135405 = CARTESIAN_POINT ( 'NONE',  ( 0.6124999999999949374, -0.7708333326505306671, -1.060881119635962211 ) ) ;
#135406 = CARTESIAN_POINT ( 'NONE',  ( -7.980945979938748103, 12.46285407657057220, 0.000000000000000000 ) ) ;
#135407 = CARTESIAN_POINT ( 'NONE',  ( 5.940443861082012944, 10.08226827123770697, 0.7998128361456462443 ) ) ;
#135408 = ADVANCED_FACE ( 'NONE', ( #14138, #153760, #5330, #137523, #69276, #138587, #166816 ), #54129, .T. ) ;
#135409 = CARTESIAN_POINT ( 'NONE',  ( 4.705793326368500118, 1.571798730262342181, 1.423547657546264000 ) ) ;
#135410 = CARTESIAN_POINT ( 'NONE',  ( 6.587282531393223728, 8.778525268082516320, 1.599625672291268286 ) ) ;
#135411 = CARTESIAN_POINT ( 'NONE',  ( -8.839026081105473054, 12.39961529701003684, -1.199719254218446718 ) ) ;
#135412 = AXIS2_PLACEMENT_3D ( 'NONE', #109758, #111893, #78246 ) ;
#135413 = CARTESIAN_POINT ( 'NONE',  ( 2.747004861044194612, -0.3495022371792326221, -2.040372298647576965 ) ) ;
#135415 = CARTESIAN_POINT ( 'NONE',  ( -1.364683531250014514, -0.4489583329919089039, -0.7879004041258359514 ) ) ;
#135414 = CARTESIAN_POINT ( 'NONE',  ( -11.96535697748077887, 11.25262667064452948, 0.9148528286454729042 ) ) ;
#135417 = ORIENTED_EDGE ( 'NONE', *, *, #77449, .T. ) ;
#135416 = CARTESIAN_POINT ( 'NONE',  ( 4.582826572872266802, -1.451171176318547529, 1.681852496032259614 ) ) ;
#135418 = CARTESIAN_POINT ( 'NONE',  ( 3.463815647965732936, -2.215898795117266840, -0.6112515151598179042 ) ) ;
#135419 = CARTESIAN_POINT ( 'NONE',  ( 8.053180056837369705, 11.37883191874353805, -1.082531754730543083 ) ) ;
#135421 = CARTESIAN_POINT ( 'NONE',  ( 1.642778471875001811, -2.792708332855376785, 2.845375778867859751 ) ) ;
#135420 = CARTESIAN_POINT ( 'NONE',  ( 6.916067756746836714, 8.201738816693689316, -1.082531754730548412 ) ) ;
#135422 = CARTESIAN_POINT ( 'NONE',  ( -10.62336932346880936, 4.106376894962319390, 5.581641476743597785 ) ) ;
#135423 = CARTESIAN_POINT ( 'NONE',  ( -5.492770192564149667, 6.262391236846517550, -0.9919644673941154789 ) ) ;
#135424 = CARTESIAN_POINT ( 'NONE',  ( 3.058751851047710080, 0.4689117840017149041, 1.853869267190631831 ) ) ;
#135425 = CARTESIAN_POINT ( 'NONE',  ( 0.000000000000000000, 3.300000000000025135, 1.561251128379126385E-14 ) ) ;
#135426 = CARTESIAN_POINT ( 'NONE',  ( 4.348488605181799471, 0.4613061074445113374, 1.661866727659202736 ) ) ;
#135427 = CARTESIAN_POINT ( 'NONE',  ( 3.731657894805060938, 0.6748485617756972976, -1.900415309456899182 ) ) ;
#135428 = CARTESIAN_POINT ( 'NONE',  ( 3.991116696687820209, -2.292486273863734603, 0.1698809440028921647 ) ) ;
#135429 = DIRECTION ( 'NONE',  ( -0.000000000000000000, 1.000000000000000000, -0.000000000000000000 ) ) ;
#135430 = CARTESIAN_POINT ( 'NONE',  ( 6.111965604441711442, -2.090389680133018846, 0.2559737671669787273 ) ) ;
#135431 = CARTESIAN_POINT ( 'NONE',  ( -4.651856103264620401, 8.441266197201775512, 0.000000000000000000 ) ) ;
#135432 = ORIENTED_EDGE ( 'NONE', *, *, #115558, .T. ) ;
#135433 = CARTESIAN_POINT ( 'NONE',  ( 4.745210919507984570, -1.367539302148174318, -1.123239564495488674 ) ) ;
#135435 = CARTESIAN_POINT ( 'NONE',  ( 0.5863596474044476814, -2.275655805637688989, -0.2749888630660061728 ) ) ;
#135434 = CARTESIAN_POINT ( 'NONE',  ( 6.821687566331318564, 7.987665577921906568, 1.199719254218452935 ) ) ;
#135436 = CARTESIAN_POINT ( 'NONE',  ( 0.3920123891120600446, 1.449622948667350641, -0.9626461102210502885 ) ) ;
#135437 = CARTESIAN_POINT ( 'NONE',  ( -6.474900878978163021, 9.711745571186627402, -1.199719254218452047 ) ) ;
#135438 = AXIS2_PLACEMENT_3D ( 'NONE', #125460, #208738, #93969 ) ;
#135439 = CARTESIAN_POINT ( 'NONE',  ( 6.456982561897790518, 0.3786298020890948024, -2.158335565738931816 ) ) ;
#135440 = CARTESIAN_POINT ( 'NONE',  ( -4.248501033035892327, 6.049946853332221153, -1.599625672291271394 ) ) ;
#135441 = CARTESIAN_POINT ( 'NONE',  ( -1.360316468750042862, -0.8489583329918899413, -0.7853790794159322131 ) ) ;
#135442 = CARTESIAN_POINT ( 'NONE',  ( 9.499984059629561273, -7.809931833644721877, 0.02724524595756149317 ) ) ;
#135443 = CARTESIAN_POINT ( 'NONE',  ( 0.2917819264270337110, -1.984717812412156501, 0.8806528889930710369 ) ) ;
#135444 = CARTESIAN_POINT ( 'NONE',  ( 0.9894706735516716201, -0.4852629857438545691, 1.957171443305204761 ) ) ;
#135445 = CARTESIAN_POINT ( 'NONE',  ( -1.364683531249997417, 5.759375000341418804, 1.214306433183764966E-14 ) ) ;
#135446 = CARTESIAN_POINT ( 'NONE',  ( 5.883413297016587329, 1.779079706761811153, -0.7395700111451685155 ) ) ;
#135447 = CARTESIAN_POINT ( 'NONE',  ( -1.364683531250000748, 11.85937500034139802, 0.000000000000000000 ) ) ;
#135448 = CARTESIAN_POINT ( 'NONE',  ( 1.055278351191447639, 0.4402236684300055991, 2.177206957374391738 ) ) ;
#135450 = ORIENTED_EDGE ( 'NONE', *, *, #111829, .F. ) ;
#135449 = CARTESIAN_POINT ( 'NONE',  ( 10.16199982864259788, 11.81442020729326536, 1.199719254218452047 ) ) ;
#135451 = CARTESIAN_POINT ( 'NONE',  ( 0.5028141819148617131, 7.728236690828134137, -1.993924427468488414 ) ) ;
#135452 = FACE_OUTER_BOUND ( 'NONE', #78837, .T. ) ;
#135454 = ADVANCED_FACE ( 'NONE', ( #136458 ), #85550, .F. ) ;
#135453 = CARTESIAN_POINT ( 'NONE',  ( 9.565441069641300587, 11.11843498845840905, -1.199719254218440723 ) ) ;
#135455 = CARTESIAN_POINT ( 'NONE',  ( 1.408343819019454993E-15, 1.000000000000000888, 11.49999999999998934 ) ) ;
#135456 = DIRECTION ( 'NONE',  ( -0.5773502691896166272, 0.000000000000000000, -0.8164965809277325848 ) ) ;
#135457 = CARTESIAN_POINT ( 'NONE',  ( 3.895860127252141591, -0.5505607855701463160, -1.651121638195630181 ) ) ;
#135458 = CARTESIAN_POINT ( 'NONE',  ( 1.961309178647975715, 1.629323162926434199, 1.092499269706406650 ) ) ;
#135460 = CARTESIAN_POINT ( 'NONE',  ( 1.364683531249988535, 3.217708333674748289, -0.7879004041258239610 ) ) ;
#135459 = CARTESIAN_POINT ( 'NONE',  ( 5.657830175604453338, 5.495223381160312393, 0.7998128361456341429 ) ) ;
#135461 = CARTESIAN_POINT ( 'NONE',  ( -5.899211624428097878, 6.007801130575932014, 0.1941222073163356709 ) ) ;
#135462 = CARTESIAN_POINT ( 'NONE',  ( 9.083072846151447166, 12.68433652289702884, 1.199719254218450271 ) ) ;
#135463 = CARTESIAN_POINT ( 'NONE',  ( 6.338335788673861160, -1.050647824335379399, 1.656640365463659670 ) ) ;
#135464 = CARTESIAN_POINT ( 'NONE',  ( -8.290974629956718189, 9.631557475493025322, -1.199719254218446718 ) ) ;
#135465 = CARTESIAN_POINT ( 'NONE',  ( -4.026408433134269771, 6.680931691089825541, 1.082531754730560403 ) ) ;
#135466 = CARTESIAN_POINT ( 'NONE',  ( 1.393865445735403830, 1.714438158727617179, 1.476448846179352348 ) ) ;
#135468 = VERTEX_POINT ( 'NONE', #19473 ) ;
#135467 = CARTESIAN_POINT ( 'NONE',  ( -4.720210035852093533, 8.658662141802762946, -0.7998128361456281477 ) ) ;
#135470 = ADVANCED_FACE ( 'NONE', ( #150576 ), #185169, .T. ) ;
#135469 = CARTESIAN_POINT ( 'NONE',  ( -1.500000000000015099, 0.4104166673494891726, -0.8660254037844383745 ) ) ;
#135471 = CARTESIAN_POINT ( 'NONE',  ( 1.616246341788161622, 1.260175398906153266, -1.382505567627971388 ) ) ;
#135472 = CARTESIAN_POINT ( 'NONE',  ( 0.7735316488602840268, 1.530413877909537979, -0.8155550471512038602 ) ) ;
#135473 = CARTESIAN_POINT ( 'NONE',  ( 3.948915171154475878, -1.822730400009948237, -1.216494452853926322 ) ) ;
#135474 = CARTESIAN_POINT ( 'NONE',  ( 5.069473898719869531, 0.2322026582469650102, -2.295885384840197663 ) ) ;
#135475 = CARTESIAN_POINT ( 'NONE',  ( 1.200152769736504421, -2.061077815970461025, -0.0008511993763692102862 ) ) ;
#135476 = CARTESIAN_POINT ( 'NONE',  ( 3.609261671491706736, -1.913043583297647565, 0.3329670706836064809 ) ) ;
#135477 = CARTESIAN_POINT ( 'NONE',  ( -5.219525951136862574, 5.191794485855519170, -0.7216878364870197293 ) ) ;
#135478 = CARTESIAN_POINT ( 'NONE',  ( 5.571519856497625156, 1.802974293077023393, -0.4980454429602265698 ) ) ;
#135479 = CARTESIAN_POINT ( 'NONE',  ( 3.994353263318512148, 7.604006752988897055, -0.01585061804776008443 ) ) ;
#135480 = CARTESIAN_POINT ( 'NONE',  ( 0.2097273702015931829, -1.334265282896981208, -1.107180986369905362 ) ) ;
#135481 = CARTESIAN_POINT ( 'NONE',  ( 5.573810548993915148, 5.675402860013913475, 0.000000000000000000 ) ) ;
#135482 = CARTESIAN_POINT ( 'NONE',  ( 1.360316468749968033, 1.015625000341371820, -4.163336342344337027E-14 ) ) ;
#135483 = CARTESIAN_POINT ( 'NONE',  ( 4.641250102003463773, 0.7743139518727223392, 1.862017545363145565 ) ) ;
#135484 = CARTESIAN_POINT ( 'NONE',  ( -3.104453987404957260, 6.565687385373657925, -0.7216878364870257245 ) ) ;
#135485 = CARTESIAN_POINT ( 'NONE',  ( 7.723341061279088038, 12.16231500480096983, -0.7998128361456291469 ) ) ;
#135487 = CARTESIAN_POINT ( 'NONE',  ( -7.100579091573052892, -6.583980363594996277, 6.484567079770450881 ) ) ;
#135486 = CARTESIAN_POINT ( 'NONE',  ( 1.681982107312831154, -0.9779208310041755947, 1.541497997293653555 ) ) ;
#135488 = CARTESIAN_POINT ( 'NONE',  ( -4.339491684825780737, 7.220434844675483355, -1.199719254218455378 ) ) ;
#135489 = CARTESIAN_POINT ( 'NONE',  ( -1.138412281109779656E-15, -6.027819618361853315, -10.79920600060117053 ) ) ;
#135490 = CARTESIAN_POINT ( 'NONE',  ( -11.75337143377970328, 4.618255228540592228, 5.022398747751031678 ) ) ;
#135491 = EDGE_LOOP ( 'NONE', ( #203530, #202669, #146030, #144366 ) ) ;
#135492 = CARTESIAN_POINT ( 'NONE',  ( -4.448483798615272100, 8.203998508444197313, 0.000000000000000000 ) ) ;
#135493 = CARTESIAN_POINT ( 'NONE',  ( -2.266184231778562541, 5.795632037050281404, 1.040834085586084257E-14 ) ) ;
#135494 = CARTESIAN_POINT ( 'NONE',  ( -9.917953063596627317, 11.52969898140628047, -1.199719254218441611 ) ) ;
#135495 = CARTESIAN_POINT ( 'NONE',  ( 5.848308768596990781, 0.9934667122631580805, -1.758341319078795761 ) ) ;
#135497 = VERTEX_POINT ( 'NONE', #2138 ) ;
#135496 = CARTESIAN_POINT ( 'NONE',  ( 6.375645204974608404, 0.3829637424261604361, -2.187886986038441339 ) ) ;
#135498 = CARTESIAN_POINT ( 'NONE',  ( -6.424584688029276514, 8.588711117491191871, 1.599625672291269396 ) ) ;
#135499 = CARTESIAN_POINT ( 'NONE',  ( 4.547870462380197765, 7.393267075163835855, 1.199719254218462483 ) ) ;
#135500 = CARTESIAN_POINT ( 'NONE',  ( 5.717669251203768788, -2.011168408518650974, 0.4492202366306179417 ) ) ;
#135501 = CARTESIAN_POINT ( 'NONE',  ( 4.658827374183164949, 1.163267680695537099, 1.646840100852072997 ) ) ;
#135502 = VERTEX_POINT ( 'NONE', #169994 ) ;
#135503 = ORIENTED_EDGE ( 'NONE', *, *, #207358, .F. ) ;
#135504 = CARTESIAN_POINT ( 'NONE',  ( 3.610856454189071751, 7.348000977992388272, 0.3914447831331854810 ) ) ;
#135505 = CARTESIAN_POINT ( 'NONE',  ( 4.390142812726693045, 4.016254791136236513, 1.214306433183764966E-14 ) ) ;
#135507 = ORIENTED_EDGE ( 'NONE', *, *, #108416, .F. ) ;
#135506 = CARTESIAN_POINT ( 'NONE',  ( -5.173318132066234476, 8.193232366456022930, -1.199719254218453823 ) ) ;
#135508 = CARTESIAN_POINT ( 'NONE',  ( 4.648548116941726427, 8.423941524322412278, -0.4686463081053967583 ) ) ;
#135509 = CARTESIAN_POINT ( 'NONE',  ( 5.536482449520531368, 1.943773098233076757, -0.5350085594507182352 ) ) ;
#135510 = CARTESIAN_POINT ( 'NONE',  ( 3.784953330938052751, 1.334695924059103644, 1.268461399425282687 ) ) ;
#135511 = PRESENTATION_LAYER_ASSIGNMENT (  '', '', ( #69753 ) ) ;
#135512 = CARTESIAN_POINT ( 'NONE',  ( -0.02338929933909470252, 2.896474228846234844, -2.200133910884606081 ) ) ;
#135513 = CARTESIAN_POINT ( 'NONE',  ( 1.665117554179825321, -1.629454703905337087, 1.634364892973801719 ) ) ;
#135514 = CARTESIAN_POINT ( 'NONE',  ( 7.340813827156391191, 7.528980651296110160, 0.7998128361456281477 ) ) ;
#135515 = CARTESIAN_POINT ( 'NONE',  ( 4.534552404040613105, 2.118918870418550870, 0.4265773709258223190 ) ) ;
#135516 = CARTESIAN_POINT ( 'NONE',  ( 8.097244055859613709, 10.46987070330147063, -1.599625672291262513 ) ) ;
#135518 = CARTESIAN_POINT ( 'NONE',  ( 2.694546298722868549, 1.457235452327232395, -1.394086077981852911 ) ) ;
#135517 = CARTESIAN_POINT ( 'NONE',  ( 0.01113493735188827126, -1.904398801838134148, 0.3797647843634504583 ) ) ;
#135519 = CARTESIAN_POINT ( 'NONE',  ( -5.382750679825375251, 6.238629533673094585, -1.199719254218446718 ) ) ;
#135520 = CARTESIAN_POINT ( 'NONE',  ( 3.849189735728062001, -1.136876111170448178, 1.997481460179703960 ) ) ;
#135521 = CARTESIAN_POINT ( 'NONE',  ( -9.367496997601206132, 15.51845925588232333, -7.499999999995496047 ) ) ;
#135522 = CARTESIAN_POINT ( 'NONE',  ( 3.080767038946086611, -0.1360980058115155988, -1.865751385159146070 ) ) ;
#135523 = CARTESIAN_POINT ( 'NONE',  ( 6.385619905723967094, 1.359199996644964381, 1.428251207276862500 ) ) ;
#135525 = CARTESIAN_POINT ( 'NONE',  ( -5.576146316970437944, 9.727530813099326323, 0.000000000000000000 ) ) ;
#135524 = CARTESIAN_POINT ( 'NONE',  ( 1.499999999999987566, -0.9437499993171851731, 0.000000000000000000 ) ) ;
#135526 = CARTESIAN_POINT ( 'NONE',  ( 1.471597369358583318, 0.1596246592955492538, -2.201166978212334424 ) ) ;
#135527 = ORIENTED_EDGE ( 'NONE', *, *, #73451, .F. ) ;
#135528 = CARTESIAN_POINT ( 'NONE',  ( -2.535011536075371996, 5.133042487381361596, 2.420000000000010587 ) ) ;
#135529 = CARTESIAN_POINT ( 'NONE',  ( 4.704842999142070603, 5.447737239542574272, -1.199719254218452047 ) ) ;
#135530 = CARTESIAN_POINT ( 'NONE',  ( -5.434120640978981065, 5.234228924097238611, -0.7998128361456221525 ) ) ;
#135531 = FACE_OUTER_BOUND ( 'NONE', #86742, .T. ) ;
#135532 = CARTESIAN_POINT ( 'NONE',  ( 0.8253839628637716919, -1.873344321310044469, 0.6141440057798281948 ) ) ;
#135533 = CARTESIAN_POINT ( 'NONE',  ( 0.3941752559601471306, 1.712991706939146486, 1.546321376980333007 ) ) ;
#135534 = CARTESIAN_POINT ( 'NONE',  ( 0.4319881149899909567, 1.126445828788334991, 1.606065282034954578 ) ) ;
#135535 = CARTESIAN_POINT ( 'NONE',  ( 4.381722380181817478, -1.975297276180818296, 0.5937428812356324581 ) ) ;
#135536 = CARTESIAN_POINT ( 'NONE',  ( 5.097502569058200983, 6.970172302033127210, -1.443375672974051449 ) ) ;
#135537 = CARTESIAN_POINT ( 'NONE',  ( 5.234329823327693809, 8.264412672927770487, 1.199719254218451159 ) ) ;
#135538 = ORIENTED_EDGE ( 'NONE', *, *, #185885, .F. ) ;
#135539 = CARTESIAN_POINT ( 'NONE',  ( 7.497295758232718654, 9.769931022736756177, -1.443375672974058777 ) ) ;
#135540 = CARTESIAN_POINT ( 'NONE',  ( 0.6823417656249917140, 5.155208333674749177, 1.181850606188765695 ) ) ;
#135541 = CARTESIAN_POINT ( 'NONE',  ( -10.51720842395916300, 3.993285388006064807, -5.782618101111140163 ) ) ;
#135542 = CARTESIAN_POINT ( 'NONE',  ( 3.945059511452237100, 6.586024615794168646, -1.082531754730548412 ) ) ;
#135543 = CARTESIAN_POINT ( 'NONE',  ( 6.672352044927558623, -1.017530931492259816, -1.917974758356699505 ) ) ;
#135545 = CARTESIAN_POINT ( 'NONE',  ( 5.249485218566787736, 1.838879873951341004, -0.09611505855997715120 ) ) ;
#135544 = CARTESIAN_POINT ( 'NONE',  ( 10.35465518852990741, -5.836144560139977955, -0.4365953560983623083 ) ) ;
#135546 = EDGE_CURVE ( 'NONE', #144017, #147946, #102057, .T. ) ;
#135547 = CARTESIAN_POINT ( 'NONE',  ( 1.843739406749228538, 8.920000000000001705, -0.7749999999999996891 ) ) ;
#135548 = CARTESIAN_POINT ( 'NONE',  ( 1.814759087649559177, 3.975067388632245624, 0.4606438099578184509 ) ) ;
#135549 = CARTESIAN_POINT ( 'NONE',  ( 1.255262969126037241E-15, 5.000000000000000888, -10.25000000000000000 ) ) ;
#135550 = CARTESIAN_POINT ( 'NONE',  ( -4.596643646408070438, 7.147595147647359148, 1.363028123281652793 ) ) ;
#135551 = CARTESIAN_POINT ( 'NONE',  ( 1.500000000000003997, 3.300000000000018030, 1.214306433183764966E-14 ) ) ;
#135552 = CARTESIAN_POINT ( 'NONE',  ( 5.207906507908255378, 7.834591108650524660, -1.266300940072472736 ) ) ;
#135553 = CARTESIAN_POINT ( 'NONE',  ( -1.001543065824772872E-14, 5.384375000341415252, 1.575800808251672791 ) ) ;
#135554 = CARTESIAN_POINT ( 'NONE',  ( 0.8383554657987003500, 1.138622818284718008, -1.536203910471350298 ) ) ;
#135555 = CARTESIAN_POINT ( 'NONE',  ( 1.867668082833298993, 0.9064309091474114233, 1.519949287764200685 ) ) ;
#135556 = CARTESIAN_POINT ( 'NONE',  ( 5.901044691261273734, -0.2977458250903759485, -1.990848032377992016 ) ) ;
#135558 = CARTESIAN_POINT ( 'NONE',  ( 4.481992950489037675, -1.915292616430896544, -0.04288535553729002497 ) ) ;
#135557 = CARTESIAN_POINT ( 'NONE',  ( -8.859363311525973117, 12.42334206583395328, -1.199719254218446718 ) ) ;
#135559 = CARTESIAN_POINT ( 'NONE',  ( -1.249999999999964695, 8.500000000000000000, -12.00100000000000122 ) ) ;
#135560 = CARTESIAN_POINT ( 'NONE',  ( 5.142998410927586583, -0.2390059684120172390, -1.954905448695958059 ) ) ;
#135561 = CARTESIAN_POINT ( 'NONE',  ( -0.1753031400193918732, -0.9122597987226389593, -1.912455998546586544 ) ) ;
#135562 = CARTESIAN_POINT ( 'NONE',  ( -1.491410138560268495, -1.333748936243116745, 1.500000000000001332 ) ) ;
#135563 = CARTESIAN_POINT ( 'NONE',  ( 3.783945140921864070, -0.9226758061156097313, 1.627204332209288395 ) ) ;
#135565 = ORIENTED_EDGE ( 'NONE', *, *, #139460, .F. ) ;
#135564 = CARTESIAN_POINT ( 'NONE',  ( 5.742733201377892449, 0.3429454505429993527, 1.690258806964558547 ) ) ;
#135567 = CARTESIAN_POINT ( 'NONE',  ( 3.877268743828270470, 5.546566172598190292, 1.443375672974062551 ) ) ;
#135566 = CARTESIAN_POINT ( 'NONE',  ( 3.756632125300945368, 0.7937082651479386852, 2.059386989456575279 ) ) ;
#135568 = CARTESIAN_POINT ( 'NONE',  ( 0.6823417656249899377, 5.238541667008086655, -1.181850606188754593 ) ) ;
#135569 = CARTESIAN_POINT ( 'NONE',  ( 0.9595213787957155294, 1.685235279958563037, 1.189114231603551675 ) ) ;
#135570 = CARTESIAN_POINT ( 'NONE',  ( 7.772902139336337335, 7.962807338847539107, 0.7998128361456341429 ) ) ;
#135571 = CARTESIAN_POINT ( 'NONE',  ( -9.450196763925152510, 10.98398329845622001, -1.199719254218441611 ) ) ;
#135572 = CARTESIAN_POINT ( 'NONE',  ( -9.096228393767150422, 0.9691415390508330008, -7.669416753559259448 ) ) ;
#135573 = CARTESIAN_POINT ( 'NONE',  ( -3.958090780185743451, 6.705190779270287393, -1.199719254218452047 ) ) ;
#135574 = AXIS2_PLACEMENT_3D ( 'NONE', #90492, #206345, #125193 ) ;
#135575 = CARTESIAN_POINT ( 'NONE',  ( -7.679448064523687556, -6.453073674884586275, -7.727353211424378365 ) ) ;
#135576 = ORIENTED_EDGE ( 'NONE', *, *, #80209, .F. ) ;
#135577 = B_SPLINE_CURVE_WITH_KNOTS ( 'NONE', 3,
 ( #82464, #120, #4387, #136574, #184224, #70458 ),
 .UNSPECIFIED., .F., .F.,
 ( 4, 2, 4 ),
 ( 0.000000000000000000, 0.0003202408338303456550, 0.0006404816676606913100 ),
 .UNSPECIFIED. ) ;
#135578 = CARTESIAN_POINT ( 'NONE',  ( 3.473154722801426786, 1.870513717286937494, 0.8877811045280564750 ) ) ;
#135579 = CARTESIAN_POINT ( 'NONE',  ( -1.201851678989727383E-14, 4.837500000000018119, -1.732050807568863648 ) ) ;
#135580 = CARTESIAN_POINT ( 'NONE',  ( 5.820528018968444961, 5.685037531751635953, 0.7998128361456341429 ) ) ;
#135581 = CARTESIAN_POINT ( 'NONE',  ( -6.611092229237963025, 6.760716375176868631, -0.1380881291089108287 ) ) ;
#135582 = CARTESIAN_POINT ( 'NONE',  ( 0.7858139957730024827, 1.945786914974199089, -0.5409757216557200543 ) ) ;
#135583 = FACE_OUTER_BOUND ( 'NONE', #206511, .T. ) ;
#135584 = EDGE_CURVE ( 'NONE', #112702, #33711, #20929, .T. ) ;
#135586 = CARTESIAN_POINT ( 'NONE',  ( 7.565086526745395723, 10.80938946696957004, -1.082531754730543083 ) ) ;
#135585 = CARTESIAN_POINT ( 'NONE',  ( 0.07479286986305369589, 0.004866263145587855152, -1.855573292446037970 ) ) ;
#135587 = CARTESIAN_POINT ( 'NONE',  ( 6.186875009713125984, -1.117664052418202658, -1.677746505241828334 ) ) ;
#135588 = CARTESIAN_POINT ( 'NONE',  ( 5.999236059146234368, -0.2270968913323672123, 1.902120139356741069 ) ) ;
#135589 = CARTESIAN_POINT ( 'NONE',  ( 6.539320575229239374, 3.684509595994990061, 2.717302710099603225 ) ) ;
#135590 = CARTESIAN_POINT ( 'NONE',  ( 3.896163805485418852, -0.6886730243073329039, -2.080591098665984795 ) ) ;
#135591 = CARTESIAN_POINT ( 'NONE',  ( 0.7499999999999920064, 4.014583334016149863, 1.299038105676669330 ) ) ;
#135592 = CARTESIAN_POINT ( 'NONE',  ( 3.199369407753744454, 1.726971514772487559, -0.8218122705464236954 ) ) ;
#135593 = CARTESIAN_POINT ( 'NONE',  ( -4.066556009095094737, 6.831733546331167695, 1.199719254218464037 ) ) ;
#135594 = CARTESIAN_POINT ( 'NONE',  ( 4.704316113817540668, 5.551085556617666228, -1.082531754730548412 ) ) ;
#135596 = CARTESIAN_POINT ( 'NONE',  ( 1.194935658704935566, 1.779638138761422628, 0.9480210990304924756 ) ) ;
#135595 = DIRECTION ( 'NONE',  ( -5.578564026256490882E-16, -1.000000000000000000, -9.066213480720158442E-32 ) ) ;
#135597 = CARTESIAN_POINT ( 'NONE',  ( -1.364683531250014514, 11.65104166700806587, -0.7879004041258335089 ) ) ;
#135599 = CARTESIAN_POINT ( 'NONE',  ( -5.601453741101424022, 6.564059448486966986, -1.199719254218453823 ) ) ;
#135598 = CARTESIAN_POINT ( 'NONE',  ( 5.952700804540857149, -1.878875186057769486, -1.127905468421293689 ) ) ;
#135601 = ORIENTED_EDGE ( 'NONE', *, *, #109387, .F. ) ;
#135600 = CARTESIAN_POINT ( 'NONE',  ( 2.572937677043420912, 0.08726698667262809683, -1.722694834735357894 ) ) ;
#135602 = CARTESIAN_POINT ( 'NONE',  ( 0.1399997263885795762, 1.361443548867202979, -2.255028951473649901 ) ) ;
#135603 = CARTESIAN_POINT ( 'NONE',  ( 5.947222937888848371, 10.09017719417900416, 1.040834085586084257E-14 ) ) ;
#135604 = CARTESIAN_POINT ( 'NONE',  ( 6.159481859310094620, 6.080483678816896109, 1.040834085586084257E-14 ) ) ;
#135605 = PRESENTATION_LAYER_ASSIGNMENT (  '', '', ( #4134 ) ) ;
#135606 = CARTESIAN_POINT ( 'NONE',  ( 1.419999999999989049, 6.280000000000042881, -2.499999999999995115 ) ) ;
#135607 = CARTESIAN_POINT ( 'NONE',  ( 1.697631272820496307, -1.418720726069604865, -1.355276769646639901 ) ) ;
#135608 = FILL_AREA_STYLE_COLOUR ( '', #116002 ) ;
#135609 = CARTESIAN_POINT ( 'NONE',  ( 5.691725559638619814, 5.534767995866836543, 1.040834085586084257E-14 ) ) ;
#135610 = CARTESIAN_POINT ( 'NONE',  ( 0.07536363704230969462, 1.333366039338843789, -2.397125032416930424 ) ) ;
#135611 = ORIENTED_EDGE ( 'NONE', *, *, #29409, .F. ) ;
#135612 = CARTESIAN_POINT ( 'NONE',  ( 0.000000000000000000, 5.499999999999998224, 0.000000000000000000 ) ) ;
#135613 = VERTEX_POINT ( 'NONE', #87686 ) ;
#135614 = CARTESIAN_POINT ( 'NONE',  ( 3.422321195131371674, -0.7368491698513750521, -1.655029553552778809 ) ) ;
#135615 = ORIENTED_EDGE ( 'NONE', *, *, #98658, .T. ) ;
#135616 = CARTESIAN_POINT ( 'NONE',  ( 2.847613298335896675E-16, 4.400000000000001243, -1.600000000000005196 ) ) ;
#135617 = EDGE_CURVE ( 'NONE', #90168, #184212, #202363, .T. ) ;
#135618 = CARTESIAN_POINT ( 'NONE',  ( 5.250580378299275708, 1.785639943600283219, 0.3038008075236381389 ) ) ;
#135619 = CARTESIAN_POINT ( 'NONE',  ( 7.810905894804431426, 8.285347430126213553, 0.000000000000000000 ) ) ;
#135620 = CARTESIAN_POINT ( 'NONE',  ( 0.2582262029270430137, -8.187798858731223817, 9.496816297611140101 ) ) ;
#135621 = CARTESIAN_POINT ( 'NONE',  ( 4.716373530444390560, 6.815548562371487762, -1.235710759775530798 ) ) ;
#135623 = CARTESIAN_POINT ( 'NONE',  ( -1.364683531250014514, 15.33854166700806587, -0.7879004041258335089 ) ) ;
#135622 = CARTESIAN_POINT ( 'NONE',  ( 4.598021663640887269, 0.7965279161250311546, -1.682138884369558607 ) ) ;
#135624 = CARTESIAN_POINT ( 'NONE',  ( 2.952642602588346321, -1.771063984568725935, -0.7304820402930515266 ) ) ;
#135625 = CARTESIAN_POINT ( 'NONE',  ( 3.919715808126649659, 7.587102519540811940, 0.000000000000000000 ) ) ;
#135626 = CARTESIAN_POINT ( 'NONE',  ( -11.13230441903222534, 5.430351611223322550, 4.009938051813186632 ) ) ;
#135627 = CARTESIAN_POINT ( 'NONE',  ( 9.499615238232420822, -9.906571760739462107, -0.08550182772145330234 ) ) ;
#135628 = CARTESIAN_POINT ( 'NONE',  ( -0.6823417656250003738, -1.032291666325242607, -1.181850606188749264 ) ) ;
#135629 = CARTESIAN_POINT ( 'NONE',  ( 5.002595493762530765, 8.780185809457538681, 1.040834085586084257E-14 ) ) ;
#135630 = CARTESIAN_POINT ( 'NONE',  ( -8.514157279702017078, 12.87700789305364069, -0.7216878364870267237 ) ) ;
#135631 = CARTESIAN_POINT ( 'NONE',  ( 0.7257156204387126275, -2.052300050329861847, 0.6792298617422781737 ) ) ;
#135632 = CARTESIAN_POINT ( 'NONE',  ( -6.961185525973791144, 7.086080966583015339, 0.7998128361456341429 ) ) ;
#135633 = CARTESIAN_POINT ( 'NONE',  ( 2.009825619773229377, -0.9864030779522957593, -1.843301731911746399 ) ) ;
#135634 = CARTESIAN_POINT ( 'NONE',  ( 6.540882763950133238, 6.595727744222092959, 0.000000000000000000 ) ) ;
#135635 = CARTESIAN_POINT ( 'NONE',  ( 0.6217474354073999621, -0.9722136304874777757, -1.544982199245432897 ) ) ;
#135636 = CARTESIAN_POINT ( 'NONE',  ( -4.232116505760120440, 8.089219690028791376, -0.7998128361456281477 ) ) ;
#135637 = CARTESIAN_POINT ( 'NONE',  ( 2.678497062878131274, -1.746332412481563345, -0.5319975912557314279 ) ) ;
#135638 = CARTESIAN_POINT ( 'NONE',  ( 12.55138299807035551, 7.397854759914610057, -0.9335798560614338992 ) ) ;
#135639 = CARTESIAN_POINT ( 'NONE',  ( 2.162237915172473546, 1.912057200688283665, 0.04323261116381121871 ) ) ;
#135640 = CARTESIAN_POINT ( 'NONE',  ( 2.769919614283973264, -1.948520106842245525, 0.2860871629452500509 ) ) ;
#135641 = CARTESIAN_POINT ( 'NONE',  ( 3.263160552478797882, 1.894124000634039851, -0.4281397233536556879 ) ) ;
#135642 = CARTESIAN_POINT ( 'NONE',  ( -4.085803189671902480, 5.860132702740892263, -1.599625672291271394 ) ) ;
#135644 = CARTESIAN_POINT ( 'NONE',  ( 4.482752736079084421, -1.382999391253452615, 1.607682512923855445 ) ) ;
#135643 = CARTESIAN_POINT ( 'NONE',  ( 6.994027139803230320, 9.253060644560830994, -1.599625672291267398 ) ) ;
#135645 = FACE_OUTER_BOUND ( 'NONE', #171365, .T. ) ;
#135646 = CARTESIAN_POINT ( 'NONE',  ( 9.772729797352075920, 10.29593960653257234, -0.7998128361456281477 ) ) ;
#135647 = CARTESIAN_POINT ( 'NONE',  ( 6.108345433475511399, 6.019830046288782377, 0.1574382575924727079 ) ) ;
#135648 = CARTESIAN_POINT ( 'NONE',  ( -1.203907071533397932, 3.087770253743141069, -0.7749999999999918066 ) ) ;
#135649 = VERTEX_POINT ( 'NONE', #154829 ) ;
#135650 = CARTESIAN_POINT ( 'NONE',  ( 7.388267364804250725, 7.584343111885245570, -0.7998128361456341429 ) ) ;
#135651 = CARTESIAN_POINT ( 'NONE',  ( 0.000000000000000000, 6.999999999999999112, 0.000000000000000000 ) ) ;
#135652 = CARTESIAN_POINT ( 'NONE',  ( 4.283705427790140519, 1.194290084605063251, 1.380960126487425166 ) ) ;
#135653 = CARTESIAN_POINT ( 'NONE',  ( 3.633072077242065861E-15, -6.802539632833518519E-15, -0.2598076211376265099 ) ) ;
#135654 = CARTESIAN_POINT ( 'NONE',  ( -8.270110514656041190, 10.67154823856396817, 1.443375672974090751 ) ) ;
#135655 = PRESENTATION_LAYER_ASSIGNMENT (  '', '', ( #156377 ) ) ;
#135656 = CARTESIAN_POINT ( 'NONE',  ( -4.804518813248800591, 8.239360463340183571, 0.8967481634083998010 ) ) ;
#135657 = CARTESIAN_POINT ( 'NONE',  ( 11.04536101718726293, 0.000000000000000000, 1.099999999999996758 ) ) ;
#135658 = CARTESIAN_POINT ( 'NONE',  ( 4.434354141042872399, 1.834536173243521917, 0.3649259964926266364 ) ) ;
#135659 = CARTESIAN_POINT ( 'NONE',  ( 7.588813295347141441, 9.876701482703580837, -1.599625672291262513 ) ) ;
#135660 = AXIS2_PLACEMENT_3D ( 'NONE', #210385, #75070, #95618 ) ;
#135661 = CARTESIAN_POINT ( 'NONE',  ( 1.840333348128117885, 1.905464876828693921, 0.2831333259317326823 ) ) ;
#135662 = CARTESIAN_POINT ( 'NONE',  ( -0.2958088229434103766, 2.800000000000024691, 1.358438285410177748 ) ) ;
#135663 = ADVANCED_FACE ( 'NONE', ( #119183 ), #202476, .T. ) ;
#135664 = CARTESIAN_POINT ( 'NONE',  ( -1.364683531250014514, 9.151041667008060543, -0.7879004041258335089 ) ) ;
#135665 = CARTESIAN_POINT ( 'NONE',  ( -5.065942953000576843, 9.062017211809330064, -0.7998128361456231517 ) ) ;
#135666 = CARTESIAN_POINT ( 'NONE',  ( 2.849184837166184536, 6.475799410002530898, 0.7998128361456362523 ) ) ;
#135667 = ADVANCED_FACE ( 'NONE', ( #35730 ), #36793, .T. ) ;
#135668 = CARTESIAN_POINT ( 'NONE',  ( -5.275531169048922386, 5.327410250078064458, -0.7216878364870338292 ) ) ;
#135669 = CARTESIAN_POINT ( 'NONE',  ( 1.054496592829538004, -1.339774933521440392, 1.639435421165438500 ) ) ;
#135670 = CARTESIAN_POINT ( 'NONE',  ( 9.028840231696797503, 12.62106513936658203, -1.199719254218446718 ) ) ;
#135671 = CARTESIAN_POINT ( 'NONE',  ( -5.345219749366619588, 4.708221922861152819, 2.500000000000000444 ) ) ;
#135672 = CARTESIAN_POINT ( 'NONE',  ( 6.209843387784004243, 0.6066176463192971546, -1.979359621541395331 ) ) ;
#135674 = CARTESIAN_POINT ( 'NONE',  ( 4.014041799177766379, 7.808471211821870206, -0.2759448393452879067 ) ) ;
#135673 = CARTESIAN_POINT ( 'NONE',  ( 0.8371598888798935656, 0.7463826720714299423, -1.683355135116317847 ) ) ;
#135675 = CARTESIAN_POINT ( 'NONE',  ( 6.604150285194997139, -0.1511744057106997885, 2.264526297252217990 ) ) ;
#135676 = CARTESIAN_POINT ( 'NONE',  ( 5.002595493762530765, 8.780185809457538681, 1.040834085586084257E-14 ) ) ;
#135678 = CYLINDRICAL_SURFACE ( 'NONE', #98151, 0.3999999999999997446 ) ;
#135677 = CARTESIAN_POINT ( 'NONE',  ( 4.773879485787624333, 4.742149952939897162, -0.7216878364870357165 ) ) ;
#135679 = CARTESIAN_POINT ( 'NONE',  ( 1.430038810223871026, 1.126473215625309887, -1.996311628086711254 ) ) ;
#135680 = CARTESIAN_POINT ( 'NONE',  ( 9.508009452425755015, 4.000007913748543587, -7.612499999891275237 ) ) ;
#135681 = CARTESIAN_POINT ( 'NONE',  ( -4.762657100150483380, 8.778460060142702304, 0.000000000000000000 ) ) ;
#135682 = CARTESIAN_POINT ( 'NONE',  ( 6.439402819763696328, 0.7408549094962694204, -1.795268486070795477 ) ) ;
#135683 = VERTEX_POINT ( 'NONE', #102878 ) ;
#135685 = ADVANCED_FACE ( 'NONE', ( #167875 ), #43135, .F. ) ;
#135684 = CARTESIAN_POINT ( 'NONE',  ( 9.368320956918616105, 10.03205532593431037, 0.7216878364870458196 ) ) ;
#135686 = CARTESIAN_POINT ( 'NONE',  ( 0.5803383592409648850, 0.9960403410373251942, 1.749501224816521816 ) ) ;
#135687 = LINE ( 'NONE', #86925, #158511 ) ;
#135689 = DIRECTION ( 'NONE',  ( 0.000000000000000000, 8.546850786086437571E-32, 1.000000000000000000 ) ) ;
#135688 = CARTESIAN_POINT ( 'NONE',  ( -8.690940161559884913, 10.09818392903003748, 1.199719254218462483 ) ) ;
#135690 = DIRECTION ( 'NONE',  ( -5.421010862427532031E-16, 0.5005768354468324022, 0.8656921114426507913 ) ) ;
#135692 = CARTESIAN_POINT ( 'NONE',  ( 0.9711603072033472284, 1.707112214499702407, -0.4667758381974375648 ) ) ;
#135691 = CARTESIAN_POINT ( 'NONE',  ( 3.328152359787967640, 2.039751367458849884, 0.4576943786474896858 ) ) ;
#135693 = CARTESIAN_POINT ( 'NONE',  ( 11.48243876534946217, 9.799999999999982947, 3.199999999999997957 ) ) ;
#135695 = CARTESIAN_POINT ( 'NONE',  ( 4.207168913946373934, -0.3938425722496830539, 2.258028373892074558 ) ) ;
#135694 = CARTESIAN_POINT ( 'NONE',  ( 4.329849954717849947, 6.144853928627882489, 1.599625672291262513 ) ) ;
#135696 = CARTESIAN_POINT ( 'NONE',  ( 3.099246252510225119, -1.738326302361908882, 0.08608614090572026811 ) ) ;
#135697 = CARTESIAN_POINT ( 'NONE',  ( 3.837121167867449945, 4.435395103055503441, 1.199719254218464037 ) ) ;
#135698 = CARTESIAN_POINT ( 'NONE',  ( -9.748756651352278979, 4.000007913748506283, -7.301653494139321410 ) ) ;
#135699 = CARTESIAN_POINT ( 'NONE',  ( 3.602662725270942445, 0.7809228151291653930, -1.548105009325143833 ) ) ;
#135700 = CARTESIAN_POINT ( 'NONE',  ( 3.402935010178400166, 0.5245792999575286109, 2.106750930608875194 ) ) ;
#135701 = CARTESIAN_POINT ( 'NONE',  ( 5.657830175604453338, 5.495223381160312393, 0.7998128361456341429 ) ) ;
#135702 = CARTESIAN_POINT ( 'NONE',  ( 5.050017674172561755, 0.9981218692422781924, 1.752141108012375437 ) ) ;
#135703 = CARTESIAN_POINT ( 'NONE',  ( 3.062500000000001776, -1.451031289061242013, -1.451031289060994656 ) ) ;
#135704 = CARTESIAN_POINT ( 'NONE',  ( -1.500000000000013101, 3.660416667349488673, -0.8660254037844313801 ) ) ;
#135705 = CARTESIAN_POINT ( 'NONE',  ( 1.606340841434449329, -0.6908775452558654218, -1.798418176235560662 ) ) ;
#135706 = CARTESIAN_POINT ( 'NONE',  ( 0.7500000000000006661, 8.447916667349467446, -1.299038105676657340 ) ) ;
#135707 = CARTESIAN_POINT ( 'NONE',  ( 5.027667009318355973, -0.3252736580323810633, 2.197331836796195592 ) ) ;
#135708 = EDGE_LOOP ( 'NONE', ( #107307, #124760, #150013, #19558 ) ) ;
#135709 = CARTESIAN_POINT ( 'NONE',  ( -0.1110810684432986112, 0.7552414886912374170, -1.881935688996359213 ) ) ;
#135710 = CARTESIAN_POINT ( 'NONE',  ( -0.7500000000000006661, 1.858333333333357595, -1.299038105676652011 ) ) ;
#135711 = CARTESIAN_POINT ( 'NONE',  ( 6.745345117998789775, 7.828323044875442172, 1.199719254218462483 ) ) ;
#135712 = CARTESIAN_POINT ( 'NONE',  ( 5.300874872818843286, 5.286701561151180506, 0.7216878364870317197 ) ) ;
#135713 = CARTESIAN_POINT ( 'NONE',  ( 3.285556943750000514, -2.413541666188708579, 1.896917185911906722 ) ) ;
#135714 = CARTESIAN_POINT ( 'NONE',  ( 0.2939904269894151323, 2.070328538627811632, -0.8053792395062376874 ) ) ;
#135715 = CARTESIAN_POINT ( 'NONE',  ( 5.916451087343006954, 0.7937011933104149985, 1.794315766958521241 ) ) ;
#135716 = CARTESIAN_POINT ( 'NONE',  ( 8.812436659202669276, 10.34389285956704363, -1.082531754730543083 ) ) ;
#135717 =( LENGTH_UNIT ( ) NAMED_UNIT ( * ) SI_UNIT ( .MILLI., .METRE. ) );
#135718 = CARTESIAN_POINT ( 'NONE',  ( 0.2984011986874868794, -2.161112683670802337, -0.05330630956579958390 ) ) ;
#135719 = VECTOR ( 'NONE', #76890, 1000.000000000000000 ) ;
#135720 = CARTESIAN_POINT ( 'NONE',  ( 4.095444919779759552, 6.935713618788495793, 1.199719254218451159 ) ) ;
#135722 = TOROIDAL_SURFACE ( 'NONE', #73390, 1.600000000000000311, 0.1000000000000000056 ) ;
#135721 = CARTESIAN_POINT ( 'NONE',  ( -4.421367491832313590, 6.251624388594711590, 1.443375672974065660 ) ) ;
#135723 = CARTESIAN_POINT ( 'NONE',  ( 3.209489602684848286, -1.684771875651757123, -1.189772946182314106 ) ) ;
#135724 = CARTESIAN_POINT ( 'NONE',  ( -6.064574784014443942, 5.969758757638621738, -0.7998128361456291469 ) ) ;
#135726 = EDGE_CURVE ( 'NONE', #21539, #21772, #10080, .T. ) ;
#135725 = CARTESIAN_POINT ( 'NONE',  ( 0.7499999999999902300, 3.514583334016149863, 1.299038105676669330 ) ) ;
#135727 = CARTESIAN_POINT ( 'NONE',  ( -1.602468905319636405E-14, -1.053124999658583638, -1.575800808251665908 ) ) ;
#135728 = CARTESIAN_POINT ( 'NONE',  ( 6.239502018287079288, -1.354773164471131164, -1.289998633004642237 ) ) ;
#135729 = CARTESIAN_POINT ( 'NONE',  ( 4.465268017702548775, -1.683484418668965921, -0.4155383358091616075 ) ) ;
#135730 = CARTESIAN_POINT ( 'NONE',  ( 3.526658842500699720, -1.606625690567566656, 0.6697392890405767796 ) ) ;
#135731 = CARTESIAN_POINT ( 'NONE',  ( 1.400361390298704656, -0.8304178796270310636, -2.136844513788013433 ) ) ;
#135732 = CARTESIAN_POINT ( 'NONE',  ( -1.201851678989727383E-14, 3.634375000341422357, 1.575800808251672791 ) ) ;
#135733 = CARTESIAN_POINT ( 'NONE',  ( 5.319903205935248458, 1.244510898466891780, -1.679860476595731233 ) ) ;
#135734 = CARTESIAN_POINT ( 'NONE',  ( 0.4449246239494052402, 0.5802587426733482046, -1.747387232072565189 ) ) ;
#135735 = EDGE_CURVE ( 'NONE', #120928, #79391, #192633, .T. ) ;
#135736 = DIRECTION ( 'NONE',  ( 1.000000000000000000, 0.000000000000000000, 0.000000000000000000 ) ) ;
#135737 = CARTESIAN_POINT ( 'NONE',  ( 1.635388916632842360, 0.6352005984417673501, 1.913803229121699534 ) ) ;
#135738 = CARTESIAN_POINT ( 'NONE',  ( 0.3752731597879420677, 2.043270790221253908, -0.7926104125151807178 ) ) ;
#135739 = CARTESIAN_POINT ( 'NONE',  ( 9.483953901554681210, 14.00935217397140953, -8.399901643884886582 ) ) ;
#135740 = CARTESIAN_POINT ( 'NONE',  ( -7.934546212495630968, 10.28005655271014795, -1.599625672291263179 ) ) ;
#135741 = CARTESIAN_POINT ( 'NONE',  ( 6.144869935491714230, 8.192100896205568361, -1.599625672291262513 ) ) ;
#135742 = CARTESIAN_POINT ( 'NONE',  ( 2.930460433956377564, -1.047063434655249647, -1.843881786051679850 ) ) ;
#135743 = CARTESIAN_POINT ( 'NONE',  ( 1.347111479061785482E-15, 0.9330127018934565308, -10.99999999999752553 ) ) ;
#135744 = CARTESIAN_POINT ( 'NONE',  ( 5.742758765878789085, 0.3605303665093100851, 1.789564367143759327 ) ) ;
#135745 = VERTEX_POINT ( 'NONE', #74641 ) ;
#135746 = CARTESIAN_POINT ( 'NONE',  ( -6.688968683495758683, 8.897159112202094988, -1.599625672291271394 ) ) ;
#135747 = CARTESIAN_POINT ( 'NONE',  ( -1.580000000000022276, 6.280000000000042881, 2.580000000000011173 ) ) ;
#135748 = CARTESIAN_POINT ( 'NONE',  ( -3.285556943749998737, -0.8677083328553740760, 1.896917185911908499 ) ) ;
#135749 = CARTESIAN_POINT ( 'NONE',  ( -8.206763054973658100, 8.468978407091068306, 0.7998128361456602331 ) ) ;
#135750 = CARTESIAN_POINT ( 'NONE',  ( 1.599874016572962798, 1.395964939349272349, 1.459955266877453806 ) ) ;
#135751 = CARTESIAN_POINT ( 'NONE',  ( 0.4992256481273240065, 1.750750569696429171, -1.170121261866068130 ) ) ;
#135752 = AXIS2_PLACEMENT_3D ( 'NONE', #167502, #85178, #116672 ) ;
#135753 = CARTESIAN_POINT ( 'NONE',  ( 8.367353357928214663, 12.91366268422496688, 1.040834085586084257E-14 ) ) ;
#135754 = CARTESIAN_POINT ( 'NONE',  ( 4.276097919418925031, -0.9535845961709583651, -1.597878833905818086 ) ) ;
#135755 = CARTESIAN_POINT ( 'NONE',  ( 8.703444544968814256, 12.24143683818393313, -1.199719254218446718 ) ) ;
#135756 = CARTESIAN_POINT ( 'NONE',  ( 11.97181042169641962, 13.88000000000000611, -0.8318531151397201562 ) ) ;
#135757 = ORIENTED_EDGE ( 'NONE', *, *, #113687, .T. ) ;
#135758 = CARTESIAN_POINT ( 'NONE',  ( -2.819205876637805641, 5.376491725131008259, -1.199719254218446718 ) ) ;
#135759 = CARTESIAN_POINT ( 'NONE',  ( -7.751511138711140170, 10.06651563329490529, -1.599625672291263179 ) ) ;
#135760 = CARTESIAN_POINT ( 'NONE',  ( 5.496661139185262002, -0.4475443406098400523, -1.769863040007889410 ) ) ;
#135762 = CARTESIAN_POINT ( 'NONE',  ( -3.978601536817720330, 7.845232424458246534, -0.1334687937623244003 ) ) ;
#135761 = CARTESIAN_POINT ( 'NONE',  ( -5.803772275101700906, 8.928762199997411386, -1.199719254218452047 ) ) ;
#135763 = CARTESIAN_POINT ( 'NONE',  ( 5.038060948978250408, 7.997685013099862239, -1.157798351953726490 ) ) ;
#135764 = CARTESIAN_POINT ( 'NONE',  ( 1.580929310206186100, 1.169321551402967119, -1.280364243709716243 ) ) ;
#135765 = CARTESIAN_POINT ( 'NONE',  ( 0.5326489567317398421, -1.227437504408007474, -1.234024486680666000 ) ) ;
#135767 = CARTESIAN_POINT ( 'NONE',  ( 7.944714827928043732, 10.29191993738131927, 1.443375672974076540 ) ) ;
#135766 = CARTESIAN_POINT ( 'NONE',  ( 5.830798129077900072, 2.222503408945066816, 0.6210771851366378993 ) ) ;
#135768 = CARTESIAN_POINT ( 'NONE',  ( 4.228163802615382494, 6.026220084508304708, -1.599625672291269396 ) ) ;
#135769 = CARTESIAN_POINT ( 'NONE',  ( 1.423197193765327384, -0.05341811584172677374, 2.060271317188705709 ) ) ;
#135770 = CARTESIAN_POINT ( 'NONE',  ( 6.830610463186557624, 6.863467050006115677, 1.040834085586084257E-14 ) ) ;
#135771 = CARTESIAN_POINT ( 'NONE',  ( 6.538407551539116902, 2.202477839928073333, -0.6571292610791487077 ) ) ;
#135772 = DIRECTION ( 'NONE',  ( 0.6507913734559606089, -0.7592566023653033458, 0.000000000000000000 ) ) ;
#135773 = CARTESIAN_POINT ( 'NONE',  ( -6.448838341955544173, 7.552674816150118708, 1.199719254218452047 ) ) ;
#135774 = CARTESIAN_POINT ( 'NONE',  ( 0.4265601315296633778, 1.885908329847274745, 0.5744540738892388587 ) ) ;
#135776 = CARTESIAN_POINT ( 'NONE',  ( -7.607533591043815768, 8.048079742405473525, 0.000000000000000000 ) ) ;
#135775 = CARTESIAN_POINT ( 'NONE',  ( 3.709155072767254868, 1.612916391665040416, -1.027221078234448859 ) ) ;
#135777 = CARTESIAN_POINT ( 'NONE',  ( 5.408869034151480903, 1.673104959687292448, -1.439203791633147267 ) ) ;
#135778 = CARTESIAN_POINT ( 'NONE',  ( -1.225000000000008082, 1.583333334016155503, 0.7072540797572817173 ) ) ;
#135779 = CARTESIAN_POINT ( 'NONE',  ( -7.878696662872776812, 8.364436659539265406, -0.7216878364870338292 ) ) ;
#135780 = CARTESIAN_POINT ( 'NONE',  ( 5.709392084686216506, 5.833581318321598985, -0.7216878364870458196 ) ) ;
#135781 = CARTESIAN_POINT ( 'NONE',  ( -3.472296738431328134, 7.065113604896248845, 0.000000000000000000 ) ) ;
#135782 = CARTESIAN_POINT ( 'NONE',  ( 5.373730994130427874, 0.4134100146411868737, -2.079626175754036410 ) ) ;
#135783 = CARTESIAN_POINT ( 'NONE',  ( 3.768876097860610397, -1.551941239651495108, 1.707908033328522146 ) ) ;
#135784 = CARTESIAN_POINT ( 'NONE',  ( 4.264078424595136418, -1.956757550135434620, 0.1421211968542570592 ) ) ;
#135785 = CARTESIAN_POINT ( 'NONE',  ( 0.6901946996495964548, 1.013433542811643440, -1.679602092450118489 ) ) ;
#135786 = CARTESIAN_POINT ( 'NONE',  ( 8.336750050606532625, 15.10367673868402605, 8.570998589250198307 ) ) ;
#135787 = CARTESIAN_POINT ( 'NONE',  ( -9.472340320762523191, 15.37246691557686873, 7.367375266019397628 ) ) ;
#135788 = ORIENTED_EDGE ( 'NONE', *, *, #8812, .T. ) ;
#135789 = CARTESIAN_POINT ( 'NONE',  ( 6.280482454654814362, -0.5424645211669875122, -1.942098458069536848 ) ) ;
#135790 = CARTESIAN_POINT ( 'NONE',  ( -8.941766003412679353, 10.39081407785832845, -1.199719254218446718 ) ) ;
#135791 = LINE ( 'NONE', #53460, #130700 ) ;
#135792 = CARTESIAN_POINT ( 'NONE',  ( 2.852568495416502703, -2.164958695077593642, -0.1640175257638913364 ) ) ;
#135793 = CARTESIAN_POINT ( 'NONE',  ( 10.26659657359305733, 10.85725357443524786, -6.218427518227997552 ) ) ;
#135794 = CARTESIAN_POINT ( 'NONE',  ( 1.090261293813089560, 1.267680250814690934, 1.699812782343253170 ) ) ;
#135795 = CARTESIAN_POINT ( 'NONE',  ( -0.7500000000000215383, 1.722916667349486008, 1.299038105676659116 ) ) ;
#135796 = CARTESIAN_POINT ( 'NONE',  ( 10.53876547652418338, 11.18964789890005918, 0.7998128361456462443 ) ) ;
#135797 = FILL_AREA_STYLE ('',( #202892 ) ) ;
#135798 = CARTESIAN_POINT ( 'NONE',  ( 6.378761646814803399, 6.917158162233129737, 0.8102004381213165907 ) ) ;
#135799 = CARTESIAN_POINT ( 'NONE',  ( 1.669287087933446490, 0.1544451976582127406, -2.055073672515697059 ) ) ;
#135801 = CARTESIAN_POINT ( 'NONE',  ( 8.790438134619869004, 13.29428800202395955, -8.101059483297389008 ) ) ;
#135800 = CARTESIAN_POINT ( 'NONE',  ( -10.31505594189871111, 10.92865344183699428, -0.7998128361456291469 ) ) ;
#135802 = CARTESIAN_POINT ( 'NONE',  ( -1.201851678989727383E-14, 2.571875000341417472, 1.575800808251672791 ) ) ;
#135803 = CARTESIAN_POINT ( 'NONE',  ( -2.449742653233033085, 3.949999999999988187, 0.4499999999999608757 ) ) ;
#135804 = ORIENTED_EDGE ( 'NONE', *, *, #39389, .T. ) ;
#135805 = CARTESIAN_POINT ( 'NONE',  ( 4.846305138012901637, 0.9798207982155520135, -1.642033262021398654 ) ) ;
#135806 = AXIS2_PLACEMENT_3D ( 'NONE', #45725, #39052, #18517 ) ;
#135807 = CARTESIAN_POINT ( 'NONE',  ( 11.84668730067608777, 10.09365272245202938, 1.399999999999998579 ) ) ;
#135808 = AXIS2_PLACEMENT_3D ( 'NONE', #34851, #67334, #115123 ) ;
#135809 = CARTESIAN_POINT ( 'NONE',  ( -4.288456660624211381, 3.897620947016656956, 1.214306433183764966E-14 ) ) ;
#135810 = CARTESIAN_POINT ( 'NONE',  ( -0.1056357528139931640, -1.757099710744941312, -0.4406103525058014392 ) ) ;
#135812 = CARTESIAN_POINT ( 'NONE',  ( 0.5322733027907312620, 0.5591794568308214863, 1.832249074504808783 ) ) ;
#135811 = CARTESIAN_POINT ( 'NONE',  ( 3.978581756310789252, 7.793429149004582612, 0.2401044915457872797 ) ) ;
#135813 = CARTESIAN_POINT ( 'NONE',  ( 2.137250951388528275, -0.09934309608320915363, -2.068088366144354318 ) ) ;
#135814 = CARTESIAN_POINT ( 'NONE',  ( 1.364683531249986537, 0.6760416670080884316, 0.7879004041258500513 ) ) ;
#135815 = CARTESIAN_POINT ( 'NONE',  ( 0.5144491564793505223, 1.361202580669124584, -1.426332009298651116 ) ) ;
#135816 = CARTESIAN_POINT ( 'NONE',  ( 3.316849939159485228, 1.650902842016691130, 0.7798126646740562995 ) ) ;
#135818 = CARTESIAN_POINT ( 'NONE',  ( 5.748548729368831545, 7.266256959964179529, 1.200940202139972435 ) ) ;
#135817 = CARTESIAN_POINT ( 'NONE',  ( 6.410767893487317792, 1.638320036227768783, -1.478771730184471389 ) ) ;
#135819 = CARTESIAN_POINT ( 'NONE',  ( 0.6823417656249882723, 1.926041667008083991, -1.181850606188749264 ) ) ;
#135820 = CARTESIAN_POINT ( 'NONE',  ( 4.141125080024585792, -0.1993089607698217136, -2.053009638179447371 ) ) ;
#135821 = CARTESIAN_POINT ( 'NONE',  ( -5.377780486114890124, 9.425827667109372143, 0.000000000000000000 ) ) ;
#135822 = CARTESIAN_POINT ( 'NONE',  ( 7.938462636001388795, 9.220293482545153907, -1.199719254218441611 ) ) ;
#135823 = CARTESIAN_POINT ( 'NONE',  ( 3.009347262367756848, 6.662655572737694598, -0.5494739808164535999 ) ) ;
#135824 = SHAPE_REPRESENTATION ( 'chamber', ( #200407 ), #110829 ) ;
#135825 = CARTESIAN_POINT ( 'NONE',  ( 5.518332215962025167, 6.396807992499198292, -1.199719254218445830 ) ) ;
#135827 = CARTESIAN_POINT ( 'NONE',  ( -1.500000000000011324, 3.670833333333356485, 0.8660254037844403729 ) ) ;
#135826 = CARTESIAN_POINT ( 'NONE',  ( 5.561587576256037835, 0.4139992630615954572, -2.064685544603379608 ) ) ;
#135828 = CARTESIAN_POINT ( 'NONE',  ( 6.549288556030710140, 1.803345607721940524, -1.016871928424132099 ) ) ;
#135829 = CARTESIAN_POINT ( 'NONE',  ( 1.364683531249986537, 1.467708333674748289, -0.7879004041258239610 ) ) ;
#135830 = CARTESIAN_POINT ( 'NONE',  ( 4.288457955665158750, -2.137403104576699242, -0.3218062170811594735 ) ) ;
#135831 = CARTESIAN_POINT ( 'NONE',  ( 4.020179312760450152, -2.014129041962478883, 0.1506293649766801690 ) ) ;
#135832 = CARTESIAN_POINT ( 'NONE',  ( 6.620655732516651071, -0.002413161512292844035, 2.173887093218453082 ) ) ;
#135835 = CARTESIAN_POINT ( 'NONE',  ( 5.341549334104188418, 7.254893527920112994, 1.443375672974062551 ) ) ;
#135834 = CARTESIAN_POINT ( 'NONE',  ( -1.642778471875000035, -2.967708332855374831, -2.845375778867859751 ) ) ;
#135833 = CARTESIAN_POINT ( 'NONE',  ( 11.48243876534946217, 11.29999999999999893, -3.200000000000001510 ) ) ;
#135836 = CARTESIAN_POINT ( 'NONE',  ( -5.661411662158206681, 8.762674818229999829, -1.199719254218452047 ) ) ;
#135837 = CARTESIAN_POINT ( 'NONE',  ( 1.991423064788412800, -0.4370762659771566527, 1.968445590580846893 ) ) ;
#135838 = CARTESIAN_POINT ( 'NONE',  ( -8.097244055859620815, 10.46987070330147063, -1.599625672291263179 ) ) ;
#135840 = FILL_AREA_STYLE_COLOUR ( '', #15590 ) ;
#135839 = CARTESIAN_POINT ( 'NONE',  ( -4.066556009095094737, 6.831733546331167695, 1.199719254218464037 ) ) ;
#135841 = FACE_OUTER_BOUND ( 'NONE', #114279, .T. ) ;
#135842 = DIRECTION ( 'NONE',  ( -1.000000000000000000, 7.771561172376097755E-16, 4.440892098500627148E-16 ) ) ;
#135843 = CARTESIAN_POINT ( 'NONE',  ( 1.734723475976807094E-15, -3.469446951953614189E-15, 0.2971265334020881110 ) ) ;
#135845 = CARTESIAN_POINT ( 'NONE',  ( 4.640250013031629095, 0.7743308749140092040, 1.862011755488258480 ) ) ;
#135844 = CARTESIAN_POINT ( 'NONE',  ( -7.388830529323428209, 8.683019041374528513, 1.082531754730549967 ) ) ;
#135846 = CARTESIAN_POINT ( 'NONE',  ( -0.7500000000000215383, 5.441666666666685082, 1.299038105676671107 ) ) ;
#135847 = CARTESIAN_POINT ( 'NONE',  ( 0.7676545703292583234, 0.8460830606174443158, 1.503042688352700829 ) ) ;
#135848 = CARTESIAN_POINT ( 'NONE',  ( 5.956828388357757298, 8.042995434541133193, 1.599625672291269396 ) ) ;
#135849 = MECHANICAL_DESIGN_GEOMETRIC_PRESENTATION_REPRESENTATION (  '', ( #208338 ), #142682 ) ;
#135851 = CARTESIAN_POINT ( 'NONE',  ( 3.615147460157889903, 7.348606074266929689, 0.4009180521483968196 ) ) ;
#135850 = CARTESIAN_POINT ( 'NONE',  ( 6.466876084038451822, 10.48851316477946582, 1.040834085586084257E-14 ) ) ;
#135852 = CARTESIAN_POINT ( 'NONE',  ( -11.13121356413584095, 7.259994163161730185, 4.367082668627133124 ) ) ;
#135853 = CARTESIAN_POINT ( 'NONE',  ( 5.430866635118035468, 0.1366067128489474591, 1.865587184704711632 ) ) ;
#135854 = CARTESIAN_POINT ( 'NONE',  ( 6.222908185483853494, 1.488938611106488841, -1.355157726057078404 ) ) ;
#135855 = FILL_AREA_STYLE_COLOUR ( '', #81701 ) ;
#135856 = CARTESIAN_POINT ( 'NONE',  ( -6.197485614778184271, 9.284131412999601096, 1.082531754730549967 ) ) ;
#135857 = ORIENTED_EDGE ( 'NONE', *, *, #189993, .T. ) ;
#135858 = CARTESIAN_POINT ( 'NONE',  ( 10.18181017373857067, 11.94149529319227909, 1.082531754730548412 ) ) ;
#135859 = CARTESIAN_POINT ( 'NONE',  ( 0.7379079170338508353, 2.013986002441462198, -0.1017714793793283723 ) ) ;
#135860 = CARTESIAN_POINT ( 'NONE',  ( 1.511653934090980034, -0.6084181080006717535, 1.706514628581125681 ) ) ;
#135861 = CARTESIAN_POINT ( 'NONE',  ( 7.201315867513990554, 8.430565262634994284, -1.199719254218452047 ) ) ;
#135862 = CARTESIAN_POINT ( 'NONE',  ( -1.843739406749240750, 8.499999999999996447, 0.7750000000000013545 ) ) ;
#135863 = CARTESIAN_POINT ( 'NONE',  ( 7.578644679914702031, 10.82520731233375955, 1.082531754730558626 ) ) ;
#135864 = EDGE_CURVE ( 'NONE', #1142, #205126, #136700, .T. ) ;
#135865 = CARTESIAN_POINT ( 'NONE',  ( 6.154511665599609493, 9.267681812253174556, 1.199719254218462483 ) ) ;
#135866 = AXIS2_PLACEMENT_3D ( 'NONE', #170938, #122295, #56134 ) ;
#135868 = CARTESIAN_POINT ( 'NONE',  ( 0.1631139290103194861, 1.786460926609586330, -0.6921882798058466291 ) ) ;
#135867 = CARTESIAN_POINT ( 'NONE',  ( -4.042302355168801320, 7.867769847672247074, 0.7998128361456341429 ) ) ;
#135869 = AXIS2_PLACEMENT_3D ( 'NONE', #130793, #114543, #180536 ) ;
#135870 = DIRECTION ( 'NONE',  ( -0.7592566023653004592, 0.6507913734559639396, -0.000000000000000000 ) ) ;
#135871 = CARTESIAN_POINT ( 'NONE',  ( -0.6823417656250246877, -1.136458332991911790, 1.181850606188755259 ) ) ;
#135873 = ORIENTED_EDGE ( 'NONE', *, *, #57116, .F. ) ;
#135872 = CARTESIAN_POINT ( 'NONE',  ( 3.795919822146273326, 5.451659097302528068, -1.443375672974051449 ) ) ;
#135874 = CARTESIAN_POINT ( 'NONE',  ( -4.620631424159025613, 4.285158171140619032, -0.7998128361456221525 ) ) ;
#135875 = CARTESIAN_POINT ( 'NONE',  ( 3.995124980148881288, 1.827535992889782523, -1.154293374375232828 ) ) ;
#135876 = CARTESIAN_POINT ( 'NONE',  ( -6.943184063974178422, 8.233374508458908281, -1.082531754730549967 ) ) ;
#135877 = CARTESIAN_POINT ( 'NONE',  ( 6.102578539926878598, 7.252668063737060855, -1.082531754730548412 ) ) ;
#135878 = CARTESIAN_POINT ( 'NONE',  ( 0.6508261300204335464, 2.090236094481153550, 0.3566229023672163878 ) ) ;
#135879 = CARTESIAN_POINT ( 'NONE',  ( 6.792070425361753649, -0.7769146798779454910, 1.650438213995283565 ) ) ;
#135880 = VECTOR ( 'NONE', #12080, 1000.000000000000000 ) ;
#135881 = CARTESIAN_POINT ( 'NONE',  ( 2.020718154849282744, 1.838011538856450855, 0.7131330410372925810 ) ) ;
#135882 = CARTESIAN_POINT ( 'NONE',  ( 4.183787391381143195, 1.853651273288700718, -0.4697857328580385960 ) ) ;
#135883 = EDGE_LOOP ( 'NONE', ( #186439, #153189, #80453, #138168 ) ) ;
#135884 = CARTESIAN_POINT ( 'NONE',  ( 9.499700864329909678, -7.154544010627095219, 0.07538891330675548397 ) ) ;
#135885 = CARTESIAN_POINT ( 'NONE',  ( 6.144967554776202157, -0.2872888210109864060, -1.948340736549762697 ) ) ;
#135887 = B_SPLINE_CURVE_WITH_KNOTS ( 'NONE', 3,
 ( #68090, #199161, #80103, #100620, #147257, #212224, #130014, #198110, #196005, #179755, #97448, #163504, #166695, #49740, #33489, #18286, #84372, #2021, #15088 ),
 .UNSPECIFIED., .F., .F.,
 ( 4, 3, 3, 3, 3, 3, 4 ),
 ( 0.000000000000000000, 4.552787399504409541E-05, 9.164501444053858924E-05, 0.0001336247809766599628, 0.0001748474261958555187, 0.0002334031072667163169, 0.0002737127687883810032 ),
 .UNSPECIFIED. ) ;
#135886 = CARTESIAN_POINT ( 'NONE',  ( 0.6209105903263291149, -1.844282116485985501, 0.6082893332694323529 ) ) ;
#135888 = EDGE_LOOP ( 'NONE', ( #123974, #70919, #107507, #96639, #82573 ) ) ;
#135889 = CARTESIAN_POINT ( 'NONE',  ( -5.309953438407606363, 6.223975762010839574, 1.199719254218452935 ) ) ;
#135890 = CARTESIAN_POINT ( 'NONE',  ( -3.688700311369816909, 6.461178242310183784, -1.199719254218450271 ) ) ;
#135892 = CARTESIAN_POINT ( 'NONE',  ( 6.007671464186825183, 8.102312356341712984, 1.443375672974064550 ) ) ;
#135891 = CARTESIAN_POINT ( 'NONE',  ( 7.416473721875251890, 8.611306416064660851, 1.199719254218462483 ) ) ;
#135894 = ORIENTED_EDGE ( 'NONE', *, *, #117909, .F. ) ;
#135893 = CARTESIAN_POINT ( 'NONE',  ( 5.461546741811521777, -1.510119879425949385, -1.173092037529008369 ) ) ;
#135895 = CARTESIAN_POINT ( 'NONE',  ( 1.307976841356368602, -0.5351398426680589182, 2.140771676462468687 ) ) ;
#135896 = CARTESIAN_POINT ( 'NONE',  ( 1.598423149420390210, 8.713846000021385763, 2.499999999999967581 ) ) ;
#135897 = CARTESIAN_POINT ( 'NONE',  ( 0.3637282827039616251, 0.5997036651611362679, -1.815894722023647656 ) ) ;
#135899 =( BOUNDED_CURVE ( )  B_SPLINE_CURVE ( 3, ( #26364, #55670, #121826, #158518 ),
 .UNSPECIFIED., .F., .T. ) 
 B_SPLINE_CURVE_WITH_KNOTS ( ( 4, 4 ),
 ( 0.000000000000000000, 0.4999999999999988898 ),
 .UNSPECIFIED. ) 
 CURVE ( )  GEOMETRIC_REPRESENTATION_ITEM ( )  RATIONAL_B_SPLINE_CURVE ( ( 1.000000000000000444, 0.3333333333333349802, 0.3333333333333334814, 0.9999999999999990008 ) ) 
 REPRESENTATION_ITEM ( '' )  );
#135898 = CARTESIAN_POINT ( 'NONE',  ( -0.02319159430949970999, 2.891346550825595774, -2.299931007135449512 ) ) ;
#135900 = DIRECTION ( 'NONE',  ( -0.000000000000000000, -1.000000000000000000, -0.000000000000000000 ) ) ;
#135901 = CARTESIAN_POINT ( 'NONE',  ( -6.400381488218095605, -6.708819892820500286, -7.008396152629720710 ) ) ;
#135902 = CARTESIAN_POINT ( 'NONE',  ( 2.822784111170244525, -1.429543836668966561, 1.497820115680066122 ) ) ;
#135903 = CARTESIAN_POINT ( 'NONE',  ( -4.252453736180621391, 8.112946458852704268, -0.7998128361456281477 ) ) ;
#135904 = CARTESIAN_POINT ( 'NONE',  ( -4.789308618567226006, 8.160042084799258078, 0.7984581689710170682 ) ) ;
#135906 = CARTESIAN_POINT ( 'NONE',  ( 0.08116279290028630133, -0.1557560750096824431, -2.127278773206460638 ) ) ;
#135905 = CARTESIAN_POINT ( 'NONE',  ( -4.790108344329849110, 4.482881244673243337, 0.7998128361456341429 ) ) ;
#135907 = CARTESIAN_POINT ( 'NONE',  ( -3.416291520519271874, 6.929497840673697340, 1.040834085586084257E-14 ) ) ;
#135908 = CARTESIAN_POINT ( 'NONE',  ( -0.6125000000000296874, 1.020833334016133076, -1.060881119635955327 ) ) ;
#135909 = CARTESIAN_POINT ( 'NONE',  ( 0.6823417656249969321, 13.08854166700806942, -1.181850606188757036 ) ) ;
#135910 = CARTESIAN_POINT ( 'NONE',  ( -6.252245114557387851, 7.323316050852266557, -1.199719254218453823 ) ) ;
#135911 = CARTESIAN_POINT ( 'NONE',  ( 5.801316117833412278, 1.158123311926442911, -1.290955512118051818 ) ) ;
#135912 = CARTESIAN_POINT ( 'NONE',  ( -3.253066792275140173, 5.882662793374543675, 1.199719254218462483 ) ) ;
#135913 = CARTESIAN_POINT ( 'NONE',  ( 3.133707330959301096, 1.967300496787489639, -0.6450458050009516553 ) ) ;
#135914 = CARTESIAN_POINT ( 'NONE',  ( 4.780926590999498238, 1.759528625808198354, -1.177310133890494548 ) ) ;
#135915 = CARTESIAN_POINT ( 'NONE',  ( 6.311484202361478779, 7.322151976631905868, -1.199719254218446718 ) ) ;
#135916 = CARTESIAN_POINT ( 'NONE',  ( 1.364683531249990311, 5.134375000341417916, 1.214306433183764966E-14 ) ) ;
#135917 = CARTESIAN_POINT ( 'NONE',  ( 2.782036810173736718, -1.130008284276774022, -1.612816519099938173 ) ) ;
#135918 = CARTESIAN_POINT ( 'NONE',  ( 0.6680393924826667496, 1.910109291395128972, -0.09634788558426229943 ) ) ;
#135919 = CARTESIAN_POINT ( 'NONE',  ( 5.156304180611417820, -1.663069175626085139, 1.577778581399520652 ) ) ;
#135920 = CARTESIAN_POINT ( 'NONE',  ( 3.387140609607977026, 1.650079954178599539, -0.7815607168924765258 ) ) ;
#135921 = CARTESIAN_POINT ( 'NONE',  ( 5.876533236880477240, 5.820653295974182129, 0.7998128361456352531 ) ) ;
#135923 = EDGE_CURVE ( 'NONE', #126346, #72572, #108276, .T. ) ;
#135922 = CARTESIAN_POINT ( 'NONE',  ( 4.460269348771534581, 8.147471973634706544, -0.7216878364870207285 ) ) ;
#135924 = CARTESIAN_POINT ( 'NONE',  ( -6.398558430645608475, 9.552403038140164782, -1.199719254218440723 ) ) ;
#135925 = B_SPLINE_CURVE_WITH_KNOTS ( 'NONE', 3,
 ( #205689, #142877, #26938, #171065 ),
 .UNSPECIFIED., .F., .F.,
 ( 4, 4 ),
 ( 0.000000000000000000, 0.0002909236271752537947 ),
 .UNSPECIFIED. ) ;
#135926 = CARTESIAN_POINT ( 'NONE',  ( 4.447525235540350508, -1.838889683631849348, 0.8198632543043646859 ) ) ;
#135927 = CARTESIAN_POINT ( 'NONE',  ( 2.782025223480470544, -1.125517505138178942, -1.606590762409945583 ) ) ;
#135928 = CARTESIAN_POINT ( 'NONE',  ( -6.021792782764022078, 10.17717534653336209, -0.7998128361456291469 ) ) ;
#135929 = CARTESIAN_POINT ( 'NONE',  ( -3.913499895838973508, 7.717500311787445000, 1.040834085586084257E-14 ) ) ;
#135930 = CARTESIAN_POINT ( 'NONE',  ( 0.1751657365761704888, 2.870293503558702497, -2.532510806204853804 ) ) ;
#135932 = CARTESIAN_POINT ( 'NONE',  ( 5.647242114940491220, -1.397150190615953358, -1.086277386216354168 ) ) ;
#135931 = CARTESIAN_POINT ( 'NONE',  ( 6.703094305332148117, -0.4564761572844484028, 2.047479069123214757 ) ) ;
#135933 = DIRECTION ( 'NONE',  ( 1.000000000000000000, 0.000000000000000000, 0.000000000000000000 ) ) ;
#135934 = CARTESIAN_POINT ( 'NONE',  ( 2.431793384409334902, 1.031818167245980744, -1.933333044699904857 ) ) ;
#135935 = CARTESIAN_POINT ( 'NONE',  ( 0.3623613221122607420, 0.1732436440316066917, -1.731762550003753898 ) ) ;
#135936 = CARTESIAN_POINT ( 'NONE',  ( 6.238723240582662477, 10.43026088065513513, -0.7998128361456291469 ) ) ;
#135937 = CARTESIAN_POINT ( 'NONE',  ( 0.2333690889706820926, 2.873202992247088083, -2.541887414127189881 ) ) ;
#135938 = CARTESIAN_POINT ( 'NONE',  ( 0.06452196833307657919, -1.538014849765593439, -0.7809378474108348289 ) ) ;
#135939 = CARTESIAN_POINT ( 'NONE',  ( 0.4217922253725381321, 0.8825364984147118230, 2.122365683989856588 ) ) ;
#135941 = EDGE_CURVE ( 'NONE', #152913, #16328, #164353, .T. ) ;
#135940 = CARTESIAN_POINT ( 'NONE',  ( 0.5916818631664167993, -0.7834642122952638621, 2.046923429677327100 ) ) ;
#135942 = CARTESIAN_POINT ( 'NONE',  ( 6.766931417284230754, -1.733354565069046505, 0.04740994324908299334 ) ) ;
#135943 = CARTESIAN_POINT ( 'NONE',  ( 2.772332522587173997, 1.181257105606844160, 1.863944272329665086 ) ) ;
#135944 = AXIS2_PLACEMENT_3D ( 'NONE', #54045, #106044, #89771 ) ;
#135945 = CARTESIAN_POINT ( 'NONE',  ( 0.3917816989358015034, -1.985425474602352525, 0.8787674391965931697 ) ) ;
#135946 = CARTESIAN_POINT ( 'NONE',  ( 1.499999999999990896, 4.025000000000021672, 1.214306433183764966E-14 ) ) ;
#135947 = CARTESIAN_POINT ( 'NONE',  ( 0.6204977360529799757, 2.087120111646578291, 0.3555802741468729877 ) ) ;
#135948 = VECTOR ( 'NONE', #1044, 1000.000000000000000 ) ;
#135949 = CARTESIAN_POINT ( 'NONE',  ( 6.620655732516624425, 7.629137130509072051, 2.773739711112707784 ) ) ;
#135950 = CARTESIAN_POINT ( 'NONE',  ( 5.297847195631281814, -0.6933188941696236673, 1.797466220796402725 ) ) ;
#135951 = ORIENTED_EDGE ( 'NONE', *, *, #55163, .F. ) ;
#135953 = CARTESIAN_POINT ( 'NONE',  ( -1.402160292154681736E-14, -0.7406249996585823059, -1.575800808251665908 ) ) ;
#135952 = CARTESIAN_POINT ( 'NONE',  ( 1.101600182630409819, -0.5506920761103645257, 2.225148091679912454 ) ) ;
#135954 = CARTESIAN_POINT ( 'NONE',  ( 3.602716132929354664, 5.226254793216122074, 1.599625672291267398 ) ) ;
#135955 = CARTESIAN_POINT ( 'NONE',  ( 4.873266149108180123, 7.772895376346490970, 1.199719254218462483 ) ) ;
#135956 = CARTESIAN_POINT ( 'NONE',  ( 3.246955274364712540, 2.167573551356954731, 0.4849624922091085866 ) ) ;
#135957 = CARTESIAN_POINT ( 'NONE',  ( -7.049876689426106680, 9.247942109129029475, -1.443375672974059665 ) ) ;
#135958 = FILL_AREA_STYLE_COLOUR ( '', #184331 ) ;
#135959 = CARTESIAN_POINT ( 'NONE',  ( 5.829642864196162400, 7.824335979694092558, 1.443375672974062551 ) ) ;
#135960 = CARTESIAN_POINT ( 'NONE',  ( -8.825994812371996900, 9.399341490629888440, 0.7216878364870438212 ) ) ;
#135961 = CARTESIAN_POINT ( 'NONE',  ( 5.234856708652227297, 7.200695141551334721, 1.443375672974065660 ) ) ;
#135962 = CARTESIAN_POINT ( 'NONE',  ( 1.547500230860882287, -1.423960469535384465, 1.427938386157491246 ) ) ;
#135964 = CARTESIAN_POINT ( 'NONE',  ( 1.147418581349904265, 1.820775857560010369, -0.9689367605143526241 ) ) ;
#135963 = CARTESIAN_POINT ( 'NONE',  ( 8.426556166093362776, 9.789735934319136135, -1.199719254218446718 ) ) ;
#135965 = CARTESIAN_POINT ( 'NONE',  ( 7.010974831598141499, 7.352094523052197239, -0.7216878364870317197 ) ) ;
#135966 = CARTESIAN_POINT ( 'NONE',  ( 0.06366010765614799061, -1.203631707120488947, 1.393476991864414760 ) ) ;
#135967 = EDGE_CURVE ( 'NONE', #172406, #187025, #60448, .T. ) ;
#135968 = CARTESIAN_POINT ( 'NONE',  ( -1.364683531250012516, 2.988541667008091096, -0.7879004041258289570 ) ) ;
#135969 = CARTESIAN_POINT ( 'NONE',  ( 2.284116761108864413, -1.734514481284253007, -0.3503773294724100706 ) ) ;
#135970 = CARTESIAN_POINT ( 'NONE',  ( 1.811172873341511336, 1.158687402475454098, -1.650082692374904125 ) ) ;
#135971 = CARTESIAN_POINT ( 'NONE',  ( 0.08126746489400815676, -0.8690269180096841239, 1.623235155968821841 ) ) ;
#135972 = CARTESIAN_POINT ( 'NONE',  ( 5.653944246587851552, 0.9260977375703757231, 2.097164529332084637 ) ) ;
#135973 = CARTESIAN_POINT ( 'NONE',  ( 2.941158370608713213, 0.6622022323767087215, -1.718108305994885177 ) ) ;
#135974 = EDGE_CURVE ( 'NONE', #193311, #99811, #205785, .T. ) ;
#135975 = CARTESIAN_POINT ( 'NONE',  ( 8.097244055859613709, 10.46987070330147063, -1.599625672291262513 ) ) ;
#135976 = CARTESIAN_POINT ( 'NONE',  ( 3.768406797884563897, -1.226484811506942441, 1.352366043108324201 ) ) ;
#135977 = CARTESIAN_POINT ( 'NONE',  ( 5.186172726741035355, 1.650080556555008293, 1.158690440749516881 ) ) ;
#135978 = CARTESIAN_POINT ( 'NONE',  ( -8.666686507633592385, 11.13422023037111330, 1.599625672291269396 ) ) ;
#135980 = CARTESIAN_POINT ( 'NONE',  ( -5.908321080505254841, 10.11506803722328129, 0.7998128361456291469 ) ) ;
#135979 = CARTESIAN_POINT ( 'NONE',  ( 3.467884472470097457, 2.207893551020873257, -0.4935151710872084929 ) ) ;
#135981 = CARTESIAN_POINT ( 'NONE',  ( 6.036178822307518566, 1.040974378708346526, -1.830621892639591630 ) ) ;
#135982 = SURFACE_STYLE_USAGE ( .BOTH. , #151170 ) ;
#135983 = CARTESIAN_POINT ( 'NONE',  ( 3.824723168590526523, -1.392635068473629500, 1.532133406949770960 ) ) ;
#135984 = CARTESIAN_POINT ( 'NONE',  ( 3.297657676621871925, 4.870353260857385180, 1.599625672291267398 ) ) ;
#135985 = CARTESIAN_POINT ( 'NONE',  ( 0.6801582343749674742, 1.755208333674734833, 1.178068619123803451 ) ) ;
#135986 = CARTESIAN_POINT ( 'NONE',  ( 5.444028431581452665, -1.345373016635186714, -1.639009079359869725 ) ) ;
#135987 = SHAPE_DEFINITION_REPRESENTATION ( #133366, #141543 ) ;
#135989 = CARTESIAN_POINT ( 'NONE',  ( 2.631371740967450634, -1.797512724518410598, 0.6935160474876176373 ) ) ;
#135988 = CARTESIAN_POINT ( 'NONE',  ( -8.306341666666730461, 12.84248237775322643, 1.040834085586084257E-14 ) ) ;
#135990 = UNCERTAINTY_MEASURE_WITH_UNIT (LENGTH_MEASURE( 1.000000000000000082E-05 ), #89847, 'distance_accuracy_value', 'NONE');
#135991 = CARTESIAN_POINT ( 'NONE',  ( -10.59765138761703085, 11.29999999999998295, 3.303242380465396977 ) ) ;
#135992 = CARTESIAN_POINT ( 'NONE',  ( 6.649268376821393822, 1.715264285883275397, -0.9675598167100638580 ) ) ;
#135993 = CARTESIAN_POINT ( 'NONE',  ( 3.892599500454932304, 7.555466827257172113, 0.7216878364870257245 ) ) ;
#135994 = CARTESIAN_POINT ( 'NONE',  ( 5.702249273124194495, 6.094009171513759426, 0.7094654760324905496 ) ) ;
#135995 = CARTESIAN_POINT ( 'NONE',  ( -2.324999999999998845, 0.000000000000000000, -0.5000000000000004441 ) ) ;
#135996 = CARTESIAN_POINT ( 'NONE',  ( -2.927671105547157371, 5.503034492191895666, 1.199719254218462483 ) ) ;
#135997 = CARTESIAN_POINT ( 'NONE',  ( 0.6686063958157261178, 2.218491797483721051, -0.1167170572400257761 ) ) ;
#135998 = AXIS2_PLACEMENT_3D ( 'NONE', #93848, #92780, #10421 ) ;
#135999 = CARTESIAN_POINT ( 'NONE',  ( 3.223755556863156180, -2.030008631501342808, 0.5602397303039460263 ) ) ;
#136000 = CARTESIAN_POINT ( 'NONE',  ( -7.262327558775498737, 8.501745569106741840, 1.199719254218452047 ) ) ;
#136001 = CARTESIAN_POINT ( 'NONE',  ( 7.775764792637399836, 9.030479331953833011, -1.199719254218441611 ) ) ;
#136002 = CARTESIAN_POINT ( 'NONE',  ( 0.9943274703284404881, 1.832596168249778446, 0.3232805840463324198 ) ) ;
#136003 = CARTESIAN_POINT ( 'NONE',  ( 6.962275575817444384, 8.081408578997208991, -1.199719254218446718 ) ) ;
#136004 = CARTESIAN_POINT ( 'NONE',  ( 4.578903193113299963, 6.365139696764064325, 1.599625672291267398 ) ) ;
#136005 = CARTESIAN_POINT ( 'NONE',  ( -6.455090533882201775, 8.624301270986276080, -1.443375672974066548 ) ) ;
#136006 = CARTESIAN_POINT ( 'NONE',  ( -7.700668062882078502, 9.046829497192987901, -1.082531754730543971 ) ) ;
#136007 = CARTESIAN_POINT ( 'NONE',  ( 1.213308285724056690, 1.730450836393576886, -1.225479750871574458 ) ) ;
#136008 = CARTESIAN_POINT ( 'NONE',  ( -7.045397100956844127, 8.248660034984974132, -1.199719254218452047 ) ) ;
#136010 = CARTESIAN_POINT ( 'NONE',  ( 4.176187491914356897, -1.006606191838583131, -1.683785057063936552 ) ) ;
#136009 = CARTESIAN_POINT ( 'NONE',  ( -2.954552044183079750E-14, 1.312499999999982236, 1.414508159514555441 ) ) ;
#136011 = CARTESIAN_POINT ( 'NONE',  ( 2.448304249002517974, 2.161202317112873139, 0.05382173394478938222 ) ) ;
#136012 = CARTESIAN_POINT ( 'NONE',  ( 1.610644152589552958, -0.2245515952020246953, 1.827417025815617935 ) ) ;
#136014 = CARTESIAN_POINT ( 'NONE',  ( -4.067982317475717480, 7.550107770606433455, 0.4684429539664070608 ) ) ;
#136013 = CARTESIAN_POINT ( 'NONE',  ( -5.157951095356222204, 4.982307464195829816, 0.000000000000000000 ) ) ;
#136015 = CARTESIAN_POINT ( 'NONE',  ( 4.663825473582838832, -1.133750416550326046, 1.320446528551111776 ) ) ;
#136016 = CARTESIAN_POINT ( 'NONE',  ( -8.065673753978270355, 13.99999996918362832, -8.613976771946813216 ) ) ;
#136017 = CARTESIAN_POINT ( 'NONE',  ( 4.690757960648213931, 8.416375354157496602, 0.7216878364870438212 ) ) ;
#136018 = CARTESIAN_POINT ( 'NONE',  ( -10.78227258717170578, 6.269840026405313793, 4.500979083849748541 ) ) ;
#136019 = CARTESIAN_POINT ( 'NONE',  ( 1.376082401959723089, 1.288024388040419632, 1.735935173841046675 ) ) ;
#136020 = CARTESIAN_POINT ( 'NONE',  ( 3.198592129611950607, -1.351947076146834403, -1.495823048609262518 ) ) ;
#136021 = CARTESIAN_POINT ( 'NONE',  ( -8.622622508166983835, 13.00355065959610279, 1.040834085586084257E-14 ) ) ;
#136023 = AXIS2_PLACEMENT_3D ( 'NONE', #115745, #36564, #150340 ) ;
#136022 = CARTESIAN_POINT ( 'NONE',  ( 0.9190830904215805397, 1.997680973563022544, 0.8264451868333838602 ) ) ;
#136024 = CARTESIAN_POINT ( 'NONE',  ( 3.713711766734467012, -1.942503170530969436, 0.3358077238896309824 ) ) ;
#136025 = CARTESIAN_POINT ( 'NONE',  ( 6.509000000000048303, 0.5949247728001515467, 1.954148248227548290 ) ) ;
#136026 = CARTESIAN_POINT ( 'NONE',  ( 2.841277192181762334, 0.6965426786647112012, -1.813031058463436818 ) ) ;
#136029 = ORIENTED_EDGE ( 'NONE', *, *, #167459, .T. ) ;
#136028 = CARTESIAN_POINT ( 'NONE',  ( -3.024877669624710386, 6.543124691288523920, 0.000000000000000000 ) ) ;
#136027 = CARTESIAN_POINT ( 'NONE',  ( -11.04978080397792972, 9.991554750122867645, 1.057339094031728211 ) ) ;
#136030 = CARTESIAN_POINT ( 'NONE',  ( -5.926322542504884439, 6.086666852443364029, -0.7216878364870338292 ) ) ;
#136031 = CARTESIAN_POINT ( 'NONE',  ( -0.1108833634136975610, 0.7331455517814323697, -1.980187714524218823 ) ) ;
#136032 = CARTESIAN_POINT ( 'NONE',  ( 4.115782150200256950, 6.959440387612411349, 1.199719254218452047 ) ) ;
#136033 = CARTESIAN_POINT ( 'NONE',  ( -5.517242166118370150, 5.401480380085008193, 0.7998128361456281477 ) ) ;
#136035 = ORIENTED_EDGE ( 'NONE', *, *, #160143, .T. ) ;
#136034 = CARTESIAN_POINT ( 'NONE',  ( -6.282224075085783177, 8.422623735723785643, 1.599625672291269396 ) ) ;
#136036 = CARTESIAN_POINT ( 'NONE',  ( -7.958272981097355370, 12.22847621134819285, 0.7216878364870458196 ) ) ;
#136037 = CARTESIAN_POINT ( 'NONE',  ( 6.563506341781633502, 0.4036857245812221495, -2.271876217655709240 ) ) ;
#136038 = DIRECTION ( 'NONE',  ( 1.000000000000000000, 0.000000000000000000, -3.706092522800016599E-15 ) ) ;
#136039 = VECTOR ( 'NONE', #174952, 1000.000000000000000 ) ;
#136040 = CARTESIAN_POINT ( 'NONE',  ( 4.557442073745519018, 1.573120015848201492, 1.171846803954358363 ) ) ;
#136041 = CARTESIAN_POINT ( 'NONE',  ( 8.796542737168120851, 9.157054702984622097, -0.7998128361456211532 ) ) ;
#136042 = CARTESIAN_POINT ( 'NONE',  ( 1.371720446232262081, -0.2986288616722633793, -1.994071132515719880 ) ) ;
#136043 = ORIENTED_EDGE ( 'NONE', *, *, #81270, .F. ) ;
#136044 = CARTESIAN_POINT ( 'NONE',  ( 2.958335891534333850, -1.257395014299323988, 1.703445231074371291 ) ) ;
#136045 = CARTESIAN_POINT ( 'NONE',  ( -1.201851678989727383E-14, 1.993750000682816381, 1.732050807568877637 ) ) ;
#136047 = CARTESIAN_POINT ( 'NONE',  ( -4.882907879216086933, 8.848476292394087395, -0.7998128361456281477 ) ) ;
#136046 =( NAMED_UNIT ( * ) SI_UNIT ( $, .STERADIAN. ) SOLID_ANGLE_UNIT ( ) );
#136048 = CARTESIAN_POINT ( 'NONE',  ( 3.679498877186979211, -0.9061679144062879665, 1.602619060095414216 ) ) ;
#136049 = VERTEX_POINT ( 'NONE', #42161 ) ;
#136050 = CARTESIAN_POINT ( 'NONE',  ( -8.158255747121117452, 10.54105100977322174, 1.599625672291295375 ) ) ;
#136051 = DIRECTION ( 'NONE',  ( 1.276756478318931402E-15, -1.000000000000000000, 0.000000000000000000 ) ) ;
#136052 = CARTESIAN_POINT ( 'NONE',  ( 3.621431001533811589, 1.820626359085864454, 1.087046460333654485 ) ) ;
#136053 = CARTESIAN_POINT ( 'NONE',  ( -1.001543065824772872E-14, 5.493750000682816825, 1.732050807568877637 ) ) ;
#136054 = CARTESIAN_POINT ( 'NONE',  ( 5.764187864104357573, 9.876636274763768597, 1.040834085586084257E-14 ) ) ;
#136055 = CARTESIAN_POINT ( 'NONE',  ( 5.044241359090890775, 2.054987069614383266, 0.1556004420267612098 ) ) ;
#136057 = CARTESIAN_POINT ( 'NONE',  ( 2.102840161960460197, -0.4018910908503615653, 1.796694178532439956 ) ) ;
#136056 = CARTESIAN_POINT ( 'NONE',  ( -6.795661308947694934, 8.951357498570873261, -1.599625672291263179 ) ) ;
#136058 = CARTESIAN_POINT ( 'NONE',  ( 9.260382613333817403, 10.76253345609967660, -1.199719254218446718 ) ) ;
#136059 = CARTESIAN_POINT ( 'NONE',  ( 1.364683531249990311, 5.613541667008087543, 0.7879004041258500513 ) ) ;
#136060 = SURFACE_STYLE_FILL_AREA ( #139264 ) ;
#136061 = CARTESIAN_POINT ( 'NONE',  ( -6.933015448541747006, 9.181880338089085214, 1.599625672291269396 ) ) ;
#136062 = CARTESIAN_POINT ( 'NONE',  ( 3.475000000000000533, -1.502083332377415870, -2.006292185433951047 ) ) ;
#136063 = CARTESIAN_POINT ( 'NONE',  ( 2.438337523484556790, 1.039148161723329578, -1.946916322307743474 ) ) ;
#136064 = CARTESIAN_POINT ( 'NONE',  ( 3.532755146446086680, 2.206387722723508915, 0.4996636332569806549 ) ) ;
#136065 = CARTESIAN_POINT ( 'NONE',  ( -6.548225005720456515, 10.58342024007512983, 0.000000000000000000 ) ) ;
#136066 = CARTESIAN_POINT ( 'NONE',  ( 5.097853226644959435, 1.222535334948423813, 1.337041937662573288 ) ) ;
#136067 = CARTESIAN_POINT ( 'NONE',  ( 4.452287505575288407, -1.246817998045848697, 1.454578644467845017 ) ) ;
#136068 = CARTESIAN_POINT ( 'NONE',  ( -0.6823417656250212460, 4.113541667008085767, 1.181850606188767472 ) ) ;
#136069 = CARTESIAN_POINT ( 'NONE',  ( 3.871915168923282913, 1.094167467933440108, 1.639771958457488132 ) ) ;
#136070 = CARTESIAN_POINT ( 'NONE',  ( 4.645289301550183936, -1.446173438076237217, -1.186536486241091204 ) ) ;
#136071 = CARTESIAN_POINT ( 'NONE',  ( 3.704037377190313673, -0.6708616879335957961, 2.208036538417802230 ) ) ;
#136072 = CARTESIAN_POINT ( 'NONE',  ( 4.808966763405270406, -1.495079835775798838, 1.108065441546413288 ) ) ;
#136073 = CARTESIAN_POINT ( 'NONE',  ( 1.364683531249988535, 5.155208333674749177, -0.7879004041258300672 ) ) ;
#136074 = SPHERICAL_SURFACE ( 'NONE', #44683, 0.08000000000000000167 ) ;
#136076 = CARTESIAN_POINT ( 'NONE',  ( 1.805437418371407254, 1.751699828856004837, 1.168899091633753384 ) ) ;
#136075 = CARTESIAN_POINT ( 'NONE',  ( -4.582292731294565158, 4.448355729372827305, 1.214306433183764966E-14 ) ) ;
#136077 = CARTESIAN_POINT ( 'NONE',  ( 7.886038904643079661, 12.35212915539230139, -0.7998128361456352531 ) ) ;
#136079 = CARTESIAN_POINT ( 'NONE',  ( -1.258302072444749564, 2.865146149352002514, -0.7749999999999892530 ) ) ;
#136078 = CARTESIAN_POINT ( 'NONE',  ( -1.364683531250012516, 4.801041667008083991, -0.7879004041258300672 ) ) ;
#136080 = CARTESIAN_POINT ( 'NONE',  ( 3.094099843433151253, 1.348383549611749332, 1.636666742212993686 ) ) ;
#136081 = CARTESIAN_POINT ( 'NONE',  ( -9.617648866954029430, -9.063431457505044975, 0.6035590660249372519 ) ) ;
#136082 = CARTESIAN_POINT ( 'NONE',  ( 0.4221360882172753293, -2.009675015244154483, 0.2020994116621494530 ) ) ;
#136083 = CARTESIAN_POINT ( 'NONE',  ( 1.364683531249986537, 0.4052083336747511200, -0.7879004041258309554 ) ) ;
#136084 = CARTESIAN_POINT ( 'NONE',  ( -3.145128448690317935, 5.652771709238564313, -1.082531754730549967 ) ) ;
#136085 = CARTESIAN_POINT ( 'NONE',  ( 5.684946482831785275, 5.526859072925533134, -0.7998128361456231517 ) ) ;
#136086 = VERTEX_POINT ( 'NONE', #60508 ) ;
#136087 = CARTESIAN_POINT ( 'NONE',  ( 2.091316376603330252, 1.881825464268515269, -1.063406855978922039 ) ) ;
#136088 = DIRECTION ( 'NONE',  ( 0.000000000000000000, 0.000000000000000000, -1.000000000000000000 ) ) ;
#136091 = DIRECTION ( 'NONE',  ( -1.000000000000000000, 0.000000000000000000, 1.665334536937734811E-16 ) ) ;
#136090 = CARTESIAN_POINT ( 'NONE',  ( -5.381422217466647062, 4.322449550048936828, -2.440471613107404902 ) ) ;
#136089 = CARTESIAN_POINT ( 'NONE',  ( 5.520104819419390907, 6.469152373191302985, 1.199719254218452935 ) ) ;
#136092 =( BOUNDED_CURVE ( )  B_SPLINE_CURVE ( 2, ( #176271, #96100, #129730, #78745, #195714, #27873, #60365 ),
 .UNSPECIFIED., .F., .T. ) 
 B_SPLINE_CURVE_WITH_KNOTS ( ( 3, 2, 2, 3 ),
 ( 0.3250000000000001776, 0.3333333333333334814, 0.3416666666666667851, 0.3500000000000000888 ),
 .UNSPECIFIED. ) 
 CURVE ( )  GEOMETRIC_REPRESENTATION_ITEM ( )  RATIONAL_B_SPLINE_CURVE ( ( 0.9999999999999973355, 0.8660254037844413721, 1.000000000000000000, 0.8660254037844387076, 1.000000000000000000, 0.8660254037844369313, 1.000000000000001776 ) ) 
 REPRESENTATION_ITEM ( '' )  );
#136093 = DIRECTION ( 'NONE',  ( -0.1775819850076547912, 0.000000000000000000, -0.9841060098387475197 ) ) ;
#136094 = CARTESIAN_POINT ( 'NONE',  ( 6.403528931544730796, -1.954801056786956259, 0.4946215565981848528 ) ) ;
#136095 = CARTESIAN_POINT ( 'NONE',  ( -7.036318535812428721, 11.15286269184909784, 0.000000000000000000 ) ) ;
#136096 = CARTESIAN_POINT ( 'NONE',  ( 6.515180868147061766, -2.027822497041928518, 0.5085933055150316795 ) ) ;
#136097 = CARTESIAN_POINT ( 'NONE',  ( 3.223391908310548028E-14, -7.616807913963251409, -10.09384657274512165 ) ) ;
#136099 = CARTESIAN_POINT ( 'NONE',  ( -0.6823417656250003738, 11.90104166700806054, 1.181850606188754593 ) ) ;
#136098 = CARTESIAN_POINT ( 'NONE',  ( 1.815646767810099149, -0.2761031220132881270, 2.245556248662975207 ) ) ;
#136100 = CARTESIAN_POINT ( 'NONE',  ( -7.147119532698295252, 11.49005655479003174, 0.000000000000000000 ) ) ;
#136101 = CARTESIAN_POINT ( 'NONE',  ( -3.917943204224913156, 7.514758138330285497, -0.7216878364870257245 ) ) ;
#136102 = CARTESIAN_POINT ( 'NONE',  ( -1.364683531250014514, 1.801041667008085767, -0.7879004041258289570 ) ) ;
#136103 = CARTESIAN_POINT ( 'NONE',  ( 0.7500000000000006661, 9.416666666666669627, -1.299038105676657340 ) ) ;
#136104 = EDGE_CURVE ( 'NONE', #183752, #34907, #23741, .T. ) ;
#136105 = CARTESIAN_POINT ( 'NONE',  ( -1.402160292154681736E-14, 9.062500000000003553, 1.732050807568881190 ) ) ;
#136106 = CARTESIAN_POINT ( 'NONE',  ( 3.615580125028591052, -1.699004861347377604, 0.2966152939984505466 ) ) ;
#136107 = CARTESIAN_POINT ( 'NONE',  ( 6.039231080244466199, 6.010467446565510130, 0.7998128361456352531 ) ) ;
#136108 = CARTESIAN_POINT ( 'NONE',  ( 2.161070758698178107, 0.3078950573750063313, -1.742579939182072657 ) ) ;
#136109 = CARTESIAN_POINT ( 'NONE',  ( 3.106110754726201240, -0.8138748988139458129, 1.841402425526596387 ) ) ;
#136110 = CARTESIAN_POINT ( 'NONE',  ( 4.840968367003476658, 0.3731960759543617723, 2.174832070070693568 ) ) ;
#136111 = AXIS2_PLACEMENT_3D ( 'NONE', #24402, #102481, #204209 ) ;
#136112 = ORIENTED_EDGE ( 'NONE', *, *, #113251, .F. ) ;
#136113 = CARTESIAN_POINT ( 'NONE',  ( 3.937764026144819685, -1.931520177269234306, 0.5904599756008358513 ) ) ;
#136114 = CARTESIAN_POINT ( 'NONE',  ( -7.370792787684826486, 8.628288336167626582, -1.199719254218452047 ) ) ;
#136116 = CARTESIAN_POINT ( 'NONE',  ( 4.200796113533305842, 1.844717850457804120, 0.8146114232021259838 ) ) ;
#136115 = CARTESIAN_POINT ( 'NONE',  ( 5.619825546450978315, -0.5151785252428126016, 2.056841324599982368 ) ) ;
#136118 = ORIENTED_EDGE ( 'NONE', *, *, #32262, .F. ) ;
#136117 = CARTESIAN_POINT ( 'NONE',  ( 4.218897050542698146, 1.396175630728054173, -1.154312599804697914 ) ) ;
#136119 = EDGE_CURVE ( 'NONE', #209973, #133641, #171160, .T. ) ;
#136120 = ORIENTED_EDGE ( 'NONE', *, *, #166530, .T. ) ;
#136121 = CARTESIAN_POINT ( 'NONE',  ( 1.305301652190330675, -0.4579020413679709689, 1.813615928118620380 ) ) ;
#136122 = EDGE_CURVE ( 'NONE', #21255, #67257, #183085, .T. ) ;
#136123 = CARTESIAN_POINT ( 'NONE',  ( -10.91804383151480629, -9.900000000000005684, 0.1905751639681794174 ) ) ;
#136124 = CARTESIAN_POINT ( 'NONE',  ( 6.147087800311862971, 0.1847020338378597137, 1.802040927518679281 ) ) ;
#136125 = CARTESIAN_POINT ( 'NONE',  ( -4.595387861177860245, 8.132925338238120361, 0.6295658974326902024 ) ) ;
#136126 = CARTESIAN_POINT ( 'NONE',  ( -10.24056286296518614, 5.004077596833054642, -7.476959758773280562 ) ) ;
#136127 = FILL_AREA_STYLE_COLOUR ( '', #118029 ) ;
#136128 = CARTESIAN_POINT ( 'NONE',  ( 1.364683531249988757, 2.446875000341415696, 1.214306433183764966E-14 ) ) ;
#136129 = CARTESIAN_POINT ( 'NONE',  ( 0.7207899753199145110, 1.446443371814851941, -1.251069288267861346 ) ) ;
#136130 = CARTESIAN_POINT ( 'NONE',  ( 4.407809338218622308, 8.156544971314787063, 0.000000000000000000 ) ) ;
#136131 = CARTESIAN_POINT ( 'NONE',  ( 1.469116868872882620, 1.728625619535430369, 0.9278086228877155950 ) ) ;
#136132 = CARTESIAN_POINT ( 'NONE',  ( 0.000000000000000000, 12.21999999999998288, 0.000000000000000000 ) ) ;
#136133 = CARTESIAN_POINT ( 'NONE',  ( -5.960744811863571968, 6.983232364376142698, 1.199719254218452935 ) ) ;
#136134 = CARTESIAN_POINT ( 'NONE',  ( 4.535463010148616192, -0.1012041512906610846, 2.118281909017679432 ) ) ;
#136136 = CARTESIAN_POINT ( 'NONE',  ( 10.96499746917716678, -5.350147675656132584, -0.1749484593404596611 ) ) ;
#136135 = CARTESIAN_POINT ( 'NONE',  ( 7.913155211870404493, 12.38376484715752213, 0.7998128361456462443 ) ) ;
#136137 = CARTESIAN_POINT ( 'NONE',  ( 5.764905551123544747, -1.781034818069273884, -0.8454043039353341671 ) ) ;
#136138 = CARTESIAN_POINT ( 'NONE',  ( -1.201851678989727383E-14, 0.8218750003414171390, 1.575800808251672791 ) ) ;
#136139 = CARTESIAN_POINT ( 'NONE',  ( 1.142838885277572825, 1.941394601512283602, 0.5327644489504842484 ) ) ;
#136140 = ORIENTED_EDGE ( 'NONE', *, *, #67115, .F. ) ;
#136141 = CARTESIAN_POINT ( 'NONE',  ( 0.9489988177146626569, -1.915858558953801749, -0.9014485902382618487 ) ) ;
#136142 = CARTESIAN_POINT ( 'NONE',  ( 11.79264299610848177, 6.877264176558675501, -1.951597671399909917 ) ) ;
#136143 = CARTESIAN_POINT ( 'NONE',  ( 2.664580169416390643, -0.7900844611210651180, -1.913877855911281234 ) ) ;
#136144 = CARTESIAN_POINT ( 'NONE',  ( 4.686278372178935392, 5.496354851410763409, 1.199719254218452047 ) ) ;
#136145 = CARTESIAN_POINT ( 'NONE',  ( 6.384963997392946844, 6.413822516572072807, 0.7998128361456352531 ) ) ;
#136147 = ORIENTED_EDGE ( 'NONE', *, *, #51899, .T. ) ;
#136146 = B_SPLINE_CURVE_WITH_KNOTS ( 'NONE', 3,
 ( #204625, #57340, #190519, #56276 ),
 .UNSPECIFIED., .F., .F.,
 ( 4, 4 ),
 ( 0.000000000000000000, 0.0004065497138311778428 ),
 .UNSPECIFIED. ) ;
#136149 = CARTESIAN_POINT ( 'NONE',  ( 3.981290663907289140, 7.796589541200495965, -0.7998128361456221525 ) ) ;
#136148 = CARTESIAN_POINT ( 'NONE',  ( 4.787105812777236125, 1.548788850919210702, 1.404477511574409920 ) ) ;
#136152 = ORIENTED_EDGE ( 'NONE', *, *, #35341, .T. ) ;
#136151 = CARTESIAN_POINT ( 'NONE',  ( 1.717148478332259254, 1.506203170942743030, 1.006022724715895045 ) ) ;
#136150 = CARTESIAN_POINT ( 'NONE',  ( 3.346530664597209714, 0.4423686283943834563, 1.771051422834311051 ) ) ;
#136153 = CARTESIAN_POINT ( 'NONE',  ( 6.639307388351803674, -1.973492857608965423, 0.9879489342229507143 ) ) ;
#136154 = PLANE ( 'NONE',  #33514 ) ;
#136155 = CARTESIAN_POINT ( 'NONE',  ( 8.642161254816231875, 12.08761591892186082, -8.327710695117993112 ) ) ;
#136156 = CARTESIAN_POINT ( 'NONE',  ( 4.823365732668142947, -0.1123398232194070118, 2.204042774474362254 ) ) ;
#136157 = CARTESIAN_POINT ( 'NONE',  ( 0.6823417656249969321, 9.338541667008065872, -1.181850606188757036 ) ) ;
#136158 = ORIENTED_EDGE ( 'NONE', *, *, #183636, .T. ) ;
#136159 = CARTESIAN_POINT ( 'NONE',  ( 3.791585636498477463, 1.799617611794877670, -0.6470144256675299799 ) ) ;
#136160 = CARTESIAN_POINT ( 'NONE',  ( -2.611917148927046295, 6.198987107056845858, 1.040834085586084257E-14 ) ) ;
#136161 = CARTESIAN_POINT ( 'NONE',  ( 9.108380270282433244, 9.520865158284665952, 1.040834085586084257E-14 ) ) ;
#136162 = CARTESIAN_POINT ( 'NONE',  ( 6.303194806757332458, -1.751150776259063457, 1.104182018118210262 ) ) ;
#136163 = CARTESIAN_POINT ( 'NONE',  ( -0.7500000000000006661, 10.23958333401612997, -1.299038105676657340 ) ) ;
#136164 = CARTESIAN_POINT ( 'NONE',  ( 5.917560222199001352, -1.216239291071326001, -1.822900893127032962 ) ) ;
#136165 = CARTESIAN_POINT ( 'NONE',  ( 4.936581118797800372, 8.100871430792054184, -1.059671831818540966 ) ) ;
#136166 = CARTESIAN_POINT ( 'NONE',  ( -3.518235019283448395, 15.44797960873222742, -11.43489012466130283 ) ) ;
#136167 = CARTESIAN_POINT ( 'NONE',  ( -0.9311234436981532525, -2.028130369558482471, 3.474999999999999201 ) ) ;
#136168 = CARTESIAN_POINT ( 'NONE',  ( 3.866346082213562685, -1.258301477641217803, 1.384200088751494251 ) ) ;
#136169 = CARTESIAN_POINT ( 'NONE',  ( -0.02319159430947541692, 2.051704324979522820, -2.228571760951563618 ) ) ;
#136170 = CARTESIAN_POINT ( 'NONE',  ( 10.56513397747884397, 9.840999034856560357, 3.405015282931167508 ) ) ;
#136171 = AXIS2_PLACEMENT_3D ( 'NONE', #130289, #213558, #62014 ) ;
#136172 = CARTESIAN_POINT ( 'NONE',  ( -7.158341918335454857, 10.33485409049125003, 1.082531754730549967 ) ) ;
#136173 = CARTESIAN_POINT ( 'NONE',  ( 3.573456005653643519, 6.326726552307992080, -1.199719254218453823 ) ) ;
#136174 = CARTESIAN_POINT ( 'NONE',  ( 5.341022448779654930, 8.318611059296550536, 1.199719254218462483 ) ) ;
#136175 = CARTESIAN_POINT ( 'NONE',  ( 6.807487347360918761, -1.659057770219806160, -1.238116672595261480 ) ) ;
#136176 = CARTESIAN_POINT ( 'NONE',  ( 0.8609541034889023337, -0.05231784723681161264, -2.015913592316537883 ) ) ;
#136177 = CIRCLE ( 'NONE', #4710, 0.1399999999999995137 ) ;
#136178 = CARTESIAN_POINT ( 'NONE',  ( -8.272446282632566650, 12.80293776304669962, 0.7998128361456481317 ) ) ;
#136179 = CARTESIAN_POINT ( 'NONE',  ( 4.857564175446106525, 8.889184981320973122, 0.7998128361456331437 ) ) ;
#136180 = DIRECTION ( 'NONE',  ( 0.000000000000000000, -1.000000000000000000, -0.000000000000000000 ) ) ;
#136181 = CARTESIAN_POINT ( 'NONE',  ( 1.183813618819636870, -0.9825931803647185436, 1.958887836816553429 ) ) ;
#136182 = CARTESIAN_POINT ( 'NONE',  ( 5.830640656690653678, 1.760721658632548037, 0.4824517239352192344 ) ) ;
#136183 = CARTESIAN_POINT ( 'NONE',  ( -2.774614992291035698, 6.388801257648172971, 1.040834085586084257E-14 ) ) ;
#136184 = CARTESIAN_POINT ( 'NONE',  ( 5.072158865288243668, 6.050511776658669127, 1.082531754730549078 ) ) ;
#136186 = EDGE_CURVE ( 'NONE', #125532, #159873, #105484, .T. ) ;
#136185 = CARTESIAN_POINT ( 'NONE',  ( 10.55910270694468345, 11.21337466772398095, 0.7998128361456462443 ) ) ;
#136187 = AXIS2_PLACEMENT_3D ( 'NONE', #168134, #203804, #202740 ) ;
#136188 = CARTESIAN_POINT ( 'NONE',  ( 2.706824224222692088, 6.309712028235118453, 0.7998128361456362523 ) ) ;
#136189 = CARTESIAN_POINT ( 'NONE',  ( 7.404161286838808920, 8.771181268467660885, -1.082531754730548412 ) ) ;
#136190 = ORIENTED_EDGE ( 'NONE', *, *, #207277, .F. ) ;
#136192 = CARTESIAN_POINT ( 'NONE',  ( 0.6979027206182022436, 1.353502529517286446, 1.490303647139071153 ) ) ;
#136191 = CARTESIAN_POINT ( 'NONE',  ( 3.298233973420101606, 1.449563003725433896, -1.135193286699177628 ) ) ;
#136193 = CARTESIAN_POINT ( 'NONE',  ( 2.144337281971959719, -0.1124944508365255252, -2.295720847718041746 ) ) ;
#136195 = CARTESIAN_POINT ( 'NONE',  ( 1.498636204049142773, 0.3563576638296832577, 1.826325547775342173 ) ) ;
#136194 = CARTESIAN_POINT ( 'NONE',  ( 5.192409644353875642, 5.160158794608717514, 1.040834085586084257E-14 ) ) ;
#136196 = CARTESIAN_POINT ( 'NONE',  ( 1.642778471875001811, -3.142708332855375986, 2.845375778867859751 ) ) ;
#136197 = CARTESIAN_POINT ( 'NONE',  ( -4.229253852459088137, 7.021547696922494808, 1.199719254218464037 ) ) ;
#136198 = PLANE ( 'NONE',  #116022 ) ;
#136199 = CARTESIAN_POINT ( 'NONE',  ( 3.972844611716894736, -1.413603510852480927, 1.288168406687495215 ) ) ;
#136200 = CARTESIAN_POINT ( 'NONE',  ( -7.797910906154257304, 12.24931315715533486, 0.000000000000000000 ) ) ;
#136201 = CARTESIAN_POINT ( 'NONE',  ( 6.365646016822680942, 6.829858545691475769, 0.5939985411197836740 ) ) ;
#136202 = CARTESIAN_POINT ( 'NONE',  ( -4.981695098378565945, 4.776675467721892332, -0.7998128361456362523 ) ) ;
#136204 = CARTESIAN_POINT ( 'NONE',  ( 2.395189659270926086, 1.444574673180216706, 1.188490415850687265 ) ) ;
#136203 = CARTESIAN_POINT ( 'NONE',  ( 4.124618644571789616, 0.1043759322204278750, 2.088280726629719197 ) ) ;
#136205 = CARTESIAN_POINT ( 'NONE',  ( 8.758204044748010730, 9.320252261735261001, 0.7216878364870438212 ) ) ;
#136206 = CARTESIAN_POINT ( 'NONE',  ( 1.364683531249988535, 4.967708333674756283, -0.7879004041258300672 ) ) ;
#136207 = CARTESIAN_POINT ( 'NONE',  ( 3.034399582073334489, -1.533639759443014894, 0.8228653360542650397 ) ) ;
#136208 = CARTESIAN_POINT ( 'NONE',  ( 5.684946482831785275, 5.526859072925533134, -0.7998128361456231517 ) ) ;
#136210 = FACE_OUTER_BOUND ( 'NONE', #186096, .T. ) ;
#136209 = CARTESIAN_POINT ( 'NONE',  ( 0.3282377607281186660, 1.176335450315366460, -1.225000000000014522 ) ) ;
#136211 = CARTESIAN_POINT ( 'NONE',  ( 3.527714679269139619, -1.028799902082434992, -1.384306889003545926 ) ) ;
#136212 = CARTESIAN_POINT ( 'NONE',  ( 3.491892070630482348, -2.189115664112693871, -0.1057334378413293807 ) ) ;
#136213 = FACE_OUTER_BOUND ( 'NONE', #119699, .T. ) ;
#136214 = CARTESIAN_POINT ( 'NONE',  ( 3.344746749068757019, -2.138148195731132351, -0.3758941404270431108 ) ) ;
#136215 = CARTESIAN_POINT ( 'NONE',  ( 2.455445036260803349, 0.4872311372507812655, -1.759406031448563557 ) ) ;
#136216 = CARTESIAN_POINT ( 'NONE',  ( 0.5144084716053355377, 0.7454083195421266073, 1.814826383214888983 ) ) ;
#136217 = CARTESIAN_POINT ( 'NONE',  ( 4.663340677796647071, 1.974402194736598837, -0.7651654921337573967 ) ) ;
#136218 = EDGE_LOOP ( 'NONE', ( #141420, #157298, #79383, #165965, #128079, #192585, #212572, #199700, #22373, #160002, #176017, #27799, #61371 ) ) ;
#136220 = CARTESIAN_POINT ( 'NONE',  ( -0.6823417656249969321, 3.280208333674754062, -1.181850606188749264 ) ) ;
#136219 = CARTESIAN_POINT ( 'NONE',  ( 4.458679977242249848, -2.047270833213535202, -1.031427349252316272 ) ) ;
#136221 = CARTESIAN_POINT ( 'NONE',  ( 6.620655732516642189, 0.6076529131340856482, 1.780684370158796881 ) ) ;
#136222 = CARTESIAN_POINT ( 'NONE',  ( 8.530051201292206287, 13.10347683481629488, 0.000000000000000000 ) ) ;
#136223 = CARTESIAN_POINT ( 'NONE',  ( 0.08289510313583270396, -1.381697626658566547, 1.608636130391014163 ) ) ;
#136224 = CARTESIAN_POINT ( 'NONE',  ( -3.619663825168619731, 7.166765529431275539, 1.040834085586084257E-14 ) ) ;
#136225 = CARTESIAN_POINT ( 'NONE',  ( 4.868786560638889149, 6.773613302202437403, 1.443375672974065660 ) ) ;
#136226 = CARTESIAN_POINT ( 'NONE',  ( -6.033015167956810920, 7.101234453113482559, -1.082531754730543083 ) ) ;
#136228 = CARTESIAN_POINT ( 'NONE',  ( 0.7500000000000006661, 11.11458333401613174, 1.299038105676657340 ) ) ;
#136227 = DIRECTION ( 'NONE',  ( 1.000000000000000000, 0.000000000000000000, 0.000000000000000000 ) ) ;
#136229 = ORIENTED_EDGE ( 'NONE', *, *, #194044, .T. ) ;
#136230 = CARTESIAN_POINT ( 'NONE',  ( 5.414685466650038137, -1.281359335986744341, -1.556910257834144051 ) ) ;
#136232 = CARTESIAN_POINT ( 'NONE',  ( 4.786014635464308498, -1.264713950826271027, -1.629283840103493253 ) ) ;
#136231 = CARTESIAN_POINT ( 'NONE',  ( 4.798696304233017074, 7.685897223992134819, -1.199719254218452047 ) ) ;
#136234 = CARTESIAN_POINT ( 'NONE',  ( -0.1409997244346087863, -0.002808977843308038246, -2.000147647483837776 ) ) ;
#136233 = CARTESIAN_POINT ( 'NONE',  ( 5.993586425693011144, 9.150212042353954800, -1.199719254218452047 ) ) ;
#136235 = CARTESIAN_POINT ( 'NONE',  ( 5.203297092594585393, 9.292540051327542017, 0.7998128361456341429 ) ) ;
#136236 = B_SPLINE_CURVE_WITH_KNOTS ( 'NONE', 3,
 ( #72976, #51421, #117542, #183536 ),
 .UNSPECIFIED., .F., .F.,
 ( 4, 4 ),
 ( 0.001855645002180106307, 0.002097104276149275998 ),
 .UNSPECIFIED. ) ;
#136238 = EDGE_CURVE ( 'NONE', #170224, #44633, #122878, .T. ) ;
#136237 = CARTESIAN_POINT ( 'NONE',  ( -3.285556943750000070, -1.509374999522042238, 0.000000000000000000 ) ) ;
#136239 = CARTESIAN_POINT ( 'NONE',  ( 0.1331565106231328566, 1.371277436080810208, -2.201942895618694607 ) ) ;
#136240 = CARTESIAN_POINT ( 'NONE',  ( 0.7618063994256699667, 1.031939465966443814, 1.818122583218291677 ) ) ;
#136241 = CARTESIAN_POINT ( 'NONE',  ( 4.500625067706437221, -1.976956227568788638, 0.3961002554062897918 ) ) ;
#136242 = CARTESIAN_POINT ( 'NONE',  ( 3.632213977189250098, 0.2737156317273430894, 1.820677940640710979 ) ) ;
#136243 = EDGE_CURVE ( 'NONE', #182271, #22322, #162222, .T. ) ;
#136244 = CARTESIAN_POINT ( 'NONE',  ( 4.469384193999260901, 8.366031992974468423, -0.7998128361456231517 ) ) ;
#136245 = CARTESIAN_POINT ( 'NONE',  ( 0.2524154375680361939, -1.389930774942317759, 1.021034751394875428 ) ) ;
#136246 = CARTESIAN_POINT ( 'NONE',  ( -3.358669367883384105, 4.941533567329135401, -1.599625672291262513 ) ) ;
#136247 = CARTESIAN_POINT ( 'NONE',  ( 0.7042444638330731532, 2.126757524241583486, 0.8727403922216511178 ) ) ;
#136248 = CARTESIAN_POINT ( 'NONE',  ( -5.065942953000576843, 9.062017211809330064, -0.7998128361456231517 ) ) ;
#136249 = CARTESIAN_POINT ( 'NONE',  ( 6.702048742255109381, -2.262191126150433274, 0.04724482429044154358 ) ) ;
#136250 = CARTESIAN_POINT ( 'NONE',  ( 2.631583836753316863, -1.964825297316885155, 0.7587525405363388931 ) ) ;
#136251 = CARTESIAN_POINT ( 'NONE',  ( -4.472210567661380587, 6.310941310395290493, 1.599625672291270506 ) ) ;
#136253 = EDGE_CURVE ( 'NONE', #170509, #163825, #90908, .T. ) ;
#136252 = CARTESIAN_POINT ( 'NONE',  ( 6.938021921891177612, 9.117444880338284818, -1.599625672291262513 ) ) ;
#136254 = CARTESIAN_POINT ( 'NONE',  ( 4.868786560638878491, 8.694351730805124134, 0.7216878364870317197 ) ) ;
#136255 = CARTESIAN_POINT ( 'NONE',  ( -7.562750758324527922, 7.717630727667075696, 1.040834085586084257E-14 ) ) ;
#136256 = CARTESIAN_POINT ( 'NONE',  ( 7.090551149822744925, 7.374657217655760100, 0.7216878364870317197 ) ) ;
#136257 = CARTESIAN_POINT ( 'NONE',  ( 4.226642156305554288, 7.541242530477547668, 0.9646342093552334740 ) ) ;
#136258 = CARTESIAN_POINT ( 'NONE',  ( -4.355193658487827690, 6.104145239700998538, -1.599625672291256295 ) ) ;
#136259 = CARTESIAN_POINT ( 'NONE',  ( 5.062811918942510481, 0.6453760322048059939, 2.125560002649288460 ) ) ;
#136260 = CARTESIAN_POINT ( 'NONE',  ( 2.502122453320880346, -0.8398649383675670377, -2.024319193490734303 ) ) ;
#136261 = CARTESIAN_POINT ( 'NONE',  ( -3.737243898861318137, 7.511868315313511069, 0.7998128361456341429 ) ) ;
#136262 = CARTESIAN_POINT ( 'NONE',  ( -4.604929450496978660, 5.401447776115099408, -1.199719254218453823 ) ) ;
#136263 = CARTESIAN_POINT ( 'NONE',  ( 5.125427350195786325, 0.1941421753944693185, -1.952251141935714696 ) ) ;
#136264 = AXIS2_PLACEMENT_3D ( 'NONE', #101926, #66187, #167992 ) ;
#136265 = CARTESIAN_POINT ( 'NONE',  ( -1.201851678989727383E-14, 2.571875000341417472, 1.575800808251672791 ) ) ;
#136266 = CARTESIAN_POINT ( 'NONE',  ( 6.889999999999996128, 2.105039946316529242, 2.031469082812328519 ) ) ;
#136267 = CARTESIAN_POINT ( 'NONE',  ( -5.097502569058221411, 6.009803087731781623, -1.082531754730544860 ) ) ;
#136268 = CARTESIAN_POINT ( 'NONE',  ( 4.412424163657523657, -2.120181911468725033, -0.04909571644767100895 ) ) ;
#136269 = CARTESIAN_POINT ( 'NONE',  ( -6.563555762791521531, 9.711213252348503744, 1.082531754730549967 ) ) ;
#136270 = ORIENTED_EDGE ( 'NONE', *, *, #82484, .T. ) ;
#136272 = CARTESIAN_POINT ( 'NONE',  ( 6.368072262247213899, 1.106822706796772193, 1.856716078747308263 ) ) ;
#136271 = CARTESIAN_POINT ( 'NONE',  ( -6.455090533882206216, 7.663932056684933158, -1.082531754730549967 ) ) ;
#136273 = CARTESIAN_POINT ( 'NONE',  ( 6.765682348419287173, 7.852049813699357728, 1.199719254218462483 ) ) ;
#136274 = CARTESIAN_POINT ( 'NONE',  ( 4.704558828624370470, 1.604442792107749760, 0.9031527321438773681 ) ) ;
#136275 = CARTESIAN_POINT ( 'NONE',  ( 0.000000000000000000, 8.500000000000000000, 0.000000000000000000 ) ) ;
#136276 = CARTESIAN_POINT ( 'NONE',  ( -1.364683531250012516, 2.801041667008090652, -0.7879004041258289570 ) ) ;
#136277 = CARTESIAN_POINT ( 'NONE',  ( 1.329236136963531489, 0.8583591509643221373, -1.513936452999464555 ) ) ;
#136278 = CARTESIAN_POINT ( 'NONE',  ( -1.115562610750309283E-14, 11.34375000068279604, 1.500000000000001554 ) ) ;
#136279 = CARTESIAN_POINT ( 'NONE',  ( -1.734723475976807094E-15, 2.999999999999988898, -6.938893903907228378E-15 ) ) ;
#136280 = DIRECTION ( 'NONE',  ( 2.949029909160572061E-17, 1.000000000000000000, -8.673600428462391266E-15 ) ) ;
#136281 = CARTESIAN_POINT ( 'NONE',  ( 5.700121470611750674, -2.161883445634639411, -0.004416275431240455560 ) ) ;
#136282 = CARTESIAN_POINT ( 'NONE',  ( -4.192495815123836955, 5.914331089109674089, -1.599625672291256295 ) ) ;
#136283 = ADVANCED_FACE ( 'NONE', ( #59449 ), #25872, .T. ) ;
#136284 = CARTESIAN_POINT ( 'NONE',  ( -7.226132685959434809, 8.493204890783200511, 1.082531754730549967 ) ) ;
#136285 = CARTESIAN_POINT ( 'NONE',  ( 4.100566281481184738, -0.6756360485904688851, -2.053482476349233643 ) ) ;
#136286 = CARTESIAN_POINT ( 'NONE',  ( -1.364683531250000748, 2.259375000341422357, 1.214306433183764966E-14 ) ) ;
#136287 = CARTESIAN_POINT ( 'NONE',  ( 4.991463202408453093, 1.458887350482462875, 1.326006969317705009 ) ) ;
#136288 = CARTESIAN_POINT ( 'NONE',  ( 3.989331682606485519, 1.645927443309925353, 0.5452122354672321869 ) ) ;
#136289 = CARTESIAN_POINT ( 'NONE',  ( 0.8377433530848135135, 0.8832496248250313320, -2.005872107257236969 ) ) ;
#136290 = CARTESIAN_POINT ( 'NONE',  ( 2.415413485888187495, 2.061215426621319402, 1.037632957015870661 ) ) ;
#136291 = CARTESIAN_POINT ( 'NONE',  ( 3.848945901207713849, -1.686846252213095365, 1.183521113291643223 ) ) ;
#136292 = CARTESIAN_POINT ( 'NONE',  ( 0.5681770160902823719, -1.828317568802136250, -0.6549081214334094847 ) ) ;
#136293 = CARTESIAN_POINT ( 'NONE',  ( -7.551528372687420720, 8.872833191965849409, 1.082531754730558626 ) ) ;
#136294 = CARTESIAN_POINT ( 'NONE',  ( -5.655686355556086120, 6.627330832017406692, 1.199719254218452935 ) ) ;
#136295 = DIRECTION ( 'NONE',  ( 1.000000000000000000, 0.000000000000000000, -0.000000000000000000 ) ) ;
#136296 = FACE_OUTER_BOUND ( 'NONE', #180691, .T. ) ;
#136297 = CARTESIAN_POINT ( 'NONE',  ( -6.141480396866151992, 9.148515648777049591, 1.082531754730548412 ) ) ;
#136298 = CARTESIAN_POINT ( 'NONE',  ( 3.768774344222697970, -1.483932802477351487, 1.633493490917396151 ) ) ;
#136299 = CARTESIAN_POINT ( 'NONE',  ( 3.285556943750000070, -2.471874999522040373, 0.000000000000000000 ) ) ;
#136300 = ORIENTED_EDGE ( 'NONE', *, *, #169774, .F. ) ;
#136301 = CARTESIAN_POINT ( 'NONE',  ( 0.3384086464433467278, -1.803039684303367141, -0.4601552930486965121 ) ) ;
#136302 = CARTESIAN_POINT ( 'NONE',  ( -0.1288028175206907822, -0.008968661790493319408, -2.273875003271645934 ) ) ;
#136303 = CARTESIAN_POINT ( 'NONE',  ( -15.75000000000000000, 12.69999999999999929, -0.7000000000000009548 ) ) ;
#136304 = CARTESIAN_POINT ( 'NONE',  ( -9.531438498077104526, -8.057097448493919956, 0.1980946632349051273 ) ) ;
#136306 = CARTESIAN_POINT ( 'NONE',  ( 6.925078400183575233, 2.022016365062285104, 2.447829694591229899 ) ) ;
#136305 = CARTESIAN_POINT ( 'NONE',  ( -6.175853536056814086, 7.055546168579414079, -1.074032317439767903 ) ) ;
#136307 = CARTESIAN_POINT ( 'NONE',  ( -15.75000000000000000, 10.89999999999998259, 3.599999999999999201 ) ) ;
#136308 = ORIENTED_EDGE ( 'NONE', *, *, #961, .F. ) ;
#136309 = CARTESIAN_POINT ( 'NONE',  ( 3.239188564323669528, -1.818332144261879613, 0.9699876223461401104 ) ) ;
#136310 = CARTESIAN_POINT ( 'NONE',  ( -0.6801582343750143256, 1.848958333674724397, -1.178068619123862515 ) ) ;
#136311 = B_SPLINE_CURVE_WITH_KNOTS ( 'NONE', 3,
 ( #108263, #146048, #162279, #160141, #47480, #126655, #147106, #180648, #77815, #192622, #64761, #210999, #177462, #62623, #195839, #13866 ),
 .UNSPECIFIED., .F., .F.,
 ( 4, 2, 2, 2, 2, 2, 2, 4 ),
 ( 0.6095821870314059865, 0.6120980958896804491, 0.6146140047479549118, 0.6196458224645037260, 0.6297094578976014656, 0.6397880689092279027, 0.6448273744150412323, 0.6498666799208544509 ),
 .UNSPECIFIED. ) ;
#136312 = CARTESIAN_POINT ( 'NONE',  ( -4.706651882238427120, 8.642844295920152575, 1.040834085586084257E-14 ) ) ;
#136314 = CIRCLE ( 'NONE', #205388, 0.07999999999999998779 ) ;
#136313 = SURFACE_STYLE_FILL_AREA ( #170925 ) ;
#136315 = CARTESIAN_POINT ( 'NONE',  ( 4.847203612085560387, 5.613824621309978724, -1.199719254218452047 ) ) ;
#136316 = CARTESIAN_POINT ( 'NONE',  ( 2.202092877552201067, -2.060466153685360791, 0.04932271190436626068 ) ) ;
#136318 = CARTESIAN_POINT ( 'NONE',  ( -1.402160292154681736E-14, 13.67187500034139447, 1.575800808251682339 ) ) ;
#136317 = CARTESIAN_POINT ( 'NONE',  ( 1.416814887940471390, 7.999555336178685749, 9.899480522462164700 ) ) ;
#136319 = CARTESIAN_POINT ( 'NONE',  ( 6.982612806237943559, 8.105135347821125436, -1.199719254218446718 ) ) ;
#136320 = CARTESIAN_POINT ( 'NONE',  ( 2.278321918429430770, 2.687264847272027968, 2.500000000000000888 ) ) ;
#136321 = EDGE_CURVE ( 'NONE', #12895, #30003, #65222, .T. ) ;
#136322 = CARTESIAN_POINT ( 'NONE',  ( 5.953802724510455668, 0.6443607167232848765, -2.110727517106169682 ) ) ;
#136323 = CARTESIAN_POINT ( 'NONE',  ( 0.9839146201040609441, 1.450980403326153301, 1.602422216231303320 ) ) ;
#136324 = CARTESIAN_POINT ( 'NONE',  ( -4.121315508874255684, 7.752025827087861920, -0.7216878364870267237 ) ) ;
#136325 = CARTESIAN_POINT ( 'NONE',  ( 1.059780186608853203, 1.205045252304644210, 1.616690996016925563 ) ) ;
#136326 = CARTESIAN_POINT ( 'NONE',  ( 2.337686028923485537, -1.414513361329417851, 1.811461888080208027 ) ) ;
#136327 = CARTESIAN_POINT ( 'NONE',  ( -1.138412281109779656E-15, -7.357813805514521910, -9.695354081530195955 ) ) ;
#136328 = CARTESIAN_POINT ( 'NONE',  ( 6.252599623108594074, 1.892168639490459325, 0.2757424028280440753 ) ) ;
#136329 = CARTESIAN_POINT ( 'NONE',  ( 1.843739406749228538, 8.923774302061360686, -0.7749999999999996891 ) ) ;
#136330 =( GEOMETRIC_REPRESENTATION_CONTEXT ( 3 ) GLOBAL_UNCERTAINTY_ASSIGNED_CONTEXT ( ( #9990 ) ) GLOBAL_UNIT_ASSIGNED_CONTEXT ( ( #73905, #191895, #59780 ) ) REPRESENTATION_CONTEXT ( 'NONE', 'WORKASPACE' ) );
#136331 = CARTESIAN_POINT ( 'NONE',  ( 2.342468781959532453, 0.4075140148256419792, 1.825566309089213579 ) ) ;
#136332 = CARTESIAN_POINT ( 'NONE',  ( 3.450407915430803385, -1.350735839785843773, 1.497501794165828626 ) ) ;
#136334 = CARTESIAN_POINT ( 'NONE',  ( 11.35573736746270335, 13.61270414413280250, 3.554362808847919553 ) ) ;
#136333 = CARTESIAN_POINT ( 'NONE',  ( -1.364683531250000748, 2.259375000341422357, 1.214306433183764966E-14 ) ) ;
#136336 = CARTESIAN_POINT ( 'NONE',  ( 4.635441201516187881, -1.925843587088198916, 0.8528682856967207959 ) ) ;
#136335 = CARTESIAN_POINT ( 'NONE',  ( -6.852756576703439961, 10.08230087520760954, 1.199719254218453823 ) ) ;
#136337 = CARTESIAN_POINT ( 'NONE',  ( 5.309989718046547402, 9.346738437696316737, 0.7998128361456462443 ) ) ;
#136339 = CARTESIAN_POINT ( 'NONE',  ( -7.497822643557261024, 8.706213491360317747, -1.199719254218446718 ) ) ;
#136338 = CARTESIAN_POINT ( 'NONE',  ( 5.520104819419390907, 6.469152373191302985, 1.199719254218452935 ) ) ;
#136340 = CARTESIAN_POINT ( 'NONE',  ( -11.33772463945036968, 13.40000000000000036, -3.680000000000001048 ) ) ;
#136341 = CARTESIAN_POINT ( 'NONE',  ( 5.080334495226257907, 0.9990293545295618749, 1.755361416599170443 ) ) ;
#136342 = CARTESIAN_POINT ( 'NONE',  ( -0.7500000000000249800, -0.7770833326505161009, 1.299038105676659116 ) ) ;
#136343 = CARTESIAN_POINT ( 'NONE',  ( 0.3212321915853528220, -1.840712657873358138, -0.9308276203483353273 ) ) ;
#136344 = CARTESIAN_POINT ( 'NONE',  ( 8.351459436338029008, 10.76645531385962862, -1.443375672974063439 ) ) ;
#136345 = CARTESIAN_POINT ( 'NONE',  ( 6.046190728430958394, 2.158797838069245412, 0.1127497994189360364 ) ) ;
#136346 = CARTESIAN_POINT ( 'NONE',  ( 6.013923656113508542, 9.173938811177871244, -1.199719254218452047 ) ) ;
#136347 = ADVANCED_FACE ( 'NONE', ( #62634 ), #98349, .F. ) ;
#136348 = CARTESIAN_POINT ( 'NONE',  ( 0.6823417656249882723, -0.2614583329919109578, -1.181850606188749264 ) ) ;
#136350 = CARTESIAN_POINT ( 'NONE',  ( -7.726139724254740493, -6.443545996361842221, 7.681709917290615586 ) ) ;
#136349 = CARTESIAN_POINT ( 'NONE',  ( 4.634908411025333130, 6.500755460986618495, 1.599625672291268286 ) ) ;
#136351 = B_SPLINE_CURVE_WITH_KNOTS ( 'NONE', 3,
 ( #207584, #141577, #25632, #42990, #59204, #125360, #44048, #162059, #109103, #91744, #127509, #176178, #13648, #26704, #140505, #92806, #60273, #128572, #194536, #158850, #58148, #10447, #192393, #142631, #209705, #27778, #93876, #159913 ),
 .UNSPECIFIED., .F., .F.,
 ( 4, 3, 3, 3, 3, 3, 3, 3, 3, 4 ),
 ( 0.000000000000000000, 4.667319012710265200E-05, 7.775567177467941214E-05, 9.418433154889146845E-05, 0.0001004198801466371470, 0.0001156098471385010821, 0.0001218465752387289092, 0.0001431384767120459612, 0.0001435705847349271001, 0.0001594483893922525955 ),
 .UNSPECIFIED. ) ;
#136352 = CARTESIAN_POINT ( 'NONE',  ( 8.717529583462654941, 9.272798723569005475, 0.7216878364870458196 ) ) ;
#136354 = DIRECTION ( 'NONE',  ( -1.000000000000000000, 0.000000000000000000, 1.224646799147352961E-16 ) ) ;
#136353 = CARTESIAN_POINT ( 'NONE',  ( 3.051421578680337809, 1.863438581370242986, -1.114033871086346217 ) ) ;
#136356 = CARTESIAN_POINT ( 'NONE',  ( 1.839159199666509981, 0.7036077657225293658, -1.701706503975081830 ) ) ;
#136355 = CARTESIAN_POINT ( 'NONE',  ( -4.609409038966229666, 8.321468278861834378, -0.7216878364870267237 ) ) ;
#136357 = CARTESIAN_POINT ( 'NONE',  ( 1.364683531249988535, 3.613541667008086211, 0.7879004041258500513 ) ) ;
#136358 = CARTESIAN_POINT ( 'NONE',  ( 3.474349307649237328, -2.112600797985896950, -0.5827812199917583591 ) ) ;
#136359 = CARTESIAN_POINT ( 'NONE',  ( 6.883263157960330503, 7.629137130509037412, 2.753810918356710769 ) ) ;
#136360 = CARTESIAN_POINT ( 'NONE',  ( 4.434621138646507532, 2.218105251380130483, 0.4453182654360221537 ) ) ;
#136361 = CARTESIAN_POINT ( 'NONE',  ( -5.208303565944065738, 9.228104593576741621, -0.7998128361456231517 ) ) ;
#136362 = CARTESIAN_POINT ( 'NONE',  ( 0.6823417656249917140, 5.655208333674749177, 1.181850606188765695 ) ) ;
#136363 = CARTESIAN_POINT ( 'NONE',  ( 5.535985025370705692, 7.434063834270491000, -1.247683609459742549 ) ) ;
#136364 = CARTESIAN_POINT ( 'NONE',  ( 0.7500000000000006661, 13.33333333333333570, 1.299038105676657340 ) ) ;
#136365 = CARTESIAN_POINT ( 'NONE',  ( -4.923019175093582334, 8.757623114335565617, 0.7216878364870267237 ) ) ;
#136366 = CARTESIAN_POINT ( 'NONE',  ( 6.699137298928158124, 6.988284068270579574, 0.7216878364870328300 ) ) ;
#136367 = CARTESIAN_POINT ( 'NONE',  ( 5.501144674179510474, 1.447219185280288700, 1.018257267444661496 ) ) ;
#136368 = B_SPLINE_CURVE_WITH_KNOTS ( 'NONE', 3,
 ( #88798, #188405, #103978, #184134, #35758, #40043, #101832, #102900, #5357, #167901, #85575 ),
 .UNSPECIFIED., .F., .F.,
 ( 4, 1, 1, 1, 1, 1, 1, 1, 4 ),
 ( 0.000000000000000000, 0.2254101072112788262, 0.3970395454107691902, 0.5239558410346354389, 0.6152342776129972046, 0.6800502191696807808, 0.7279184599320936977, 0.7685697607527866015, 1.000000000000000000 ),
 .UNSPECIFIED. ) ;
#136369 = CARTESIAN_POINT ( 'NONE',  ( 9.257519960032755790, 9.694861462993381807, 0.7998128361456462443 ) ) ;
#136370 = CARTESIAN_POINT ( 'NONE',  ( 1.518734001684220347, 1.414770742371696644, -1.560122519311944345 ) ) ;
#136372 = CARTESIAN_POINT ( 'NONE',  ( -1.500000000000013101, 2.879166666666688634, -0.8660254037844313801 ) ) ;
#136371 = CARTESIAN_POINT ( 'NONE',  ( 1.364683531250000303, 12.25520833367473195, -0.7879004041258355073 ) ) ;
#136373 = CARTESIAN_POINT ( 'NONE',  ( 2.260148812482842828, -1.969196485324760326, 0.04527702327579082725 ) ) ;
#136374 = CARTESIAN_POINT ( 'NONE',  ( 6.727182134110200273, -0.004969159814478123736, 2.189081792362323586 ) ) ;
#136375 = DIRECTION ( 'NONE',  ( 1.000000000000000000, 2.168404344971003188E-14, 0.000000000000000000 ) ) ;
#136377 = ORIENTED_EDGE ( 'NONE', *, *, #83031, .F. ) ;
#136376 = CARTESIAN_POINT ( 'NONE',  ( 6.363521484574993003, -1.460773276151544176, -1.071267404939825640 ) ) ;
#136378 = CARTESIAN_POINT ( 'NONE',  ( 7.144783764721768904, 7.437928601704619780, 1.040834085586084257E-14 ) ) ;
#136379 = EDGE_CURVE ( 'NONE', #44793, #17896, #30151, .T. ) ;
#136380 = CARTESIAN_POINT ( 'NONE',  ( -1.402160292154681736E-14, -1.115624999658584082, 1.575800808251672791 ) ) ;
#136381 = CARTESIAN_POINT ( 'NONE',  ( 5.418772907935071714, 1.728844841293469159, 0.7149302089985640762 ) ) ;
#136382 = ORIENTED_EDGE ( 'NONE', *, *, #52780, .T. ) ;
#136383 = CARTESIAN_POINT ( 'NONE',  ( 5.453992358814952368, -0.7503507308065425763, 1.929658000011783336 ) ) ;
#136384 = PRESENTATION_STYLE_ASSIGNMENT (( #17258 ) ) ;
#136385 = CARTESIAN_POINT ( 'NONE',  ( -6.089020385868876062, 6.276481003034692030, -0.7216878364870338292 ) ) ;
#136387 = CARTESIAN_POINT ( 'NONE',  ( 0.1333692844072559280, 0.001398348041498076455, -2.053671342968105051 ) ) ;
#136386 = CIRCLE ( 'NONE', #43011, 9.579999999999992966 ) ;
#136388 = CARTESIAN_POINT ( 'NONE',  ( -1.500000000000015099, -0.1208333333333093396, -0.8660254037844383745 ) ) ;
#136389 = CARTESIAN_POINT ( 'NONE',  ( 6.889514614038635187, 11.18951748302043114, -0.7998128361456291469 ) ) ;
#136390 = CARTESIAN_POINT ( 'NONE',  ( -7.818248136574758256, 12.27303992597924420, 0.000000000000000000 ) ) ;
#136391 = CARTESIAN_POINT ( 'NONE',  ( 4.844006021832467646, 8.873367135438366304, 0.000000000000000000 ) ) ;
#136392 = CARTESIAN_POINT ( 'NONE',  ( -0.6823417656250003738, 0.4677083336747517306, -1.181850606188749264 ) ) ;
#136393 = CARTESIAN_POINT ( 'NONE',  ( 1.499999999999987121, 1.254166666666689300, 0.8660254037844524744 ) ) ;
#136395 = CARTESIAN_POINT ( 'NONE',  ( 5.769158057814842699, 6.689438141327490150, 1.199719254218462483 ) ) ;
#136394 = CARTESIAN_POINT ( 'NONE',  ( 5.178158156489047315, -1.047961880893449882, -1.658324637040713867 ) ) ;
#136396 = CARTESIAN_POINT ( 'NONE',  ( 3.409529676982744562, 0.4871283372531940992, 1.956261718130556160 ) ) ;
#136397 = CARTESIAN_POINT ( 'NONE',  ( 2.149496333622540334, 1.877876629180765589, -0.3779552698702989266 ) ) ;
#136398 = EDGE_CURVE ( 'NONE', #84217, #138803, #196907, .T. ) ;
#136399 = FACE_OUTER_BOUND ( 'NONE', #121669, .T. ) ;
#136400 = CARTESIAN_POINT ( 'NONE',  ( 0.7322823680011962821, 2.160084099745246178, 0.3691886501416344335 ) ) ;
#136401 = CARTESIAN_POINT ( 'NONE',  ( 0.2333690889706926119, 0.7157316027301027228, -2.136973218959358434 ) ) ;
#136402 = CARTESIAN_POINT ( 'NONE',  ( 2.319419987651088810, -1.815478447740950685, 0.4500915571382518854 ) ) ;
#136403 = CARTESIAN_POINT ( 'NONE',  ( 1.364683531249992088, 5.384375000341417916, 1.214306433183764966E-14 ) ) ;
#136404 = CARTESIAN_POINT ( 'NONE',  ( 4.394793396725252599, -1.953840400094335905, -0.4849018877997012256 ) ) ;
#136405 = CARTESIAN_POINT ( 'NONE',  ( -8.290974629956718189, 9.631557475493025322, -1.199719254218446718 ) ) ;
#136407 = CARTESIAN_POINT ( 'NONE',  ( 4.482099252480286289, -2.116778089722763045, -0.05043497882678028149 ) ) ;
#136406 = CARTESIAN_POINT ( 'NONE',  ( -4.772106882330227506, 7.550913215151819458, -1.082531754730549967 ) ) ;
#136408 = CARTESIAN_POINT ( 'NONE',  ( -0.09916492693109210665, -9.920000000000095852, -9.499482423651642193 ) ) ;
#136409 = CARTESIAN_POINT ( 'NONE',  ( 6.443811375169310907, 1.424792453395683500, 1.502365266013883538 ) ) ;
#136411 = CARTESIAN_POINT ( 'NONE',  ( -4.163763581353360443, 7.871824920094959488, -5.011504818508299590E-05 ) ) ;
#136410 = CARTESIAN_POINT ( 'NONE',  ( 0.6618065864371965867, 1.033746398093362773, 1.817239694416083795 ) ) ;
#136413 = VERTEX_POINT ( 'NONE', #99420 ) ;
#136412 = CARTESIAN_POINT ( 'NONE',  ( 6.821331453475777629, -0.1281762050449504198, 1.796388512460028286 ) ) ;
#136414 = CARTESIAN_POINT ( 'NONE',  ( 7.182068686937156166, 9.402166106225269715, 1.599625672291281386 ) ) ;
#136415 = CARTESIAN_POINT ( 'NONE',  ( -5.422898255786213539, 5.429062174613084935, -0.7216878364870178419 ) ) ;
#136416 = CARTESIAN_POINT ( 'NONE',  ( -11.89942855770814134, 13.79999999999999893, 0.6999999999999992895 ) ) ;
#136417 = CARTESIAN_POINT ( 'NONE',  ( -9.956232484441596142, 5.504245459870187318, 6.026037945409589369 ) ) ;
#136418 = CARTESIAN_POINT ( 'NONE',  ( 7.578644679914718019, 7.944099669429731669, 0.7216878364870317197 ) ) ;
#136419 = CARTESIAN_POINT ( 'NONE',  ( 0.6823417656249969321, 12.83854166700806942, -1.181850606188757036 ) ) ;
#136421 = CARTESIAN_POINT ( 'NONE',  ( 0.4690326002820300877, -1.529415377529659503, -0.9703845247886667691 ) ) ;
#136420 = CARTESIAN_POINT ( 'NONE',  ( 6.912678218121202534, 9.158153569265168770, 1.599625672291268286 ) ) ;
#136422 = CARTESIAN_POINT ( 'NONE',  ( -6.509886312855995172, 10.74661779830734254, -0.7998128361456291469 ) ) ;
#136423 = CARTESIAN_POINT ( 'NONE',  ( 5.575427483717746213, 7.527751369135936343, 1.599625672291267398 ) ) ;
#136424 = CARTESIAN_POINT ( 'NONE',  ( -0.08058608058608779379, -6.134628647623513231, 10.99970480893080804 ) ) ;
#136425 = CARTESIAN_POINT ( 'NONE',  ( 4.189106276498237413, 3.989638198777126110, -0.7216878364870188411 ) ) ;
#136426 = LINE ( 'NONE', #82317, #179030 ) ;
#136427 = CARTESIAN_POINT ( 'NONE',  ( 2.523789150438203510, 6.096171108819874007, 0.7998128361456462443 ) ) ;
#136428 = ORIENTED_EDGE ( 'NONE', *, *, #169120, .F. ) ;
#136429 = CARTESIAN_POINT ( 'NONE',  ( 6.028922772295511656, -1.701938481575874684, 1.081082441910637071 ) ) ;
#136430 = CARTESIAN_POINT ( 'NONE',  ( -0.04015575566676531788, -1.641981170221143094, -1.341450104213978589 ) ) ;
#136431 = DIRECTION ( 'NONE',  ( 0.000000000000000000, 1.000000000000000000, 0.000000000000000000 ) ) ;
#136432 = CLOSED_SHELL ( 'NONE', ( #36810, #1742, #126462, #53802, #49851, #121890, #114026, #210444, #21023, #81823 ) ) ;
#136433 = DIRECTION ( 'NONE',  ( 0.000000000000000000, -1.000000000000000000, 0.000000000000000000 ) ) ;
#136434 = DIRECTION ( 'NONE',  ( 1.000000000000000000, 0.000000000000000000, -6.695352868347765393E-17 ) ) ;
#136435 = CARTESIAN_POINT ( 'NONE',  ( -3.131570295076647525, 6.597323077657299528, 1.040834085586084257E-14 ) ) ;
#136436 = CARTESIAN_POINT ( 'NONE',  ( 10.54788032175191326, 11.40820791823982994, 0.7216878364870317197 ) ) ;
#136437 = CARTESIAN_POINT ( 'NONE',  ( 2.992966325197043531, 0.2361965902525232364, 1.955129705961492270 ) ) ;
#136438 = CARTESIAN_POINT ( 'NONE',  ( 4.394157760337158436, -0.8647400765994193161, -1.821735888681835558 ) ) ;
#136439 = CARTESIAN_POINT ( 'NONE',  ( -6.043183783389232566, 8.073467052085995022, 1.599625672291269396 ) ) ;
#136440 = SURFACE_STYLE_FILL_AREA ( #37854 ) ;
#136441 = DIRECTION ( 'NONE',  ( -0.6507913734559658270, 0.7592566023652989049, 0.000000000000000000 ) ) ;
#136442 = CARTESIAN_POINT ( 'NONE',  ( 5.279302027902110339, 1.469929824498400039, 1.625505876179579534 ) ) ;
#136443 = CARTESIAN_POINT ( 'NONE',  ( -1.201851678989727383E-14, 3.009375000341419693, -1.575800808251660134 ) ) ;
#136444 = CARTESIAN_POINT ( 'NONE',  ( 3.539987092570716865, 0.8674169631235107980, -1.720131978839019693 ) ) ;
#136445 = CARTESIAN_POINT ( 'NONE',  ( -8.518600588087975822, 8.832788862391110385, 1.040834085586084257E-14 ) ) ;
#136446 = CARTESIAN_POINT ( 'NONE',  ( -0.02988540731101250320, 5.726092063503692486, -2.320384613474982594 ) ) ;
#136447 = CARTESIAN_POINT ( 'NONE',  ( 0.1331565106231328843, 0.003911343561965873426, -1.946049565259087455 ) ) ;
#136448 = ADVANCED_FACE ( 'NONE', ( #181708 ), #47492, .F. ) ;
#136449 = VERTEX_POINT ( 'NONE', #33338 ) ;
#136450 = CARTESIAN_POINT ( 'NONE',  ( 4.502716413514295191, 6.346531463890372926, -1.443375672974068769 ) ) ;
#136451 = CARTESIAN_POINT ( 'NONE',  ( 5.506690373602650901, 0.5681407172444596920, 1.885743917740757114 ) ) ;
#136453 = CARTESIAN_POINT ( 'NONE',  ( 4.213543065054736303, 1.618255708775760970, 1.197237177376732964 ) ) ;
#136452 = CARTESIAN_POINT ( 'NONE',  ( 0.09902944379243035222, -0.5168498253214492966, 1.871975360678623579 ) ) ;
#136454 = CARTESIAN_POINT ( 'NONE',  ( 5.431170548343748905, 1.126412363255802518, 2.003379520639406497 ) ) ;
#136456 = CARTESIAN_POINT ( 'NONE',  ( 3.836619860451701669, -1.792334419201064399, -0.5002748670543122333 ) ) ;
#136455 = CARTESIAN_POINT ( 'NONE',  ( 1.500000000000053291, 7.750000000000000000, 15.74999999999999289 ) ) ;
#136457 = CARTESIAN_POINT ( 'NONE',  ( 7.225569521440261767, 7.394528961293920233, -0.7998128361456341429 ) ) ;
#136458 = FACE_OUTER_BOUND ( 'NONE', #53833, .T. ) ;
#136459 = CARTESIAN_POINT ( 'NONE',  ( 1.734723475976807094E-15, 15.42733875946000133, 11.91973154060105955 ) ) ;
#136460 = CARTESIAN_POINT ( 'NONE',  ( -7.477485413136760073, 8.682486722536401302, -1.199719254218446718 ) ) ;
#136461 = CARTESIAN_POINT ( 'NONE',  ( -4.014622883422329203, 6.737458226417744278, -1.082531754730546636 ) ) ;
#136462 = CARTESIAN_POINT ( 'NONE',  ( 0.1346727191937693857, 0.3808678606769915209, 2.158067550307264604 ) ) ;
#136463 = CARTESIAN_POINT ( 'NONE',  ( 6.819388077993785657, 7.058300300521964665, 1.040834085586084257E-14 ) ) ;
#136464 = VERTEX_POINT ( 'NONE', #164415 ) ;
#136465 = DIRECTION ( 'NONE',  ( 0.000000000000000000, 0.000000000000000000, 1.000000000000000000 ) ) ;
#136466 = DIRECTION ( 'NONE',  ( -0.7806247497998004548, 0.000000000000000000, -0.6249999999999992228 ) ) ;
#136467 = CARTESIAN_POINT ( 'NONE',  ( 0.8381832108898427114, 1.798179982845280467, 0.3147962740308178353 ) ) ;
#136468 = CARTESIAN_POINT ( 'NONE',  ( -4.959585264500673496, 4.680604318205876524, 1.214306433183764966E-14 ) ) ;
#136469 = CARTESIAN_POINT ( 'NONE',  ( 2.795252500310735133, 1.254151915811404061, -1.197898925204267995 ) ) ;
#136470 = CARTESIAN_POINT ( 'NONE',  ( -6.138158007735671440, 5.995864564798076835, -0.1121503744203552477 ) ) ;
#136471 = CARTESIAN_POINT ( 'NONE',  ( -0.3282377607281363741, 0.1986645496846400905, -1.225000000000038725 ) ) ;
#136472 = CARTESIAN_POINT ( 'NONE',  ( 5.848246728868278232, 1.823843535133644389, 0.08496628090458313576 ) ) ;
#136473 = CARTESIAN_POINT ( 'NONE',  ( 3.766413727395605093, -0.7909564911158167844, -1.795405819223389488 ) ) ;
#136474 = CARTESIAN_POINT ( 'NONE',  ( -0.6125000000000089262, -0.1458333326505162342, 1.060881119635894487 ) ) ;
#136475 = CARTESIAN_POINT ( 'NONE',  ( -7.343712760096452463, 11.71941532008788833, -0.7998128361456291469 ) ) ;
#136476 = CARTESIAN_POINT ( 'NONE',  ( 6.805303039055573322, 10.02693841461847057, 1.199719254218460707 ) ) ;
#136477 = CARTESIAN_POINT ( 'NONE',  ( 3.897227946829431300, -0.2092540311423168320, -2.110150122182581356 ) ) ;
#136478 = CARTESIAN_POINT ( 'NONE',  ( 6.481679955784983349, 9.719654494127929922, -1.199719254218452047 ) ) ;
#136479 = CIRCLE ( 'NONE', #126189, 11.99999999999999112 ) ;
#136480 = CARTESIAN_POINT ( 'NONE',  ( 2.219664259111033378, 0.3580842396277704176, -2.038906786875307020 ) ) ;
#136482 = CARTESIAN_POINT ( 'NONE',  ( 1.364683531249984538, -1.032291666325247714, -0.7879004041258309554 ) ) ;
#136481 = CARTESIAN_POINT ( 'NONE',  ( -11.48243876534946217, 12.22000000000000064, -3.200000000000001510 ) ) ;
#136485 = ORIENTED_EDGE ( 'NONE', *, *, #209073, .T. ) ;
#136484 = CARTESIAN_POINT ( 'NONE',  ( 4.125785508553894587, -0.3794599818576475658, 2.188496638732019495 ) ) ;
#136483 = AXIS2_PLACEMENT_3D ( 'NONE', #53296, #183289, #55430 ) ;
#136486 = CARTESIAN_POINT ( 'NONE',  ( 1.372188323541504218, -0.3435771540031757332, -2.272792483656468576 ) ) ;
#136487 = CARTESIAN_POINT ( 'NONE',  ( 9.747949258545622442, 10.47495501116581984, 0.000000000000000000 ) ) ;
#136489 = CARTESIAN_POINT ( 'NONE',  ( 1.001543065824772753E-15, -2.471874999522041705, 3.793834371823811669 ) ) ;
#136488 = CARTESIAN_POINT ( 'NONE',  ( 5.090160327287878594, 4.903218234782778850, -0.7998128361456481317 ) ) ;
#136490 = EDGE_CURVE ( 'NONE', #11835, #64117, #134235, .T. ) ;
#136491 = DIRECTION ( 'NONE',  ( 0.000000000000000000, -1.000000000000000000, -0.000000000000000000 ) ) ;
#136492 = CARTESIAN_POINT ( 'NONE',  ( -10.52558186178533539, 3.957600067444659420, 5.763924342718092397 ) ) ;
#136493 = DIRECTION ( 'NONE',  ( 0.000000000000000000, 0.000000000000000000, 1.000000000000000000 ) ) ;
#136494 = CARTESIAN_POINT ( 'NONE',  ( 2.707167837304753633, 1.638089068140319071, -0.9866689735503200165 ) ) ;
#136495 = CARTESIAN_POINT ( 'NONE',  ( -0.04822499102144637423, 6.344199970485692397, -3.092266627314186334 ) ) ;
#136496 = CARTESIAN_POINT ( 'NONE',  ( 3.908989539853875428, 1.479446464633243474, 0.8863536201247077528 ) ) ;
#136497 = CARTESIAN_POINT ( 'NONE',  ( 2.009000277268524481, 0.004839059525654776373, 2.016708403978189956 ) ) ;
#136498 = CARTESIAN_POINT ( 'NONE',  ( 3.709890859234076466, 2.183183022688690578, 0.7197655052363950423 ) ) ;
#136499 = DIRECTION ( 'NONE',  ( -0.000000000000000000, -1.000000000000000000, -0.000000000000000000 ) ) ;
#136500 = CARTESIAN_POINT ( 'NONE',  ( -0.02244404828157658613, -0.004869073801674199918, -2.189079685368473527 ) ) ;
#136501 = CARTESIAN_POINT ( 'NONE',  ( -6.794044374223859428, 7.099008989448849505, 0.000000000000000000 ) ) ;
#136502 = CARTESIAN_POINT ( 'NONE',  ( 5.290226454957744018, -1.756441682966399132, -0.2160651130965525468 ) ) ;
#136503 = ADVANCED_FACE ( 'NONE', ( #49594 ), #212072, .F. ) ;
#136505 = CARTESIAN_POINT ( 'NONE',  ( 1.078551950277906402, -2.237456700407819632, -0.4976139165283523513 ) ) ;
#136504 = CARTESIAN_POINT ( 'NONE',  ( 5.851225812749518695, 8.984124660586543243, -1.199719254218452047 ) ) ;
#136506 = CARTESIAN_POINT ( 'NONE',  ( 0.1986093482617317107, -0.4694325260376422948, 1.675759954737522150 ) ) ;
#136507 = CARTESIAN_POINT ( 'NONE',  ( -4.647747731386360215, 4.316793862905830892, 0.7998128361456341429 ) ) ;
#136508 = CARTESIAN_POINT ( 'NONE',  ( 5.208995777154565410, -0.3238732214236837992, 2.167259527466679270 ) ) ;
#136509 = CARTESIAN_POINT ( 'NONE',  ( -5.926849427829407269, 6.943687749669614995, -1.199719254218453823 ) ) ;
#136510 = CARTESIAN_POINT ( 'NONE',  ( 0.6801582343749970061, -0.4947916663252532876, 1.178068619123832983 ) ) ;
#136511 = CARTESIAN_POINT ( 'NONE',  ( 9.495732322661975644, -8.202835266173755357, -0.2934966634902085869 ) ) ;
#136512 =( BOUNDED_CURVE ( )  B_SPLINE_CURVE ( 2, ( #31119, #145953, #48439, #45239, #111355 ),
 .UNSPECIFIED., .F., .T. ) 
 B_SPLINE_CURVE_WITH_KNOTS ( ( 3, 2, 3 ),
 ( 0.2585522869718673844, 0.2625000000000000111, 0.2644396091801784476 ),
 .UNSPECIFIED. ) 
 CURVE ( )  GEOMETRIC_REPRESENTATION_ITEM ( )  RATIONAL_B_SPLINE_CURVE ( ( 0.9866594824841232736, 0.8730656178594444761, 1.000000000000000000, 0.9376339943847032954, 0.9333315137402016237 ) ) 
 REPRESENTATION_ITEM ( '' )  );
#136513 = CARTESIAN_POINT ( 'NONE',  ( 6.760220206081136496, -2.069995208266177666, 0.04663682477341199450 ) ) ;
#136514 = CARTESIAN_POINT ( 'NONE',  ( 1.393767942625488532, -2.000731169080074423, 0.2516357431460446992 ) ) ;
#136515 = CARTESIAN_POINT ( 'NONE',  ( -1.500000000000015099, -0.8395833326505166561, -0.8660254037844383745 ) ) ;
#136516 = CARTESIAN_POINT ( 'NONE',  ( 4.354074215503287881, 1.926045596674738514, -0.04874250487575670227 ) ) ;
#136517 = CARTESIAN_POINT ( 'NONE',  ( 1.364683531249996529, 11.46354166700806410, 0.7879004041258405033 ) ) ;
#136518 = COLOUR_RGB ( '', 0.66274510, 0.83137255, 0.94901961) ;
#136519 = CARTESIAN_POINT ( 'NONE',  ( 1.424421946217780732, -2.203867130488819548, 0.2783968414596868501 ) ) ;
#136521 = ORIENTED_EDGE ( 'NONE', *, *, #41655, .T. ) ;
#136520 = CARTESIAN_POINT ( 'NONE',  ( 8.703444544968814256, 12.24143683818393313, -1.199719254218446718 ) ) ;
#136522 = DIRECTION ( 'NONE',  ( 1.000000000000000000, 0.000000000000000000, -1.478457507935129867E-17 ) ) ;
#136523 = CARTESIAN_POINT ( 'NONE',  ( 1.499999999999959588, 7.750000000000000000, -10.86128356754324820 ) ) ;
#136524 = CARTESIAN_POINT ( 'NONE',  ( 3.623053363349855172, 5.249981562040033189, 1.599625672291267398 ) ) ;
#136525 = CARTESIAN_POINT ( 'NONE',  ( -0.4019237886466871523, 8.979914550367425363, -1.499999999999998668 ) ) ;
#136526 = CARTESIAN_POINT ( 'NONE',  ( 4.686888010602763721, 1.293897920562389947, 1.164242640570410714 ) ) ;
#136527 = CARTESIAN_POINT ( 'NONE',  ( 1.873419974815058842, -0.2433403713097622156, 1.946663811685337420 ) ) ;
#136529 = CARTESIAN_POINT ( 'NONE',  ( -0.6823417656249969321, 3.280208333674754062, -1.181850606188749264 ) ) ;
#136528 = CARTESIAN_POINT ( 'NONE',  ( 3.988069740714122791, 7.804498464141805592, 0.7998128361456321445 ) ) ;
#136530 = CARTESIAN_POINT ( 'NONE',  ( -4.884136011505287200, 6.706951837855620546, 1.250136565965910274 ) ) ;
#136531 = CARTESIAN_POINT ( 'NONE',  ( -11.41010744128099219, 2.630042260599918080, 3.716153451272427688 ) ) ;
#136532 = CARTESIAN_POINT ( 'NONE',  ( 6.496542546517183325, 1.940334402339534581, 0.2891159199209930031 ) ) ;
#136533 = CARTESIAN_POINT ( 'NONE',  ( -6.886651960737580680, 10.12184548991413457, -1.199719254218440723 ) ) ;
#136534 = EDGE_CURVE ( 'NONE', #195844, #205382, #172584, .T. ) ;
#136535 = CARTESIAN_POINT ( 'NONE',  ( -3.755245360860919757, 7.324943987738961049, -0.7216878364870257245 ) ) ;
#136536 = AXIS2_PLACEMENT_3D ( 'NONE', #72585, #57418, #139762 ) ;
#136537 = CARTESIAN_POINT ( 'NONE',  ( 0.8489190418228099722, 0.6593363751366092540, 2.164330503585075505 ) ) ;
#136539 = ORIENTED_EDGE ( 'NONE', *, *, #1866, .F. ) ;
#136538 = CARTESIAN_POINT ( 'NONE',  ( -5.693534442735004752, 8.729875052244421951, 1.199719254218452047 ) ) ;
#136540 = CARTESIAN_POINT ( 'NONE',  ( 0.7499999999999867883, -0.4020833326505157679, -1.299038105676652899 ) ) ;
#136541 = CARTESIAN_POINT ( 'NONE',  ( 1.334983872447586872, -1.693447605269988276, 0.7947349781701130711 ) ) ;
#136542 = CARTESIAN_POINT ( 'NONE',  ( -0.05262932013434371004, -1.547529252455181581, -0.7825623337873451879 ) ) ;
#136543 = CARTESIAN_POINT ( 'NONE',  ( 4.159861740090546434, 1.033864333764370702, 1.932389678422803181 ) ) ;
#136544 = CARTESIAN_POINT ( 'NONE',  ( 5.878008146920711496, 1.368277704907730374, 1.858044196986943675 ) ) ;
#136545 = CARTESIAN_POINT ( 'NONE',  ( 1.305620473665240366, -0.5016907458927004626, 1.998752541464960952 ) ) ;
#136546 = CARTESIAN_POINT ( 'NONE',  ( 3.785046133934614865, 1.407330997726879973, 1.338362524258763786 ) ) ;
#136547 = CARTESIAN_POINT ( 'NONE',  ( -5.056828107772872727, 5.001980335264194721, -0.7216878364870197293 ) ) ;
#136548 = CIRCLE ( 'NONE', #146921, 2.400000000000007461 ) ;
#136549 = CARTESIAN_POINT ( 'NONE',  ( 5.430866635118035468, 0.1366067128489474591, 1.865587184704711632 ) ) ;
#136550 = CARTESIAN_POINT ( 'NONE',  ( 0.6801582343749744686, 0.4739583336747441034, 1.178068619123803451 ) ) ;
#136551 = CARTESIAN_POINT ( 'NONE',  ( 4.465470312728934132, -1.956561007648183192, -0.4872041746135646889 ) ) ;
#136552 = CARTESIAN_POINT ( 'NONE',  ( -3.836594282542926226, 5.499112634431936542, 1.443375672974064550 ) ) ;
#136553 = CARTESIAN_POINT ( 'NONE',  ( -6.089547271193396227, 7.133501900260939443, -1.199719254218453823 ) ) ;
#136554 = CARTESIAN_POINT ( 'NONE',  ( 7.086107841436786181, 11.41887624831828418, 1.040834085586084257E-14 ) ) ;
#136556 = CARTESIAN_POINT ( 'NONE',  ( -6.743487189263854376, -7.020359948792041394, 6.692370362266554906 ) ) ;
#136555 = CARTESIAN_POINT ( 'NONE',  ( 1.137010146156680834, -1.651496384925277283, 0.7785749969668461778 ) ) ;
#136557 = CARTESIAN_POINT ( 'NONE',  ( -4.827585214917754719, 7.789877296449459365, -1.199719254218453823 ) ) ;
#136558 = CARTESIAN_POINT ( 'NONE',  ( -3.793249116773374841, 7.647484079536056356, 0.7998128361456350310 ) ) ;
#136559 = CARTESIAN_POINT ( 'NONE',  ( -10.22583553578405358, 2.999999999999999556, 7.498742284419905424 ) ) ;
#136560 = ORIENTED_EDGE ( 'NONE', *, *, #204060, .F. ) ;
#136561 = CARTESIAN_POINT ( 'NONE',  ( 6.491097285755237145, 1.794469726164525492, -1.013322515520258538 ) ) ;
#136562 = CARTESIAN_POINT ( 'NONE',  ( -5.085717018457573957, 8.947437264926888290, 0.7216878364870267237 ) ) ;
#136563 = CARTESIAN_POINT ( 'NONE',  ( -4.115063316947640715, 4.759660943649018705, 1.199719254218462483 ) ) ;
#136564 = CARTESIAN_POINT ( 'NONE',  ( -4.733481511527885210, 4.890303307122107590, -0.5491554243041256722 ) ) ;
#136565 = CARTESIAN_POINT ( 'NONE',  ( 6.129558478109055741, -0.2449627755865962375, 2.004677898944156489 ) ) ;
#136567 = ORIENTED_EDGE ( 'NONE', *, *, #53039, .T. ) ;
#136566 = CARTESIAN_POINT ( 'NONE',  ( 6.076846083367460238, -1.572777764080468321, 1.568860064416939037 ) ) ;
#136568 = CARTESIAN_POINT ( 'NONE',  ( -6.400331034103001748, 9.624747418832267698, 1.199719254218452935 ) ) ;
#136569 = CARTESIAN_POINT ( 'NONE',  ( 6.518772930072240790, 6.499656594706071822, -0.7998128361456281477 ) ) ;
#136570 = CARTESIAN_POINT ( 'NONE',  ( 5.489158015974754612, 1.818697853212094095, -0.9693054586683967910 ) ) ;
#136571 = CARTESIAN_POINT ( 'NONE',  ( 4.483046177357690176, -2.016033783801042034, -0.04667830911464498911 ) ) ;
#136572 = VERTEX_POINT ( 'NONE', #51741 ) ;
#136573 = EDGE_LOOP ( 'NONE', ( #186907, #198342 ) ) ;
#136574 = CARTESIAN_POINT ( 'NONE',  ( 10.56502152068524758, 11.25866949347406631, -3.405356014006697407 ) ) ;
#136575 = CARTESIAN_POINT ( 'NONE',  ( 3.728655938958122196, 4.308852335994623139, -1.199719254218446718 ) ) ;
#136576 =( BOUNDED_CURVE ( )  B_SPLINE_CURVE ( 3, ( #181866, #81192, #163516, #48703 ),
 .UNSPECIFIED., .F., .T. ) 
 B_SPLINE_CURVE_WITH_KNOTS ( ( 4, 4 ),
 ( 1.570796326795016462, 3.141592653589631468 ),
 .UNSPECIFIED. ) 
 CURVE ( )  GEOMETRIC_REPRESENTATION_ITEM ( )  RATIONAL_B_SPLINE_CURVE ( ( 1.000000000000000000, 0.8047378541244312178, 0.8047378541244312178, 1.000000000000000000 ) ) 
 REPRESENTATION_ITEM ( '' )  );
#136578 = ORIENTED_EDGE ( 'NONE', *, *, #65255, .T. ) ;
#136577 = CARTESIAN_POINT ( 'NONE',  ( -5.772739544368596043, 9.956889578397179363, -0.7998128361456362523 ) ) ;
#136579 = CARTESIAN_POINT ( 'NONE',  ( 4.757636082118741783, 8.295611710538327799, 0.7840751985381082534 ) ) ;
#136580 = CARTESIAN_POINT ( 'NONE',  ( 4.393907559866160994, 0.09612058942952760032, 2.013924333851605297 ) ) ;
#136581 = CARTESIAN_POINT ( 'NONE',  ( 4.083814069670049562, -1.821384084514931612, -0.2681248149544179227 ) ) ;
#136582 = CARTESIAN_POINT ( 'NONE',  ( 0.000000000000000000, 0.5000000000000004441, 0.000000000000000000 ) ) ;
#136583 = CARTESIAN_POINT ( 'NONE',  ( 2.280263026629821166, 1.421315682977505546, 1.817977143087915026 ) ) ;
#136584 = CARTESIAN_POINT ( 'NONE',  ( 3.413620815590684199, 7.204584394822967752, 0.7998128361456281477 ) ) ;
#136585 = CARTESIAN_POINT ( 'NONE',  ( 4.464260128311710041, 1.014592192358022338, 1.908665273222116543 ) ) ;
#136586 = CARTESIAN_POINT ( 'NONE',  ( 7.934546212495622086, 10.28005655271014795, -1.599625672291262513 ) ) ;
#136587 = CARTESIAN_POINT ( 'NONE',  ( -0.09434409087969403140, -0.8304652339055562660, -1.753633067539569490 ) ) ;
#136588 = CARTESIAN_POINT ( 'NONE',  ( -4.141125853970233806, 6.918731698685530063, -1.199719254218452047 ) ) ;
#136589 = CARTESIAN_POINT ( 'NONE',  ( -9.367496996949647325, 15.51845925588232333, 7.500000000809289524 ) ) ;
#136590 = CARTESIAN_POINT ( 'NONE',  ( -5.056828107772866510, 5.962349549565537643, -1.082531754730543971 ) ) ;
#136591 = CARTESIAN_POINT ( 'NONE',  ( 2.694054421766533203, -1.865511834602461949, -0.1395888279770511053 ) ) ;
#136592 = CARTESIAN_POINT ( 'NONE',  ( 6.754760782388981255, -1.524083220479439005, 1.250168222439652421 ) ) ;
#136594 = CARTESIAN_POINT ( 'NONE',  ( -6.400331034103001748, 9.624747418832267698, 1.199719254218452935 ) ) ;
#136593 = CARTESIAN_POINT ( 'NONE',  ( 1.499999999999985123, -1.172916665983846363, -0.8660254037844323793 ) ) ;
#136595 = CARTESIAN_POINT ( 'NONE',  ( 1.682535984017709874, -1.178549783888741320, 1.865657194899547733 ) ) ;
#136596 = ORIENTED_EDGE ( 'NONE', *, *, #9209, .F. ) ;
#136597 = CARTESIAN_POINT ( 'NONE',  ( 3.940069096733910037, 8.986657997193951530, -0.7749999999999996891 ) ) ;
#136598 = CARTESIAN_POINT ( 'NONE',  ( 4.029797971759831121, 5.724516938518342535, -1.599625672291255185 ) ) ;
#136599 = CARTESIAN_POINT ( 'NONE',  ( -5.382750679825375251, 6.238629533673094585, -1.199719254218446718 ) ) ;
#136600 = CARTESIAN_POINT ( 'NONE',  ( 11.96209379583854293, 13.82792940594236519, 0.9572398070798464609 ) ) ;
#136601 = CARTESIAN_POINT ( 'NONE',  ( 5.664905584638975533, -1.781982755157806908, -0.8436340872482649411 ) ) ;
#136602 = CARTESIAN_POINT ( 'NONE',  ( 6.375599228498684212, 2.210405824868751701, -0.6629917143727501738 ) ) ;
#136603 = CARTESIAN_POINT ( 'NONE',  ( 0.7132427667453158371, -1.655377960257615966, -1.052639099659122390 ) ) ;
#136604 = CARTESIAN_POINT ( 'NONE',  ( 4.012594160722949610, 0.7376926799337081286, 1.926325278971857236 ) ) ;
#136605 = CARTESIAN_POINT ( 'NONE',  ( 5.287316719649520991, 8.151991358691011769, -1.082531754730549078 ) ) ;
#136606 = CARTESIAN_POINT ( 'NONE',  ( 6.855582950365507244, 8.027210192628430718, -1.199719254218452047 ) ) ;
#136607 = ORIENTED_EDGE ( 'NONE', *, *, #198949, .T. ) ;
#136608 = CARTESIAN_POINT ( 'NONE',  ( 7.361714222096048310, 10.57212177821199184, -1.082531754730537976 ) ) ;
#136609 = CARTESIAN_POINT ( 'NONE',  ( -1.201851678989727383E-14, 3.134375000341420137, 1.575800808251672791 ) ) ;
#136610 = CARTESIAN_POINT ( 'NONE',  ( 1.255262969126037241E-15, 12.31951671548121219, -10.25000000000000000 ) ) ;
#136611 = CARTESIAN_POINT ( 'NONE',  ( 4.595850884908202261, 7.345281218159464665, -1.082531754730549078 ) ) ;
#136612 = CARTESIAN_POINT ( 'NONE',  ( 6.004372733575126020, 2.168386774327632160, 0.1126981005201161401 ) ) ;
#136614 = CARTESIAN_POINT ( 'NONE',  ( 5.495603940606402560, -1.841430844871448258, 0.006098274996368944698 ) ) ;
#136613 = CARTESIAN_POINT ( 'NONE',  ( 1.930226670627029684, 8.999999999999998224, 0.7750000000000004663 ) ) ;
#136615 = CARTESIAN_POINT ( 'NONE',  ( 11.92619526913699701, 12.69999999999998153, 1.328859060402682868 ) ) ;
#136616 = CARTESIAN_POINT ( 'NONE',  ( -4.260029445439560192, 7.236136616047151193, 2.419999999999999485 ) ) ;
#136617 = CARTESIAN_POINT ( 'NONE',  ( 0.6494046996203367561, 0.5928216254872006319, -1.774177939146783345 ) ) ;
#136618 = CARTESIAN_POINT ( 'NONE',  ( -5.229776604766065873, 6.614552831964506829, 1.409540066939333425 ) ) ;
#136619 = CARTESIAN_POINT ( 'NONE',  ( -10.87247189006428449, -6.708723052947955345, 0.1888596022590807721 ) ) ;
#136620 = CARTESIAN_POINT ( 'NONE',  ( 5.959663945170571075, 7.214374732172471383, -1.219933935757764099 ) ) ;
#136621 = CARTESIAN_POINT ( 'NONE',  ( 1.436035868020806738, -1.063167577064242142, -1.589284522738307448 ) ) ;
#136622 = CARTESIAN_POINT ( 'NONE',  ( 2.465387952175815744, 1.736178859682969700, -0.3425752158293988159 ) ) ;
#136623 = CARTESIAN_POINT ( 'NONE',  ( 6.217445370822936468, 1.674971474680493788, 1.116412877057591624 ) ) ;
#136625 = CARTESIAN_POINT ( 'NONE',  ( 4.376519623831674366, -0.4236097701148673900, -1.868001571610947043 ) ) ;
#136624 = CARTESIAN_POINT ( 'NONE',  ( -9.775592450653132204, 11.36361159963886891, -1.199719254218441611 ) ) ;
#136626 = CARTESIAN_POINT ( 'NONE',  ( -1.600055350837869428, 1.204204895297060096, 1.480038727545138766 ) ) ;
#136627 = CARTESIAN_POINT ( 'NONE',  ( 5.002387483831562953, 1.964158282178072312, 0.1467643733194800570 ) ) ;
#136628 = CARTESIAN_POINT ( 'NONE',  ( 0.1234922912959918878, 1.848187084301698757, 1.039613981531524400 ) ) ;
#136629 = CARTESIAN_POINT ( 'NONE',  ( -3.002240950422295995, 5.590032644546251817, -1.199719254218452935 ) ) ;
#136630 = CARTESIAN_POINT ( 'NONE',  ( 3.713615009860570915, -1.843089489661839053, 0.3189824552965599969 ) ) ;
#136632 = ORIENTED_EDGE ( 'NONE', *, *, #183283, .F. ) ;
#136631 = CARTESIAN_POINT ( 'NONE',  ( 6.375633740537438143, 1.648238817998586958, -0.5085109915310691564 ) ) ;
#136634 = CARTESIAN_POINT ( 'NONE',  ( 2.236732156574683827, 5.553345249405011508, 1.040834085586084257E-14 ) ) ;
#136633 = CARTESIAN_POINT ( 'NONE',  ( 3.721466898765386500, -0.1629207441977159332, 2.200919931280575170 ) ) ;
#136635 = EDGE_CURVE ( 'NONE', #193266, #14088, #195450, .T. ) ;
#136636 = CARTESIAN_POINT ( 'NONE',  ( 0.6823417656249899377, 3.238541667008085323, -1.181850606188754593 ) ) ;
#136637 = CARTESIAN_POINT ( 'NONE',  ( 0.6255240776356413290, 0.2040786869749251498, -2.052575575099666150 ) ) ;
#136638 = CARTESIAN_POINT ( 'NONE',  ( 6.262976894508937242, 9.394224579314053969, -1.199719254218440723 ) ) ;
#136640 = CARTESIAN_POINT ( 'NONE',  ( -8.157201976916404362, 12.66848607304450702, -0.7998128361456281477 ) ) ;
#136639 = CIRCLE ( 'NONE', #74320, 0.07999999999999998779 ) ;
#136641 = CARTESIAN_POINT ( 'NONE',  ( -1.120076944892877790, 15.44751560850434302, -11.90518184135781077 ) ) ;
#136642 = CARTESIAN_POINT ( 'NONE',  ( -3.632695093457760649, 6.325562478087638496, -1.199719254218452047 ) ) ;
#136643 = CARTESIAN_POINT ( 'NONE',  ( -5.578701055370745010, 7.405485896932115786, -1.243560882958130387 ) ) ;
#136644 = VERTEX_POINT ( 'NONE', #67939 ) ;
#136645 = CARTESIAN_POINT ( 'NONE',  ( 2.805202726412972858, -1.722705984639979704, 1.148039668612794051 ) ) ;
#136647 = CARTESIAN_POINT ( 'NONE',  ( -1.499999999999997780, 4.150000000000021672, 1.214306433183764966E-14 ) ) ;
#136646 = AXIS2_PLACEMENT_3D ( 'NONE', #79146, #145262, #212328 ) ;
#136648 = CARTESIAN_POINT ( 'NONE',  ( 3.662674053986138656, 7.424870162959149589, 0.7998128361456321445 ) ) ;
#136649 = CARTESIAN_POINT ( 'NONE',  ( -6.365373075063135211, 6.924066019909299818, 0.8511317711424144505 ) ) ;
#136650 = CARTESIAN_POINT ( 'NONE',  ( 1.225266875139136458, 1.782313340379863442, 0.9499306202595361182 ) ) ;
#136651 =( NAMED_UNIT ( * ) PLANE_ANGLE_UNIT ( ) SI_UNIT ( $, .RADIAN. ) );
#136652 = B_SPLINE_CURVE_WITH_KNOTS ( 'NONE', 3,
 ( #96607, #13186, #93406, #11041, #146426, #47861 ),
 .UNSPECIFIED., .F., .F.,
 ( 4, 2, 4 ),
 ( 0.000000000000000000, 0.0003767643964918265939, 0.0007535287929836531878 ),
 .UNSPECIFIED. ) ;
#136653 = CARTESIAN_POINT ( 'NONE',  ( 1.364683531249988535, 3.863541667008087543, 0.7879004041258500513 ) ) ;
#136654 = ORIENTED_EDGE ( 'NONE', *, *, #77746, .F. ) ;
#136656 = CARTESIAN_POINT ( 'NONE',  ( 8.270110514656021650, 11.63191745286530576, 1.082531754730557072 ) ) ;
#136655 = CARTESIAN_POINT ( 'NONE',  ( 0.1749903794560748460, 0.004523422195302355051, -1.955468523092759314 ) ) ;
#136657 = CARTESIAN_POINT ( 'NONE',  ( 6.643907658006512840, -0.09612306880287316280, -2.013924184692199137 ) ) ;
#136658 = CARTESIAN_POINT ( 'NONE',  ( 6.298046708350548251, -0.9096110389208410529, -1.686033347247811731 ) ) ;
#136659 = FACE_BOUND ( 'NONE', #95482, .T. ) ;
#136660 = CARTESIAN_POINT ( 'NONE',  ( 3.421585747727782678, -1.306972202059282218, -1.759028276249123168 ) ) ;
#136661 = CARTESIAN_POINT ( 'NONE',  ( -1.402160292154681736E-14, 1.868750000682816381, -1.732050807568863648 ) ) ;
#136662 = CARTESIAN_POINT ( 'NONE',  ( 2.548957913124219044, 0.2380835140640500114, 1.897471792728817386 ) ) ;
#136663 = CARTESIAN_POINT ( 'NONE',  ( -4.608882153641705059, 7.464447381635583412, -1.199719254218452047 ) ) ;
#136664 = CARTESIAN_POINT ( 'NONE',  ( 3.185802909086937973, 6.660594460669327255, 0.7216878364870317197 ) ) ;
#136666 = CARTESIAN_POINT ( 'NONE',  ( 1.335564786618839817, 0.5826355126458090394, -1.930425043884366865 ) ) ;
#136665 = CARTESIAN_POINT ( 'NONE',  ( 3.571793831781210127, 7.341190112860298100, -0.2923163854498100345 ) ) ;
#136667 = CARTESIAN_POINT ( 'NONE',  ( 1.364683531250000303, 10.81770833367473195, -0.7879004041258355073 ) ) ;
#136669 = CARTESIAN_POINT ( 'NONE',  ( -5.926849427829407269, 6.943687749669614995, -1.199719254218453823 ) ) ;
#136668 = CARTESIAN_POINT ( 'NONE',  ( 6.233935805145816467, 2.167428969419796125, 0.3234103439683775894 ) ) ;
#136671 = ORIENTED_EDGE ( 'NONE', *, *, #89227, .F. ) ;
#136670 = CARTESIAN_POINT ( 'NONE',  ( 2.977275877015468364, 1.638319938685417476, -0.5394319952881917457 ) ) ;
#136672 = CARTESIAN_POINT ( 'NONE',  ( 0.1394461523057084484, 7.629137130509043629, -2.319723760180956607 ) ) ;
#136673 = CARTESIAN_POINT ( 'NONE',  ( 7.983053520348166288, 8.207983950027992748, -0.7998128361456281477 ) ) ;
#136674 = CARTESIAN_POINT ( 'NONE',  ( 4.955668840994886359, 5.740367388370866131, 1.199719254218462483 ) ) ;
#136675 = PLANE ( 'NONE',  #106089 ) ;
#136676 = CARTESIAN_POINT ( 'NONE',  ( 1.258172656280614365, -1.962046632281065461, -0.003472340283867945618 ) ) ;
#136677 = FACE_OUTER_BOUND ( 'NONE', #151761, .T. ) ;
#136678 = CARTESIAN_POINT ( 'NONE',  ( 3.506755287428983792, 7.242964935309132990, 1.040834085586084257E-14 ) ) ;
#136679 = CARTESIAN_POINT ( 'NONE',  ( 0.1399997263886020860, 0.7221123407896400392, -2.083281383436136558 ) ) ;
#136680 = ORIENTED_EDGE ( 'NONE', *, *, #158371, .T. ) ;
#136681 = CARTESIAN_POINT ( 'NONE',  ( 4.020002786455856736, -1.806352922022226304, 0.1370799816429474904 ) ) ;
#136682 = AXIS2_PLACEMENT_3D ( 'NONE', #47681, #126862, #162487 ) ;
#136683 = ORIENTED_EDGE ( 'NONE', *, *, #58248, .F. ) ;
#136684 = CARTESIAN_POINT ( 'NONE',  ( 9.053093885623066939, 11.58502883802551153, -1.599625672291262513 ) ) ;
#136685 = CARTESIAN_POINT ( 'NONE',  ( 4.706615602599436343, 5.520081620234675412, 1.199719254218452935 ) ) ;
#136686 = CARTESIAN_POINT ( 'NONE',  ( 5.320911890206324379, 1.367686037040320768, -1.187891890861958899 ) ) ;
#136687 = CARTESIAN_POINT ( 'NONE',  ( 7.146556367734764770, 9.431011410480991231, 1.443375672974063439 ) ) ;
#136688 = DIRECTION ( 'NONE',  ( 0.000000000000000000, 1.000000000000000000, 0.000000000000000000 ) ) ;
#136689 = CARTESIAN_POINT ( 'NONE',  ( 5.880650534977156063, 5.984130091214588276, -0.1889179825720621597 ) ) ;
#136691 = CARTESIAN_POINT ( 'NONE',  ( 9.728138913005292210, 11.30824913904973705, -1.199719254218440723 ) ) ;
#136690 = CARTESIAN_POINT ( 'NONE',  ( 5.090230039108806892, 0.9569469540476289726, -1.596034515973473455 ) ) ;
#136692 = CARTESIAN_POINT ( 'NONE',  ( 2.724132717865447084, 1.901453608201342238, 0.2316716071539808575 ) ) ;
#136693 = DIRECTION ( 'NONE',  ( -0.6483454320283800199, 0.000000000000000000, 0.7613463080411786432 ) ) ;
#136694 = CARTESIAN_POINT ( 'NONE',  ( -11.37872555039425748, 6.127336012342636806, -3.407788289652350588 ) ) ;
#136695 = CARTESIAN_POINT ( 'NONE',  ( 9.499606442108964544, -9.901472054505708442, -0.08647222121513538362 ) ) ;
#136696 = CARTESIAN_POINT ( 'NONE',  ( 6.333067150914817312, 6.561202228921680479, 0.7216878364870358276 ) ) ;
#136697 = CARTESIAN_POINT ( 'NONE',  ( 7.782016984564060103, 9.141736572488651902, 1.082531754730558626 ) ) ;
#136698 = CARTESIAN_POINT ( 'NONE',  ( -3.469997250093771246, 6.135748327496311383, -1.199719254218452935 ) ) ;
#136699 = CARTESIAN_POINT ( 'NONE',  ( 7.032126278729658786, 15.00000000000000000, -9.944928355699694578 ) ) ;
#136700 = CIRCLE ( 'NONE', #167760, 10.25000000000000000 ) ;
#136701 = CARTESIAN_POINT ( 'NONE',  ( 1.271554197678253839, 1.246673013970694077, 1.678101005879296004 ) ) ;
#136702 = CARTESIAN_POINT ( 'NONE',  ( 6.717138760927786834, 6.801359740696030443, -0.7998128361456481317 ) ) ;
#136703 = CARTESIAN_POINT ( 'NONE',  ( 6.036148348713140876, 0.9492135318787934262, -1.676240969703364891 ) ) ;
#136704 = CARTESIAN_POINT ( 'NONE',  ( -3.554208825076827782, 7.298327395898266623, 0.7998128361456341429 ) ) ;
#136705 = CARTESIAN_POINT ( 'NONE',  ( 2.168725436055967570, -1.667931858681595880, -0.7425449061374130855 ) ) ;
#136706 = CARTESIAN_POINT ( 'NONE',  ( -6.509799877575655813, 5.178456542363094606, 2.499999999999998668 ) ) ;
#136707 = CARTESIAN_POINT ( 'NONE',  ( 2.267699027020404490, 0.5063876334258295975, -1.844086191983687062 ) ) ;
#136708 = CARTESIAN_POINT ( 'NONE',  ( 1.539439451811152493, 1.821048954109681706, -0.7507764504887379786 ) ) ;
#136709 = CARTESIAN_POINT ( 'NONE',  ( 3.790518096397344383, 1.638939831120878932, -1.041601972383674468 ) ) ;
#136710 = EDGE_LOOP ( 'NONE', ( #40947, #49445, #162157, #18128 ) ) ;
#136711 = CARTESIAN_POINT ( 'NONE',  ( -4.911752498546917423, 4.707425932596563278, -0.3822207396134598145 ) ) ;
#136712 = CARTESIAN_POINT ( 'NONE',  ( -4.492547798081878874, 6.334668079219206049, 1.599625672291263179 ) ) ;
#136714 = CARTESIAN_POINT ( 'NONE',  ( 3.920270587443940080, -2.114697630030224929, 0.1593259359235904837 ) ) ;
#136713 = CARTESIAN_POINT ( 'NONE',  ( 4.934241560730721510, 4.721313007132757811, 0.000000000000000000 ) ) ;
#136715 = CARTESIAN_POINT ( 'NONE',  ( 6.447678837262253104, -6.532648880269189107, 6.949550370341235350 ) ) ;
#136716 = CARTESIAN_POINT ( 'NONE',  ( 7.411503528164766763, 11.79850454950093841, 1.040834085586084257E-14 ) ) ;
#136717 = CARTESIAN_POINT ( 'NONE',  ( 6.114332400817464652, 6.016105027659348181, -0.05221600309115309591 ) ) ;
#136718 = CARTESIAN_POINT ( 'NONE',  ( -10.98535488200955079, 9.841774432527699901, -1.593017372382190766 ) ) ;
#136719 = CARTESIAN_POINT ( 'NONE',  ( 4.850785098639300408, 8.881276058379668825, -0.7998128361456481317 ) ) ;
#136720 = DIRECTION ( 'NONE',  ( 1.000000000000000000, 0.000000000000000000, 0.000000000000000000 ) ) ;
#136722 = CARTESIAN_POINT ( 'NONE',  ( 6.157435431667657610, 1.928259211291092123, -0.5899821858514133766 ) ) ;
#136721 = CARTESIAN_POINT ( 'NONE',  ( 3.967279163243800255, 0.2216459979678051528, -1.812115712870238537 ) ) ;
#136723 = DIRECTION ( 'NONE',  ( 0.000000000000000000, 0.000000000000000000, -1.000000000000000000 ) ) ;
#136724 = CARTESIAN_POINT ( 'NONE',  ( -9.978437869977950569, 11.70422760547153906, -1.082531754730539753 ) ) ;
#136725 = CARTESIAN_POINT ( 'NONE',  ( -4.762965077474956566, 8.286028185285090331, 0.8196324637163689975 ) ) ;
#136726 = CARTESIAN_POINT ( 'NONE',  ( 0.000000000000000000, 2.999999999999975131, 0.000000000000000000 ) ) ;
#136727 = CARTESIAN_POINT ( 'NONE',  ( 4.451927283622527654, 1.870250842541102410, -0.04591718433973044494 ) ) ;
#136728 = CARTESIAN_POINT ( 'NONE',  ( 8.762647353133951711, 9.117510088278095282, 1.040834085586084257E-14 ) ) ;
#136729 = CARTESIAN_POINT ( 'NONE',  ( 2.297378195909089982, 1.489297080225897574, 1.222053532002062903 ) ) ;
#136730 = CARTESIAN_POINT ( 'NONE',  ( 6.877797714452785094, -1.903667959252927533, 0.4735691183095217527 ) ) ;
#136731 = CARTESIAN_POINT ( 'NONE',  ( 1.364683531249997417, 8.796875000341403350, 2.602085213965210642E-15 ) ) ;
#136732 = CARTESIAN_POINT ( 'NONE',  ( -5.377780486114890124, 9.425827667109372143, 0.000000000000000000 ) ) ;
#136733 = CARTESIAN_POINT ( 'NONE',  ( 4.630273154266905777, 5.360739087188218122, 1.199719254218464037 ) ) ;
#136734 = CARTESIAN_POINT ( 'NONE',  ( -4.950135482320929370, 5.908151163196758482, -1.082531754730549967 ) ) ;
#136735 = AXIS2_PLACEMENT_3D ( 'NONE', #34758, #30529, #100832 ) ;
#136736 = CARTESIAN_POINT ( 'NONE',  ( 1.142374532877686644, 0.8619398222155623124, 1.934021905983105416 ) ) ;
#136737 = CARTESIAN_POINT ( 'NONE',  ( 10.70146331988817323, 11.37946204949139251, 0.7998128361456341429 ) ) ;
#136738 = CARTESIAN_POINT ( 'NONE',  ( 5.120015143727554729, 2.048507142264085701, -0.2983452141967629645 ) ) ;
#136740 = CARTESIAN_POINT ( 'NONE',  ( 4.051511279158463985, 7.758049153162790645, -0.5006740859710266944 ) ) ;
#136739 = CARTESIAN_POINT ( 'NONE',  ( 0.6965153189463432204, 1.505040478001760107, 1.060415605250275339 ) ) ;
#136741 = CARTESIAN_POINT ( 'NONE',  ( 5.924520554715382303, -1.662438412150448963, -1.587772413480701639 ) ) ;
#136742 = CARTESIAN_POINT ( 'NONE',  ( 4.202664430556241726, 7.846932902383524144, 0.7216878364870298324 ) ) ;
#136744 = SURFACE_STYLE_FILL_AREA ( #17618 ) ;
#136743 = CARTESIAN_POINT ( 'NONE',  ( 4.475600106286968582, 5.354526557823810151, -1.082531754730548412 ) ) ;
#136745 = CARTESIAN_POINT ( 'NONE',  ( 0.9555020568867471642, 0.4423240407584581035, -2.249030425913514541 ) ) ;
#136746 = CARTESIAN_POINT ( 'NONE',  ( -0.1000000000000028644, -9.999999999999994671, -9.579478065113972818 ) ) ;
#136747 = CARTESIAN_POINT ( 'NONE',  ( -5.611095471209320174, 7.639640364534566075, 1.599625672291263179 ) ) ;
#136748 = CARTESIAN_POINT ( 'NONE',  ( 6.193304230345664685, -0.6518728838521523627, 1.829399646200319252 ) ) ;
#136749 = ORIENTED_EDGE ( 'NONE', *, *, #177765, .T. ) ;
#136750 = CARTESIAN_POINT ( 'NONE',  ( 6.751597309481075726, 10.82068792779586985, 1.040834085586084257E-14 ) ) ;
#136751 = VERTEX_POINT ( 'NONE', #152435 ) ;
#136752 = CARTESIAN_POINT ( 'NONE',  ( -0.05247892273943338681, -1.838936383286099652, 0.8197664084235550819 ) ) ;
#136753 = CARTESIAN_POINT ( 'NONE',  ( 0.1333692844072559280, 0.001398348041498076455, -2.053671342968105051 ) ) ;
#136754 = CARTESIAN_POINT ( 'NONE',  ( -8.877891658850122880, 9.251961778280284321, 0.7998128361456462443 ) ) ;
#136755 = CARTESIAN_POINT ( 'NONE',  ( -1.642778471875000035, -0.2552083328553750308, -2.845375778867859751 ) ) ;
#136757 = CARTESIAN_POINT ( 'NONE',  ( 1.146904862891504173, -1.391901254704702273, -1.093021760518765539 ) ) ;
#136756 = CARTESIAN_POINT ( 'NONE',  ( 2.660199397079235695, -1.441175001385604393, 1.514759066650630093 ) ) ;
#136758 = CYLINDRICAL_SURFACE ( 'NONE', #67673, 1.224999999999996980 ) ;
#136759 = EDGE_CURVE ( 'NONE', #195016, #86803, #167615, .T. ) ;
#136761 = CARTESIAN_POINT ( 'NONE',  ( 4.013863964491473979, -1.177108192605724746, -1.966824220290509961 ) ) ;
#136760 = CARTESIAN_POINT ( 'NONE',  ( 4.004454267989866700, 5.765225627445230927, 1.599625672291262513 ) ) ;
#136762 = CARTESIAN_POINT ( 'NONE',  ( 3.028976774107559944, -1.169381637243168903, -1.289075744332576878 ) ) ;
#136763 = CARTESIAN_POINT ( 'NONE',  ( 4.566398809704347528, 4.221886787610169556, -0.7998128361456211532 ) ) ;
#136764 = CARTESIAN_POINT ( 'NONE',  ( 4.362691568547327314, 8.311833606605697256, -0.7998128361456381397 ) ) ;
#136765 = CARTESIAN_POINT ( 'NONE',  ( 3.655360161107966022, -0.3364991752431121808, -1.700650080047048318 ) ) ;
#136766 = CARTESIAN_POINT ( 'NONE',  ( 4.053319971960964274, 1.836175303466779374, -1.158372938815607656 ) ) ;
#136767 = CARTESIAN_POINT ( 'NONE',  ( 5.820528018968444961, 5.685037531751635953, 0.7998128361456341429 ) ) ;
#136768 = CARTESIAN_POINT ( 'NONE',  ( 4.364470425680367249, -1.957169923074707274, -0.4852690807995581057 ) ) ;
#136769 = CARTESIAN_POINT ( 'NONE',  ( 1.593750000000000666, -1.895863743164122983, -0.7852924748298991675 ) ) ;
#136770 = CARTESIAN_POINT ( 'NONE',  ( 0.7499999999999885647, 2.347916667349486453, -1.299038105676652899 ) ) ;
#136771 = CARTESIAN_POINT ( 'NONE',  ( 0.9910896068104644296, 1.700257414060426964, -0.9055851426933002601 ) ) ;
#136772 = CARTESIAN_POINT ( 'NONE',  ( 1.500000000000001332, 8.656250000682797818, 0.000000000000000000 ) ) ;
#136773 = CARTESIAN_POINT ( 'NONE',  ( 4.693709758858874537, 2.072258576215581183, -0.8006532145865407069 ) ) ;
#136774 = ORIENTED_EDGE ( 'NONE', *, *, #87175, .F. ) ;
#136775 = LINE ( 'NONE', #185497, #167250 ) ;
#136776 = CARTESIAN_POINT ( 'NONE',  ( -0.7500000000000215383, 1.941666666666688634, 1.299038105676659116 ) ) ;
#136777 = CARTESIAN_POINT ( 'NONE',  ( 7.935599982700328958, 8.152621489438862667, 0.7998128361456481317 ) ) ;
#136778 = CARTESIAN_POINT ( 'NONE',  ( 4.324687812634882000, 7.028924300507257250, 1.082531754730558626 ) ) ;
#136779 = CARTESIAN_POINT ( 'NONE',  ( 0.000000000000000000, 0.03624871340549007392, 0.000000000000000000 ) ) ;
#136780 = CARTESIAN_POINT ( 'NONE',  ( 0.1885310067011408963, 1.284270987554763765, 1.812239126532013689 ) ) ;
#136781 = CARTESIAN_POINT ( 'NONE',  ( 5.441838459065293065, 1.316327937319297758, 1.454900926449454124 ) ) ;
#136782 = CARTESIAN_POINT ( 'NONE',  ( 9.924205255523292024, 10.68058700763975466, -0.7216878364870257245 ) ) ;
#136783 = CARTESIAN_POINT ( 'NONE',  ( -0.3364766900451948706, 3.351562295342669806, 1.974266290975867699 ) ) ;
#136784 = CARTESIAN_POINT ( 'NONE',  ( 6.327429347084096101, -2.133486974870369313, 0.7532543551938327697 ) ) ;
#136785 = MECHANICAL_DESIGN_GEOMETRIC_PRESENTATION_REPRESENTATION (  '', ( #22635 ), #129894 ) ;
#136786 = CARTESIAN_POINT ( 'NONE',  ( -5.316205630334268406, 6.335233002545657577, -1.082531754730549967 ) ) ;
#136787 = CARTESIAN_POINT ( 'NONE',  ( 3.508308746731583216, 2.062851380131548229, 0.002797760368935045105 ) ) ;
#136788 = CARTESIAN_POINT ( 'NONE',  ( -4.771579997005698459, 7.654261532226910525, -1.199719254218452047 ) ) ;
#136789 = EDGE_CURVE ( 'NONE', #179029, #7836, #89720, .T. ) ;
#136790 = AXIS2_PLACEMENT_3D ( 'NONE', #66364, #33892, #17620 ) ;
#136791 = CARTESIAN_POINT ( 'NONE',  ( -1.499999999999997780, 4.431250000682819490, 1.214306433183764966E-14 ) ) ;
#136792 = CARTESIAN_POINT ( 'NONE',  ( 1.364683531249990311, 4.926041667008083991, 0.7879004041258500513 ) ) ;
#136794 = B_SPLINE_CURVE_WITH_KNOTS ( 'NONE', 3,
 ( #85399, #119033, #16107, #131024, #3055, #918, #114768, #163465 ),
 .UNSPECIFIED., .F., .F.,
 ( 4, 2, 2, 4 ),
 ( 0.000000000000000000, 0.0005156231957999649930, 0.0007734347936999474895, 0.001031246391599929986 ),
 .UNSPECIFIED. ) ;
#136793 = CARTESIAN_POINT ( 'NONE',  ( 4.639837347815604751, 0.8015432297804045980, -1.690266223530467293 ) ) ;
#136795 = CARTESIAN_POINT ( 'NONE',  ( 3.832397100292153524, 0.5799717274662331556, -1.634443932507266384 ) ) ;
#136796 = CARTESIAN_POINT ( 'NONE',  ( 3.860698480431251411, 0.2083224649859614919, -1.727840645513075923 ) ) ;
#136797 = CARTESIAN_POINT ( 'NONE',  ( 0.9961154782066735658, -2.292545471836278992, 0.006648471028786878678 ) ) ;
#136798 = CARTESIAN_POINT ( 'NONE',  ( 1.364683531249990311, 4.446875000341417028, 1.214306433183764966E-14 ) ) ;
#136799 = CARTESIAN_POINT ( 'NONE',  ( 4.405862271158119903, -0.8954353465763136288, -1.889446048457727789 ) ) ;
#136800 = CARTESIAN_POINT ( 'NONE',  ( 0.005434845660363255178, -0.7843016415976924449, -1.664241202765592176 ) ) ;
#136801 = DIRECTION ( 'NONE',  ( 0.7431448254773955764, 0.000000000000000000, 0.6691306063588566833 ) ) ;
#136802 = CARTESIAN_POINT ( 'NONE',  ( 1.178361531996233280, 1.528742360773158282, 1.314995429398260196 ) ) ;
#136803 = CARTESIAN_POINT ( 'NONE',  ( 0.5861907285475282947, -2.175377356269320828, -0.2643977408666315365 ) ) ;
#136804 = CARTESIAN_POINT ( 'NONE',  ( 7.826754997383993384, 14.96923099944252478, -9.976823565866945742 ) ) ;
#136805 = CARTESIAN_POINT ( 'NONE',  ( -8.552495972122143186, 8.872333477097637200, 0.7998128361456462443 ) ) ;
#136806 = CARTESIAN_POINT ( 'NONE',  ( 6.765682348419287173, 7.852049813699357728, 1.199719254218462483 ) ) ;
#136807 = CARTESIAN_POINT ( 'NONE',  ( 2.842561206135377994, 1.176089095116246153, -1.764248410475676820 ) ) ;
#136808 = DIRECTION ( 'NONE',  ( 0.000000000000000000, 0.000000000000000000, -1.000000000000000000 ) ) ;
#136809 = CARTESIAN_POINT ( 'NONE',  ( 5.531824841778981927, -1.161409778037244100, -1.408645805323349487 ) ) ;
#136810 = ORIENTED_EDGE ( 'NONE', *, *, #75639, .F. ) ;
#136811 = CARTESIAN_POINT ( 'NONE',  ( -6.282224075085783177, 8.422623735723785643, 1.599625672291269396 ) ) ;
#136812 = DIRECTION ( 'NONE',  ( -1.000000000000000000, 0.000000000000000000, 1.224646799147352961E-16 ) ) ;
#136813 = CARTESIAN_POINT ( 'NONE',  ( 1.642778471875000035, -1.363541666188707646, -2.845375778867859751 ) ) ;
#136814 = CARTESIAN_POINT ( 'NONE',  ( -8.369460898337653276, 8.658792557682392754, 0.7998128361456462443 ) ) ;
#136815 = CARTESIAN_POINT ( 'NONE',  ( 2.109634291106620818, 1.563931847922779728, 1.278184196155268904 ) ) ;
#136816 = CARTESIAN_POINT ( 'NONE',  ( 0.4289210115673793844, 2.015304021226202558, 0.6111801191295732627 ) ) ;
#136817 = CARTESIAN_POINT ( 'NONE',  ( 10.53876547652418338, 11.18964789890005918, 0.7998128361456462443 ) ) ;
#136818 = CARTESIAN_POINT ( 'NONE',  ( 3.819077715518546690, -1.639399709636097713, -0.8806717989592935947 ) ) ;
#136819 = CARTESIAN_POINT ( 'NONE',  ( 8.540746701604824409, 12.05162268759261224, -1.199719254218446718 ) ) ;
#136820 = CARTESIAN_POINT ( 'NONE',  ( 11.89844258446855818, 13.82852689329961215, -1.560502987793222163 ) ) ;
#136821 = ORIENTED_EDGE ( 'NONE', *, *, #32706, .T. ) ;
#136822 = CARTESIAN_POINT ( 'NONE',  ( -5.915435094264120508, 5.795762452929912101, 0.000000000000000000 ) ) ;
#136823 = CARTESIAN_POINT ( 'NONE',  ( -7.537443334193545397, 10.88110209227943770, -1.199719254218446718 ) ) ;
#136824 = CARTESIAN_POINT ( 'NONE',  ( 5.162654993523497993, -1.319871331358621669, 1.261628347558927166 ) ) ;
#136825 = VECTOR ( 'NONE', #211539, 1000.000000000000000 ) ;
#136827 = CARTESIAN_POINT ( 'NONE',  ( -3.990270464981529486, 7.829052896380438220, 0.2716399205876223744 ) ) ;
#136826 = CARTESIAN_POINT ( 'NONE',  ( -3.305155586681401303, 7.078041627762083898, 0.7998128361456352531 ) ) ;
#136828 = CARTESIAN_POINT ( 'NONE',  ( -1.364683531250000748, -0.9906249996585805295, 0.000000000000000000 ) ) ;
#136829 = CARTESIAN_POINT ( 'NONE',  ( 0.8426186123336505407, -0.9696909581486823360, 1.437080622210512360 ) ) ;
#136830 = CARTESIAN_POINT ( 'NONE',  ( 0.6029369919973374126, -1.732405018438128552, 0.1659646143751663805 ) ) ;
#136831 = CARTESIAN_POINT ( 'NONE',  ( 5.865930957382810895, 2.274600175340906638, -0.3886535673101945143 ) ) ;
#136832 = CARTESIAN_POINT ( 'NONE',  ( 6.586134412937156846, 6.778852895089745090, 0.3294091213778785887 ) ) ;
#136833 = CARTESIAN_POINT ( 'NONE',  ( 1.300152579660202923, -2.060967562519558705, -0.002860995899278336550 ) ) ;
#136834 = CARTESIAN_POINT ( 'NONE',  ( 6.518772930072240790, 6.499656594706071822, -0.7998128361456281477 ) ) ;
#136835 = EDGE_CURVE ( 'NONE', #36555, #168625, #115871, .T. ) ;
#136836 = CARTESIAN_POINT ( 'NONE',  ( 0.2103132415818432799, -1.556605082263945228, -1.280954711483893727 ) ) ;
#136837 = CARTESIAN_POINT ( 'NONE',  ( -1.225000000000042277, 0.9791666666666766217, -0.7072540797572898219 ) ) ;
#136838 = CARTESIAN_POINT ( 'NONE',  ( -5.237192476628793614, 9.332084666034067055, 0.7998128361456291469 ) ) ;
#136839 = CARTESIAN_POINT ( 'NONE',  ( 5.401189721097995111, 1.529905263132097071, 1.076157610686766075 ) ) ;
#136840 =( GEOMETRIC_REPRESENTATION_CONTEXT ( 3 ) GLOBAL_UNCERTAINTY_ASSIGNED_CONTEXT ( ( #99477 ) ) GLOBAL_UNIT_ASSIGNED_CONTEXT ( ( #108248, #159061, #158015 ) ) REPRESENTATION_CONTEXT ( 'NONE', 'WORKASPACE' ) );
#136842 = CARTESIAN_POINT ( 'NONE',  ( -5.483346782084204563, 5.361935765378481378, 0.000000000000000000 ) ) ;
#136841 = CARTESIAN_POINT ( 'NONE',  ( 3.884940529579200774, -1.786240503712609895, -0.6835825222790415934 ) ) ;
#136843 = CARTESIAN_POINT ( 'NONE',  ( 4.565167970240332274, -1.970479184476851886, -0.9938812724585781577 ) ) ;
#136844 = CARTESIAN_POINT ( 'NONE',  ( 1.224999999999976996, 1.666666667349515851, 0.7072540797572517413 ) ) ;
#136845 = CARTESIAN_POINT ( 'NONE',  ( -7.987977580929922716, -5.530730635397378414, -7.987977580929888077 ) ) ;
#136846 = CARTESIAN_POINT ( 'NONE',  ( 3.892599500454941630, 6.595097612955829192, 1.082531754730549078 ) ) ;
#136847 = VECTOR ( 'NONE', #148977, 1000.000000000000000 ) ;
#136848 = CARTESIAN_POINT ( 'NONE',  ( -5.492461626867567226, 6.540864998501174199, 1.082531754730549078 ) ) ;
#136849 = CARTESIAN_POINT ( 'NONE',  ( 6.129554906816851556, -0.2598956320666659381, 2.104415924757463419 ) ) ;
#136850 = ORIENTED_EDGE ( 'NONE', *, *, #159917, .T. ) ;
#136851 = CARTESIAN_POINT ( 'NONE',  ( 3.399772400530599370, 1.817812331725022101, 1.421335012277170629 ) ) ;
#136852 = CARTESIAN_POINT ( 'NONE',  ( 3.771884902471400292, -1.933230903833718539, 0.3329965046865584477 ) ) ;
#136853 = CARTESIAN_POINT ( 'NONE',  ( -3.949167883330528372, 7.829389307186077396, 1.214306433183764966E-14 ) ) ;
#136854 = CARTESIAN_POINT ( 'NONE',  ( 0.8659734994756922433, -1.952832785578303199, 0.1866259229855102009 ) ) ;
#136855 = SPHERICAL_SURFACE ( 'NONE', #16132, 0.08000000000000000167 ) ;
#136856 = CARTESIAN_POINT ( 'NONE',  ( -9.367496997602181352, 15.51845925588869690, 7.499999999994336974 ) ) ;
#136857 = ORIENTED_EDGE ( 'NONE', *, *, #60607, .T. ) ;
#136858 = CARTESIAN_POINT ( 'NONE',  ( 6.122279814772176643, 1.995267444086584296, 0.2910868170948808786 ) ) ;
#136859 = CARTESIAN_POINT ( 'NONE',  ( -7.374745490829552885, 10.69128794168811680, -1.199719254218446718 ) ) ;
#136860 = SURFACE_SIDE_STYLE ('',( #150979 ) ) ;
#136861 = CARTESIAN_POINT ( 'NONE',  ( 2.729531698892784242, 0.1106738598409856555, -2.168390435917330716 ) ) ;
#136862 = CARTESIAN_POINT ( 'NONE',  ( 3.854260808034858155, 7.718664386007802136, -0.7998128361456361413 ) ) ;
#136863 = CARTESIAN_POINT ( 'NONE',  ( 1.230900525853476868, 1.420129835883350955, -1.575055732827963295 ) ) ;
#136864 = CARTESIAN_POINT ( 'NONE',  ( 0.7499999999999885647, 1.597916667349486008, -1.299038105676652899 ) ) ;
#136865 = CARTESIAN_POINT ( 'NONE',  ( 9.402743226277308963, 10.92862083786708816, -1.199719254218446718 ) ) ;
#136866 = CARTESIAN_POINT ( 'NONE',  ( 0.3701041174201537554, 2.825470661167653663, -2.033038120852537656 ) ) ;
#136867 = CARTESIAN_POINT ( 'NONE',  ( 5.017113787211129328, 8.018716392533608683, 1.139262206072016559 ) ) ;
#136868 = ORIENTED_EDGE ( 'NONE', *, *, #135040, .T. ) ;
#136869 = CARTESIAN_POINT ( 'NONE',  ( 0.5794586325245559832, 1.923780613697351427, -0.7393501692522960189 ) ) ;
#136871 = CARTESIAN_POINT ( 'NONE',  ( 6.827182134110161726, 7.629137130509051623, 2.510944104600740356 ) ) ;
#136870 = CARTESIAN_POINT ( 'NONE',  ( -9.130526383799315582, 12.73969898348616070, 1.199719254218462483 ) ) ;
#136872 = CARTESIAN_POINT ( 'NONE',  ( 0.6823417656249882723, 1.426041667008083547, -1.181850606188749264 ) ) ;
#136873 = CARTESIAN_POINT ( 'NONE',  ( 4.082413651490639062, 7.776916670132135501, 0.000000000000000000 ) ) ;
#136874 = ORIENTED_EDGE ( 'NONE', *, *, #83130, .T. ) ;
#136875 = CARTESIAN_POINT ( 'NONE',  ( 4.020093958671668410, -1.906945023982812515, 0.1437811316862200317 ) ) ;
#136876 = CARTESIAN_POINT ( 'NONE',  ( 5.471497560916138703, 1.704843785431299219, -0.4750155384096472755 ) ) ;
#136877 = CARTESIAN_POINT ( 'NONE',  ( 5.091969210384201361, 8.098325291160362482, 1.199719254218452047 ) ) ;
#136878 = CARTESIAN_POINT ( 'NONE',  ( -3.440018289565379028, 5.036440642624797626, 1.599625672291267398 ) ) ;
#136879 = CARTESIAN_POINT ( 'NONE',  ( 0.07017708175168728413, 0.6932349927748741036, 1.673895389460538397 ) ) ;
#136881 = CARTESIAN_POINT ( 'NONE',  ( 1.288148359701014600, -0.6930021182445024186, -1.786147582385696486 ) ) ;
#136880 = CARTESIAN_POINT ( 'NONE',  ( -0.4308379095628913080, 6.611440747340219914, -3.285375171801879990 ) ) ;
#136882 = CARTESIAN_POINT ( 'NONE',  ( 1.522023487246677798, 2.040062638832959241, -0.3519594530456415793 ) ) ;
#136883 = CARTESIAN_POINT ( 'NONE',  ( -1.364683531250012516, 0.8427083336747532849, 0.7879004041258379498 ) ) ;
#136884 = CARTESIAN_POINT ( 'NONE',  ( 0.6023365795125863453, -0.6618663087945526602, -1.857178468014776263 ) ) ;
#136885 = CARTESIAN_POINT ( 'NONE',  ( 3.334410585898534674, 1.781380905032422746, 0.3990451814587444024 ) ) ;
#136887 = CARTESIAN_POINT ( 'NONE',  ( 5.975194856099406593, 7.098212677808693805, 1.080521340106417982 ) ) ;
#136886 = CARTESIAN_POINT ( 'NONE',  ( 0.2941754776928190429, 1.714430973684363257, 1.544913290951188012 ) ) ;
#136888 = ADVANCED_FACE ( 'NONE', ( #153506 ), #136198, .F. ) ;
#136889 = CARTESIAN_POINT ( 'NONE',  ( 1.364683531249986537, -0.1364583329919154264, 0.7879004041258500513 ) ) ;
#136890 = CARTESIAN_POINT ( 'NONE',  ( 4.088373676034792403, 1.106037789618707912, -1.740905279395239758 ) ) ;
#136891 = CARTESIAN_POINT ( 'NONE',  ( -5.280010757518168063, 8.247430752824802980, -1.199719254218446718 ) ) ;
#136892 = CARTESIAN_POINT ( 'NONE',  ( 6.740374924288304648, 11.01552117831172062, 1.040834085586084257E-14 ) ) ;
#136893 = DIRECTION ( 'NONE',  ( 3.330669073875478989E-16, -3.540251991789410786E-16, -1.000000000000000000 ) ) ;
#136894 = CARTESIAN_POINT ( 'NONE',  ( 4.493637847925535667, 7.329995691633395261, -1.199719254218452047 ) ) ;
#136896 = CARTESIAN_POINT ( 'NONE',  ( 1.499999999999989120, 3.275000000000020783, 1.214306433183764966E-14 ) ) ;
#136895 = CARTESIAN_POINT ( 'NONE',  ( 5.702208657235168232, -2.106147099624333219, -0.003344702849475410765 ) ) ;
#136897 = CARTESIAN_POINT ( 'NONE',  ( 6.637176860265922684, -0.09746846054551477900, -2.068182370504913159 ) ) ;
#136898 = CARTESIAN_POINT ( 'NONE',  ( 1.364683531249988535, 1.676041667008085101, 0.7879004041258500513 ) ) ;
#136899 = CARTESIAN_POINT ( 'NONE',  ( 4.200566210393744448, -0.6737006675727378324, -2.054019326127386691 ) ) ;
#136900 = CARTESIAN_POINT ( 'NONE',  ( 4.090493647085408746, -1.161108546167070488, 1.652349136562575760 ) ) ;
#136901 = FILL_AREA_STYLE_COLOUR ( '', #97791 ) ;
#136902 = EDGE_CURVE ( 'NONE', #49683, #53056, #137268, .T. ) ;
#136905 = CARTESIAN_POINT ( 'NONE',  ( 4.500943810056890371, 8.194925511800951412, -0.7216878364870207285 ) ) ;
#136904 = CARTESIAN_POINT ( 'NONE',  ( 3.285556943750000070, -3.784374999522041705, 0.000000000000000000 ) ) ;
#136903 = CARTESIAN_POINT ( 'NONE',  ( -9.508009452553693563, 15.00000000001204370, -7.612499999986095389 ) ) ;
#136906 = CARTESIAN_POINT ( 'NONE',  ( -6.252245114557387851, 7.323316050852266557, -1.199719254218453823 ) ) ;
#136907 = CARTESIAN_POINT ( 'NONE',  ( 2.817592499383800853, -1.357869084745389809, -1.490969456672403881 ) ) ;
#136908 = CARTESIAN_POINT ( 'NONE',  ( -9.040589502214116280, 9.441775928871617651, 0.7998128361456462443 ) ) ;
#136910 = CARTESIAN_POINT ( 'NONE',  ( -11.33772463945037146, 10.89999999999998259, 3.599999999999999201 ) ) ;
#136909 = CARTESIAN_POINT ( 'NONE',  ( -3.632695093457760649, 6.325562478087638496, -1.199719254218452047 ) ) ;
#136911 = CARTESIAN_POINT ( 'NONE',  ( 1.499999999999990674, 8.226407212580419070, 3.114167208185194990 ) ) ;
#136912 = CARTESIAN_POINT ( 'NONE',  ( 5.343983030329363615, -1.218012673290536974, -1.474316871017399944 ) ) ;
#136913 = CARTESIAN_POINT ( 'NONE',  ( 8.499999999999980460, 6.216000000000041048, 2.921333333333346882 ) ) ;
#136915 = CARTESIAN_POINT ( 'NONE',  ( 4.728138764314923748, 2.011206665557175199, 0.1455158850461671372 ) ) ;
#136914 = CARTESIAN_POINT ( 'NONE',  ( -7.659993601596710278, 10.92011438762942355, -1.082531754730543083 ) ) ;
#136916 = CARTESIAN_POINT ( 'NONE',  ( -1.499999999999997780, 5.650000000000023448, 1.214306433183764966E-14 ) ) ;
#136917 = CARTESIAN_POINT ( 'NONE',  ( -8.012344526598182026E-15, 8.546875000341403350, -1.575800808251669460 ) ) ;
#136918 = CARTESIAN_POINT ( 'NONE',  ( 6.686556848510641693, -1.692700875910668312, -0.3300756604382968362 ) ) ;
#136919 = CARTESIAN_POINT ( 'NONE',  ( 5.224688093219824303, 7.188831756880171397, -1.599625672291283607 ) ) ;
#136921 = CARTESIAN_POINT ( 'NONE',  ( -15.75000000000000000, 10.19999999999999929, -3.600000000000000977 ) ) ;
#136920 = CARTESIAN_POINT ( 'NONE',  ( 8.839552966430002101, 11.33589776563360019, -1.443375672974052559 ) ) ;
#136922 = DIRECTION ( 'NONE',  ( 1.000000000000000000, -7.771561172376097755E-16, -4.440892098500627148E-16 ) ) ;
#136923 = CARTESIAN_POINT ( 'NONE',  ( 5.219927230130699591, -0.9996001844756461363, -1.580852690948472361 ) ) ;
#136924 = CARTESIAN_POINT ( 'NONE',  ( 6.521754290436940771, -0.4404898795188401106, 1.971875975034496742 ) ) ;
#136925 = FILL_AREA_STYLE_COLOUR ( '', #185582 ) ;
#136926 = CARTESIAN_POINT ( 'NONE',  ( 1.956005403265232978, -0.7013823251572397499, 1.947930506816720087 ) ) ;
#136927 = CARTESIAN_POINT ( 'NONE',  ( -1.468321960012591409, 7.242494692102439124, -4.289992922803198994 ) ) ;
#136928 = ORIENTED_EDGE ( 'NONE', *, *, #166608, .T. ) ;
#136929 = CARTESIAN_POINT ( 'NONE',  ( 8.365017589507326434, 12.70301158782650397, -0.7216878364870338292 ) ) ;
#136931 = ADVANCED_FACE ( 'NONE', ( #121087 ), #802, .F. ) ;
#136930 = CARTESIAN_POINT ( 'NONE',  ( 0.8257962581623284892, 0.8146080751335778025, -1.844719337431327544 ) ) ;
#136932 = CARTESIAN_POINT ( 'NONE',  ( 1.669862777068024995, 1.806593842016694484, -0.1355503349984941153 ) ) ;
#136933 = CARTESIAN_POINT ( 'NONE',  ( 5.031484404002889654, 6.003058238492422483, 1.082531754730549078 ) ) ;
#136934 = FACE_OUTER_BOUND ( 'NONE', #24099, .T. ) ;
#136935 = CARTESIAN_POINT ( 'NONE',  ( 7.578644679914706472, 9.864838098032418401, 1.443375672974076540 ) ) ;
#136936 = AXIS2_PLACEMENT_3D ( 'NONE', #47875, #27317, #177857 ) ;
#136937 = CARTESIAN_POINT ( 'NONE',  ( 7.070740804726770357, 8.207951346058097286, 1.199719254218462483 ) ) ;
#136939 = CARTESIAN_POINT ( 'NONE',  ( 6.556256410252866651, -1.173993033552203968, 1.514159254448317782 ) ) ;
#136938 = CARTESIAN_POINT ( 'NONE',  ( -6.579784621333750749, 6.570836901177822931, 0.7998128361456341429 ) ) ;
#136940 = FILL_AREA_STYLE ('',( #152115 ) ) ;
#136941 = CARTESIAN_POINT ( 'NONE',  ( -4.296393142825893463, -0.4330127018922214077, 4.470011852588161361 ) ) ;
#136942 = ADVANCED_FACE ( 'NONE', ( #104765 ), #133015, .F. ) ;
#136943 = CARTESIAN_POINT ( 'NONE',  ( -10.99967557777140925, -6.699439830718301181, 0.09581361862939005714 ) ) ;
#136945 = ORIENTED_EDGE ( 'NONE', *, *, #102377, .T. ) ;
#136944 = CARTESIAN_POINT ( 'NONE',  ( 2.873965376416980355, 6.296784005887697155, -0.7216878364870267237 ) ) ;
#136946 = CARTESIAN_POINT ( 'NONE',  ( -2.839543107058306592, 5.400218493954923815, -1.199719254218446718 ) ) ;
#136947 = CARTESIAN_POINT ( 'NONE',  ( 3.116266767097406909, -1.064116542966097922, -1.881565754655416756 ) ) ;
#136948 = ADVANCED_FACE ( 'NONE', ( #34401 ), #100473, .T. ) ;
#136949 = CARTESIAN_POINT ( 'NONE',  ( -6.129694847154211423, 9.205042184104968328, -1.082531754730549967 ) ) ;
#136950 = CARTESIAN_POINT ( 'NONE',  ( 6.726253606155519371, 7.019919760035800316, -0.7216878364870458196 ) ) ;
#136951 = CARTESIAN_POINT ( 'NONE',  ( 1.178162429063234207, 2.088287186665960693, -0.3679680078583212333 ) ) ;
#136952 = CARTESIAN_POINT ( 'NONE',  ( 6.071303273277399271, 0.1315155018670917386, -1.820917815106848359 ) ) ;
#136953 = CARTESIAN_POINT ( 'NONE',  ( 1.844934828179781050, -1.667470251784016089, 1.051280099994149841 ) ) ;
#136954 = CARTESIAN_POINT ( 'NONE',  ( 4.535362393419643645, -0.08824616237496611670, 1.910463848342447202 ) ) ;
#136955 = FACE_OUTER_BOUND ( 'NONE', #104462, .T. ) ;
#136956 = CARTESIAN_POINT ( 'NONE',  ( 4.633233401965040521, 0.002145104102065781716, -1.969739563307022712 ) ) ;
#136957 = CARTESIAN_POINT ( 'NONE',  ( 0.9549039013059671399, 0.3793949951976150481, -1.904366508208689357 ) ) ;
#136958 = VERTEX_POINT ( 'NONE', #1879 ) ;
#136959 = CARTESIAN_POINT ( 'NONE',  ( -5.469788628470539926, 5.346117919495872783, -0.7998128361456362523 ) ) ;
#136960 = CARTESIAN_POINT ( 'NONE',  ( -4.821859908315634158, 5.654533310236863564, 1.199719254218452935 ) ) ;
#136962 = CARTESIAN_POINT ( 'NONE',  ( 6.007671464186834065, 7.141943142040370063, 1.082531754730549967 ) ) ;
#136961 = CARTESIAN_POINT ( 'NONE',  ( 8.555358625423188812, 9.940005470203933768, 1.199719254218462483 ) ) ;
#136964 = ORIENTED_EDGE ( 'NONE', *, *, #152781, .T. ) ;
#136963 = CARTESIAN_POINT ( 'NONE',  ( 5.215449470722859360, 1.565665547294055715, 1.097690013397538022 ) ) ;
#136965 = CARTESIAN_POINT ( 'NONE',  ( 0.9739772326014316528, 2.126351460888118883, -0.5901193814053447007 ) ) ;
#136966 = CARTESIAN_POINT ( 'NONE',  ( 7.721398836998394799, -5.907420853759296264, 7.721398836998372595 ) ) ;
#136967 = CARTESIAN_POINT ( 'NONE',  ( 6.340495571224031401, 1.157139813629002756, -1.647119299906736556 ) ) ;
#136968 = CARTESIAN_POINT ( 'NONE',  ( -9.604686356149274573, 4.518459255872632419, 7.193747284969079558 ) ) ;
#136969 = CARTESIAN_POINT ( 'NONE',  ( -0.01238645465998293969, 15.45067886748792851, 11.96329637218392072 ) ) ;
#136970 = CARTESIAN_POINT ( 'NONE',  ( -0.2766633939784177154, 6.383776174518168034, 3.145034899357514124 ) ) ;
#136971 = CARTESIAN_POINT ( 'NONE',  ( 3.104029480343179603, 0.7476448069429382226, -1.930825944200013966 ) ) ;
#136972 = CARTESIAN_POINT ( 'NONE',  ( -4.574986769607567894, 7.424902766929059261, 1.199719254218464037 ) ) ;
#136973 = AXIS2_PLACEMENT_3D ( 'NONE', #155775, #139540, #26826 ) ;
#136974 = CARTESIAN_POINT ( 'NONE',  ( -4.636404737997885661, 8.342837909782009120, -0.3584692566244596645 ) ) ;
#136976 = CARTESIAN_POINT ( 'NONE',  ( 1.147603855448702248, -1.704515299458901012, -1.329379018566230641 ) ) ;
#136975 = CARTESIAN_POINT ( 'NONE',  ( -5.440899717785814715, 5.242137847038546461, 0.7998128361456341429 ) ) ;
#136977 = FACE_OUTER_BOUND ( 'NONE', #133062, .T. ) ;
#136978 = CARTESIAN_POINT ( 'NONE',  ( 4.177320726786311056, 5.966903162707725805, -1.443375672974068769 ) ) ;
#136979 = CARTESIAN_POINT ( 'NONE',  ( -5.426287360647527258, 6.306760859481674864, -1.047964138152550406 ) ) ;
#136980 = CARTESIAN_POINT ( 'NONE',  ( 1.364683531249997417, 12.54687500034139980, 2.602085213965210642E-15 ) ) ;
#136982 = CARTESIAN_POINT ( 'NONE',  ( -6.140917232347002042, 6.129101290685087911, -0.7998128361456362523 ) ) ;
#136981 = CARTESIAN_POINT ( 'NONE',  ( 6.925078400183531713, 7.629137130509038300, 2.555651831298339616 ) ) ;
#136983 = CARTESIAN_POINT ( 'NONE',  ( 5.625553438129872852, 0.3468616029342861951, 1.698903693450015684 ) ) ;
#136984 = CARTESIAN_POINT ( 'NONE',  ( -4.223528545856940042, 4.886203710709899006, -1.199719254218446718 ) ) ;
#136985 = CARTESIAN_POINT ( 'NONE',  ( 3.748938768049938197, -0.3990674421511587466, -2.031259957477090428 ) ) ;
#136986 = CARTESIAN_POINT ( 'NONE',  ( 4.095393968650405725, -0.3601260033815486539, 2.086223071001345630 ) ) ;
#136987 = CARTESIAN_POINT ( 'NONE',  ( 7.558834334818744338, 8.777393797832065303, 1.199719254218462483 ) ) ;
#136988 = CARTESIAN_POINT ( 'NONE',  ( -1.201851678989727383E-14, 4.696875000341419693, -1.575800808251660134 ) ) ;
#136989 = CARTESIAN_POINT ( 'NONE',  ( 2.606253914610905387, 1.968914028630329272, 0.05319026939461755227 ) ) ;
#136990 = CARTESIAN_POINT ( 'NONE',  ( 0.8262462788446511830, -0.8622288892402606431, -1.707089296137359158 ) ) ;
#136991 = CARTESIAN_POINT ( 'NONE',  ( 4.365347222306335873, 2.224029864950861857, -0.5546456485611241938 ) ) ;
#136992 = CARTESIAN_POINT ( 'NONE',  ( 2.103868193876055503, -1.825329726703457833, 0.04394198290156441783 ) ) ;
#136993 = CARTESIAN_POINT ( 'NONE',  ( 5.228604516725597229, 6.129068686715179126, -1.199719254218450271 ) ) ;
#136994 = CARTESIAN_POINT ( 'NONE',  ( 6.168596704093459060, 7.259412911939593371, -1.082531754730543083 ) ) ;
#136995 = CARTESIAN_POINT ( 'NONE',  ( -7.914208982075130905, 10.25632978388623684, -1.599625672291263179 ) ) ;
#136996 = CARTESIAN_POINT ( 'NONE',  ( 2.390887483786011014, -1.927808053674067823, -0.5802275739894193762 ) ) ;
#136997 = CARTESIAN_POINT ( 'NONE',  ( 3.608209768781400761, 1.961936380018937331, 0.004537341891153179319 ) ) ;
#136998 = CARTESIAN_POINT ( 'NONE',  ( -6.645467848992654858, 10.90479625713344625, 0.7998128361456481317 ) ) ;
#136999 = CARTESIAN_POINT ( 'NONE',  ( -4.924636110261798372, 6.768494766770632332, 1.599625672291267398 ) ) ;
#137000 = CARTESIAN_POINT ( 'NONE',  ( 0.07536363704237906969, 4.084105538841027894, -2.698926661290324880 ) ) ;
#137002 = CARTESIAN_POINT ( 'NONE',  ( 5.084699950150380232, -0.2187599903600515594, -1.756180685135479091 ) ) ;
#137001 = CARTESIAN_POINT ( 'NONE',  ( 6.456985077987440924, 0.3587005216530990692, -2.059463350302393359 ) ) ;
#137003 = CARTESIAN_POINT ( 'NONE',  ( -1.225000000000038058, 2.270833333333395210, 0.7072540797572858251 ) ) ;
#137004 = EDGE_CURVE ( 'NONE', #155662, #93347, #23474, .T. ) ;
#137005 = CARTESIAN_POINT ( 'NONE',  ( 1.324469081069843623, 2.112754910877081560, 0.5817525768514880680 ) ) ;
#137006 = CARTESIAN_POINT ( 'NONE',  ( -0.1123202547218312558, -0.3730905450354308206, -1.705658634530213602 ) ) ;
#137007 = CARTESIAN_POINT ( 'NONE',  ( 5.777746017718023097, 9.892454120646377191, 0.7998128361456462443 ) ) ;
#137008 = CARTESIAN_POINT ( 'NONE',  ( 3.469446951953614189E-15, 8.900000000000025224, 1.214306433183764966E-14 ) ) ;
#137009 = CARTESIAN_POINT ( 'NONE',  ( 0.3163000706473735879, -1.844146670390820475, 1.371622413452098233 ) ) ;
#137010 = CARTESIAN_POINT ( 'NONE',  ( 0.01162390915069450026, -2.148011843722149372, 0.4338911918742721641 ) ) ;
#137011 = CARTESIAN_POINT ( 'NONE',  ( 6.415404398373737216, 0.5482957075174756945, 1.644958459601528755 ) ) ;
#137012 = CARTESIAN_POINT ( 'NONE',  ( 3.176612885197922953, -1.314426786483071208, 1.772596291930063739 ) ) ;
#137013 = CARTESIAN_POINT ( 'NONE',  ( 0.2687526973377635797, -0.9260139170579514412, -1.961338766822422919 ) ) ;
#137014 = CYLINDRICAL_SURFACE ( 'NONE', #186377, 0.5000000000000003331 ) ;
#137015 = CARTESIAN_POINT ( 'NONE',  ( 1.270887751945870336, -0.3167050496251391234, -2.093436144997854687 ) ) ;
#137016 = CARTESIAN_POINT ( 'NONE',  ( 3.687500000000002665, -1.451031289060967788, 1.451031289061265550 ) ) ;
#137017 = CARTESIAN_POINT ( 'NONE',  ( 6.727182134110222478, 7.629137130509071163, 2.789055895399249252 ) ) ;
#137018 = CARTESIAN_POINT ( 'NONE',  ( 5.807627864512785898, -0.4676060548664852101, 1.868651349408587681 ) ) ;
#137019 = EDGE_LOOP ( 'NONE', ( #120760, #52173, #161004, #110250 ) ) ;
#137021 = CARTESIAN_POINT ( 'NONE',  ( -0.7499999999999972244, 5.858333333333353821, -1.299038105676652011 ) ) ;
#137020 = CARTESIAN_POINT ( 'NONE',  ( 1.558568218312964326, -1.617219677351620089, 1.624929221499067600 ) ) ;
#137022 = CARTESIAN_POINT ( 'NONE',  ( 5.183294799126148433, 4.941598775268944976, 1.040834085586084257E-14 ) ) ;
#137023 = CARTESIAN_POINT ( 'NONE',  ( 6.844168616800228477, 6.879284895888727824, -0.7998128361456281477 ) ) ;
#137024 = CARTESIAN_POINT ( 'NONE',  ( 3.440272213978716742, -1.324219266349660806, -1.783276862766651760 ) ) ;
#137025 = CARTESIAN_POINT ( 'NONE',  ( -8.568389894156720032, 10.05917163368005163, 1.082531754730558626 ) ) ;
#137026 = CARTESIAN_POINT ( 'NONE',  ( 5.450014563013511726, 8.341805509282339770, -1.082531754730543083 ) ) ;
#137027 = EDGE_CURVE ( 'NONE', #82118, #185927, #147213, .T. ) ;
#137028 = CARTESIAN_POINT ( 'NONE',  ( -8.527715432871366019, 10.01171809551380143, 1.082531754730558626 ) ) ;
#137029 = CARTESIAN_POINT ( 'NONE',  ( 4.245111494854632461, 7.966730820723463502, 0.000000000000000000 ) ) ;
#137030 = ORIENTED_EDGE ( 'NONE', *, *, #166683, .T. ) ;
#137031 = CARTESIAN_POINT ( 'NONE',  ( 1.442029965644067158, -1.730867108953790590, -1.034163949609874233 ) ) ;
#137033 = CARTESIAN_POINT ( 'NONE',  ( 6.812941044521420686, -1.596950470092706853, 1.305146078352089845 ) ) ;
#137032 = CARTESIAN_POINT ( 'NONE',  ( 8.423693512792301163, 8.722063941212843119, 0.7998128361456481317 ) ) ;
#137034 = CARTESIAN_POINT ( 'NONE',  ( -10.99387514841215463, -6.699757570937981299, 0.3793797362571516008 ) ) ;
#137035 = CARTESIAN_POINT ( 'NONE',  ( 4.977251789548238214, 7.860525283564661514, -1.082531754730548412 ) ) ;
#137036 = CARTESIAN_POINT ( 'NONE',  ( 0.04610459085982108324, -1.479553692838073475, 1.095721268101347734 ) ) ;
#137037 = CARTESIAN_POINT ( 'NONE',  ( 1.364683531249988535, 2.113541667008087099, 0.7879004041258500513 ) ) ;
#137038 = CARTESIAN_POINT ( 'NONE',  ( 1.791920237496129609, -1.760627435414298558, -0.1794978127376868071 ) ) ;
#137039 = CARTESIAN_POINT ( 'NONE',  ( 0.0006249722829775038483, -1.976948959267275541, 0.3961041280396286890 ) ) ;
#137040 = CARTESIAN_POINT ( 'NONE',  ( 6.462468575563847573, -1.595429648854440385, -0.6960047898553810564 ) ) ;
#137041 = CARTESIAN_POINT ( 'NONE',  ( 4.124787647867947271, 0.1125639427311639490, 2.289740828591101174 ) ) ;
#137042 = CARTESIAN_POINT ( 'NONE',  ( 3.908013947242465314, 1.300727540704300633, -1.303293010247716488 ) ) ;
#137043 = EDGE_CURVE ( 'NONE', #2366, #137116, #48674, .T. ) ;
#137044 = CARTESIAN_POINT ( 'NONE',  ( 7.397945374551106568, 11.78268670361832093, -0.7998128361456291469 ) ) ;
#137045 = CARTESIAN_POINT ( 'NONE',  ( 9.086253353280454803, 13.39999999999999680, -7.838367176906162470 ) ) ;
#137046 = CARTESIAN_POINT ( 'NONE',  ( 3.944226942909400346, 1.816763600636053688, 0.1792749827478901103 ) ) ;
#137047 = CARTESIAN_POINT ( 'NONE',  ( 4.817029820108094995, 1.034167108704350024, -1.730865207599366240 ) ) ;
#137048 = CARTESIAN_POINT ( 'NONE',  ( -7.994504133552415404, 12.47867192245318435, -0.7998128361456281477 ) ) ;
#137050 = CARTESIAN_POINT ( 'NONE',  ( -7.391130018105325661, 8.652015104991543026, -1.199719254218452047 ) ) ;
#137049 = CARTESIAN_POINT ( 'NONE',  ( 2.923041840916926315, 2.129999922893408559, 0.7632657742467786610 ) ) ;
#137051 = CARTESIAN_POINT ( 'NONE',  ( 0.1882882188262140766, -0.9905318517600868455, 1.858590670187587612 ) ) ;
#137052 = CARTESIAN_POINT ( 'NONE',  ( 1.387358672525637715, 7.251968950354889643, -4.302625267139783993 ) ) ;
#137053 = CARTESIAN_POINT ( 'NONE',  ( 3.402844027952243167, 0.5003511028610057032, 2.008882729757965890 ) ) ;
#137054 = CARTESIAN_POINT ( 'NONE',  ( 4.701980345841006326, 4.380065246436280368, 0.7998128361456341429 ) ) ;
#137055 = CARTESIAN_POINT ( 'NONE',  ( -0.6801582343750229853, 1.380208333674720622, -1.178068619123855409 ) ) ;
#137056 = CARTESIAN_POINT ( 'NONE',  ( 5.672555391165950311, 0.8593836824349295744, 1.938725756316476589 ) ) ;
#137057 = AXIS2_PLACEMENT_3D ( 'NONE', #92464, #187781, #89248 ) ;
#137059 = CARTESIAN_POINT ( 'NONE',  ( 1.523919215901398783, -1.069746099203742418, -1.602010878309991559 ) ) ;
#137058 = CARTESIAN_POINT ( 'NONE',  ( -8.642432853707342488, 12.17025653171218558, 1.199719254218462483 ) ) ;
#137060 = CARTESIAN_POINT ( 'NONE',  ( -3.285556943750000070, -0.1093749995220438809, 0.000000000000000000 ) ) ;
#137061 = CARTESIAN_POINT ( 'NONE',  ( 6.631706394207740551, 1.885626601332585306, -0.5685293109318545479 ) ) ;
#137062 = CARTESIAN_POINT ( 'NONE',  ( 3.729901657090948230, 6.405283462364505631, 1.082531754730549078 ) ) ;
#137063 = CARTESIAN_POINT ( 'NONE',  ( 5.891030527642284298, 5.977876296848656956, -0.06656325335930267373 ) ) ;
#137064 = CARTESIAN_POINT ( 'NONE',  ( 1.220146605508150803E-14, 9.468750000682799595, -1.499999999999998446 ) ) ;
#137065 = CARTESIAN_POINT ( 'NONE',  ( -5.576481253922474401, 5.400316305864651056, -0.7998128361456221525 ) ) ;
#137066 = CARTESIAN_POINT ( 'NONE',  ( 0.8619570425896695420, -1.755772037458620316, -1.360811342731186979 ) ) ;
#137067 = CARTESIAN_POINT ( 'NONE',  ( 3.083145409929681335, -0.1532580487927890645, -2.100430568508942830 ) ) ;
#137068 = CARTESIAN_POINT ( 'NONE',  ( -6.563028877466991595, 9.814561569423593923, 1.199719254218452935 ) ) ;
#137069 = CARTESIAN_POINT ( 'NONE',  ( 6.588372581236919601, 9.773852880496709972, -1.199719254218440723 ) ) ;
#137070 = CARTESIAN_POINT ( 'NONE',  ( 0.5372768211588532239, 1.738583335619352077, -0.6644854061606010331 ) ) ;
#137071 = CARTESIAN_POINT ( 'NONE',  ( 4.964256800898067645, 8.943383367689749619, 0.7998128361456462443 ) ) ;
#137072 = CARTESIAN_POINT ( 'NONE',  ( 3.499976210622149253, 7.235056012367825140, 0.7998128361456321445 ) ) ;
#137073 = CARTESIAN_POINT ( 'NONE',  ( -7.160114521792834807, 8.486460042580672436, 1.082531754730549078 ) ) ;
#137074 = CARTESIAN_POINT ( 'NONE',  ( -9.341204650135658483, 10.00041963468749984, 1.040834085586084257E-14 ) ) ;
#137075 = CARTESIAN_POINT ( 'NONE',  ( 1.090261293813089560, 1.267680250814690934, 1.699812782343253170 ) ) ;
#137076 = CARTESIAN_POINT ( 'NONE',  ( -5.915100157312088491, 10.12297696016459092, -0.7998128361456362523 ) ) ;
#137078 = CARTESIAN_POINT ( 'NONE',  ( 3.543363863352413823, 1.774678991803163575, -0.8365776047038612218 ) ) ;
#137077 = CARTESIAN_POINT ( 'NONE',  ( 1.224999999999974998, 0.6041666666666989371, 0.7072540797572456350 ) ) ;
#137079 = CARTESIAN_POINT ( 'NONE',  ( 2.483474991488154870, 1.976725341044349271, -0.8753317036461552014 ) ) ;
#137080 = CARTESIAN_POINT ( 'NONE',  ( 1.206327419354651820, 1.623952629372883427, 0.8676893986077349741 ) ) ;
#137082 = CARTESIAN_POINT ( 'NONE',  ( -4.822091459260241741, 6.758233420496813082, -1.248138317850192580 ) ) ;
#137081 = CARTESIAN_POINT ( 'NONE',  ( -3.526002468005825286, 6.271364091718859335, -1.199719254218450271 ) ) ;
#137083 = CARTESIAN_POINT ( 'NONE',  ( 3.802475355173411842, 1.493833042257145305, 0.8925963562203437229 ) ) ;
#137084 = CARTESIAN_POINT ( 'NONE',  ( 1.050790385994986309, 14.00000000000000711, -12.64745918785790657 ) ) ;
#137085 = CARTESIAN_POINT ( 'NONE',  ( 5.666945020832177882, 6.674152614801420746, 1.082531754730558626 ) ) ;
#137086 = CARTESIAN_POINT ( 'NONE',  ( -10.83925572545688176, 5.627432043407306850, 6.488667418600651438 ) ) ;
#137087 = CARTESIAN_POINT ( 'NONE',  ( 0.7784641540938314064, -1.199969256800371697, 1.797863220954009966 ) ) ;
#137088 = EDGE_CURVE ( 'NONE', #56038, #141384, #109606, .T. ) ;
#137089 = CARTESIAN_POINT ( 'NONE',  ( 3.848982377512807140, -0.9961485462514390044, 1.752762419822328832 ) ) ;
#137090 = CARTESIAN_POINT ( 'NONE',  ( 1.499999999999996891, 12.92708333401612997, -0.8660254037844378194 ) ) ;
#137091 = CARTESIAN_POINT ( 'NONE',  ( 0.5323697292517782786, 1.110078392871534314, -1.854780036684190669 ) ) ;
#137092 = SHAPE_REPRESENTATION ( 'positive pin', ( #200407 ), #197031 ) ;
#137093 = CARTESIAN_POINT ( 'NONE',  ( 3.696128747971284323, -1.969148060776576337, -0.09815990810512796594 ) ) ;
#137094 = VECTOR ( 'NONE', #121889, 1000.000000000000000 ) ;
#137095 = CARTESIAN_POINT ( 'NONE',  ( 6.509000000000035868, 7.629137130509092479, 2.600000000000000977 ) ) ;
#137096 = CARTESIAN_POINT ( 'NONE',  ( 2.788543057918268619, 1.664307371569521132, -1.000645113138714848 ) ) ;
#137099 = VERTEX_POINT ( 'NONE', #40836 ) ;
#137098 = CARTESIAN_POINT ( 'NONE',  ( -4.502716413514301408, 7.306900678191715848, -1.082531754730549967 ) ) ;
#137097 = CARTESIAN_POINT ( 'NONE',  ( -11.04536101718726293, 10.09542727035991483, 1.099999999999998757 ) ) ;
#137100 = CARTESIAN_POINT ( 'NONE',  ( -5.600926855776894975, 6.667407765562058053, -1.082531754730549967 ) ) ;
#137101 = CARTESIAN_POINT ( 'NONE',  ( 4.603875680292229156, 7.528882839386387360, 1.199719254218452047 ) ) ;
#137102 = CARTESIAN_POINT ( 'NONE',  ( -4.281342646865346602, 8.216926531310035031, 0.7998128361456352531 ) ) ;
#137103 = CARTESIAN_POINT ( 'NONE',  ( -5.932574734431526942, 9.079031735882207244, 1.199719254218454489 ) ) ;
#137104 = CARTESIAN_POINT ( 'NONE',  ( -2.788906526875773208E-15, 11.96875000068279604, -1.499999999999998446 ) ) ;
#137105 = CARTESIAN_POINT ( 'NONE',  ( 6.493248230727125758, 2.012220109224418518, -1.129477038640940734 ) ) ;
#137106 = DIRECTION ( 'NONE',  ( 0.000000000000000000, 0.000000000000000000, -1.000000000000000000 ) ) ;
#137107 = CARTESIAN_POINT ( 'NONE',  ( 4.575024454672827368, 1.791946274209740952, 0.7988320279663924106 ) ) ;
#137108 = CARTESIAN_POINT ( 'NONE',  ( 6.421758314367153275, 10.64380180007036891, -0.7998128361456291469 ) ) ;
#137109 = CARTESIAN_POINT ( 'NONE',  ( 1.529922885524273912, -1.701946718671920600, 1.081067414773040802 ) ) ;
#137110 = ORIENTED_EDGE ( 'NONE', *, *, #63516, .F. ) ;
#137111 = CARTESIAN_POINT ( 'NONE',  ( 2.132168502032088409, 2.116975549207784635, 0.04667972686168975205 ) ) ;
#137112 = CARTESIAN_POINT ( 'NONE',  ( 1.499999999999989120, 1.556250000682817047, 0.000000000000000000 ) ) ;
#137114 = CARTESIAN_POINT ( 'NONE',  ( -5.422371370461663176, 8.413518134592214537, -1.199719254218446718 ) ) ;
#137113 = CARTESIAN_POINT ( 'NONE',  ( -2.785310492603665367, 5.336947110424484109, 1.199719254218462483 ) ) ;
#137115 = CARTESIAN_POINT ( 'NONE',  ( 3.169683937527142170, -1.096016708463069422, 1.479218548343118389 ) ) ;
#137116 = VERTEX_POINT ( 'NONE', #141565 ) ;
#137117 = CARTESIAN_POINT ( 'NONE',  ( -10.13202086811422475, 10.71511252242175161, -0.7998128361456291469 ) ) ;
#137118 = CARTESIAN_POINT ( 'NONE',  ( 10.35123481171224569, 10.47441674329072114, 5.983190950231344729 ) ) ;
#137119 = CARTESIAN_POINT ( 'NONE',  ( 4.060867369437678676, 0.5686956411946364476, 2.042824496258560441 ) ) ;
#137120 = CARTESIAN_POINT ( 'NONE',  ( 5.452350330990040739, 9.512825819463730070, 0.7998128361456462443 ) ) ;
#137121 = ADVANCED_FACE ( 'NONE', ( #110154 ), #131704, .F. ) ;
#137122 = CARTESIAN_POINT ( 'NONE',  ( 4.358703909566331802, -1.529595902882211256, 1.381216288725060082 ) ) ;
#137124 = CARTESIAN_POINT ( 'NONE',  ( 2.384105128782065819, -0.3166398734758494315, -1.813660976904336808 ) ) ;
#137123 = CARTESIAN_POINT ( 'NONE',  ( -6.958359152311683893, 9.141171649162195934, -1.599625672291263179 ) ) ;
#137125 = CARTESIAN_POINT ( 'NONE',  ( 9.284636267260101050, 9.726497154758602548, -0.7998128361456281477 ) ) ;
#137126 =( LENGTH_UNIT ( ) NAMED_UNIT ( * ) SI_UNIT ( .MILLI., .METRE. ) );
#137127 = DIRECTION ( 'NONE',  ( 0.000000000000000000, 0.000000000000000000, 1.000000000000000000 ) ) ;
#137128 = CARTESIAN_POINT ( 'NONE',  ( 0.4000000000000000777, 2.999999999999999112, -2.420000000000000373 ) ) ;
#137129 = PRESENTATION_LAYER_ASSIGNMENT (  '', '', ( #178555 ) ) ;
#137130 = CARTESIAN_POINT ( 'NONE',  ( 1.787996309160574837, 1.523479866092191548, 1.596893430481533649 ) ) ;
#137131 = CARTESIAN_POINT ( 'NONE',  ( 3.321791363677785380, -2.181432725256218674, 0.5997193178089550436 ) ) ;
#137132 = CARTESIAN_POINT ( 'NONE',  ( -7.158341918335454857, 10.33485409049125003, 1.082531754730549967 ) ) ;
#137133 = CARTESIAN_POINT ( 'NONE',  ( 3.058660868685322498, 0.4446918012569016643, 1.755998500949424113 ) ) ;
#137134 = EDGE_CURVE ( 'NONE', #109006, #54631, #185204, .T. ) ;
#137135 = CARTESIAN_POINT ( 'NONE',  ( 3.924928585964591932, -1.664043332733669667, 0.9490909334420574162 ) ) ;
#137136 = CARTESIAN_POINT ( 'NONE',  ( 5.406714943436663035, 0.5975561702324573288, 1.982271326387271770 ) ) ;
#137137 = CARTESIAN_POINT ( 'NONE',  ( 1.364683531249988535, 4.426041667008082214, 0.7879004041258500513 ) ) ;
#137138 =( GEOMETRIC_REPRESENTATION_CONTEXT ( 3 ) GLOBAL_UNCERTAINTY_ASSIGNED_CONTEXT ( ( #74750 ) ) GLOBAL_UNIT_ASSIGNED_CONTEXT ( ( #117905, #167655, #24591 ) ) REPRESENTATION_CONTEXT ( 'NONE', 'WORKASPACE' ) );
#137139 = CARTESIAN_POINT ( 'NONE',  ( 4.311372413323046437, -0.3381597629931332172, 1.942102657548309796 ) ) ;
#137140 = CARTESIAN_POINT ( 'NONE',  ( 1.500868375504460728, 1.576442195784112155, -1.106916717273882300 ) ) ;
#137141 = CARTESIAN_POINT ( 'NONE',  ( 4.750782166719051069, -1.502237938222051650, 1.114538048626475986 ) ) ;
#137142 = CARTESIAN_POINT ( 'NONE',  ( 3.123938245303990335, -2.224009237659807958, 0.6155878327348850432 ) ) ;
#137143 = CARTESIAN_POINT ( 'NONE',  ( 4.299146511743386689, -1.619905129461503224, 0.9160139579608633786 ) ) ;
#137144 = CARTESIAN_POINT ( 'NONE',  ( -1.201851678989727383E-14, 5.196875000341422357, -1.575800808251660134 ) ) ;
#137145 = CARTESIAN_POINT ( 'NONE',  ( 1.500000000000001332, 8.906250000682797818, 0.000000000000000000 ) ) ;
#137147 = CARTESIAN_POINT ( 'NONE',  ( 2.086679739605776351, -2.065639965682735557, -0.4097663305358787977 ) ) ;
#137146 = CARTESIAN_POINT ( 'NONE',  ( -4.907688418022547516, 4.827984030555475314, 1.214306433183764966E-14 ) ) ;
#137148 = CARTESIAN_POINT ( 'NONE',  ( 4.677199806590210507, 4.559080650551097236, -0.7216878364870197293 ) ) ;
#137150 = CARTESIAN_POINT ( 'NONE',  ( -9.992522908471816123, 11.61669713376064372, 1.199719254218462483 ) ) ;
#137149 = CARTESIAN_POINT ( 'NONE',  ( 1.364683531249988535, 5.467708333674750953, -0.7879004041258300672 ) ) ;
#137151 = CARTESIAN_POINT ( 'NONE',  ( 1.382866120668046150, 4.316195966766219527, 0.2144190051505707739 ) ) ;
#137152 = CARTESIAN_POINT ( 'NONE',  ( 3.217144136595586179, 1.669276650691432495, -1.307696563879121365 ) ) ;
#137153 = CARTESIAN_POINT ( 'NONE',  ( 7.006746397889325628, 6.052176462752766106, -2.500000000000000444 ) ) ;
#137154 = CARTESIAN_POINT ( 'NONE',  ( 1.230729765704338563, 1.353420925896263061, -1.499466043412321703 ) ) ;
#137155 = CARTESIAN_POINT ( 'NONE',  ( 0.6823417656249899377, 1.092708333674752286, 1.181850606188755259 ) ) ;
#137156 = VECTOR ( 'NONE', #32069, 1000.000000000000000 ) ;
#137157 = CARTESIAN_POINT ( 'NONE',  ( -3.958617665510283601, 4.681104033592509595, -1.082531754730549967 ) ) ;
#137158 = CARTESIAN_POINT ( 'NONE',  ( 5.281064527722868718, 6.119995689553514140, 1.199719254218462483 ) ) ;
#137159 = ORIENTED_EDGE ( 'NONE', *, *, #107594, .F. ) ;
#137160 = EDGE_CURVE ( 'NONE', #19237, #19391, #133851, .T. ) ;
#137161 = CARTESIAN_POINT ( 'NONE',  ( 1.774925396934714295, -2.051924176137665423, -0.6798970441593693570 ) ) ;
#137162 = CARTESIAN_POINT ( 'NONE',  ( 6.610000000000018083, 6.039292104641935666, 2.314898989754467618 ) ) ;
#137165 = CARTESIAN_POINT ( 'NONE',  ( 2.353140975214496944, 2.704741401632033249, -2.456000212125921678 ) ) ;
#137164 = CARTESIAN_POINT ( 'NONE',  ( 6.925078400183546812, 2.074047572655359328, 2.163550030515603684 ) ) ;
#137163 = CARTESIAN_POINT ( 'NONE',  ( 4.362691568547328202, 8.311833606605697256, -0.7998128361456381397 ) ) ;
#137166 = LINE ( 'NONE', #54836, #130944 ) ;
#137167 = CARTESIAN_POINT ( 'NONE',  ( 6.262907710099243630, -0.1037740067610822270, -2.014008436551452785 ) ) ;
#137168 = CARTESIAN_POINT ( 'NONE',  ( -7.049876689426097798, 11.16868053773170821, -0.7216878364870267237 ) ) ;
#137169 = CARTESIAN_POINT ( 'NONE',  ( 6.444877668667830406, -1.679477184941297496, -1.245029935506683838 ) ) ;
#137170 = CARTESIAN_POINT ( 'NONE',  ( -10.39230484541327826, 3.447199233515649386, -5.999999999999975131 ) ) ;
#137172 = CARTESIAN_POINT ( 'NONE',  ( -0.6823417656250003738, 12.65104166700806232, 1.181850606188754593 ) ) ;
#137171 = CARTESIAN_POINT ( 'NONE',  ( 0.6555950923613624859, -1.913042455388717311, -1.207739878423098823 ) ) ;
#137173 = CARTESIAN_POINT ( 'NONE',  ( -7.811469059767924605, 12.26513100303794168, -0.7998128361456281477 ) ) ;
#137174 = CARTESIAN_POINT ( 'NONE',  ( -4.067082893975237035, 7.688754443039000464, 1.040834085586084257E-14 ) ) ;
#137175 = CARTESIAN_POINT ( 'NONE',  ( -1.364683531250012516, 2.551041667008089320, -0.7879004041258289570 ) ) ;
#137176 = CARTESIAN_POINT ( 'NONE',  ( 1.499999999999990896, 4.525000000000021672, 1.214306433183764966E-14 ) ) ;
#137177 = CARTESIAN_POINT ( 'NONE',  ( 1.499999999999997113, 10.14583333333333570, -0.8660254037844378194 ) ) ;
#137178 = CARTESIAN_POINT ( 'NONE',  ( 2.631144668424452604, -1.609571295485120457, 0.6205441041484575093 ) ) ;
#137179 = CARTESIAN_POINT ( 'NONE',  ( 5.041653019435334393, 6.975290837464928728, -1.599625672291269396 ) ) ;
#137180 = CARTESIAN_POINT ( 'NONE',  ( 2.530210103492841256, 1.715365446638704494, 0.4347029418121580169 ) ) ;
#137181 =( BOUNDED_CURVE ( )  B_SPLINE_CURVE ( 2, ( #189644, #10879, #109547 ),
 .UNSPECIFIED., .F., .T. ) 
 B_SPLINE_CURVE_WITH_KNOTS ( ( 3, 3 ),
 ( 0.1229783203405390019, 0.1249999999999998751 ),
 .UNSPECIFIED. ) 
 CURVE ( )  GEOMETRIC_REPRESENTATION_ITEM ( )  RATIONAL_B_SPLINE_CURVE ( ( 0.9330713687540070911, 0.9349951081471596925, 0.9999999999999960032 ) ) 
 REPRESENTATION_ITEM ( '' )  );
#137182 = CARTESIAN_POINT ( 'NONE',  ( 2.613933768341146102, -0.6292564844058865514, 1.912298747220711359 ) ) ;
#137183 = CARTESIAN_POINT ( 'NONE',  ( 9.049177462117294013, 12.64479190819049670, -1.199719254218446718 ) ) ;
#137184 = CARTESIAN_POINT ( 'NONE',  ( 5.561621765989873900, 0.4355406452380207738, -2.163202247768724718 ) ) ;
#137185 = EDGE_LOOP ( 'NONE', ( #211526, #10381, #85782, #11874 ) ) ;
#137186 = CARTESIAN_POINT ( 'NONE',  ( 4.552993113364055766, 0.3493383367317858257, 1.989188622967730025 ) ) ;
#137187 = CARTESIAN_POINT ( 'NONE',  ( -5.413448473606448985, 9.537716662508005427, 0.000000000000000000 ) ) ;
#137189 = CARTESIAN_POINT ( 'NONE',  ( 4.341422844945469706, 0.4390097190783425196, -1.967893369681630533 ) ) ;
#137188 = CARTESIAN_POINT ( 'NONE',  ( 4.494861206476631565, -2.057060146276223023, -0.5143016718046622415 ) ) ;
#137191 = ORIENTED_EDGE ( 'NONE', *, *, #103751, .T. ) ;
#137190 = CARTESIAN_POINT ( 'NONE',  ( 4.377109366116209266, -1.621248278760094363, -0.8084319655582442588 ) ) ;
#137192 = CARTESIAN_POINT ( 'NONE',  ( 4.817943484809818600, 6.714296380401858499, 1.599625672291269396 ) ) ;
#137193 = ORIENTED_EDGE ( 'NONE', *, *, #125522, .F. ) ;
#137194 = CARTESIAN_POINT ( 'NONE',  ( 1.147088892781012781, -1.472398045354219587, -1.153743250124287689 ) ) ;
#137195 = CARTESIAN_POINT ( 'NONE',  ( 0.4999999999999605316, 3.999999999999989786, 0.3999999999999611644 ) ) ;
#137196 = CARTESIAN_POINT ( 'NONE',  ( 5.672461423068217989, 0.7400952288921599509, 1.653588109013460095 ) ) ;
#137197 = CARTESIAN_POINT ( 'NONE',  ( -5.963818478108997567, 6.870746658508759097, 0.9995729632361770589 ) ) ;
#137198 = CARTESIAN_POINT ( 'NONE',  ( -11.23979429089589033, 4.930458577253933328, -5.866063493660276684 ) ) ;
#137199 = CARTESIAN_POINT ( 'NONE',  ( 0.000000000000000000, 15.50000000000019362, 0.000000000000000000 ) ) ;
#137200 = EDGE_CURVE ( 'NONE', #157346, #74053, #139399, .T. ) ;
#137201 = CARTESIAN_POINT ( 'NONE',  ( -1.201851678989727383E-14, 2.884375000341418804, 1.575800808251672791 ) ) ;
#137202 = CARTESIAN_POINT ( 'NONE',  ( 0.6856317642073318508, 1.842354612247762091, -0.5124485439033445999 ) ) ;
#137203 = CARTESIAN_POINT ( 'NONE',  ( 4.746763178560241769, 8.551991118380046331, 0.7216878364870328300 ) ) ;
#137204 = CARTESIAN_POINT ( 'NONE',  ( 1.328483007144948935, -1.247240240105648601, 1.514344512384787622 ) ) ;
#137205 = ADVANCED_FACE ( 'NONE', ( #115219 ), #111222, .F. ) ;
#137206 = CARTESIAN_POINT ( 'NONE',  ( -4.665414256878304577, 5.575976400180357118, -1.082531754730549967 ) ) ;
#137207 = CARTESIAN_POINT ( 'NONE',  ( -5.098748287191073203, 8.106234214101666780, 1.199719254218452935 ) ) ;
#137208 = CARTESIAN_POINT ( 'NONE',  ( 3.621431001533811589, 1.820626359085864454, 1.087046460333654485 ) ) ;
#137210 = CARTESIAN_POINT ( 'NONE',  ( -10.45142682343936791, 5.144546645612242841, 5.216777551074719632 ) ) ;
#137209 = CARTESIAN_POINT ( 'NONE',  ( -0.1294898018152226826, 6.948707995275583471, -2.521562306467279857 ) ) ;
#137211 = CARTESIAN_POINT ( 'NONE',  ( 5.800065155369113157, -1.971530342684927772, -0.002616305567698303924 ) ) ;
#137212 = CARTESIAN_POINT ( 'NONE',  ( -1.402160292154681736E-14, 0.6968750003414164729, -1.575800808251659024 ) ) ;
#137213 = CARTESIAN_POINT ( 'NONE',  ( 1.248292583380994136, 0.9887404755159521219, -1.753579541237253903 ) ) ;
#137214 = EDGE_LOOP ( 'NONE', ( #210466, #46879, #355, #209000 ) ) ;
#137215 = COLOUR_RGB ( '', 0.40784314, 0.44705882, 0.49803922) ;
#137216 = CARTESIAN_POINT ( 'NONE',  ( 1.177538910780148385, 1.606043500598727247, 1.379722209976147251 ) ) ;
#137217 = CARTESIAN_POINT ( 'NONE',  ( 11.82993880136642417, 6.822466781481484333, -1.712400514339024626 ) ) ;
#137218 = CARTESIAN_POINT ( 'NONE',  ( 2.436061438456170958, 1.271862942251865691, 1.633573898902056731 ) ) ;
#137219 = VERTEX_POINT ( 'NONE', #82641 ) ;
#137220 = CARTESIAN_POINT ( 'NONE',  ( 3.054329744828568227, 6.785411478933790264, 0.000000000000000000 ) ) ;
#137221 = CARTESIAN_POINT ( 'NONE',  ( 5.143339171537801846, 7.093924681584509173, 1.599625672291269396 ) ) ;
#137222 = ORIENTED_EDGE ( 'NONE', *, *, #166535, .T. ) ;
#137224 = CARTESIAN_POINT ( 'NONE',  ( 4.680589345215795838, 6.483773540883647435, -1.599625672291256295 ) ) ;
#137223 = CARTESIAN_POINT ( 'NONE',  ( 4.347661206880347073, 2.090185315053775472, -0.05106478779118817091 ) ) ;
#137227 = ORIENTED_EDGE ( 'NONE', *, *, #13474, .T. ) ;
#137226 = CARTESIAN_POINT ( 'NONE',  ( 1.418313031307829153, -0.6519236697288594007, -1.690267533947023892 ) ) ;
#137225 = CARTESIAN_POINT ( 'NONE',  ( 2.959763373685083909, 1.816946311034864703, -0.1772020141349931188 ) ) ;
#137228 = CARTESIAN_POINT ( 'NONE',  ( 6.129534211984397629, -2.079372889712034489, 0.7396383780838566846 ) ) ;
#137229 = CARTESIAN_POINT ( 'NONE',  ( 4.155453238874762256, -1.833011353516471154, -1.228491751752130323 ) ) ;
#137230 = CARTESIAN_POINT ( 'NONE',  ( 7.958799866421889746, 9.244020251369077457, -1.199719254218441611 ) ) ;
#137231 = CARTESIAN_POINT ( 'NONE',  ( 0.6823417656249934904, 8.755208333674733723, 1.181850606188764807 ) ) ;
#137232 = CARTESIAN_POINT ( 'NONE',  ( 3.404848115249804685, -0.3755933644018424888, -1.874856250562627391 ) ) ;
#137233 = CARTESIAN_POINT ( 'NONE',  ( -3.327636637150278798, 5.969660945728899826, -1.199719254218452935 ) ) ;
#137234 = CARTESIAN_POINT ( 'NONE',  ( 7.313733799568044702, 10.62010763521636214, 1.199719254218460707 ) ) ;
#137235 = CARTESIAN_POINT ( 'NONE',  ( 6.584440175795505112, 1.195396180001909059, -1.690200020538407566 ) ) ;
#137236 = CARTESIAN_POINT ( 'NONE',  ( 0.6801582343749726922, 0.7552083336747339448, 1.178068619123784355 ) ) ;
#137237 = CARTESIAN_POINT ( 'NONE',  ( 5.601184584505256581, -0.5335315006234629953, 2.125516261704554211 ) ) ;
#137238 = CARTESIAN_POINT ( 'NONE',  ( 5.544801429207002030, 7.539493339695484408, -1.337888636821100041 ) ) ;
#137239 = CARTESIAN_POINT ( 'NONE',  ( -8.804420911738874977, 15.51845923041438979, -8.203281805575960206 ) ) ;
#137240 = ORIENTED_EDGE ( 'NONE', *, *, #98017, .T. ) ;
#137241 = CARTESIAN_POINT ( 'NONE',  ( 11.41042268598792653, 3.467171072964057910, -3.707471073020402574 ) ) ;
#137242 = CARTESIAN_POINT ( 'NONE',  ( 3.057714436724996876, 1.861869414292870006, -0.1796979844640861634 ) ) ;
#137243 = CARTESIAN_POINT ( 'NONE',  ( -3.285556943750000514, -0.9260416661887073131, -1.896917185911906722 ) ) ;
#137244 = AXIS2_PLACEMENT_3D ( 'NONE', #152034, #3605, #20926 ) ;
#137245 = CARTESIAN_POINT ( 'NONE',  ( 10.91970695577495043, -5.907420853759282053, 8.673617379884035472E-15 ) ) ;
#137246 = CARTESIAN_POINT ( 'NONE',  ( -8.215877900201387973, 8.687538426430837291, 0.7216878364870578100 ) ) ;
#137248 = CARTESIAN_POINT ( 'NONE',  ( 5.408776937209000657, 5.274937613024121674, 0.7998128361456352531 ) ) ;
#137247 = AXIS2_PLACEMENT_3D ( 'NONE', #92580, #26470, #139172 ) ;
#137249 = CARTESIAN_POINT ( 'NONE',  ( 6.789897376884641567, -1.347643488625469121, -1.571692526165118009 ) ) ;
#137250 = CARTESIAN_POINT ( 'NONE',  ( 1.265250157614560278, 1.862010354082012098, -0.7743342583275418800 ) ) ;
#137251 = CARTESIAN_POINT ( 'NONE',  ( -8.459397779922852578, 11.95671561229694824, 1.199719254218453823 ) ) ;
#137252 = CARTESIAN_POINT ( 'NONE',  ( 5.969332771766739931, 10.18624834369502885, -0.7998128361456481317 ) ) ;
#137253 = DIRECTION ( 'NONE',  ( 1.000000000000000000, 0.000000000000000000, 1.224646799147353207E-16 ) ) ;
#137254 = CARTESIAN_POINT ( 'NONE',  ( 1.658417429842372393, -1.548019161032044844, 1.551412955586493947 ) ) ;
#137255 = CARTESIAN_POINT ( 'NONE',  ( 6.727182134110222478, 0.005875948494733079785, 1.810970247402940547 ) ) ;
#137256 = CARTESIAN_POINT ( 'NONE',  ( -3.755772246185468788, 4.340488027759846545, -1.199719254218452047 ) ) ;
#137257 = CARTESIAN_POINT ( 'NONE',  ( 4.733205024946604667, 8.536173272497439513, 0.000000000000000000 ) ) ;
#137258 = CARTESIAN_POINT ( 'NONE',  ( 10.07100917685271035, 10.64393221595000938, 0.7998128361456462443 ) ) ;
#137259 = CARTESIAN_POINT ( 'NONE',  ( 4.704842999142070603, 5.447737239542574272, -1.199719254218452047 ) ) ;
#137260 = CARTESIAN_POINT ( 'NONE',  ( 3.054329744828568227, 6.785411478933790264, 0.000000000000000000 ) ) ;
#137261 = ORIENTED_EDGE ( 'NONE', *, *, #194552, .T. ) ;
#137263 = CARTESIAN_POINT ( 'NONE',  ( 1.119790083981372142, -0.4868965817936173335, 1.953217858147300090 ) ) ;
#137262 = CARTESIAN_POINT ( 'NONE',  ( 3.473999211503727036, -1.775402473473717935, -0.4878004006634574230 ) ) ;
#137264 = CARTESIAN_POINT ( 'NONE',  ( 1.581885565347431966, 1.542867095709683056, -1.703685752350136751 ) ) ;
#137266 = CARTESIAN_POINT ( 'NONE',  ( 6.086763564210844635, 1.889667650816441391, 0.5265613530214608984 ) ) ;
#137265 = CARTESIAN_POINT ( 'NONE',  ( 3.172244755917638770, 5.684407401003788607, -1.082531754730543083 ) ) ;
#137267 = CARTESIAN_POINT ( 'NONE',  ( -3.741160322367112379, 6.452105245148518797, 1.199719254218464037 ) ) ;
#137268 = LINE ( 'NONE', #203288, #109242 ) ;
#137269 = CARTESIAN_POINT ( 'NONE',  ( 3.937688585161042809, -1.828529804631402023, 0.5600222464785462595 ) ) ;
#137270 = CARTESIAN_POINT ( 'NONE',  ( -9.996439331977562404, 10.55693406359564790, 0.7998128361456462443 ) ) ;
#137271 = CARTESIAN_POINT ( 'NONE',  ( 5.969043672405669909, 7.102642550806028687, -1.084880274121432064 ) ) ;
#137272 = CARTESIAN_POINT ( 'NONE',  ( -3.298376509874564988, 7.070132704820777825, 0.000000000000000000 ) ) ;
#137274 = CARTESIAN_POINT ( 'NONE',  ( 0.8834254411415434216, 1.253375741028007084, 1.388844808110502038 ) ) ;
#137273 = CARTESIAN_POINT ( 'NONE',  ( 2.278955919255227336, 1.910372346673551602, -0.8499720230255493059 ) ) ;
#137275 = CARTESIAN_POINT ( 'NONE',  ( 1.651720012567552853, -0.2930234437087535504, -1.994564656426714988 ) ) ;
#137276 = CARTESIAN_POINT ( 'NONE',  ( 6.968527767744088663, 11.07377346243604599, 0.7216878364870438212 ) ) ;
#137277 = CARTESIAN_POINT ( 'NONE',  ( -1.364683531250010740, 4.592708333674755394, 0.7879004041258379498 ) ) ;
#137278 = CARTESIAN_POINT ( 'NONE',  ( 2.717972786412402364, 1.639536828598524121, 0.5844088115515410076 ) ) ;
#137279 = CARTESIAN_POINT ( 'NONE',  ( 4.009460741339333723, 5.700790169694431420, -1.599625672291256295 ) ) ;
#137281 = CARTESIAN_POINT ( 'NONE',  ( 0.1216811705908975444, 2.536982183874235908, -1.996294991408742447 ) ) ;
#137280 = CARTESIAN_POINT ( 'NONE',  ( 0.000000000000000000, 7.000000000000000000, 0.000000000000000000 ) ) ;
#137282 = CARTESIAN_POINT ( 'NONE',  ( 4.424228590228207914, 1.058368455644955963, -1.361911123238012111 ) ) ;
#137283 = CARTESIAN_POINT ( 'NONE',  ( 3.456733517523991051, -1.933646301634945885, -1.031433503814835007 ) ) ;
#137284 = CARTESIAN_POINT ( 'NONE',  ( 6.182275136424624229, -1.184133725572718676, 1.862117674348878760 ) ) ;
#137285 = FACE_OUTER_BOUND ( 'NONE', #32235, .T. ) ;
#137286 = AXIS2_PLACEMENT_3D ( 'NONE', #6373, #5289, #202431 ) ;
#137287 = CARTESIAN_POINT ( 'NONE',  ( 3.538082186586584577, 1.373364251514897383, 1.681533162179976060 ) ) ;
#137288 = CARTESIAN_POINT ( 'NONE',  ( 2.402731849113007190, 1.466575434288765800, -1.087121784572639527 ) ) ;
#137289 = CARTESIAN_POINT ( 'NONE',  ( 0.4968289091572677396, 0.3296062100675010154, 1.933703066120408431 ) ) ;
#137290 = CARTESIAN_POINT ( 'NONE',  ( 4.962167979565689002, -1.173633690672538865, 1.762117774576977602 ) ) ;
#137291 = CARTESIAN_POINT ( 'NONE',  ( 5.847644326195775122, 5.716673223516857583, -0.7998128361456282587 ) ) ;
#137292 = ORIENTED_EDGE ( 'NONE', *, *, #208628, .T. ) ;
#137294 = CARTESIAN_POINT ( 'NONE',  ( -1.364683531250012516, 3.301041667008084879, -0.7879004041258289570 ) ) ;
#137293 = CARTESIAN_POINT ( 'NONE',  ( 4.827800031893906052, 1.179792396777184615, -1.965320743881134646 ) ) ;
#137295 = LINE ( 'NONE', #130163, #98756 ) ;
#137296 = CARTESIAN_POINT ( 'NONE',  ( 9.028840231696797503, 12.62106513936658203, -1.199719254218446718 ) ) ;
#137297 = CIRCLE ( 'NONE', #67965, 0.5000000000000004441 ) ;
#137298 = CARTESIAN_POINT ( 'NONE',  ( 0.4344390223590781641, -1.137927343861804053, -1.789123301873453364 ) ) ;
#137299 = CARTESIAN_POINT ( 'NONE',  ( -5.910991785878183080, 5.998504626387068051, -0.7216878364870278340 ) ) ;
#137300 = CYLINDRICAL_SURFACE ( 'NONE', #4549, 1.500000000000000222 ) ;
#137301 = CARTESIAN_POINT ( 'NONE',  ( -4.677199806590235376, 7.440188293455128665, 1.082531754730560403 ) ) ;
#137302 = CYLINDRICAL_SURFACE ( 'NONE', #34087, 0.5000000000000003331 ) ;
#137303 = VERTEX_POINT ( 'NONE', #49099 ) ;
#137304 = CARTESIAN_POINT ( 'NONE',  ( 4.869767617671093340, -0.2496050341583149201, -2.000857388266870984 ) ) ;
#137306 = CARTESIAN_POINT ( 'NONE',  ( 3.520431386055590917, 0.9232258726861832798, 1.844449542969233358 ) ) ;
#137305 = CARTESIAN_POINT ( 'NONE',  ( 5.823390672269506574, 6.752709524857930745, -1.199719254218446718 ) ) ;
#137308 = CARTESIAN_POINT ( 'NONE',  ( -0.2409995289980246813, 5.721856934700204178, -2.594540323675114113 ) ) ;
#137307 = CARTESIAN_POINT ( 'NONE',  ( 5.559725510055676168, 8.644040974110419384, 1.199719254218451159 ) ) ;
#137309 = CARTESIAN_POINT ( 'NONE',  ( 6.875920180786008196, 8.050936961452347163, -1.199719254218452047 ) ) ;
#137310 = CARTESIAN_POINT ( 'NONE',  ( -3.285556943749998737, -2.180208332855376518, 1.896917185911908499 ) ) ;
#137311 = CARTESIAN_POINT ( 'NONE',  ( 6.123007039855313138, -2.064672272812938747, 0.7349105657750015785 ) ) ;
#137312 = CARTESIAN_POINT ( 'NONE',  ( 4.289685514112329123, 1.556909497225898109, -1.281360267751927129 ) ) ;
#137313 = CARTESIAN_POINT ( 'NONE',  ( 3.192734241421916419, 1.453351889590439816, 1.130385295574042104 ) ) ;
#137314 = AXIS2_PLACEMENT_3D ( 'NONE', #134915, #117641, #18987 ) ;
#137315 = CARTESIAN_POINT ( 'NONE',  ( 4.632082037363250748, 8.555846143565791095, -0.7998128361456231517 ) ) ;
#137316 = CARTESIAN_POINT ( 'NONE',  ( 0.9380131109506375520, 1.698111720264935620, 0.3011209518388803241 ) ) ;
#137317 = CARTESIAN_POINT ( 'NONE',  ( 0.1309013025973270183, -5.411711732698802457, 10.96028113393447434 ) ) ;
#137318 = CARTESIAN_POINT ( 'NONE',  ( 0.5460333347737976739, -1.659586600764794584, 1.590741637488497062 ) ) ;
#137319 = CARTESIAN_POINT ( 'NONE',  ( -7.061099074618889304, 7.132370430010492868, -0.7998128361456291469 ) ) ;
#137320 = CARTESIAN_POINT ( 'NONE',  ( 6.579017896966585788, -0.1030185651522512180, -2.260299859776133236 ) ) ;
#137321 = CARTESIAN_POINT ( 'NONE',  ( 3.352270206574393008, 2.106257355090755290, -0.0002192025019883553090 ) ) ;
#137322 = CARTESIAN_POINT ( 'NONE',  ( -3.637330350216213759, 7.465578851886037093, -0.7998128361456481317 ) ) ;
#137323 = CARTESIAN_POINT ( 'NONE',  ( 6.076025397218672630, 10.24044673006381245, -0.7998128361456291469 ) ) ;
#137324 = CARTESIAN_POINT ( 'NONE',  ( 5.682275777458841048, 8.683053269460405232, 1.082531754730547524 ) ) ;
#137325 = CARTESIAN_POINT ( 'NONE',  ( 5.625000000000003553, -2.052068128417940951, 3.204627906038193246E-13 ) ) ;
#137326 = CARTESIAN_POINT ( 'NONE',  ( -5.215082642750900277, 9.236013516518044142, 0.000000000000000000 ) ) ;
#137327 = CARTESIAN_POINT ( 'NONE',  ( 5.761852095683461350, 9.665985178365305686, -0.7216878364870267237 ) ) ;
#137328 = CARTESIAN_POINT ( 'NONE',  ( 4.363209728991265024, 7.389406413240373617, 1.150570763150955633 ) ) ;
#137329 = EDGE_CURVE ( 'NONE', #201525, #147150, #129966, .T. ) ;
#137330 = CARTESIAN_POINT ( 'NONE',  ( -3.913499895838973508, 7.717500311787445000, 1.040834085586084257E-14 ) ) ;
#137331 = CARTESIAN_POINT ( 'NONE',  ( 3.428187820690358656, -2.188011084934568196, 0.3830038565930964367 ) ) ;
#137332 = CARTESIAN_POINT ( 'NONE',  ( 2.748186945943337012, 0.7392028471469231921, 2.063141171074922120 ) ) ;
#137333 = CARTESIAN_POINT ( 'NONE',  ( -5.065942953000576843, 9.062017211809330064, -0.7998128361456231517 ) ) ;
#137334 = CARTESIAN_POINT ( 'NONE',  ( -3.447516199624892419, 7.244129009529488350, 0.7998128361456352531 ) ) ;
#137335 = CARTESIAN_POINT ( 'NONE',  ( 5.266048140081638351, -1.952571265509401854, 0.1905133553196102503 ) ) ;
#137336 = CARTESIAN_POINT ( 'NONE',  ( 1.364683531249988535, 2.363541667008088432, 0.7879004041258500513 ) ) ;
#137337 = CARTESIAN_POINT ( 'NONE',  ( 6.610000000000042952, 1.321253023796984172, 1.840686448008920229 ) ) ;
#137338 = CARTESIAN_POINT ( 'NONE',  ( -5.938108093105513241, 6.030140318152288792, 0.7216878364870317197 ) ) ;
#137339 = CARTESIAN_POINT ( 'NONE',  ( 4.394861267144759331, -2.057662932662501110, -0.5123870273424437904 ) ) ;
#137340 = CARTESIAN_POINT ( 'NONE',  ( -5.632486471834530661, 5.535932070087196344, -0.7998128361456362523 ) ) ;
#137341 = VERTEX_POINT ( 'NONE', #28838 ) ;
#137343 = CARTESIAN_POINT ( 'NONE',  ( 5.155217493315787713, -1.824165352752779246, -1.159627250419709155 ) ) ;
#137342 = CARTESIAN_POINT ( 'NONE',  ( -4.977251789992602760, 8.820894498384422633, 0.000000000000000000 ) ) ;
#137344 = CARTESIAN_POINT ( 'NONE',  ( 4.984594031318565932, 8.967110136513669616, 0.7998128361456462443 ) ) ;
#137345 = CARTESIAN_POINT ( 'NONE',  ( 5.073706409418358376, -1.018251046719556685, 1.533866337327425056 ) ) ;
#137346 = CARTESIAN_POINT ( 'NONE',  ( -5.672026259827416261, 6.146810915570031675, 0.7861540255039052294 ) ) ;
#137347 = CARTESIAN_POINT ( 'NONE',  ( -1.201851678989727383E-14, 1.384375000341419693, 1.575800808251672791 ) ) ;
#137348 = CARTESIAN_POINT ( 'NONE',  ( 6.333937804992649134, 1.722499169431927601, 0.2476611369811829999 ) ) ;
#137350 = EDGE_CURVE ( 'NONE', #42278, #85030, #67731, .T. ) ;
#137349 = CARTESIAN_POINT ( 'NONE',  ( -0.4019237886467001974, 11.33258545099816317, 1.500000000000001998 ) ) ;
#137351 = CARTESIAN_POINT ( 'NONE',  ( -0.1638468497727919582, 7.035416012003069319, 1.994423973928958205 ) ) ;
#137352 = CARTESIAN_POINT ( 'NONE',  ( 6.717278222822382183, 7.849261790823902629, -6.830415307812251591 ) ) ;
#137353 = CARTESIAN_POINT ( 'NONE',  ( 4.645497774645744649, -1.668943667408796294, -1.373881373981879594 ) ) ;
#137354 = EDGE_CURVE ( 'NONE', #106915, #185927, #120842, .T. ) ;
#137355 = CARTESIAN_POINT ( 'NONE',  ( -5.298539104842322267, 5.076050465271134016, 0.7998128361456341429 ) ) ;
#137356 = CARTESIAN_POINT ( 'NONE',  ( -6.358410854684777291, 10.36197039720016022, -0.7216878364870267237 ) ) ;
#137357 = CARTESIAN_POINT ( 'NONE',  ( 3.836934241894359054, 0.3148432204054998351, 2.138525872868973998 ) ) ;
#137358 = CARTESIAN_POINT ( 'NONE',  ( 4.604731966549804767, 1.525920046185350376, -1.248162976031294003 ) ) ;
#137359 = CARTESIAN_POINT ( 'NONE',  ( 3.795997188448175130, -1.602592684597732298, 0.6622489764130984335 ) ) ;
#137360 = CARTESIAN_POINT ( 'NONE',  ( 1.083813775577105565, -0.9808430935620198188, 1.959877696171570927 ) ) ;
#137361 = CARTESIAN_POINT ( 'NONE',  ( 2.538448204128932240, 1.088115672400795431, -2.034946615453626872 ) ) ;
#137362 = CARTESIAN_POINT ( 'NONE',  ( 3.971991334398959239, 1.141669855754149365, 1.715422085859653833 ) ) ;
#137363 = CARTESIAN_POINT ( 'NONE',  ( 6.110880135979408045, -0.2334805506369178330, 1.927903797987507106 ) ) ;
#137364 = CARTESIAN_POINT ( 'NONE',  ( -7.822691444960709006, 10.14955932391940330, -1.443375672974058777 ) ) ;
#137365 = CARTESIAN_POINT ( 'NONE',  ( -6.252245114557387851, 7.323316050852266557, -1.199719254218453823 ) ) ;
#137366 =( NAMED_UNIT ( * ) SI_UNIT ( $, .STERADIAN. ) SOLID_ANGLE_UNIT ( ) );
#137367 = CARTESIAN_POINT ( 'NONE',  ( -4.167152111353897403, 5.955039778036558040, 1.599625672291270506 ) ) ;
#137368 = CARTESIAN_POINT ( 'NONE',  ( -6.507550544435101614, 10.53596670190887963, 0.000000000000000000 ) ) ;
#137369 = CARTESIAN_POINT ( 'NONE',  ( 3.118423654462946892, -1.086285162511631652, -1.920806481261853493 ) ) ;
#137370 = CARTESIAN_POINT ( 'NONE',  ( 1.642778471875001811, -2.880208332855377584, 2.845375778867859751 ) ) ;
#137371 = VERTEX_POINT ( 'NONE', #159901 ) ;
#137372 = CARTESIAN_POINT ( 'NONE',  ( 1.129495572712395646, 1.795378659943444033, -0.4894723102292392047 ) ) ;
#137373 =( BOUNDED_CURVE ( )  B_SPLINE_CURVE ( 2, ( #71476, #155962, #88838, #188446, #7548 ),
 .UNSPECIFIED., .F., .T. ) 
 B_SPLINE_CURVE_WITH_KNOTS ( ( 3, 2, 3 ),
 ( 0.2915250305792598251, 0.2916666666666666852, 0.2946428571428571508 ),
 .UNSPECIFIED. ) 
 CURVE ( )  GEOMETRIC_REPRESENTATION_ITEM ( )  RATIONAL_B_SPLINE_CURVE ( ( 0.9937758973840666865, 0.9968120928798591684, 1.000000000000000000, 0.9330127018922194093, 0.9330127018922194093 ) ) 
 REPRESENTATION_ITEM ( '' )  );
#137374 = CARTESIAN_POINT ( 'NONE',  ( -0.02919842301645457147, -0.002306431287177941429, -2.073770398395402115 ) ) ;
#137375 = CARTESIAN_POINT ( 'NONE',  ( -9.495705940876565165, -8.203192640252289891, 0.2943368945748078280 ) ) ;
#137377 = CARTESIAN_POINT ( 'NONE',  ( 6.925078400183553029, 2.042159606913606762, 2.349846261904017464 ) ) ;
#137376 = CARTESIAN_POINT ( 'NONE',  ( -6.462985781203115287, 6.858296038324478872, -0.6802466501308057634 ) ) ;
#137378 = CARTESIAN_POINT ( 'NONE',  ( 6.421814705521882161, 1.055779539018763646, -1.508159643570324393 ) ) ;
#137379 = ORIENTED_EDGE ( 'NONE', *, *, #5161, .F. ) ;
#137380 = CARTESIAN_POINT ( 'NONE',  ( 3.713790661510278923, -2.030684131657393365, 0.3505542424454102246 ) ) ;
#137381 = CARTESIAN_POINT ( 'NONE',  ( 1.360316468749988683, 0.2656250003413990202, -1.387778780781445676E-14 ) ) ;
#137382 = CARTESIAN_POINT ( 'NONE',  ( -4.381256195510448315, 8.263215994737505454, 1.040834085586084257E-14 ) ) ;
#137383 = FACE_OUTER_BOUND ( 'NONE', #10000, .T. ) ;
#137384 = DIRECTION ( 'NONE',  ( 0.7592566023653003482, 0.6507913734559641616, 0.000000000000000000 ) ) ;
#137385 = CARTESIAN_POINT ( 'NONE',  ( 4.359110081993588182, 5.044382169536003602, -1.199719254218452047 ) ) ;
#137386 = CARTESIAN_POINT ( 'NONE',  ( 2.166935907724653720, -1.883791910722651952, -0.8362540481525667646 ) ) ;
#137388 = CARTESIAN_POINT ( 'NONE',  ( 1.364683531249996529, 13.46354166700806765, 0.7879004041258405033 ) ) ;
#137387 = CARTESIAN_POINT ( 'NONE',  ( 4.888966637111398228, 4.912082840724287358, 0.6391686513922645307 ) ) ;
#137389 = CARTESIAN_POINT ( 'NONE',  ( 5.307127064745490230, 8.279066444590018392, -1.199719254218452935 ) ) ;
#137390 = CARTESIAN_POINT ( 'NONE',  ( 4.046711340876006702, 3.801480273782092745, 2.500000000000000444 ) ) ;
#137391 = CARTESIAN_POINT ( 'NONE',  ( 5.391335350415090488, 1.947751002805158560, -1.037606470750504828 ) ) ;
#137392 = CARTESIAN_POINT ( 'NONE',  ( 0.3862812426984676972, -1.019270635400490121, 1.906220128828392646 ) ) ;
#137393 = CARTESIAN_POINT ( 'NONE',  ( -3.294268138440636928, 6.787137228248626641, 1.040834085586084257E-14 ) ) ;
#137394 = CARTESIAN_POINT ( 'NONE',  ( 0.6379081216283178923, 2.014007883293071899, -0.1037844182863178755 ) ) ;
#137395 = CARTESIAN_POINT ( 'NONE',  ( 4.635512016184385686, 8.422473116793771197, 0.5971484286424336707 ) ) ;
#137396 = CYLINDRICAL_SURFACE ( 'NONE', #197993, 0.08000000000000020983 ) ;
#137397 = FILL_AREA_STYLE ('',( #186116 ) ) ;
#137398 = CARTESIAN_POINT ( 'NONE',  ( 2.166681600665042229, -1.709288833360942617, -0.7604731621856930524 ) ) ;
#137399 = AXIS2_PLACEMENT_3D ( 'NONE', #170722, #8216, #154487 ) ;
#137400 = CARTESIAN_POINT ( 'NONE',  ( 3.292204118033771110, -0.8216723425069611952, -1.841733987974409237 ) ) ;
#137401 = CARTESIAN_POINT ( 'NONE',  ( -1.402160292154681736E-14, 0.5718750003414239114, 1.575800808251672791 ) ) ;
#137403 = CARTESIAN_POINT ( 'NONE',  ( 4.916683514525310272, 1.453009998446822992, -1.524801812277425839 ) ) ;
#137402 = CARTESIAN_POINT ( 'NONE',  ( -8.962103233833181193, 10.41454084668224489, -1.199719254218446718 ) ) ;
#137404 = CARTESIAN_POINT ( 'NONE',  ( 8.782984583554449998, 9.141236857102018831, 1.040834085586084257E-14 ) ) ;
#137406 = CARTESIAN_POINT ( 'NONE',  ( -6.852756576703439961, 10.08230087520760954, 1.199719254218453823 ) ) ;
#137405 = CARTESIAN_POINT ( 'NONE',  ( 4.869313445963426190, 5.709895770826003414, 1.199719254218452935 ) ) ;
#137407 = LINE ( 'NONE', #5220, #199899 ) ;
#137408 = CARTESIAN_POINT ( 'NONE',  ( 4.412371012857700947, -2.019438640443659505, -0.04532404540058888875 ) ) ;
#137409 = CARTESIAN_POINT ( 'NONE',  ( -1.001543065824772872E-14, 4.571875000341418804, 1.575800808251672791 ) ) ;
#137410 = CARTESIAN_POINT ( 'NONE',  ( 6.215292634054179643, -1.767141628190834757, -1.063693359622622125 ) ) ;
#137411 = CARTESIAN_POINT ( 'NONE',  ( 8.432808358020004391, 12.78210081775797669, 0.7216878364870438212 ) ) ;
#137412 = EDGE_CURVE ( 'NONE', #203495, #130695, #39908, .T. ) ;
#137413 = CARTESIAN_POINT ( 'NONE',  ( 5.940740243836844847, 0.4152237956781511530, 2.121177236311201586 ) ) ;
#137414 = CARTESIAN_POINT ( 'NONE',  ( 6.496291879603339758, 7.608037276739255006, 1.199719254218452935 ) ) ;
#137415 = CARTESIAN_POINT ( 'NONE',  ( -1.402160292154681736E-14, -0.9906249996585834161, -1.575800808251665908 ) ) ;
#137417 = DIRECTION ( 'NONE',  ( 0.000000000000000000, -1.000000000000000000, 0.000000000000000000 ) ) ;
#137416 = CARTESIAN_POINT ( 'NONE',  ( 6.866278450678116485, 6.975356045404744521, 0.000000000000000000 ) ) ;
#137418 = CARTESIAN_POINT ( 'NONE',  ( 7.741342523278698096, 10.05465224862374285, 1.443375672974076540 ) ) ;
#137420 = DIRECTION ( 'NONE',  ( -5.551115123125766062E-17, 0.000000000000000000, 1.000000000000000000 ) ) ;
#137419 = CARTESIAN_POINT ( 'NONE',  ( 3.561125603554469610, 1.713606050895712718, -1.333181090037469652 ) ) ;
#137422 = CARTESIAN_POINT ( 'NONE',  ( 2.050122339901743196, -1.422379512129726908, 1.169167124061460949 ) ) ;
#137421 = CARTESIAN_POINT ( 'NONE',  ( -5.205967797967562483, 8.057084283395347768, 1.082531754730548412 ) ) ;
#137423 = CARTESIAN_POINT ( 'NONE',  ( 1.364683531249988535, 2.905208333674754506, -0.7879004041258239610 ) ) ;
#137424 = CARTESIAN_POINT ( 'NONE',  ( 3.702820756938397295, 1.880440254450808757, 1.125299312022425280 ) ) ;
#137425 = CARTESIAN_POINT ( 'NONE',  ( 6.883263157960365142, -0.007059606330772279746, 2.153658854459541416 ) ) ;
#137426 = CARTESIAN_POINT ( 'NONE',  ( 4.100629699907013759, -0.7064081464536530186, -2.149486123859779330 ) ) ;
#137427 = CARTESIAN_POINT ( 'NONE',  ( -7.040761844198392794, 7.108643661186573759, -0.7998128361456291469 ) ) ;
#137428 = B_SPLINE_CURVE_WITH_KNOTS ( 'NONE', 3,
 ( #213096, #14891, #99377, #98308, #67898, #83103, #117824, #165430, #183814, #113559, #182741 ),
 .UNSPECIFIED., .F., .F.,
 ( 4, 1, 1, 1, 1, 1, 1, 1, 4 ),
 ( 0.000000000000000000, 0.2255619619413396781, 0.3975297875667437308, 0.5250373104567740423, 0.6172314665434700531, 0.6832587661106447330, 0.7322037845459880012, 0.7729093456892226488, 1.000000000000000000 ),
 .UNSPECIFIED. ) ;
#137429 = CARTESIAN_POINT ( 'NONE',  ( 0.6823417656249899377, 5.738541667008087543, -1.181850606188754593 ) ) ;
#137430 = CARTESIAN_POINT ( 'NONE',  ( 6.484283628081795037, 6.752753718119230975, 0.1579380340677779548 ) ) ;
#137431 = CARTESIAN_POINT ( 'NONE',  ( -6.009258394948636914E-15, 13.68750000000000178, -1.732050807568875195 ) ) ;
#137432 = CARTESIAN_POINT ( 'NONE',  ( 6.387299765813869712, 6.624473612970537495, 0.000000000000000000 ) ) ;
#137433 = EDGE_CURVE ( 'NONE', #19959, #195013, #91879, .T. ) ;
#137434 = CARTESIAN_POINT ( 'NONE',  ( 5.465970981792784400, 0.8728298736929670509, 1.539401198699318352 ) ) ;
#137435 = CIRCLE ( 'NONE', #210070, 0.7500000000000011102 ) ;
#137436 = CARTESIAN_POINT ( 'NONE',  ( 3.387361027847039185, 0.04724124570358113201, -2.012690625139363032 ) ) ;
#137437 = CARTESIAN_POINT ( 'NONE',  ( 7.072549687823125097, 11.40305840243567381, -0.7998128361456291469 ) ) ;
#137438 = CARTESIAN_POINT ( 'NONE',  ( 2.274573006691050558, -1.296483931956838198, 1.659472957066634669 ) ) ;
#137440 = CARTESIAN_POINT ( 'NONE',  ( -0.7500000000000215383, 2.191666666666689078, 1.299038105676671107 ) ) ;
#137439 = CARTESIAN_POINT ( 'NONE',  ( -1.364683531250000748, 11.60937500034139802, 0.000000000000000000 ) ) ;
#137441 = CARTESIAN_POINT ( 'NONE',  ( 0.6780957659633795043, -1.050550344063156061, -1.665771736420356808 ) ) ;
#137442 = CARTESIAN_POINT ( 'NONE',  ( -2.986538976760251263, 6.706322249520737522, -0.7998128361456481317 ) ) ;
#137443 = DIRECTION ( 'NONE',  ( 2.168462536859579677E-14, -1.000000000000000000, 9.418999208338882750E-28 ) ) ;
#137445 = ORIENTED_EDGE ( 'NONE', *, *, #159917, .F. ) ;
#137444 = CARTESIAN_POINT ( 'NONE',  ( 5.590068458682615038, 1.086043493620889144, 1.449778898616445488 ) ) ;
#137446 = CARTESIAN_POINT ( 'NONE',  ( 6.317736394288140822, 7.433409217166723870, 1.082531754730558626 ) ) ;
#137447 =( GEOMETRIC_REPRESENTATION_CONTEXT ( 3 ) GLOBAL_UNCERTAINTY_ASSIGNED_CONTEXT ( ( #124653 ) ) GLOBAL_UNIT_ASSIGNED_CONTEXT ( ( #205548, #89706, #5195 ) ) REPRESENTATION_CONTEXT ( 'NONE', 'WORKASPACE' ) );
#137448 = CARTESIAN_POINT ( 'NONE',  ( -1.402160292154681736E-14, -0.2406249996585799189, -1.575800808251665908 ) ) ;
#137449 = CARTESIAN_POINT ( 'NONE',  ( 4.645289301550183936, -1.446173438076237217, -1.186536486241091204 ) ) ;
#137450 = CARTESIAN_POINT ( 'NONE',  ( 2.354312230267378236, 5.898448035287240820, -0.7998128361456281477 ) ) ;
#137451 = ORIENTED_EDGE ( 'NONE', *, *, #78072, .F. ) ;
#137452 = CARTESIAN_POINT ( 'NONE',  ( 5.383670357325340383, -1.967593191946028996, 0.6441560278484457225 ) ) ;
#137453 = CARTESIAN_POINT ( 'NONE',  ( -1.225000000000026512, 1.750000000000015543, -1.734723475976807094E-14 ) ) ;
#137454 = CARTESIAN_POINT ( 'NONE',  ( -6.116136693096208887, 6.308116694799912771, 0.7216878364870257245 ) ) ;
#137455 = CARTESIAN_POINT ( 'NONE',  ( 2.046417720077495783, -0.9634407361576915463, 2.739321268633221340 ) ) ;
#137456 = CARTESIAN_POINT ( 'NONE',  ( 1.499999999999987121, 0.5041666666666856367, 0.8660254037844524744 ) ) ;
#137457 = CARTESIAN_POINT ( 'NONE',  ( 7.182068686937156166, 9.402166106225269715, 1.599625672291281386 ) ) ;
#137458 = CARTESIAN_POINT ( 'NONE',  ( -7.994504133552415404, 12.47867192245318435, -0.7998128361456281477 ) ) ;
#137459 = CARTESIAN_POINT ( 'NONE',  ( 7.340813827156391191, 7.528980651296110160, 0.7998128361456281477 ) ) ;
#137460 = ADVANCED_FACE ( 'NONE', ( #51224 ), #198510, .T. ) ;
#137461 = CARTESIAN_POINT ( 'NONE',  ( -0.6823417656250246877, 0.3010416670080895418, 1.181850606188755259 ) ) ;
#137462 = CARTESIAN_POINT ( 'NONE',  ( 0.7499999999999885647, 1.316666666666688190, -1.299038105676652899 ) ) ;
#137464 = CARTESIAN_POINT ( 'NONE',  ( 4.822949958159288286, 6.649860922651058992, -1.599625672291256295 ) ) ;
#137463 = CARTESIAN_POINT ( 'NONE',  ( 5.055110333045015558, 1.632132345252810035, -1.088295032039228172 ) ) ;
#137465 = EDGE_CURVE ( 'NONE', #86628, #148246, #157572, .T. ) ;
#137466 = CARTESIAN_POINT ( 'NONE',  ( 2.143907462275076892, -0.09611812122205246056, -2.013924455302518624 ) ) ;
#137467 = DIRECTION ( 'NONE',  ( -1.000000000000000000, 0.000000000000000000, 0.000000000000000000 ) ) ;
#137468 = CARTESIAN_POINT ( 'NONE',  ( 0.08191350661116909848, -1.027414926483052326, 1.935800647029708665 ) ) ;
#137469 = CARTESIAN_POINT ( 'NONE',  ( -11.86239285000045918, 9.799999999999981171, 1.812080536912751283 ) ) ;
#137470 = CARTESIAN_POINT ( 'NONE',  ( 2.530351333283612281, 1.813318468827030072, 0.4585936022679508728 ) ) ;
#137471 = CARTESIAN_POINT ( 'NONE',  ( -1.364683531250010295, 5.238541667008086655, -0.7879004041258300672 ) ) ;
#137472 = CARTESIAN_POINT ( 'NONE',  ( 4.517842040498582179, -0.5326873650394120530, 1.941415848259191446 ) ) ;
#137473 = CARTESIAN_POINT ( 'NONE',  ( -7.635213062790267458, 12.05949900656400686, 0.000000000000000000 ) ) ;
#137475 = CARTESIAN_POINT ( 'NONE',  ( 4.095393968650405725, -0.3601260033815486539, 2.086223071001345630 ) ) ;
#137474 = CARTESIAN_POINT ( 'NONE',  ( -6.426201623197489887, 6.599582769926260362, 0.7216878364870317197 ) ) ;
#137476 = CARTESIAN_POINT ( 'NONE',  ( -3.667627899390105473, 3.521066046765052970, -2.447586748966623649 ) ) ;
#137477 = CARTESIAN_POINT ( 'NONE',  ( 6.197728532230423859, -1.496850047335227085, -1.430563974149069661 ) ) ;
#137479 = CARTESIAN_POINT ( 'NONE',  ( 6.720655732516644498, 4.691561721546229968, 2.636312907496433322 ) ) ;
#137478 = CARTESIAN_POINT ( 'NONE',  ( 1.101248736683122953, -0.5045743719560727980, 2.028828713580214771 ) ) ;
#137481 = ORIENTED_EDGE ( 'NONE', *, *, #187556, .T. ) ;
#137480 = CARTESIAN_POINT ( 'NONE',  ( 6.264658373536385660, -1.288822541704701452, 1.293195164663100583 ) ) ;
#137482 = CARTESIAN_POINT ( 'NONE',  ( 6.076025397218672630, 10.24044673006381245, -0.7998128361456291469 ) ) ;
#137483 = CARTESIAN_POINT ( 'NONE',  ( 0.000000000000000000, 0.000000000000000000, 10.99999999999999112 ) ) ;
#137484 = CARTESIAN_POINT ( 'NONE',  ( 5.802526556524483681, 5.871961858807763335, 1.040834085586084257E-14 ) ) ;
#137485 = CARTESIAN_POINT ( 'NONE',  ( -9.669761313225400556, 3.035266360176858136, 6.558537842936834394 ) ) ;
#137486 = CARTESIAN_POINT ( 'NONE',  ( 6.819388077549422889, 8.018669514304889390, -1.082531754730543971 ) ) ;
#137487 = CARTESIAN_POINT ( 'NONE',  ( -1.364683531250010740, 12.94270833367473550, 0.7879004041258445001 ) ) ;
#137488 = CARTESIAN_POINT ( 'NONE',  ( 0.5745104438982637785, -1.313040981126518902, 1.248171054211825171 ) ) ;
#137489 = CARTESIAN_POINT ( 'NONE',  ( -7.965578943228732278, 9.251929174310385307, -1.199719254218446718 ) ) ;
#137490 = CARTESIAN_POINT ( 'NONE',  ( 4.645640190976921602, 8.571663989448405019, 1.040834085586084257E-14 ) ) ;
#137491 = CARTESIAN_POINT ( 'NONE',  ( 0.3811408430856297880, -6.893136995914741050, 10.99374989157288063 ) ) ;
#137492 = CARTESIAN_POINT ( 'NONE',  ( 0.000000000000000000, 8.600000000000017408, -0.3999999999999819811 ) ) ;
#137493 = CARTESIAN_POINT ( 'NONE',  ( 3.358669367883368118, 4.941533567329135401, -1.599625672291262513 ) ) ;
#137494 = ORIENTED_EDGE ( 'NONE', *, *, #58928, .F. ) ;
#137495 = CARTESIAN_POINT ( 'NONE',  ( 5.624625116526842383, 0.3961212581503182339, 1.976953148079656719 ) ) ;
#137496 = CARTESIAN_POINT ( 'NONE',  ( 1.299038105676669330, 5.999999999999998224, -0.7500000000000006661 ) ) ;
#137497 = CARTESIAN_POINT ( 'NONE',  ( 1.452583904633400591, 1.374772708486753370, 1.500000000000001332 ) ) ;
#137498 = CARTESIAN_POINT ( 'NONE',  ( -0.1394461523061195918, 6.947787103499363681, -2.875373568546248482 ) ) ;
#137499 = CARTESIAN_POINT ( 'NONE',  ( -6.073689629242176480, 6.188318776978391611, -0.7216878364870278340 ) ) ;
#137500 = CARTESIAN_POINT ( 'NONE',  ( 10.08690309888728187, 10.87040115823107911, -0.7216878364870257245 ) ) ;
#137501 = CARTESIAN_POINT ( 'NONE',  ( 3.994935505748583360, 0.2844874371618256736, 1.948636269439333546 ) ) ;
#137502 = CARTESIAN_POINT ( 'NONE',  ( 4.359000025081374297, -0.002827702239943663542, -2.016598147179492262 ) ) ;
#137503 = CARTESIAN_POINT ( 'NONE',  ( -6.073162743917628781, 9.172774736957510555, -1.199719254218440723 ) ) ;
#137504 = CARTESIAN_POINT ( 'NONE',  ( -0.4019237886466871523, 10.19866454968463110, -1.499999999999998668 ) ) ;
#137505 = CARTESIAN_POINT ( 'NONE',  ( 5.103566685217446164, -2.181124530238859993, 0.2125310249164805709 ) ) ;
#137506 = DIRECTION ( 'NONE',  ( 0.6250000000000005551, -0.000000000000000000, 0.7806247497997993445 ) ) ;
#137507 = CARTESIAN_POINT ( 'NONE',  ( 3.329043352767379282, 0.04595412404927168293, 1.925998307505512486 ) ) ;
#137508 = CARTESIAN_POINT ( 'NONE',  ( -7.751511138711140170, 10.06651563329490529, -1.599625672291263179 ) ) ;
#137509 = DIRECTION ( 'NONE',  ( 0.6724985119639503850, 0.7071067811865539010, -0.2185080122244115464 ) ) ;
#137510 = CARTESIAN_POINT ( 'NONE',  ( 0.4170028235400899397, 1.518763190251697370, -1.601383572969114599 ) ) ;
#137511 = CARTESIAN_POINT ( 'NONE',  ( -0.4504913314191360540, 15.51845925279681815, -11.99999999998148326 ) ) ;
#137512 = CARTESIAN_POINT ( 'NONE',  ( -8.012344526598182026E-15, 12.79687500034139802, -1.575800808251669460 ) ) ;
#137513 = ORIENTED_EDGE ( 'NONE', *, *, #156758, .F. ) ;
#137514 = CARTESIAN_POINT ( 'NONE',  ( 3.716343503921665459, 6.389465617000312569, -1.082531754730549967 ) ) ;
#137515 = CARTESIAN_POINT ( 'NONE',  ( 5.524252356588593926, 0.9672068372908498857, 1.715464803677963834 ) ) ;
#137516 = VERTEX_POINT ( 'NONE', #182268 ) ;
#137518 = CARTESIAN_POINT ( 'NONE',  ( 3.492840887459470522, -1.940756296261561209, -0.5346130827820451126 ) ) ;
#137517 = CARTESIAN_POINT ( 'NONE',  ( -0.006442494416806704600, -1.941642170872309281, -0.04679624317607820189 ) ) ;
#137519 = CARTESIAN_POINT ( 'NONE',  ( 5.466298696655274902, 1.874607906009964964, 1.329618201824170898 ) ) ;
#137521 = CARTESIAN_POINT ( 'NONE',  ( 2.957670719111748614, -0.5886736602933821949, 1.765425544305933014 ) ) ;
#137520 = CARTESIAN_POINT ( 'NONE',  ( -5.908321080505254841, 10.11506803722328129, 0.7998128361456291469 ) ) ;
#137522 = CARTESIAN_POINT ( 'NONE',  ( 7.523848900940885542, 7.742521570711348389, 0.7998128361456291469 ) ) ;
#137523 = FACE_BOUND ( 'NONE', #55312, .T. ) ;
#137524 = EDGE_CURVE ( 'NONE', #210323, #37563, #64186, .T. ) ;
#137525 = DIRECTION ( 'NONE',  ( 0.000000000000000000, 0.000000000000000000, 1.000000000000000000 ) ) ;
#137526 = CARTESIAN_POINT ( 'NONE',  ( -7.369020184227459858, 8.555943955475521889, 1.199719254218450271 ) ) ;
#137527 = CARTESIAN_POINT ( 'NONE',  ( -4.001064729808656573, 7.682009594836471500, 1.214306433183764966E-14 ) ) ;
#137528 = CARTESIAN_POINT ( 'NONE',  ( 6.216366674833015971, 1.951045902775162322, 0.7519257042096252341 ) ) ;
#137529 = CARTESIAN_POINT ( 'NONE',  ( 5.883875478650832491, 6.927238148923188454, -1.082531754730543083 ) ) ;
#137530 = SURFACE_STYLE_USAGE ( .BOTH. , #69283 ) ;
#137531 = FACE_OUTER_BOUND ( 'NONE', #156127, .T. ) ;
#137532 = CARTESIAN_POINT ( 'NONE',  ( 0.6272434487209905818, -1.734552980249819631, 0.5698080454362154379 ) ) ;
#137533 = CARTESIAN_POINT ( 'NONE',  ( -4.076197739202962467, 7.907314462378773001, 1.040834085586084257E-14 ) ) ;
#137534 = CARTESIAN_POINT ( 'NONE',  ( 2.250263858207638634, 1.700335624809163004, -0.3396627995243851061 ) ) ;
#137535 = SURFACE_STYLE_FILL_AREA ( #87699 ) ;
#137536 = CARTESIAN_POINT ( 'NONE',  ( 6.609000000000052388, 1.285212548570794588, 2.017169166534539038 ) ) ;
#137537 = EDGE_CURVE ( 'NONE', #195274, #25627, #60765, .T. ) ;
#137538 = CARTESIAN_POINT ( 'NONE',  ( -5.208303565944065738, 9.228104593576741621, -0.7998128361456231517 ) ) ;
#137539 = DIRECTION ( 'NONE',  ( 0.000000000000000000, 0.000000000000000000, -1.000000000000000000 ) ) ;
#137540 = CARTESIAN_POINT ( 'NONE',  ( 0.6903901511902330590, 1.067356595782501749, -1.773781848916009096 ) ) ;
#137541 = CARTESIAN_POINT ( 'NONE',  ( 5.654876981934024549, -1.436564326775534806, 1.126588154728463742 ) ) ;
#137542 = CARTESIAN_POINT ( 'NONE',  ( 3.555471618195928496, 1.543666060651678551, 1.210462546525910010 ) ) ;
#137543 = CARTESIAN_POINT ( 'NONE',  ( -0.6125000000000105915, -0.4791666659838753062, -1.060881119635955327 ) ) ;
#137544 = CARTESIAN_POINT ( 'NONE',  ( -8.045874094706015001, 11.47427131287732927, -1.199719254218446718 ) ) ;
#137545 = CARTESIAN_POINT ( 'NONE',  ( 7.935599982700328958, 8.152621489438862667, 0.7998128361456481317 ) ) ;
#137546 = CARTESIAN_POINT ( 'NONE',  ( 3.598385148150527346, -1.043669326629501848, 1.845773325594574077 ) ) ;
#137547 = CARTESIAN_POINT ( 'NONE',  ( 6.964048179274811012, 8.153752959689313684, 1.199719254218452047 ) ) ;
#137548 = CARTESIAN_POINT ( 'NONE',  ( -8.676328237741483207, 12.20980114641871062, -1.199719254218446718 ) ) ;
#137549 = AXIS2_PLACEMENT_3D ( 'NONE', #183829, #134058, #150284 ) ;
#137550 = CARTESIAN_POINT ( 'NONE',  ( 1.586871713678970730, 1.994102569620255228, 0.5559867524188369936 ) ) ;
#137552 = CARTESIAN_POINT ( 'NONE',  ( 1.364683531249988757, -0.8031249996585804185, 0.000000000000000000 ) ) ;
#137551 = CARTESIAN_POINT ( 'NONE',  ( -11.94980361490429921, 11.00332124735865769, 1.099999952233555733 ) ) ;
#137554 = ORIENTED_EDGE ( 'NONE', *, *, #70817, .T. ) ;
#137553 = CARTESIAN_POINT ( 'NONE',  ( 4.354274701107041956, 0.9498992632326860308, -2.008065553403962422 ) ) ;
#137555 = CARTESIAN_POINT ( 'NONE',  ( 1.301886090224623205, 1.538925899722990431, -1.707713671238730635 ) ) ;
#137557 = CARTESIAN_POINT ( 'NONE',  ( 0.5495624486224826022, 1.449728300881658383, 1.321815246172884040 ) ) ;
#137556 = CARTESIAN_POINT ( 'NONE',  ( 9.571693261567961741, 11.22969222899322617, 1.082531754730548412 ) ) ;
#137559 = CARTESIAN_POINT ( 'NONE',  ( 0.000000000000000000, -0.7875000000000005329, -4.012584370867899430 ) ) ;
#137558 = CARTESIAN_POINT ( 'NONE',  ( 7.688882512725796481, 8.142986817701137525, 0.000000000000000000 ) ) ;
#137560 = DIRECTION ( 'NONE',  ( 0.000000000000000000, 1.000000000000000000, 0.000000000000000000 ) ) ;
#137561 = PLANE ( 'NONE',  #134318 ) ;
#137562 = ORIENTED_EDGE ( 'NONE', *, *, #118912, .T. ) ;
#137563 = CARTESIAN_POINT ( 'NONE',  ( -5.576221682296247373, 6.207884856865704570, -0.9076712001952822462 ) ) ;
#137564 = CARTESIAN_POINT ( 'NONE',  ( 2.601700882821424976, 1.355260107747566334, 1.349524769375435973 ) ) ;
#137565 = CARTESIAN_POINT ( 'NONE',  ( -0.4573399425327669965, 6.471653648908428202, -3.262204865211126403 ) ) ;
#137566 = CARTESIAN_POINT ( 'NONE',  ( 4.190264469598516506, -1.706116514292443931, -0.2520994348873573654 ) ) ;
#137567 = CARTESIAN_POINT ( 'NONE',  ( 2.114470590943520634, 1.957170936680457052, 0.4852650170619755565 ) ) ;
#137568 = CARTESIAN_POINT ( 'NONE',  ( 4.465672607755381662, -2.229637596627360718, -0.5588700134179708234 ) ) ;
#137569 = CARTESIAN_POINT ( 'NONE',  ( 3.479979345725477291, 1.432071248269211505, 1.751504329374527158 ) ) ;
#137570 = CARTESIAN_POINT ( 'NONE',  ( 6.235009869002534622, 0.2045095422857303724, 2.096118580758222549 ) ) ;
#137571 = CARTESIAN_POINT ( 'NONE',  ( -4.312902262922974295, 8.045820050136510915, 0.7216878364870338292 ) ) ;
#137572 = CARTESIAN_POINT ( 'NONE',  ( 4.253014324580971284, -1.470476824294727702, -0.9843664617138027095 ) ) ;
#137574 = CARTESIAN_POINT ( 'NONE',  ( 1.113678556162515543, -2.235424308229993162, 0.5066684154252357741 ) ) ;
#137573 = CARTESIAN_POINT ( 'NONE',  ( 5.691390622686558487, 9.861982503101517139, 0.7998128361456341429 ) ) ;
#137575 = CARTESIAN_POINT ( 'NONE',  ( 6.140549721451361798, -1.552764191669778304, 0.9890077265983505672 ) ) ;
#137576 = CARTESIAN_POINT ( 'NONE',  ( -3.110706179331648169, 5.716575411607132118, 1.199719254218462483 ) ) ;
#137577 = CARTESIAN_POINT ( 'NONE',  ( 5.982419568921025999, -0.3181065885738461607, -2.168126298386578110 ) ) ;
#137578 = CARTESIAN_POINT ( 'NONE',  ( -4.817943484809863008, 6.714296380401858499, 1.599625672291263179 ) ) ;
#137579 = CARTESIAN_POINT ( 'NONE',  ( -2.123823618835070537, 5.629544655282869847, 1.040834085586084257E-14 ) ) ;
#137580 = CARTESIAN_POINT ( 'NONE',  ( -7.105968778775219263, 15.51980109384565409, 9.680178325039504372 ) ) ;
#137581 = CARTESIAN_POINT ( 'NONE',  ( 5.353992430378140099, -0.7485205528568983357, 1.930488744064068785 ) ) ;
#137582 = CARTESIAN_POINT ( 'NONE',  ( 0.9367328597341374463, -1.586666764284098807, 1.244388658875786424 ) ) ;
#137583 = VECTOR ( 'NONE', #201223, 1000.000000000000000 ) ;
#137584 = CARTESIAN_POINT ( 'NONE',  ( -1.364683531250010295, 5.738541667008088432, -0.7879004041258300672 ) ) ;
#137585 = CARTESIAN_POINT ( 'NONE',  ( 4.635331898966036590, -1.760702172612697458, 0.7822757977788937778 ) ) ;
#137586 = CARTESIAN_POINT ( 'NONE',  ( -8.012344526598182026E-15, 9.796875000341399797, -1.575800808251669460 ) ) ;
#137587 = CARTESIAN_POINT ( 'NONE',  ( 0.9498388403609931974, -2.005144016916958982, 0.9564107486674018332 ) ) ;
#137589 = VERTEX_POINT ( 'NONE', #61338 ) ;
#137588 = CARTESIAN_POINT ( 'NONE',  ( 2.876381804795541619, 6.437993120328354024, 0.3511878651327338674 ) ) ;
#137590 = DIRECTION ( 'NONE',  ( 0.000000000000000000, 0.000000000000000000, 1.000000000000000000 ) ) ;
#137591 = CARTESIAN_POINT ( 'NONE',  ( 2.191614386903386613, 5.708633884695917260, -0.7998128361456281477 ) ) ;
#137592 = CARTESIAN_POINT ( 'NONE',  ( -1.500000000000008216, 9.031250000682797818, 3.469446951953614189E-15 ) ) ;
#137593 = LINE ( 'NONE', #122490, #59568 ) ;
#137594 = CARTESIAN_POINT ( 'NONE',  ( 4.440767568709752311, -1.349020001278607550, -1.099687749275481741 ) ) ;
#137597 = EDGE_CURVE ( 'NONE', #20233, #139854, #176167, .T. ) ;
#137596 = CARTESIAN_POINT ( 'NONE',  ( 2.471086628630547288, 1.751123931924388089, 0.8847596551376719631 ) ) ;
#137595 = AXIS2_PLACEMENT_3D ( 'NONE', #140079, #123893, #58798 ) ;
#137599 = CARTESIAN_POINT ( 'NONE',  ( 1.364683531249988757, 2.446875000341415696, 1.214306433183764966E-14 ) ) ;
#137598 = CARTESIAN_POINT ( 'NONE',  ( 4.690231075323689325, 7.559354456931247412, 1.199719254218462483 ) ) ;
#137600 = CARTESIAN_POINT ( 'NONE',  ( -4.932365459154965492, 6.668011768565191844, 1.248136097290372337 ) ) ;
#137601 = CARTESIAN_POINT ( 'NONE',  ( 10.05353459973327368, 11.68787744023238417, -1.199719254218440723 ) ) ;
#137602 = CARTESIAN_POINT ( 'NONE',  ( 0.1333542156527478262, 0.001576319744088505292, -2.046049510433409768 ) ) ;
#137603 = CARTESIAN_POINT ( 'NONE',  ( -7.635213062790267458, 12.05949900656400686, 0.000000000000000000 ) ) ;
#137604 = CARTESIAN_POINT ( 'NONE',  ( -5.409340101728186134, 5.413244328212063472, 0.7216878364870317197 ) ) ;
#137605 = CARTESIAN_POINT ( 'NONE',  ( 4.874232570624013050, -2.001857581374043349, -0.2420344392276354561 ) ) ;
#137606 = CARTESIAN_POINT ( 'NONE',  ( 0.7258825447220511595, -2.147484179761431022, 0.7124928158122600941 ) ) ;
#137608 = EDGE_LOOP ( 'NONE', ( #25716, #84523, #192060, #198418 ) ) ;
#137607 = CARTESIAN_POINT ( 'NONE',  ( -5.717788096661253761, 7.693838750903348789, 1.599625672291269396 ) ) ;
#137609 = CARTESIAN_POINT ( 'NONE',  ( 0.6823417656249899377, 5.426041667008087543, -1.181850606188754593 ) ) ;
#137610 = CARTESIAN_POINT ( 'NONE',  ( 1.528351178377739927, 1.801267752838480840, 0.5040548479407629401 ) ) ;
#137611 = CARTESIAN_POINT ( 'NONE',  ( 0.3692042219665427893, -0.2092721526018372635, -1.721406745681583583 ) ) ;
#137613 = CARTESIAN_POINT ( 'NONE',  ( 3.720431430916489646, 2.081484170424623859, 0.6860852429351402826 ) ) ;
#137612 = CARTESIAN_POINT ( 'NONE',  ( 0.6801582343749761339, 1.973958333674710630, 1.178068619123801675 ) ) ;
#137614 = CARTESIAN_POINT ( 'NONE',  ( 5.754963864978503985, -1.823789643192383014, 1.413694633616706886 ) ) ;
#137615 = CARTESIAN_POINT ( 'NONE',  ( 6.784453644556415419, -2.020073987206136401, -0.4066529033334795873 ) ) ;
#137616 = CARTESIAN_POINT ( 'NONE',  ( 2.185399619353834311, -0.8303394849570409075, 1.755606585091240568 ) ) ;
#137617 = CARTESIAN_POINT ( 'NONE',  ( -4.812781342726871969, 6.637997537979888563, 1.443375672974064550 ) ) ;
#137619 = EDGE_CURVE ( 'NONE', #17249, #12495, #140271, .T. ) ;
#137618 = CARTESIAN_POINT ( 'NONE',  ( 3.607878275012302627, 7.223292064240769861, 0.7216878364870257245 ) ) ;
#137620 = CARTESIAN_POINT ( 'NONE',  ( -2.754243431018125239E-14, 0.2031250003414269978, 1.570758158831750295 ) ) ;
#137621 = CARTESIAN_POINT ( 'NONE',  ( 2.953750172290268150, -1.864168560446223033, -0.7691209412190866956 ) ) ;
#137622 = CARTESIAN_POINT ( 'NONE',  ( -3.416291520519271874, 6.929497840673697340, 1.040834085586084257E-14 ) ) ;
#137623 = CARTESIAN_POINT ( 'NONE',  ( -6.200875153403786477, 8.327716660428123419, -1.599625672291271394 ) ) ;
#137624 = CARTESIAN_POINT ( 'NONE',  ( 9.260382613333817403, 10.76253345609967660, -1.199719254218446718 ) ) ;
#137626 = CARTESIAN_POINT ( 'NONE',  ( 7.893838479094925198, -5.325441678136449752, -7.661067326845484970 ) ) ;
#137625 = CARTESIAN_POINT ( 'NONE',  ( 0.9788029507734037349, -0.04229004422508231970, -1.825371421953936757 ) ) ;
#137627 = CARTESIAN_POINT ( 'NONE',  ( -4.423703259808839938, 8.383013913077441259, 0.7998128361456352531 ) ) ;
#137628 = CARTESIAN_POINT ( 'NONE',  ( -1.040834085586084257E-14, -7.246166700194011767, -9.579665964935651701 ) ) ;
#137629 = CARTESIAN_POINT ( 'NONE',  ( -10.67000816626867810, 5.238978589329153834, 6.814456324518622488 ) ) ;
#137630 = ORIENTED_EDGE ( 'NONE', *, *, #132078, .F. ) ;
#137631 = CARTESIAN_POINT ( 'NONE',  ( 0.3038912542124502236, -0.5749842496362895794, 2.083749421223294540 ) ) ;
#137632 = CARTESIAN_POINT ( 'NONE',  ( -6.821160681006823268, 9.051383109298335228, 1.443375672974064550 ) ) ;
#137633 = CARTESIAN_POINT ( 'NONE',  ( 0.000000000000000000, 13.79999999999999893, 0.000000000000000000 ) ) ;
#137634 = CARTESIAN_POINT ( 'NONE',  ( -8.462260433223891098, 13.02438760540324481, -0.7998128361456281477 ) ) ;
#137635 = CARTESIAN_POINT ( 'NONE',  ( 5.549475203002828927, -1.825015992387307273, 0.8654263401719575199 ) ) ;
#137637 = ORIENTED_EDGE ( 'NONE', *, *, #75347, .T. ) ;
#137636 = CARTESIAN_POINT ( 'NONE',  ( 5.461676247742112800, -1.750072316323016963, -1.367929348606132800 ) ) ;
#137638 = CARTESIAN_POINT ( 'NONE',  ( -7.425025402139490360, 8.691559719698066289, 1.199719254218452047 ) ) ;
#137639 = CARTESIAN_POINT ( 'NONE',  ( 7.006866460164219212, 7.069099046480051385, -0.7998128361456281477 ) ) ;
#137640 = CARTESIAN_POINT ( 'NONE',  ( 5.559468503951485729, 0.4043298029084033685, -2.020654889403751486 ) ) ;
#137641 = CARTESIAN_POINT ( 'NONE',  ( 3.867814693791224112, -0.2004342644464084944, -2.006446243107910199 ) ) ;
#137642 = ORIENTED_EDGE ( 'NONE', *, *, #196604, .T. ) ;
#137643 = PRESENTATION_STYLE_ASSIGNMENT (( #55313 ) ) ;
#137644 = CARTESIAN_POINT ( 'NONE',  ( 2.920892028740289081, 5.495125569250587816, 1.199719254218452047 ) ) ;
#137646 = ORIENTED_EDGE ( 'NONE', *, *, #125292, .T. ) ;
#137645 = CARTESIAN_POINT ( 'NONE',  ( -7.469616286486262524, 7.679250187180907794, 0.7998128361456341429 ) ) ;
#137647 = CARTESIAN_POINT ( 'NONE',  ( 5.834480046583573554, 7.201333694826374199, -1.164487238324034557 ) ) ;
#137648 = CARTESIAN_POINT ( 'NONE',  ( 4.306017418194902469, -1.755500069608874281, 0.9912479507018998603 ) ) ;
#137649 = CARTESIAN_POINT ( 'NONE',  ( 3.573999110145977820, -1.774750109099573869, -0.4897004633943187191 ) ) ;
#137650 = CARTESIAN_POINT ( 'NONE',  ( 2.493954129951861720, 3.487142912321097299, -11.73313169142967460 ) ) ;
#137651 = CARTESIAN_POINT ( 'NONE',  ( 1.981525833354264243, -0.1160811445666837666, -2.304894087891403487 ) ) ;
#137652 = CARTESIAN_POINT ( 'NONE',  ( 3.386504508363381571, 7.172948703057747011, -0.7998128361456362523 ) ) ;
#137653 = CARTESIAN_POINT ( 'NONE',  ( 3.163507678178357541, 0.3205598832158839673, -2.137589075770351066 ) ) ;
#137654 = CARTESIAN_POINT ( 'NONE',  ( 8.341290820905593151, 10.75459192918846618, 1.599625672291281386 ) ) ;
#137655 = CIRCLE ( 'NONE', #148148, 0.08000000000000020983 ) ;
#137656 = CARTESIAN_POINT ( 'NONE',  ( -4.900382456335551140, 7.804531068111707270, 1.199719254218464037 ) ) ;
#137657 = CARTESIAN_POINT ( 'NONE',  ( -9.508802380709459712, 14.89824926832925911, -7.212919681761617241 ) ) ;
#137658 = DIRECTION ( 'NONE',  ( 0.000000000000000000, 1.000000000000000000, 0.000000000000000000 ) ) ;
#137659 = CARTESIAN_POINT ( 'NONE',  ( 2.711613914024712191, -1.850561042518297672, 0.2725550856255419818 ) ) ;
#137660 = CARTESIAN_POINT ( 'NONE',  ( 6.508667090220362716, 1.461156067397894054, -1.323708773930740268 ) ) ;
#137662 = CARTESIAN_POINT ( 'NONE',  ( -7.370792787684826486, 8.628288336167626582, -1.199719254218452047 ) ) ;
#137661 = CARTESIAN_POINT ( 'NONE',  ( 0.6823417656249899377, 4.926041667008086655, -1.181850606188754593 ) ) ;
#137663 = CARTESIAN_POINT ( 'NONE',  ( 1.787996309160574837, 1.523479866092191548, 1.596893430481533649 ) ) ;
#137664 = EDGE_LOOP ( 'NONE', ( #211411, #107629, #44805, #89076, #209103, #15992, #188091 ) ) ;
#137665 = CARTESIAN_POINT ( 'NONE',  ( 2.938820208668512901, 6.442724320172973584, -0.2506311418671491320 ) ) ;
#137666 = CARTESIAN_POINT ( 'NONE',  ( 5.203632029546647608, 4.965325544092860532, 1.040834085586084257E-14 ) ) ;
#137667 = CARTESIAN_POINT ( 'NONE',  ( -4.517891501851816649, 6.293959390292322986, -1.599625672291256295 ) ) ;
#137668 = DIRECTION ( 'NONE',  ( 0.000000000000000000, 0.000000000000000000, 1.000000000000000000 ) ) ;
#137669 = CARTESIAN_POINT ( 'NONE',  ( 6.016478623866945874, 1.324313071814016141, -1.460584582105582285 ) ) ;
#137670 = CARTESIAN_POINT ( 'NONE',  ( 5.690114378391165850, -1.042650834883801947, 2.058788517775663962 ) ) ;
#137671 = CARTESIAN_POINT ( 'NONE',  ( 0.2034672893990868703, -1.513989045467616146, -1.247398002513319781 ) ) ;
#137672 = CARTESIAN_POINT ( 'NONE',  ( 4.698127260392297444, 0.8867148737545665904, -1.862399597460895784 ) ) ;
#137673 = CARTESIAN_POINT ( 'NONE',  ( 6.182154858151487353, 6.314861544039274577, -0.7216878364870257245 ) ) ;
#137674 = EDGE_CURVE ( 'NONE', #101925, #58795, #200910, .T. ) ;
#137675 = CARTESIAN_POINT ( 'NONE',  ( 4.543917759235442944, 5.330267469643351852, 1.199719254218452935 ) ) ;
#137676 = CARTESIAN_POINT ( 'NONE',  ( 8.405692050348340771, 8.908988268268968724, 1.040834085586084257E-14 ) ) ;
#137677 = CARTESIAN_POINT ( 'NONE',  ( 1.364683531249988535, 3.967708333674751842, -0.7879004041258239610 ) ) ;
#137678 = CARTESIAN_POINT ( 'NONE',  ( -3.435200284438673535, 14.55196833484455254, 11.46022242559163473 ) ) ;
#137679 = CARTESIAN_POINT ( 'NONE',  ( 3.646780131951580461, 7.198401220678078971, -0.7216878364870267237 ) ) ;
#137680 = CARTESIAN_POINT ( 'NONE',  ( 6.514155524301521005, 2.165825943586483504, -0.1531846826740568268 ) ) ;
#137682 = CARTESIAN_POINT ( 'NONE',  ( 5.548353751603532835, -1.447698842669535413, 1.137588655622793876 ) ) ;
#137681 = CARTESIAN_POINT ( 'NONE',  ( 0.000000000000000000, -8.176568542494919711, 0.000000000000000000 ) ) ;
#137683 = CARTESIAN_POINT ( 'NONE',  ( 6.620655732516623537, 7.629137130509068498, 2.426260288887295058 ) ) ;
#137684 = CARTESIAN_POINT ( 'NONE',  ( 6.093348126157794198, -0.7399906200981146709, 2.062998119606203939 ) ) ;
#137685 = CARTESIAN_POINT ( 'NONE',  ( -0.3000000000000051514, 3.322650755865477645, -0.5865692111443002732 ) ) ;
#137686 = CARTESIAN_POINT ( 'NONE',  ( -5.029856876702963220, 6.770753873564038017, 1.447965164949674310 ) ) ;
#137687 = CARTESIAN_POINT ( 'NONE',  ( 0.000000000000000000, 0.4330127018922214077, 0.000000000000000000 ) ) ;
#137688 = CARTESIAN_POINT ( 'NONE',  ( 5.917965873332177829, 7.245500866451762612, 1.242176317587460943 ) ) ;
#137689 = CARTESIAN_POINT ( 'NONE',  ( -0.02298948590537253783, -1.708053232816408196, -0.8599758793098393195 ) ) ;
#137690 = CARTESIAN_POINT ( 'NONE',  ( 1.832500204630353124, 0.1694391671427826207, 1.761704050274701894 ) ) ;
#137692 = CARTESIAN_POINT ( 'NONE',  ( 6.393232662110455600, -0.1012007143085277561, -2.010677637860050382 ) ) ;
#137691 = STYLED_ITEM ( 'NONE', ( #63992 ), #210444 ) ;
#137694 = CARTESIAN_POINT ( 'NONE',  ( 4.341351955572036125, 0.4158663518127497793, -1.869753321735210916 ) ) ;
#137693 = CARTESIAN_POINT ( 'NONE',  ( -10.66756793585402363, 11.33991743478486391, 0.7998128361456462443 ) ) ;
#137695 = LINE ( 'NONE', #135559, #36395 ) ;
#137696 = CARTESIAN_POINT ( 'NONE',  ( 5.389095231685527843, 0.1428881311146198430, 1.964408359074652388 ) ) ;
#137697 = CARTESIAN_POINT ( 'NONE',  ( 6.533471379370169529, -0.1492333671020330821, 1.986230151431379598 ) ) ;
#137698 = CARTESIAN_POINT ( 'NONE',  ( -1.115562610750309283E-14, 11.06250000000000178, 1.500000000000001554 ) ) ;
#137699 = CARTESIAN_POINT ( 'NONE',  ( 2.904993682805886213, 1.579364189935757778, 1.002181356900035070 ) ) ;
#137701 = VERTEX_POINT ( 'NONE', #64538 ) ;
#137700 = CARTESIAN_POINT ( 'NONE',  ( 6.024008130617486856, -0.9641997184709062418, -1.430004917837023104 ) ) ;
#137703 = CARTESIAN_POINT ( 'NONE',  ( 2.575685996916329046, 5.948791396470269888, 0.7216878364870438212 ) ) ;
#137702 = CARTESIAN_POINT ( 'NONE',  ( 2.455956380646412196, 0.5873987694336445520, -2.127207350628975924 ) ) ;
#137704 = CARTESIAN_POINT ( 'NONE',  ( -1.201851678989727383E-14, 2.884375000341418804, 1.575800808251672791 ) ) ;
#137705 = CARTESIAN_POINT ( 'NONE',  ( 0.4146024514614836676, 0.7878568475925759040, 1.906473239439598677 ) ) ;
#137706 = CARTESIAN_POINT ( 'NONE',  ( 7.100719765255169236, 9.307259030929609267, -1.599625672291262513 ) ) ;
#137707 = CARTESIAN_POINT ( 'NONE',  ( -10.49131193887636826, 11.13428543831092909, 1.040834085586084257E-14 ) ) ;
#137708 = CARTESIAN_POINT ( 'NONE',  ( 10.91970695577495043, -6.134628647623513231, 5.204170427930421283E-15 ) ) ;
#137709 = CARTESIAN_POINT ( 'NONE',  ( -3.903858165731105778, 6.641919395739846799, 1.199719254218464037 ) ) ;
#137710 = CARTESIAN_POINT ( 'NONE',  ( -7.547439985188169054, -6.717993526550385397, -7.827294160508111887 ) ) ;
#137712 = CIRCLE ( 'NONE', #179135, 2.350000000000000533 ) ;
#137711 = STYLED_ITEM ( 'NONE', ( #97594 ), #203108 ) ;
#137713 = ORIENTED_EDGE ( 'NONE', *, *, #57944, .F. ) ;
#137714 = CARTESIAN_POINT ( 'NONE',  ( 2.875506610227479332, -0.2054619808779626633, 2.060159609288146232 ) ) ;
#137715 = CARTESIAN_POINT ( 'NONE',  ( 1.499999999999989120, 4.754166666666689522, 0.8660254037844524744 ) ) ;
#137716 = CARTESIAN_POINT ( 'NONE',  ( 3.988069740714122791, 7.804498464141805592, 0.7998128361456321445 ) ) ;
#137717 = CARTESIAN_POINT ( 'NONE',  ( -5.922807744518227224, 7.239652023730190677, 1.252291340712426981 ) ) ;
#137718 = CARTESIAN_POINT ( 'NONE',  ( 0.5045642862554244878, -2.004696059604444081, -0.2448167134727705085 ) ) ;
#137719 = CARTESIAN_POINT ( 'NONE',  ( -1.201851678989727383E-14, 2.884375000341418804, 1.575800808251672791 ) ) ;
#137720 = EDGE_CURVE ( 'NONE', #207748, #69931, #89945, .T. ) ;
#137721 = CARTESIAN_POINT ( 'NONE',  ( 1.364683531249988535, 3.905208333674751842, -0.7879004041258239610 ) ) ;
#137722 = ORIENTED_EDGE ( 'NONE', *, *, #45594, .F. ) ;
#137724 = CARTESIAN_POINT ( 'NONE',  ( 7.768458830950378591, 12.00702636951006497, 1.040834085586084257E-14 ) ) ;
#137723 = CARTESIAN_POINT ( 'NONE',  ( 0.07459516483346911864, 0.007201286963446140027, -1.755573347271717211 ) ) ;
#137725 = CARTESIAN_POINT ( 'NONE',  ( 6.784528966312857179, -1.956291195211720346, 0.4871289682274528299 ) ) ;
#137726 = CARTESIAN_POINT ( 'NONE',  ( 6.456256392861089211, -1.172487466661990663, 1.515489988593403226 ) ) ;
#137727 = FACE_BOUND ( 'NONE', #38658, .T. ) ;
#137728 = CARTESIAN_POINT ( 'NONE',  ( 3.878626735558046157, -0.2160506499642600997, -2.180900317982924275 ) ) ;
#137729 = CARTESIAN_POINT ( 'NONE',  ( 0.7499999999999885647, 2.347916667349486453, -1.299038105676652899 ) ) ;
#137730 = CARTESIAN_POINT ( 'NONE',  ( 2.654443970922310214, 1.898414275235399407, 0.2300336082040748686 ) ) ;
#137731 = CARTESIAN_POINT ( 'NONE',  ( -4.706651882238427120, 8.642844295920152575, 1.040834085586084257E-14 ) ) ;
#137732 = EDGE_CURVE ( 'NONE', #55162, #146442, #102748, .T. ) ;
#137733 = CARTESIAN_POINT ( 'NONE',  ( 4.487385655998878953, 6.258369236797239665, 1.443375672974062551 ) ) ;
#137735 = CARTESIAN_POINT ( 'NONE',  ( 1.124625310196948558, 0.3961260723950796314, 1.976952190469769111 ) ) ;
#137734 = PRESENTATION_STYLE_ASSIGNMENT (( #71621 ) ) ;
#137736 = CARTESIAN_POINT ( 'NONE',  ( -8.012344526598182026E-15, 11.35937500034139980, -1.575800808251669460 ) ) ;
#137738 = CARTESIAN_POINT ( 'NONE',  ( -4.782994330570982555, 8.802186828966616972, 0.000000000000000000 ) ) ;
#137737 = CARTESIAN_POINT ( 'NONE',  ( 6.462441986028243157, -2.002789442531027309, -0.8901952361822995652 ) ) ;
#137740 = EDGE_LOOP ( 'NONE', ( #130866, #84408, #99103, #80360 ) ) ;
#137739 = CARTESIAN_POINT ( 'NONE',  ( 3.539825753290166688, 0.7759033148657649148, -1.540472896381483769 ) ) ;
#137741 = CARTESIAN_POINT ( 'NONE',  ( 0.1399997263885795484, 5.723012109828673921, -2.593777676649943409 ) ) ;
#137742 = CARTESIAN_POINT ( 'NONE',  ( 6.446011968293428041, 9.607765498729298415, -1.199719254218440723 ) ) ;
#137743 = CARTESIAN_POINT ( 'NONE',  ( 4.904298879841284098, 6.744767997946721216, 1.599625672291267398 ) ) ;
#137744 = PLANE ( 'NONE',  #95565 ) ;
#137745 = CARTESIAN_POINT ( 'NONE',  ( 0.6780837441340243910, -1.046368970337024473, -1.659334490400856454 ) ) ;
#137746 = CYLINDRICAL_SURFACE ( 'NONE', #53621, 1.000000000000000000 ) ;
#137747 = CARTESIAN_POINT ( 'NONE',  ( 5.138703914779377158, 5.953908307786102583, 1.199719254218462483 ) ) ;
#137748 = CARTESIAN_POINT ( 'NONE',  ( 3.673896439623286714, 4.156855427197417185, -0.9999999999999940048 ) ) ;
#137749 = EDGE_LOOP ( 'NONE', ( #150693, #35954, #103921, #122679, #139295, #134336, #190793, #94344, #176626 ) ) ;
#137750 = DIRECTION ( 'NONE',  ( -1.000000000000000000, 0.000000000000000000, 0.000000000000000000 ) ) ;
#137751 = ORIENTED_EDGE ( 'NONE', *, *, #198196, .T. ) ;
#137752 = CARTESIAN_POINT ( 'NONE',  ( 3.791515551631476910, 1.704436734775734985, -0.6137984976519753610 ) ) ;
#137753 = ORIENTED_EDGE ( 'NONE', *, *, #77660, .F. ) ;
#137754 = CARTESIAN_POINT ( 'NONE',  ( 7.865701674222579598, 12.32840238656838139, -0.7998128361456352531 ) ) ;
#137755 = CARTESIAN_POINT ( 'NONE',  ( 5.110497557708379546, 4.926945003606695295, -0.7998128361456481317 ) ) ;
#137756 = CARTESIAN_POINT ( 'NONE',  ( 4.916585655956178691, -0.6154711373431708266, -1.703840371469134807 ) ) ;
#137757 = CARTESIAN_POINT ( 'NONE',  ( 5.817857313595521163, 9.801600942587855414, -0.7216878364870458196 ) ) ;
#137758 = CARTESIAN_POINT ( 'NONE',  ( 5.102592784488711786, 6.504070869828495027, 1.211835919174956366 ) ) ;
#137759 = MECHANICAL_DESIGN_GEOMETRIC_PRESENTATION_REPRESENTATION (  '', ( #196501 ), #33984 ) ;
#137761 = CARTESIAN_POINT ( 'NONE',  ( 1.364683531249997417, 13.98437500034140157, 2.602085213965210642E-15 ) ) ;
#137760 = CARTESIAN_POINT ( 'NONE',  ( 5.055058894927250357, 1.547480351173950552, -1.033501273311630886 ) ) ;
#137762 = CARTESIAN_POINT ( 'NONE',  ( 2.917496427270527715, -1.288711974188415654, -1.417462588220135933 ) ) ;
#137763 = CARTESIAN_POINT ( 'NONE',  ( -11.55950211276791428, 12.22000000000000064, -3.221476510067114329 ) ) ;
#137764 = CARTESIAN_POINT ( 'NONE',  ( -11.01567899581106325, 5.044704703271206903, 4.264317011375222677 ) ) ;
#137765 = EDGE_CURVE ( 'NONE', #73840, #171296, #178291, .T. ) ;
#137766 = CARTESIAN_POINT ( 'NONE',  ( -1.084637062511556005, 3.182371192708035146, 1.105835307554803082 ) ) ;
#137767 = CARTESIAN_POINT ( 'NONE',  ( 0.000000000000000000, 8.500000000000000000, 0.000000000000000000 ) ) ;
#137768 = CARTESIAN_POINT ( 'NONE',  ( 7.836249599018724865, 9.205007956019091608, -1.082531754730537976 ) ) ;
#137769 = CARTESIAN_POINT ( 'NONE',  ( -2.591579918506545344, 6.175260338232929413, 1.040834085586084257E-14 ) ) ;
#137770 = SURFACE_SIDE_STYLE ('',( #21828 ) ) ;
#137771 = CARTESIAN_POINT ( 'NONE',  ( 0.8496949173334772398, 2.088161746953997255, -0.1042977956757246832 ) ) ;
#137772 = CARTESIAN_POINT ( 'NONE',  ( 5.367048706163317640, 7.354919138647580290, -1.599625672291281386 ) ) ;
#137773 = CARTESIAN_POINT ( 'NONE',  ( 0.1119280604304096899, -0.7754228321929098611, -1.651232954423286436 ) ) ;
#137774 = CARTESIAN_POINT ( 'NONE',  ( -3.879604511804807032, 7.677955697080923514, 0.7998128361456341429 ) ) ;
#137775 = CARTESIAN_POINT ( 'NONE',  ( 2.819161699164650869, -0.1809198688003388622, 1.816599095187728219 ) ) ;
#137776 = CARTESIAN_POINT ( 'NONE',  ( -5.951324661304366437, 4.742844146919000359, 2.438848701836275001 ) ) ;
#137777 = CARTESIAN_POINT ( 'NONE',  ( 1.652457426684301955, 1.892030339952909035, 0.2773405859870237133 ) ) ;
#137778 = CARTESIAN_POINT ( 'NONE',  ( 1.855843448759408210, -0.6666243292093411155, 1.853429361541816700 ) ) ;
#137779 = CARTESIAN_POINT ( 'NONE',  ( 3.386211154777326815, -0.3816624740031882568, -1.904027918096486527 ) ) ;
#137780 = VERTEX_POINT ( 'NONE', #93869 ) ;
#137781 = CARTESIAN_POINT ( 'NONE',  ( 3.649297074908570321E-15, -6.789018801444764277E-15, 0.2598076211376221800 ) ) ;
#137782 = CARTESIAN_POINT ( 'NONE',  ( -5.004894982100124068, 5.868074229652107121, 1.199719254218452935 ) ) ;
#137784 = CARTESIAN_POINT ( 'NONE',  ( 4.465154236216789307, -1.701427117168831549, 1.265499569954648962 ) ) ;
#137783 = CARTESIAN_POINT ( 'NONE',  ( 5.982890925380405456, 10.20206618957764100, 0.000000000000000000 ) ) ;
#137785 = CARTESIAN_POINT ( 'NONE',  ( 0.1421055763938798289, -7.985988503423667062, 9.537847510268184337 ) ) ;
#137786 = CARTESIAN_POINT ( 'NONE',  ( 8.561083932025322696, 12.07534945641652158, -1.199719254218446718 ) ) ;
#137787 = CARTESIAN_POINT ( 'NONE',  ( -4.437261413422502798, 8.398831758960053406, 0.000000000000000000 ) ) ;
#137788 = VERTEX_POINT ( 'NONE', #159907 ) ;
#137789 = AXIS2_PLACEMENT_3D ( 'NONE', #43125, #140635, #62537 ) ;
#137790 = CARTESIAN_POINT ( 'NONE',  ( 5.688527969385528849, 8.794310509995222347, -1.199719254218452047 ) ) ;
#137792 =( BOUNDED_CURVE ( )  B_SPLINE_CURVE ( 2, ( #95426, #79138, #149469 ),
 .UNSPECIFIED., .F., .T. ) 
 B_SPLINE_CURVE_WITH_KNOTS ( ( 3, 3 ),
 ( 0.6458333333333333703, 0.6514247127752519351 ),
 .UNSPECIFIED. ) 
 CURVE ( )  GEOMETRIC_REPRESENTATION_ITEM ( )  RATIONAL_B_SPLINE_CURVE ( ( 0.9330127018922192983, 0.9330127018922197424, 0.9764392566477293478 ) ) 
 REPRESENTATION_ITEM ( '' )  );
#137791 = CARTESIAN_POINT ( 'NONE',  ( 0.000000000000000000, -5.199999999999996625, 0.000000000000000000 ) ) ;
#137793 = CARTESIAN_POINT ( 'NONE',  ( 4.389149243953620605, 1.629682310347341456, -0.8231139397327084106 ) ) ;
#137794 = CARTESIAN_POINT ( 'NONE',  ( 3.929058411375439874, 5.499999999999998224, 0.7500000000000006661 ) ) ;
#137795 = CARTESIAN_POINT ( 'NONE',  ( -8.351459436338023679, 12.68719374246231624, -0.7216878364870267237 ) ) ;
#137796 = CARTESIAN_POINT ( 'NONE',  ( -5.386518286579200954, 7.671588192869585043, 1.336358942847740927 ) ) ;
#137797 = CARTESIAN_POINT ( 'NONE',  ( 3.880185816268708177, 5.955652630921238533, -1.265242915204408458 ) ) ;
#137798 = CARTESIAN_POINT ( 'NONE',  ( 4.153091690245942047, -1.555063956268587066, -1.039456662654779207 ) ) ;
#137799 = CARTESIAN_POINT ( 'NONE',  ( 7.391166297744269365, 11.77477778067701664, 1.040834085586084257E-14 ) ) ;
#137800 = CARTESIAN_POINT ( 'NONE',  ( 2.578635874325632127, -1.843646926959886523, -0.5589146710999506329 ) ) ;
#137801 = CARTESIAN_POINT ( 'NONE',  ( 1.145901822213557075, 2.800000000000024247, 0.9291478600312689240 ) ) ;
#137802 = AXIS2_PLACEMENT_3D ( 'NONE', #212505, #130288, #170157 ) ;
#137803 = CARTESIAN_POINT ( 'NONE',  ( 1.364683531249996529, 8.526041667008065872, 0.7879004041258405033 ) ) ;
#137804 = CARTESIAN_POINT ( 'NONE',  ( -7.074657228232555717, 7.148188275893099686, 1.040834085586084257E-14 ) ) ;
#137805 = CARTESIAN_POINT ( 'NONE',  ( 4.792970997630896512, 5.550553237779539018, 1.199719254218464037 ) ) ;
#137806 = CARTESIAN_POINT ( 'NONE',  ( -6.265276382846530545, 6.482112999508623297, 0.000000000000000000 ) ) ;
#137807 = CARTESIAN_POINT ( 'NONE',  ( 0.7029266809492543677, 1.957958796488759035, 0.8061104088524527755 ) ) ;
#137808 = CARTESIAN_POINT ( 'NONE',  ( 8.380911511541880188, 12.92948053010758258, 0.7998128361456462443 ) ) ;
#137810 = ORIENTED_EDGE ( 'NONE', *, *, #173301, .T. ) ;
#137809 = CARTESIAN_POINT ( 'NONE',  ( -1.455271222711091106, 4.347661690319585048, 0.3949897977301430885 ) ) ;
#137811 = CARTESIAN_POINT ( 'NONE',  ( 5.453992358814952368, -0.7503507308065425763, 1.929658000011783336 ) ) ;
#137813 = CARTESIAN_POINT ( 'NONE',  ( 1.364683531249988535, 2.676041667008082214, 0.7879004041258500513 ) ) ;
#137812 = CARTESIAN_POINT ( 'NONE',  ( 0.1691535571452691677, 1.059206136818511501, 1.505872603892892458 ) ) ;
#137814 = CARTESIAN_POINT ( 'NONE',  ( 5.274211419651455124, 2.028235465341983623, -1.081840468886515305 ) ) ;
#137815 = CARTESIAN_POINT ( 'NONE',  ( 5.314433026876846711, 9.143996264757578984, -0.7216878364870267237 ) ) ;
#137817 = FACE_OUTER_BOUND ( 'NONE', #125724, .T. ) ;
#137816 = CARTESIAN_POINT ( 'NONE',  ( 3.607878275012302627, 7.223292064240769861, 0.7216878364870257245 ) ) ;
#137818 = CARTESIAN_POINT ( 'NONE',  ( 1.254322107098894801, 0.9329652568456588968, 2.093986936342966398 ) ) ;
#137819 = CARTESIAN_POINT ( 'NONE',  ( 7.726139724254739605, -6.443545996361851103, -7.681709917290612921 ) ) ;
#137820 = CARTESIAN_POINT ( 'NONE',  ( -5.915100157312088491, 10.12297696016459092, -0.7998128361456362523 ) ) ;
#137821 = CARTESIAN_POINT ( 'NONE',  ( 4.505766059781188382, -0.8317635995198893184, -1.754939027834252485 ) ) ;
#137822 = ORIENTED_EDGE ( 'NONE', *, *, #163282, .T. ) ;
#137823 = CARTESIAN_POINT ( 'NONE',  ( 8.066738210006679566, 10.43428054980638997, 1.443375672974076540 ) ) ;
#137824 = ORIENTED_EDGE ( 'NONE', *, *, #63903, .T. ) ;
#137825 = CARTESIAN_POINT ( 'NONE',  ( 5.906500813101932756, -1.903809282439900219, -0.1807861040028224398 ) ) ;
#137826 = CARTESIAN_POINT ( 'NONE',  ( 5.155482549980198392, 1.942097955248718533, -0.5424665614216088727 ) ) ;
#137828 = DIRECTION ( 'NONE',  ( 1.000000000000000000, 0.000000000000000000, -3.491481338843133355E-15 ) ) ;
#137827 = CARTESIAN_POINT ( 'NONE',  ( -8.715193815486133033, 9.062147627688959872, 0.7998128361456462443 ) ) ;
#137829 = CARTESIAN_POINT ( 'NONE',  ( 1.001543065824772753E-15, -1.859374999522040550, 3.793834371823811669 ) ) ;
#137831 = CARTESIAN_POINT ( 'NONE',  ( 1.199668116878411128, -1.770032029468296964, -0.005122706785119778526 ) ) ;
#137830 = CARTESIAN_POINT ( 'NONE',  ( 2.923863239626739663, 1.160869195616637706, -1.738502609096896467 ) ) ;
#137832 = CARTESIAN_POINT ( 'NONE',  ( 11.33772463945037146, 10.19999999999998153, 3.599999999999999201 ) ) ;
#137834 = CARTESIAN_POINT ( 'NONE',  ( 3.644716121489647076, -1.874467426877159504, 1.319156965210349197 ) ) ;
#137833 = CARTESIAN_POINT ( 'NONE',  ( 2.898410978271408922, 6.603506251283770112, -0.7998128361456362523 ) ) ;
#137835 = CARTESIAN_POINT ( 'NONE',  ( 1.851089384485626210, 1.735827849189163663, -0.1260499613615853887 ) ) ;
#137836 = CARTESIAN_POINT ( 'NONE',  ( 2.842405760359353106, 6.467890487061221272, -0.7998128361456291469 ) ) ;
#137837 = CARTESIAN_POINT ( 'NONE',  ( -4.875303370615012177, 4.879929216858088559, -0.6230339956202604057 ) ) ;
#137838 = CARTESIAN_POINT ( 'NONE',  ( 2.389626358114539162, -0.004507738041977306029, 1.734034291262590788 ) ) ;
#137839 = CARTESIAN_POINT ( 'NONE',  ( 2.190095119440739424, -1.416971674389384761, -1.645159614449900776 ) ) ;
#137840 = CARTESIAN_POINT ( 'NONE',  ( 5.341022448779654930, 8.318611059296550536, 1.199719254218462483 ) ) ;
#137841 = CARTESIAN_POINT ( 'NONE',  ( 5.032435514249763209, 0.5899841883351600869, 1.928258608204669766 ) ) ;
#137842 = CARTESIAN_POINT ( 'NONE',  ( 1.968750000000001332, 0.7852924748298835134, -1.895863743164130755 ) ) ;
#137843 =( BOUNDED_CURVE ( )  B_SPLINE_CURVE ( 2, ( #184035, #166738, #18330, #2062, #68134, #51925, #82269 ),
 .UNSPECIFIED., .F., .T. ) 
 B_SPLINE_CURVE_WITH_KNOTS ( ( 3, 2, 2, 3 ),
 ( 0.4141369526679988811, 0.4166666666666666852, 0.4226190476190476164, 0.4227888527529243823 ),
 .UNSPECIFIED. ) 
 CURVE ( )  GEOMETRIC_REPRESENTATION_ITEM ( )  RATIONAL_B_SPLINE_CURVE ( ( 0.9345202395942611151, 0.9430618748659218564, 1.000000000000000000, 0.8660254037844387076, 1.000000000000000000, 0.9961780715265932118, 0.9925742013667540053 ) ) 
 REPRESENTATION_ITEM ( '' )  );
#137844 = CONICAL_SURFACE ( 'NONE', #193174, 2.000000000000000000, 0.01725463330310792257 ) ;
#137845 = CARTESIAN_POINT ( 'NONE',  ( -1.201851678989727383E-14, 2.868750000682821266, -1.732050807568863648 ) ) ;
#137846 = CARTESIAN_POINT ( 'NONE',  ( 1.131717742382963632, -1.219707097817297692, -1.491085513105432581 ) ) ;
#137847 = CARTESIAN_POINT ( 'NONE',  ( -1.402160292154681736E-14, 15.17187500034140157, 1.575800808251682339 ) ) ;
#137848 = CARTESIAN_POINT ( 'NONE',  ( 4.553117645631366450, 0.3812515705259692522, 2.188315991368384505 ) ) ;
#137849 = ORIENTED_EDGE ( 'NONE', *, *, #182170, .F. ) ;
#137850 = CARTESIAN_POINT ( 'NONE',  ( -0.1110810684433168327, 2.049790377237853178, -2.213868588080004418 ) ) ;
#137851 = CARTESIAN_POINT ( 'NONE',  ( -0.7500000000000006661, -0.1416666666666441254, -1.299038105676652011 ) ) ;
#137852 = CARTESIAN_POINT ( 'NONE',  ( 7.019370843573166319, 9.212351955633947043, 1.599625672291281386 ) ) ;
#137853 = CARTESIAN_POINT ( 'NONE',  ( 5.246642258364164313, 8.104537820524768676, -1.082531754730549078 ) ) ;
#137854 = CARTESIAN_POINT ( 'NONE',  ( 1.001543065824772753E-15, -1.771874999522040861, 3.793834371823810780 ) ) ;
#137855 = CARTESIAN_POINT ( 'NONE',  ( 0.6104036325267605534, -0.7939654203579590286, 2.074740863049700845 ) ) ;
#137857 = EDGE_CURVE ( 'NONE', #190246, #116745, #17558, .T. ) ;
#137856 = CARTESIAN_POINT ( 'NONE',  ( 6.162552467866693640, -0.7048080804108979303, -1.831077584432870609 ) ) ;
#137858 = CARTESIAN_POINT ( 'NONE',  ( 8.419250204406344196, 12.76628297187536809, 1.040834085586084257E-14 ) ) ;
#137859 = CARTESIAN_POINT ( 'NONE',  ( -1.422919017935815766, 3.902251674285432514, -0.5004465702263605209 ) ) ;
#137860 = CARTESIAN_POINT ( 'NONE',  ( 6.503223684228603751, 1.875565888388399660, 1.264963274899598256 ) ) ;
#137861 = COLOUR_RGB ( '', 0.08235294, 0.09019608, 0.10196078) ;
#137862 = CARTESIAN_POINT ( 'NONE',  ( -5.506019780925599960, 5.596313630600862510, 0.7216878364870257245 ) ) ;
#137863 = CARTESIAN_POINT ( 'NONE',  ( 3.279784535431028658, -1.988673744353728123, 0.5473864365612387539 ) ) ;
#137864 = CARTESIAN_POINT ( 'NONE',  ( -4.381256195510448315, 8.263215994737505454, 1.040834085586084257E-14 ) ) ;
#137865 = CARTESIAN_POINT ( 'NONE',  ( 1.499999999999989120, 3.285416667349486897, 0.8660254037844524744 ) ) ;
#137866 = CARTESIAN_POINT ( 'NONE',  ( -1.001543065824772872E-14, 5.134375000341421469, 1.575800808251672791 ) ) ;
#137867 = CARTESIAN_POINT ( 'NONE',  ( 4.868341698904518289, -1.223052743625025141, 1.415352931214426846 ) ) ;
#137868 = CARTESIAN_POINT ( 'NONE',  ( 3.357800782942537143, 0.03855433513636970927, -1.733892557700001502 ) ) ;
#137869 = CARTESIAN_POINT ( 'NONE',  ( 3.350842269037973331, 0.4194941847268919832, -1.688999647770361490 ) ) ;
#137870 = CARTESIAN_POINT ( 'NONE',  ( 0.8027370721926800901, 1.731296644042874755, -1.502618532894074876 ) ) ;
#137871 = CARTESIAN_POINT ( 'NONE',  ( -1.364683531250012516, 4.051041667008088432, -0.7879004041258300672 ) ) ;
#137872 = CARTESIAN_POINT ( 'NONE',  ( 4.827721544939969966, 1.073412050285113661, -1.793994897088858176 ) ) ;
#137873 = CARTESIAN_POINT ( 'NONE',  ( 0.3043191165176573620, 1.600368420507289668, 0.9101283655772866021 ) ) ;
#137875 = EDGE_LOOP ( 'NONE', ( #121461, #145915, #3409, #23916 ) ) ;
#137874 = DIRECTION ( 'NONE',  ( 0.000000000000000000, -1.000000000000000000, 0.000000000000000000 ) ) ;
#137876 = CARTESIAN_POINT ( 'NONE',  ( 0.5807041986926939625, -0.7231374404764076003, 1.882475062126743204 ) ) ;
#137877 = CARTESIAN_POINT ( 'NONE',  ( 0.9848172835694012361, -1.340914915981223476, 1.642866500755429948 ) ) ;
#137878 = CARTESIAN_POINT ( 'NONE',  ( -1.138412281109779656E-15, -9.418601272600234608, 9.907592596884327918 ) ) ;
#137879 = CARTESIAN_POINT ( 'NONE',  ( -2.937312835655025101, 6.578615408239493867, 1.040834085586084257E-14 ) ) ;
#137880 = CARTESIAN_POINT ( 'NONE',  ( -8.202846631467911820, 9.528741477256060577, 1.199719254218462483 ) ) ;
#137881 = CARTESIAN_POINT ( 'NONE',  ( 4.981731378017507872, 7.899438143407371271, -1.199719254218452047 ) ) ;
#137882 = CARTESIAN_POINT ( 'NONE',  ( 2.772263606761758759, 2.110060413066455975, -0.2101530891244970389 ) ) ;
#137883 = CYLINDRICAL_SURFACE ( 'NONE', #129185, 2.000000000000000000 ) ;
#137884 = CARTESIAN_POINT ( 'NONE',  ( 4.477060521952030747, -0.002618581577289170060, -1.825872481161804561 ) ) ;
#137885 = ORIENTED_EDGE ( 'NONE', *, *, #156347, .T. ) ;
#137886 = CARTESIAN_POINT ( 'NONE',  ( -7.469616286486262524, 7.679250187180907794, 0.7998128361456341429 ) ) ;
#137887 = UNCERTAINTY_MEASURE_WITH_UNIT (LENGTH_MEASURE( 1.000000000000000082E-05 ), #198809, 'distance_accuracy_value', 'NONE');
#137888 = DIRECTION ( 'NONE',  ( -4.440892098500630106E-16, -3.330669073875473073E-16, -1.000000000000000000 ) ) ;
#137889 = CARTESIAN_POINT ( 'NONE',  ( 1.001543065824772753E-15, -0.4593749995220425819, 3.793834371823811669 ) ) ;
#137890 = CARTESIAN_POINT ( 'NONE',  ( -6.398558430645608475, 9.552403038140164782, -1.199719254218440723 ) ) ;
#137891 = CARTESIAN_POINT ( 'NONE',  ( 2.654562054903885304, 2.005031730908119147, 0.2428967267811207309 ) ) ;
#137892 = CARTESIAN_POINT ( 'NONE',  ( 6.036183878773405453, 1.092744051193066834, -1.917163762461614240 ) ) ;
#137893 = CARTESIAN_POINT ( 'NONE',  ( -3.610214042988883598, 7.433943160120816351, 0.7998128361456352531 ) ) ;
#137894 = CARTESIAN_POINT ( 'NONE',  ( 4.381604285809827637, -1.781765127997904763, 0.5371461504297748712 ) ) ;
#137895 = CARTESIAN_POINT ( 'NONE',  ( 3.728655938958122196, 4.308852335994623139, -1.199719254218446718 ) ) ;
#137896 = CARTESIAN_POINT ( 'NONE',  ( 0.000000000000000000, 0.000000000000000000, 0.4894596299587841703 ) ) ;
#137897 = CARTESIAN_POINT ( 'NONE',  ( -5.427341564172148303, 5.226320001155936090, 0.000000000000000000 ) ) ;
#137898 = CARTESIAN_POINT ( 'NONE',  ( -8.320953590485107298, 10.73086516036454618, 1.599625672291269396 ) ) ;
#137899 = CARTESIAN_POINT ( 'NONE',  ( 5.584540971669589737, -1.782103179330214449, -0.3958202769075992444 ) ) ;
#137901 = CARTESIAN_POINT ( 'NONE',  ( -3.975490874141025088, 7.849583646728635955, 0.01022619435145193101 ) ) ;
#137900 = CARTESIAN_POINT ( 'NONE',  ( -5.164730172163054966, 4.990216387137135889, -0.7998128361456362523 ) ) ;
#137902 = CARTESIAN_POINT ( 'NONE',  ( -1.364683531250014514, -0.4697916663252449943, 0.7879004041258379498 ) ) ;
#137903 = CARTESIAN_POINT ( 'NONE',  ( 0.3679294144470013905, -0.4713284034136792644, 1.668465712161566916 ) ) ;
#137904 = CARTESIAN_POINT ( 'NONE',  ( 0.6381061630796550643, -1.494939029692418320, 0.8907679528266756463 ) ) ;
#137905 = CARTESIAN_POINT ( 'NONE',  ( 5.479250216003205054, -0.05159697844352681417, -2.307286710698839727 ) ) ;
#137906 = CARTESIAN_POINT ( 'NONE',  ( 4.258142763143749399, 7.125527769379820242, 1.199719254218451159 ) ) ;
#137907 = CARTESIAN_POINT ( 'NONE',  ( 1.616555492630408875, 1.386288697630438715, -1.524948804171057493 ) ) ;
#137908 = CARTESIAN_POINT ( 'NONE',  ( 6.362725135800558540, -0.7832434641057796076, 2.160938040253687742 ) ) ;
#137909 = CARTESIAN_POINT ( 'NONE',  ( 1.499999999999993117, 11.38541666734946567, 0.8660254037844408170 ) ) ;
#137910 = CARTESIAN_POINT ( 'NONE',  ( -7.259464905474441565, 7.434073576000447048, -0.7998128361456362523 ) ) ;
#137911 = CARTESIAN_POINT ( 'NONE',  ( 6.121928861531041655, -1.040746078065577063, -1.554202398018275755 ) ) ;
#137913 = CARTESIAN_POINT ( 'NONE',  ( -4.390861645979385663, 6.216034235099629157, -1.599625672291271394 ) ) ;
#137912 = CARTESIAN_POINT ( 'NONE',  ( 3.041163856788456687, 0.05134138945498378792, 1.911883771832747048 ) ) ;
#137914 = CARTESIAN_POINT ( 'NONE',  ( 5.356176587289051660, 2.204499490778097481, -0.1052899746726426722 ) ) ;
#137915 = CARTESIAN_POINT ( 'NONE',  ( -1.225000000000056044, 1.291666667349482100, -0.7072540797573317883 ) ) ;
#137916 = CARTESIAN_POINT ( 'NONE',  ( 0.7500000000000006661, 10.58333333333333393, 1.299038105676657340 ) ) ;
#137917 = CARTESIAN_POINT ( 'NONE',  ( 5.085717018457579286, 6.066329622022862189, -1.082531754730548412 ) ) ;
#137918 = CARTESIAN_POINT ( 'NONE',  ( -3.973948422136968084, 7.650373902552835226, -0.7216878364870458196 ) ) ;
#137919 = CARTESIAN_POINT ( 'NONE',  ( 5.690118541956746157, 1.263103799472656164, 1.703077153987264669 ) ) ;
#137920 = CARTESIAN_POINT ( 'NONE',  ( 2.766999470516241288, -1.591810197153446182, 1.670866638877396060 ) ) ;
#137921 = CARTESIAN_POINT ( 'NONE',  ( 3.508209890309890167, 1.962046631884439174, 0.002529298861464468473 ) ) ;
#137922 = CARTESIAN_POINT ( 'NONE',  ( 0.9362904128984714802, -1.094497954693674391, 1.627855050370475620 ) ) ;
#137923 = CARTESIAN_POINT ( 'NONE',  ( 2.684151225825664788, 5.114964949229812596, -1.082531754730543083 ) ) ;
#137924 = CARTESIAN_POINT ( 'NONE',  ( 5.727393547130178675, 5.646656991265468939, 0.000000000000000000 ) ) ;
#137925 = ORIENTED_EDGE ( 'NONE', *, *, #175342, .T. ) ;
#137926 = CARTESIAN_POINT ( 'NONE',  ( 5.682827415814322158, 1.645762192317705486, -1.164983060713747909 ) ) ;
#137927 = CARTESIAN_POINT ( 'NONE',  ( -10.15913717534155047, 10.74674821418697057, 0.7998128361456462443 ) ) ;
#137928 = DIRECTION ( 'NONE',  ( -0.9998757926790047268, 0.01538962834599434497, -0.003399787332182534986 ) ) ;
#137929 = CARTESIAN_POINT ( 'NONE',  ( 3.344746749068757019, -2.138148195731132351, -0.3758941404270431108 ) ) ;
#137930 = FACE_OUTER_BOUND ( 'NONE', #97484, .T. ) ;
#137931 = CARTESIAN_POINT ( 'NONE',  ( 1.037531286769650452, -0.04638328994046451298, 2.120250110247793085 ) ) ;
#137932 = CARTESIAN_POINT ( 'NONE',  ( -1.402160292154681736E-14, 1.118750000682820378, -1.732050807568863648 ) ) ;
#137933 = CARTESIAN_POINT ( 'NONE',  ( 8.543609354905870035, 13.11929468069890525, 0.7998128361456462443 ) ) ;
#137934 =( LENGTH_UNIT ( ) NAMED_UNIT ( * ) SI_UNIT ( .MILLI., .METRE. ) );
#137935 = CARTESIAN_POINT ( 'NONE',  ( 6.013528089337225602, 7.174620582783560963, 1.187335689305318853 ) ) ;
#137936 =( GEOMETRIC_REPRESENTATION_CONTEXT ( 3 ) GLOBAL_UNCERTAINTY_ASSIGNED_CONTEXT ( ( #14754 ) ) GLOBAL_UNIT_ASSIGNED_CONTEXT ( ( #46865, #63088, #112978 ) ) REPRESENTATION_CONTEXT ( 'NONE', 'WORKASPACE' ) );
#137937 = CARTESIAN_POINT ( 'NONE',  ( 1.335309304440901235, -1.864295028495915441, 0.8784465167368092908 ) ) ;
#137939 = CARTESIAN_POINT ( 'NONE',  ( -5.692136587293078698, 5.855332880448203881, -2.499999999999996003 ) ) ;
#137938 = CARTESIAN_POINT ( 'NONE',  ( -7.967387826325084355, 12.44703623068796361, 0.7998128361456481317 ) ) ;
#137940 = CARTESIAN_POINT ( 'NONE',  ( 1.364683531249986537, 0.9052083336747533959, -0.7879004041258239610 ) ) ;
#137941 = SURFACE_SIDE_STYLE ('',( #54543 ) ) ;
#137942 = VERTEX_POINT ( 'NONE', #79715 ) ;
#137943 = CARTESIAN_POINT ( 'NONE',  ( 3.141163725242692273, 0.04933110545866059571, 1.911816780882446221 ) ) ;
#137944 = CARTESIAN_POINT ( 'NONE',  ( 5.787929806067755756, -0.7924508370336593721, 1.582612139130882278 ) ) ;
#137945 = CARTESIAN_POINT ( 'NONE',  ( 5.688527969385528849, 8.794310509995222347, -1.199719254218452047 ) ) ;
#137946 = CARTESIAN_POINT ( 'NONE',  ( -3.242371291962510504, 6.934516940598226320, 1.040834085586084257E-14 ) ) ;
#137947 = CARTESIAN_POINT ( 'NONE',  ( 0.4920785707626255112, -1.005892833030905598, 1.506422592618541278 ) ) ;
#137949 = CARTESIAN_POINT ( 'NONE',  ( 0.5146670378583360073, 0.1438656263933698054, 1.910404373559170477 ) ) ;
#137948 = CARTESIAN_POINT ( 'NONE',  ( -6.662118508819848905, -7.185026885899485016, 6.772457744868685126 ) ) ;
#137950 = AXIS2_PLACEMENT_3D ( 'NONE', #153930, #103043, #70503 ) ;
#137951 = CARTESIAN_POINT ( 'NONE',  ( 1.908725956546155178, 0.6474277305483535638, 1.966616875269424192 ) ) ;
#137952 = CARTESIAN_POINT ( 'NONE',  ( -1.402160292154681736E-14, -0.3656249996585805295, 1.575800808251672791 ) ) ;
#137953 = CARTESIAN_POINT ( 'NONE',  ( 6.543822781336226413, 0.7137633992815132222, -1.729328153040734506 ) ) ;
#137954 = CARTESIAN_POINT ( 'NONE',  ( 2.807047293222181494, 1.542382716246639474, 0.9765254425028799812 ) ) ;
#137956 = CARTESIAN_POINT ( 'NONE',  ( 5.871284023695358734, 7.173991544917035945, 1.145568358895364458 ) ) ;
#137955 = CARTESIAN_POINT ( 'NONE',  ( -0.02224634325198419221, -0.007204097619508199532, -2.289079630542793620 ) ) ;
#137957 = CARTESIAN_POINT ( 'NONE',  ( 0.6823417656249882723, 0.09270833367475139752, 1.181850606188755259 ) ) ;
#137958 = CARTESIAN_POINT ( 'NONE',  ( 3.754389245258652252, -2.060177385294372776, -0.1042076536686628307 ) ) ;
#137959 = CARTESIAN_POINT ( 'NONE',  ( -6.911959384868566758, 6.958374125301778790, 1.040834085586084257E-14 ) ) ;
#137960 = CARTESIAN_POINT ( 'NONE',  ( 7.242026607993941489, 11.60078147596829901, 0.7998128361456462443 ) ) ;
#137961 = CARTESIAN_POINT ( 'NONE',  ( 3.357615597678655917, 7.068968630600413583, 0.7998128361456321445 ) ) ;
#137962 = CARTESIAN_POINT ( 'NONE',  ( 0.5269342146079664113, 2.068330297753611546, 0.6279826202375409228 ) ) ;
#137963 = CARTESIAN_POINT ( 'NONE',  ( 0.1511277727459575393, -0.4806850054440474085, -2.125521221522770787 ) ) ;
#137964 = CARTESIAN_POINT ( 'NONE',  ( 1.364683531249988535, 1.926041667008086211, 0.7879004041258500513 ) ) ;
#137965 = CARTESIAN_POINT ( 'NONE',  ( 4.130267194010744269, 1.160198474277823300, -1.823679694223250491 ) ) ;
#137966 = CARTESIAN_POINT ( 'NONE',  ( 3.914717006531149401, -0.6357662484684013515, -1.917053231858157236 ) ) ;
#137967 = PRESENTATION_STYLE_ASSIGNMENT (( #19920 ) ) ;
#137968 = EDGE_CURVE ( 'NONE', #137099, #206526, #82012, .T. ) ;
#137971 = CARTESIAN_POINT ( 'NONE',  ( 5.666945020832160118, 9.555260257705446847, 0.7216878364870438212 ) ) ;
#137970 = CARTESIAN_POINT ( 'NONE',  ( -1.642778471874998480, -2.851041666188706802, 2.845375778867863303 ) ) ;
#137969 = DIRECTION ( 'NONE',  ( -3.330669073875478989E-16, 3.330669073875478989E-16, 1.000000000000000000 ) ) ;
#137972 = CARTESIAN_POINT ( 'NONE',  ( -4.308458954092677651, 8.248562223075252220, -0.7998128361456362523 ) ) ;
#137973 = CARTESIAN_POINT ( 'NONE',  ( 2.202361591730035428, 1.313542931311746598, -1.530159205979222170 ) ) ;
#137974 = CARTESIAN_POINT ( 'NONE',  ( -7.823218330285243383, 9.085841792542966644, -1.199719254218446718 ) ) ;
#137976 = CARTESIAN_POINT ( 'NONE',  ( -10.99970480906932302, -5.741816521215535651, -0.08058606168007156900 ) ) ;
#137975 = CARTESIAN_POINT ( 'NONE',  ( -4.874319919312905647, 5.645460313075203018, -1.199719254218446718 ) ) ;
#137977 = DIRECTION ( 'NONE',  ( 0.000000000000000000, 0.000000000000000000, -1.000000000000000000 ) ) ;
#137978 = CARTESIAN_POINT ( 'NONE',  ( 5.326388512780113160, -0.8654452107222168067, -1.705464787417856787 ) ) ;
#137979 = DIRECTION ( 'NONE',  ( 4.440892098500630106E-16, 3.330669073875473073E-16, 1.000000000000000000 ) ) ;
#137980 = EDGE_CURVE ( 'NONE', #213748, #40754, #61307, .T. ) ;
#137981 = CARTESIAN_POINT ( 'NONE',  ( 5.517805330637495231, 6.500156309574290248, -1.082531754730543083 ) ) ;
#137983 = CARTESIAN_POINT ( 'NONE',  ( 3.972279928656559100, -1.994873972748755442, -0.2930500606010341125 ) ) ;
#137982 = CARTESIAN_POINT ( 'NONE',  ( -8.825994812371996900, 9.399341490629888440, 0.7216878364870438212 ) ) ;
#137984 = CARTESIAN_POINT ( 'NONE',  ( 1.499999999999990896, 4.275000000000021672, 1.214306433183764966E-14 ) ) ;
#137985 = CARTESIAN_POINT ( 'NONE',  ( 0.6823417656249934904, 14.50520833367473195, 1.181850606188764807 ) ) ;
#137986 = CARTESIAN_POINT ( 'NONE',  ( 6.387718858896353602, 1.193691027695796825, 1.245227284122518485 ) ) ;
#137987 = CARTESIAN_POINT ( 'NONE',  ( 6.723917837734620484, 6.809268663637336516, 0.000000000000000000 ) ) ;
#137988 = CARTESIAN_POINT ( 'NONE',  ( 9.246297574839980271, 10.85006392781057905, 1.082531754730549967 ) ) ;
#137989 = CARTESIAN_POINT ( 'NONE',  ( 10.99943592164173012, -9.900000000000019895, -0.1113975120799794716 ) ) ;
#137990 = CARTESIAN_POINT ( 'NONE',  ( 5.553920895479774522, 1.868435625992425742, -0.09091641586010666687 ) ) ;
#137991 = CARTESIAN_POINT ( 'NONE',  ( 5.941657920834610529, -1.894198565178412119, 0.6822040374353780523 ) ) ;
#137992 = CARTESIAN_POINT ( 'NONE',  ( -0.1290005225502675879, -0.006633637972621592160, -2.173875058097324064 ) ) ;
#137993 = CARTESIAN_POINT ( 'NONE',  ( 2.026315959858393967, 1.060668813445601044, 1.777738962378045295 ) ) ;
#137994 = CIRCLE ( 'NONE', #134612, 2.750000000000000000 ) ;
#137995 = CARTESIAN_POINT ( 'NONE',  ( -6.238160075619175515, 10.29195416494877513, 0.000000000000000000 ) ) ;
#137996 = EDGE_LOOP ( 'NONE', ( #61693, #125463, #67632, #116645 ) ) ;
#137997 = CARTESIAN_POINT ( 'NONE',  ( 1.124625310196948558, 0.3961260723950796314, 1.976952190469769111 ) ) ;
#137998 = CARTESIAN_POINT ( 'NONE',  ( 1.230386416485089729, 1.215489027575139769, -1.343484786563201805 ) ) ;
#137999 = CARTESIAN_POINT ( 'NONE',  ( 4.055297343818931033, 6.784911763547157193, 1.082531754730549078 ) ) ;
#138000 = CARTESIAN_POINT ( 'NONE',  ( -0.008173644115966258172, -6.287979527546275982, -10.90726532705803820 ) ) ;
#138001 = CARTESIAN_POINT ( 'NONE',  ( 8.731087737076324018, 9.288616569451617622, 1.040834085586084257E-14 ) ) ;
#138002 = CARTESIAN_POINT ( 'NONE',  ( 7.564559641420864899, 10.91273778404466199, -1.199719254218446718 ) ) ;
#138004 = CARTESIAN_POINT ( 'NONE',  ( 6.134394303309665730, 0.6061128391178214336, 1.817247008912269646 ) ) ;
#138003 = CARTESIAN_POINT ( 'NONE',  ( -6.555530967407501741, 7.606873202518897870, 1.199719254218450271 ) ) ;
#138005 = AXIS2_PLACEMENT_3D ( 'NONE', #187872, #166303, #39500 ) ;
#138006 = CARTESIAN_POINT ( 'NONE',  ( -11.52901446936762575, 13.79425527467597234, 3.330874149801142270 ) ) ;
#138007 = CARTESIAN_POINT ( 'NONE',  ( -3.565431210269620621, 7.103494145382398095, 0.7216878364870484841 ) ) ;
#138008 = ADVANCED_FACE ( 'NONE', ( #211836 ), #15748, .T. ) ;
#138009 = CARTESIAN_POINT ( 'NONE',  ( -10.99970480893081870, -6.134628647623513231, -0.08058608058607828750 ) ) ;
#138011 = VERTEX_POINT ( 'NONE', #113364 ) ;
#138010 = CARTESIAN_POINT ( 'NONE',  ( 5.178851490740207453, 5.144340948726102702, 0.7216878364870317197 ) ) ;
#138012 = CARTESIAN_POINT ( 'NONE',  ( -8.351459436338041442, 9.806086099558291025, -1.082531754730543971 ) ) ;
#138013 = CARTESIAN_POINT ( 'NONE',  ( 3.344745324850742385, 0.5235245934552492653, 2.097234944377385002 ) ) ;
#138014 = CARTESIAN_POINT ( 'NONE',  ( -3.902768115887413014, 5.646591783325653147, -1.599625672291283607 ) ) ;
#138015 = CARTESIAN_POINT ( 'NONE',  ( 6.861835142292143530, 8.138467433163244280, 1.082531754730549967 ) ) ;
#138016 = CARTESIAN_POINT ( 'NONE',  ( 0.3871773095200456982, -1.998849835692744659, -0.7086421328065874992 ) ) ;
#138017 = CARTESIAN_POINT ( 'NONE',  ( 6.247073575888860475, -1.540555741078741825, 0.9791950884799265342 ) ) ;
#138018 = CARTESIAN_POINT ( 'NONE',  ( 2.565645918639497314, 1.934049084626581205, -0.3809019065194594877 ) ) ;
#138019 = CARTESIAN_POINT ( 'NONE',  ( 4.834190613173367623, -1.027981871586785889, -1.612434056610718480 ) ) ;
#138020 = ORIENTED_EDGE ( 'NONE', *, *, #48333, .F. ) ;
#138021 = DIRECTION ( 'NONE',  ( 1.014813233446432150E-15, 1.000000000000000000, -4.583713267641621330E-32 ) ) ;
#138022 = CARTESIAN_POINT ( 'NONE',  ( 4.439879492920996817, 1.284938098365424164, 1.492779756951348125 ) ) ;
#138023 = CARTESIAN_POINT ( 'NONE',  ( 0.6033350840282033500, -1.932664299774440098, 0.1897328419256556487 ) ) ;
#138024 = EDGE_LOOP ( 'NONE', ( #197676, #13326, #4765, #173348 ) ) ;
#138025 = CARTESIAN_POINT ( 'NONE',  ( -6.459533842268148973, 6.500820668926428958, 0.000000000000000000 ) ) ;
#138027 = CARTESIAN_POINT ( 'NONE',  ( -0.3782569160207209791, 3.049340702855438234, 0.4285286083245324895 ) ) ;
#138026 = CARTESIAN_POINT ( 'NONE',  ( -4.228163802615396705, 6.026220084508304708, -1.599625672291271394 ) ) ;
#138029 = CARTESIAN_POINT ( 'NONE',  ( 6.089020385868848528, 8.197219431637373432, -1.443375672974078761 ) ) ;
#138028 = CARTESIAN_POINT ( 'NONE',  ( 8.308449207076147758, 8.587612251210650527, -0.7998128361456281477 ) ) ;
#138031 = ORIENTED_EDGE ( 'NONE', *, *, #26674, .F. ) ;
#138030 = CARTESIAN_POINT ( 'NONE',  ( 5.496708366351358066, -1.866603419165157041, -0.4147590543357379533 ) ) ;
#138032 = CARTESIAN_POINT ( 'NONE',  ( 1.026743138268666922, 1.313310656681260680, -1.773271738842125300 ) ) ;
#138033 = AXIS2_PLACEMENT_3D ( 'NONE', #179682, #31302, #196982 ) ;
#138034 = CARTESIAN_POINT ( 'NONE',  ( 9.367496997597593023, 3.481540744127370690, -7.500000000000005329 ) ) ;
#138035 = CARTESIAN_POINT ( 'NONE',  ( 5.813144886445268611, 1.644464822582414332, -1.160890557811714352 ) ) ;
#138036 = CARTESIAN_POINT ( 'NONE',  ( -0.02319159430949970999, 0.003959926571647092407, -1.810968101872318714 ) ) ;
#138037 = FACE_OUTER_BOUND ( 'NONE', #202103, .T. ) ;
#138038 = CARTESIAN_POINT ( 'NONE',  ( 6.875062624577638282, -8.049367966558001797, -6.605500049835221432 ) ) ;
#138039 = CARTESIAN_POINT ( 'NONE',  ( 3.314952806421948672, -1.569539724514938950, 1.350292352848787569 ) ) ;
#138040 = CARTESIAN_POINT ( 'NONE',  ( -6.911959384868566758, 6.958374125301778790, 1.040834085586084257E-14 ) ) ;
#138041 = CARTESIAN_POINT ( 'NONE',  ( -4.784432227305938312, 8.165582598138012571, -0.7895561949947740299 ) ) ;
#138043 = CARTESIAN_POINT ( 'NONE',  ( 0.1456854043008250221, -1.672057201651616642, -1.369741535119282982 ) ) ;
#138042 = CARTESIAN_POINT ( 'NONE',  ( -5.901876940650454095, 5.779944607047298177, -0.7998128361456291469 ) ) ;
#138044 = CARTESIAN_POINT ( 'NONE',  ( -10.89798411099869035, 6.655715830334343330, 5.027853787196250757 ) ) ;
#138045 = CARTESIAN_POINT ( 'NONE',  ( 4.204437034013637664, 6.958908068774287692, -1.082531754730548412 ) ) ;
#138046 = CARTESIAN_POINT ( 'NONE',  ( 0.2633404184768576850, -6.747343053191802831, 9.488968570712993156 ) ) ;
#138047 = CARTESIAN_POINT ( 'NONE',  ( -1.364683531250010295, 13.19270833367472839, 0.7879004041258445001 ) ) ;
#138049 = CARTESIAN_POINT ( 'NONE',  ( -6.089547271193396227, 7.133501900260939443, -1.199719254218453823 ) ) ;
#138048 = CARTESIAN_POINT ( 'NONE',  ( 6.925078400183550364, 2.474256779287649088, 2.140290375984225335 ) ) ;
#138050 = CIRCLE ( 'NONE', #186426, 0.08000000000000014044 ) ;
#138051 = CARTESIAN_POINT ( 'NONE',  ( 5.309090426574582189, 1.026673973311197585, -1.397408945856312590 ) ) ;
#138052 = CARTESIAN_POINT ( 'NONE',  ( -2.279742385392243165, 5.811449882932888222, -0.7998128361456281477 ) ) ;
#138053 = CARTESIAN_POINT ( 'NONE',  ( 2.342711862795249012, -2.029470198211943632, -0.4080651701656515251 ) ) ;
#138054 = CARTESIAN_POINT ( 'NONE',  ( 4.025106843427800563, -1.841118617500647314, 1.045351873429276601 ) ) ;
#138055 = CARTESIAN_POINT ( 'NONE',  ( 8.111855979677986994, 8.358253485912799263, 1.040834085586084257E-14 ) ) ;
#138056 = CARTESIAN_POINT ( 'NONE',  ( 0.3978093821460517154, 3.011896635411783762, 0.3978093821460513824 ) ) ;
#138057 = CARTESIAN_POINT ( 'NONE',  ( 2.289847402107755947, -1.282740503449712577, -1.494545344566786449 ) ) ;
#138058 = CARTESIAN_POINT ( 'NONE',  ( 6.115167699822185554, 6.015585554489271125, 0.01814796302670486361 ) ) ;
#138059 = CARTESIAN_POINT ( 'NONE',  ( 1.318461241437279607, -0.6911404020932455650, -1.783297644634279200 ) ) ;
#138060 = CARTESIAN_POINT ( 'NONE',  ( 4.822401350889861327, 2.192639013963990635, 0.6684651760814497301 ) ) ;
#138061 = CARTESIAN_POINT ( 'NONE',  ( 1.646812808029130215, -1.543121136568927243, 0.9753659028155501343 ) ) ;
#138062 = CARTESIAN_POINT ( 'NONE',  ( 4.797606254389322089, 6.690569611577942943, 1.599625672291268286 ) ) ;
#138063 = CARTESIAN_POINT ( 'NONE',  ( 4.650083499362856365, 8.368921815991249957, 0.7216878364870438212 ) ) ;
#138064 = CARTESIAN_POINT ( 'NONE',  ( -6.170932472514347289, 10.35117165124207972, 0.000000000000000000 ) ) ;
#138065 = CARTESIAN_POINT ( 'NONE',  ( 3.392840988816598902, -1.941408766427907384, -0.5327130583171105771 ) ) ;
#138066 = CARTESIAN_POINT ( 'NONE',  ( 3.098438489093110704, 1.946378968836332213, 0.2448508753878294586 ) ) ;
#138067 = CARTESIAN_POINT ( 'NONE',  ( -7.832860060393135093, 10.16142270859057462, 1.599625672291295375 ) ) ;
#138068 = CARTESIAN_POINT ( 'NONE',  ( -6.033542053281340856, 6.997886136038390603, -1.199719254218446718 ) ) ;
#138069 = CARTESIAN_POINT ( 'NONE',  ( -1.292658234375014592, 2.960937500170686576, -3.295974604355933479E-14 ) ) ;
#138071 = CARTESIAN_POINT ( 'NONE',  ( 4.276060399186999206, -1.018433877553532207, 1.447237009025013732 ) ) ;
#138070 = CARTESIAN_POINT ( 'NONE',  ( 5.701146808890831252, -0.5089937999912234057, 2.027600676370949095 ) ) ;
#138072 = CARTESIAN_POINT ( 'NONE',  ( -2.398572866711294438, 5.287202466803544887, -0.8077998227820496480 ) ) ;
#138073 = CARTESIAN_POINT ( 'NONE',  ( 0.9025786099917804117, 1.657183926254527595, -1.434042119274607563 ) ) ;
#138074 = CARTESIAN_POINT ( 'NONE',  ( 0.06344835015564037617, -1.139564578658038618, 1.315610641012928239 ) ) ;
#138075 = CARTESIAN_POINT ( 'NONE',  ( 7.800018446563675489, 7.994443030612759848, -0.7998128361456281477 ) ) ;
#138076 = CARTESIAN_POINT ( 'NONE',  ( 0.1331715793776574175, 0.2412765091673596263, -1.987739918565622821 ) ) ;
#138077 = CARTESIAN_POINT ( 'NONE',  ( 0.2284049197783468987, -2.054502581980635956, -1.030649272238814085 ) ) ;
#138078 = DIRECTION ( 'NONE',  ( 0.000000000000000000, 1.000000000000000000, 0.000000000000000000 ) ) ;
#138079 = CARTESIAN_POINT ( 'NONE',  ( 5.483642203991152542, 1.602890455293109584, 0.6615300989148454880 ) ) ;
#138080 = CARTESIAN_POINT ( 'NONE',  ( 2.174722684859807575, -1.356406721008751814, 1.740749382485320407 ) ) ;
#138081 = CARTESIAN_POINT ( 'NONE',  ( 0.4972420419220639487, 0.3698279840313797862, 2.139175918340649574 ) ) ;
#138082 = DIRECTION ( 'NONE',  ( 6.314299915563594049E-62, 8.546850786086437571E-32, 1.000000000000000000 ) ) ;
#138083 = CARTESIAN_POINT ( 'NONE',  ( 1.358780451569325365, -2.012465911620679115, -0.6584304486853159721 ) ) ;
#138084 = CARTESIAN_POINT ( 'NONE',  ( 3.218750000000001776, -0.7852924748298164559, 1.895863743164153847 ) ) ;
#138085 = CARTESIAN_POINT ( 'NONE',  ( 6.827182134110235445, 0.5726250382554041174, 2.141766166723162002 ) ) ;
#138086 = CARTESIAN_POINT ( 'NONE',  ( 4.524389607583827910, 1.185449959155547850, -1.518358881950541139 ) ) ;
#138087 = CARTESIAN_POINT ( 'NONE',  ( 1.313460851834074905, 1.813262283420258525, -1.282816764689881373 ) ) ;
#138088 = ORIENTED_EDGE ( 'NONE', *, *, #65889, .T. ) ;
#138089 =( GEOMETRIC_REPRESENTATION_CONTEXT ( 3 ) GLOBAL_UNCERTAINTY_ASSIGNED_CONTEXT ( ( #97117 ) ) GLOBAL_UNIT_ASSIGNED_CONTEXT ( ( #74601, #38899, #140705 ) ) REPRESENTATION_CONTEXT ( 'NONE', 'WORKASPACE' ) );
#138091 = CARTESIAN_POINT ( 'NONE',  ( -1.001543065824772872E-14, 4.962500000000019007, 1.732050807568877637 ) ) ;
#138090 = CARTESIAN_POINT ( 'NONE',  ( 1.892491709730130145, -0.6158747592755541289, -2.208019654398277520 ) ) ;
#138092 = CARTESIAN_POINT ( 'NONE',  ( 3.310162060030825248, 7.013606170011280838, -0.7998128361456291469 ) ) ;
#138093 = CARTESIAN_POINT ( 'NONE',  ( 6.667912619822566000, 6.673652899414787676, 1.040834085586084257E-14 ) ) ;
#138094 = CARTESIAN_POINT ( 'NONE',  ( 3.598459204466686323, -1.093923138158871433, 1.933176262723006467 ) ) ;
#138095 = CARTESIAN_POINT ( 'NONE',  ( -7.049876689426097798, 11.16868053773170821, -0.7216878364870267237 ) ) ;
#138098 = EDGE_CURVE ( 'NONE', #140828, #62036, #80795, .T. ) ;
#138097 =( NAMED_UNIT ( * ) SI_UNIT ( $, .STERADIAN. ) SOLID_ANGLE_UNIT ( ) );
#138096 = COLOUR_RGB ( '', 0.31764706, 0.68627451, 0.89019608) ;
#138099 = CARTESIAN_POINT ( 'NONE',  ( 6.263503779833467178, 9.290876262238963790, -1.082531754730537088 ) ) ;
#138100 = CARTESIAN_POINT ( 'NONE',  ( -9.802181872555943087, 10.53822639417784046, 0.7216878364870438212 ) ) ;
#138101 = CARTESIAN_POINT ( 'NONE',  ( 5.872089928494542477, 9.864872326636710653, 0.000000000000000000 ) ) ;
#138102 = ORIENTED_EDGE ( 'NONE', *, *, #140329, .T. ) ;
#138103 = CARTESIAN_POINT ( 'NONE',  ( 1.406875202279284753, -1.122500148236497575, -1.674886495921081631 ) ) ;
#138105 = CARTESIAN_POINT ( 'NONE',  ( 6.408646180098039657, 0.6432782940990633413, 1.959889192978042205 ) ) ;
#138104 = CARTESIAN_POINT ( 'NONE',  ( 7.052212457402625922, 11.37933163361175382, -0.7998128361456291469 ) ) ;
#138106 = CARTESIAN_POINT ( 'NONE',  ( 5.953438849732186178, 8.999410187112612647, -1.082531754730548412 ) ) ;
#138107 = CARTESIAN_POINT ( 'NONE',  ( 0.1691535571452691677, 1.059206136818511501, 1.505872603892892458 ) ) ;
#138108 = CARTESIAN_POINT ( 'NONE',  ( -9.367496997601300279, 15.00000000000599165, -7.679999999987998649 ) ) ;
#138109 = CARTESIAN_POINT ( 'NONE',  ( -1.364683531250014514, 1.988541667008086655, -0.7879004041258289570 ) ) ;
#138110 = CARTESIAN_POINT ( 'NONE',  ( 1.686396851806533315, -0.2532433360125495025, -1.751381468886082038 ) ) ;
#138111 = CARTESIAN_POINT ( 'NONE',  ( 6.451818256879360725, -1.589883334587833152, -0.6930036952102114345 ) ) ;
#138112 = CARTESIAN_POINT ( 'NONE',  ( 6.620655732516682157, 0.01042156863441953685, 1.726407961933309476 ) ) ;
#138113 = CARTESIAN_POINT ( 'NONE',  ( 4.704755546018094314, 1.993839351151542427, 1.131020188671335136 ) ) ;
#138114 = CARTESIAN_POINT ( 'NONE',  ( 3.222423357234117436, 0.04607595322191247733, 1.840729346561786661 ) ) ;
#138115 = ADVANCED_FACE ( 'NONE', ( #53607 ), #95273, .F. ) ;
#138116 = CARTESIAN_POINT ( 'NONE',  ( 9.108380270282433244, 9.520865158284665952, 1.040834085586084257E-14 ) ) ;
#138117 =( NAMED_UNIT ( * ) PLANE_ANGLE_UNIT ( ) SI_UNIT ( $, .RADIAN. ) );
#138118 = CARTESIAN_POINT ( 'NONE',  ( 4.506759567000420574, 1.410888988908312047, -1.158519065656477220 ) ) ;
#138119 = CARTESIAN_POINT ( 'NONE',  ( 3.287732575140737801, 1.587837554856496691, -1.242726844152845178 ) ) ;
#138120 = CARTESIAN_POINT ( 'NONE',  ( -9.450196763925152510, 10.98398329845622001, -1.199719254218441611 ) ) ;
#138122 = CARTESIAN_POINT ( 'NONE',  ( -6.084577077482911101, 10.32070003369722144, 0.000000000000000000 ) ) ;
#138121 = CARTESIAN_POINT ( 'NONE',  ( 3.713984175222109663, -2.229511888261398678, 0.3841874803040145059 ) ) ;
#138123 = CARTESIAN_POINT ( 'NONE',  ( 5.631892205062830392, -1.333580992396019571, -1.629923671128389762 ) ) ;
#138124 = CARTESIAN_POINT ( 'NONE',  ( -11.92045683181315674, 13.65275927879484819, -1.382340670101859237 ) ) ;
#138125 = CARTESIAN_POINT ( 'NONE',  ( 3.736834853878097107, -1.994506513866915576, -0.5549897870569252545 ) ) ;
#138126 = CARTESIAN_POINT ( 'NONE',  ( 4.241003122976366058, 3.842258486427521103, -0.7998128361456211532 ) ) ;
#138127 = CARTESIAN_POINT ( 'NONE',  ( 1.360316468749987129, 1.796875000341410900, -3.295974604355933479E-14 ) ) ;
#138128 = CARTESIAN_POINT ( 'NONE',  ( 5.338584462458719315, 1.262900380722062454, -1.703257760751579530 ) ) ;
#138130 = CARTESIAN_POINT ( 'NONE',  ( 0.6977243349758615043, -0.6943943954660827256, 1.797178231592330588 ) ) ;
#138129 = CARTESIAN_POINT ( 'NONE',  ( -9.341731535015849630, 10.85744053139533349, 1.199719254218462483 ) ) ;
#138131 = CARTESIAN_POINT ( 'NONE',  ( -4.462568837553487100, 5.235360394347691404, -1.199719254218453823 ) ) ;
#138132 = CARTESIAN_POINT ( 'NONE',  ( 0.4495734683114894215, 1.456899865409568617, 1.325532655419828787 ) ) ;
#138133 = CARTESIAN_POINT ( 'NONE',  ( 4.597623488365603528, 5.496887170248887067, -1.082531754730548412 ) ) ;
#138134 = CARTESIAN_POINT ( 'NONE',  ( 5.880650534977156063, 5.984130091214588276, -0.1889179825720621597 ) ) ;
#138135 = FACE_OUTER_BOUND ( 'NONE', #77088, .T. ) ;
#138136 = CARTESIAN_POINT ( 'NONE',  ( -3.255929445576174697, 6.950334786480840243, -0.7998128361456281477 ) ) ;
#138137 = CARTESIAN_POINT ( 'NONE',  ( 1.072868727471010253, 0.9067168766181363804, 2.028134479351159314 ) ) ;
#138138 = CARTESIAN_POINT ( 'NONE',  ( 2.731583703245387351, -1.965451047913500116, 0.7568412939000405126 ) ) ;
#138139 = CARTESIAN_POINT ( 'NONE',  ( -2.979759899953417612, 6.698413326579433225, 0.7998128361456352531 ) ) ;
#138140 = CARTESIAN_POINT ( 'NONE',  ( 8.372323551638698902, 9.726464550788689323, 1.199719254218462483 ) ) ;
#138141 = CARTESIAN_POINT ( 'NONE',  ( 0.5548465212725885998, 1.550470960922016861, -1.029025501433494583 ) ) ;
#138142 = CARTESIAN_POINT ( 'NONE',  ( 7.311924916471702396, 7.425000578838787391, -0.7998128361456281477 ) ) ;
#138143 = CARTESIAN_POINT ( 'NONE',  ( -1.499999999999997780, 8.627523663848661428, -2.579999999999990301 ) ) ;
#138144 = CARTESIAN_POINT ( 'NONE',  ( -6.129694847154220305, 8.244672969803623630, -1.443375672974066548 ) ) ;
#138145 = CARTESIAN_POINT ( 'NONE',  ( -7.673551755654729689, 11.89630144833179060, 0.7216878364870458196 ) ) ;
#138147 = CARTESIAN_POINT ( 'NONE',  ( 1.301209403646291118, -0.3165094942152619772, -2.096747597609450953 ) ) ;
#138146 = STYLED_ITEM ( 'NONE', ( #12852 ), #37156 ) ;
#138148 = CARTESIAN_POINT ( 'NONE',  ( -6.424584688029276514, 8.588711117491191871, 1.599625672291269396 ) ) ;
#138150 = CARTESIAN_POINT ( 'NONE',  ( 3.736726379466179804, -1.890069333072645241, -0.5255722985574098338 ) ) ;
#138149 = CARTESIAN_POINT ( 'NONE',  ( 1.225000000000010747, 0.3749999999999864553, -2.081668171172168513E-14 ) ) ;
#138151 = CARTESIAN_POINT ( 'NONE',  ( 2.307699607974790901, -0.4742087202370263155, 2.108885336910087283 ) ) ;
#138152 = CARTESIAN_POINT ( 'NONE',  ( 1.874305484616908934, -0.09156810461483089192, -1.839108553062768214 ) ) ;
#138154 = CARTESIAN_POINT ( 'NONE',  ( -6.025499844618653178, 6.066343344509915525, -0.6079853925319089747 ) ) ;
#138153 = CARTESIAN_POINT ( 'NONE',  ( -6.147696309153835692, 6.137010213626392208, 0.7998128361456281477 ) ) ;
#138155 = ADVANCED_FACE ( 'NONE', ( #198766 ), #119584, .T. ) ;
#138156 = CARTESIAN_POINT ( 'NONE',  ( 3.187183321348503018, -0.7043554338151243321, 1.591608241653941214 ) ) ;
#138157 = CARTESIAN_POINT ( 'NONE',  ( 5.395781948558860286, 6.357795697149212444, -1.082531754730542195 ) ) ;
#138158 = CARTESIAN_POINT ( 'NONE',  ( -12.04410816989902955, 7.377574010548016759, -3.959763750030863783 ) ) ;
#138159 = CARTESIAN_POINT ( 'NONE',  ( 0.5148121308554790554, 1.489681748880047563, -1.566682057046255849 ) ) ;
#138160 = CARTESIAN_POINT ( 'NONE',  ( 3.866564406427867251, -0.5879305547937460075, 1.928456347981069019 ) ) ;
#138161 = CARTESIAN_POINT ( 'NONE',  ( 4.650083499807233345, 5.295740330745369207, -7.499999999999997335 ) ) ;
#138162 = CARTESIAN_POINT ( 'NONE',  ( 0.4444780689869810564, 2.156031605563761833, 0.1575401717312311101 ) ) ;
#138163 = CARTESIAN_POINT ( 'NONE',  ( 1.991034414115494089, 1.716142376821601534, -0.9701854037313780710 ) ) ;
#138164 = ADVANCED_FACE ( 'NONE', ( #165227 ), #112143, .T. ) ;
#138165 = CARTESIAN_POINT ( 'NONE',  ( 6.509000000000034980, 7.629137130509102249, 2.499999999999994227 ) ) ;
#138166 = CARTESIAN_POINT ( 'NONE',  ( 2.419391519165543070, -1.120004824200554916, -1.586377984052749879 ) ) ;
#138168 = ORIENTED_EDGE ( 'NONE', *, *, #104484, .F. ) ;
#138167 = CARTESIAN_POINT ( 'NONE',  ( -5.655159470675923394, 5.770309935309573923, 0.000000000000000000 ) ) ;
#138169 = CARTESIAN_POINT ( 'NONE',  ( -3.621436428181653788, 7.239109909604962922, 0.7216878364870338292 ) ) ;
#138170 = CARTESIAN_POINT ( 'NONE',  ( 5.224688093219824303, 7.188831756880171397, -1.599625672291283607 ) ) ;
#138171 = CARTESIAN_POINT ( 'NONE',  ( -4.793689830883590020, 7.750332681742931662, 1.199719254218452935 ) ) ;
#138172 = CARTESIAN_POINT ( 'NONE',  ( -6.957269102468015554, 8.145844036748005834, 1.199719254218452047 ) ) ;
#138173 = CARTESIAN_POINT ( 'NONE',  ( -1.264911064067355984, 3.850000000000006306, -0.5000000000000004441 ) ) ;
#138174 = CARTESIAN_POINT ( 'NONE',  ( 6.387736634265912983, 1.584785628913528699, 1.677562689604541468 ) ) ;
#138175 = CARTESIAN_POINT ( 'NONE',  ( 6.830524215763060347, -1.208013408316032322, 1.546442907991877558 ) ) ;
#138176 = CARTESIAN_POINT ( 'NONE',  ( 3.731260466781026963, 0.05263058604075031982, -1.961233346245725429 ) ) ;
#138177 = CARTESIAN_POINT ( 'NONE',  ( 8.392660782059197189, 9.750191319612612872, 1.199719254218462483 ) ) ;
#138178 = CARTESIAN_POINT ( 'NONE',  ( 1.600232647554021392, -0.2440283035436350279, 2.001511509883910911 ) ) ;
#138179 = ORIENTED_EDGE ( 'NONE', *, *, #97346, .T. ) ;
#138180 = CARTESIAN_POINT ( 'NONE',  ( 1.868513053102664356, -2.077584836267523105, -0.4075993926472165074 ) ) ;
#138181 = CARTESIAN_POINT ( 'NONE',  ( 1.499999999999987121, 1.077083334016148308, -0.8660254037844253849 ) ) ;
#138183 = CARTESIAN_POINT ( 'NONE',  ( -5.506582945444718824, 9.576097202994168001, 0.7998128361456481317 ) ) ;
#138182 = CARTESIAN_POINT ( 'NONE',  ( -10.00050683067322765, 3.975933801733735340, 5.773795310721945739 ) ) ;
#138184 = CARTESIAN_POINT ( 'NONE',  ( 3.152128525617302834, -1.393660036906883226, 1.203213496783587910 ) ) ;
#138185 = ORIENTED_EDGE ( 'NONE', *, *, #124333, .F. ) ;
#138186 = B_SPLINE_CURVE_WITH_KNOTS ( 'NONE', 3,
 ( #45228, #157910, #75577, #207699 ),
 .UNSPECIFIED., .F., .F.,
 ( 4, 4 ),
 ( 0.000000000000000000, 0.0001873600508426472261 ),
 .UNSPECIFIED. ) ;
#138187 = CARTESIAN_POINT ( 'NONE',  ( -8.448702279610222021, 13.00856975952063088, 1.040834085586084257E-14 ) ) ;
#138188 = CARTESIAN_POINT ( 'NONE',  ( -1.435115314735526448, 7.268684689231142748, 4.324912918974801457 ) ) ;
#138189 = CARTESIAN_POINT ( 'NONE',  ( 4.289387122732970958, -0.003046686910593982868, -2.120778211268215419 ) ) ;
#138190 = CARTESIAN_POINT ( 'NONE',  ( 0.04061758243546764735, -1.421021341975825969, -1.170429047309962112 ) ) ;
#138191 = CARTESIAN_POINT ( 'NONE',  ( -1.500000000000011324, 5.410416667349489117, -0.8660254037844313801 ) ) ;
#138192 = CARTESIAN_POINT ( 'NONE',  ( 7.298366762858032430, 7.409182732956175244, 1.040834085586084257E-14 ) ) ;
#138193 = CARTESIAN_POINT ( 'NONE',  ( 5.712781623311797397, 7.758274208654143855, -1.599625672291283607 ) ) ;
#138194 = CARTESIAN_POINT ( 'NONE',  ( 4.886040457987857799, -0.9749269275126177803, 1.815604017143893634 ) ) ;
#138195 = CIRCLE ( 'NONE', #48225, 1.500000000000000222 ) ;
#138197 = CARTESIAN_POINT ( 'NONE',  ( 1.487592393518050837, -1.832424703912252317, -0.1798031890194173865 ) ) ;
#138196 = CARTESIAN_POINT ( 'NONE',  ( -7.389357414647957256, 8.579670724299436557, 1.199719254218450271 ) ) ;
#138198 = CARTESIAN_POINT ( 'NONE',  ( 5.751721435176966324, 6.248267645806530268, -1.064211863609406672 ) ) ;
#138199 = CARTESIAN_POINT ( 'NONE',  ( -9.579665964948882007, -7.325744180092283564, 5.204170427930421283E-15 ) ) ;
#138200 = CARTESIAN_POINT ( 'NONE',  ( 10.98194350564910415, -7.699999999999993072, -0.6300133639306324529 ) ) ;
#138201 = CARTESIAN_POINT ( 'NONE',  ( 1.014635385311330795, -0.9952708415592588231, -1.969785480804244315 ) ) ;
#138202 = CARTESIAN_POINT ( 'NONE',  ( 4.270984383450874944, -2.108973115933824527, -0.8193970387949424117 ) ) ;
#138203 = CARTESIAN_POINT ( 'NONE',  ( -7.361714222540411967, 11.53249099303175385, 0.000000000000000000 ) ) ;
#138204 = CARTESIAN_POINT ( 'NONE',  ( 4.113381391103660967, 1.458659968308340993, 1.074121561303176264 ) ) ;
#138205 = CARTESIAN_POINT ( 'NONE',  ( 4.012823373000539817, 0.09967532595039167720, 1.913279002700827514 ) ) ;
#138206 = CARTESIAN_POINT ( 'NONE',  ( 5.037584538744971141, 1.933038169019934527, -0.7419538039311265321 ) ) ;
#138207 = CARTESIAN_POINT ( 'NONE',  ( -1.364683531249997417, 3.821875000341416584, 1.214306433183764966E-14 ) ) ;
#138208 = CARTESIAN_POINT ( 'NONE',  ( 2.289859582131337223, -0.8446868967569521880, 1.781483357239101117 ) ) ;
#138209 = CARTESIAN_POINT ( 'NONE',  ( 1.096560174117457764, -0.4650716533593258761, -1.869300808490617305 ) ) ;
#138210 = CARTESIAN_POINT ( 'NONE',  ( 4.065207594588423845, 0.2294239933214488880, -1.856472568989680161 ) ) ;
#138211 = COLOUR_RGB ( '', 0.09019608, 0.27058824, 0.51372549) ;
#138212 = CARTESIAN_POINT ( 'NONE',  ( 3.721538942197761379, -0.1710094959430948913, 2.301408321908961607 ) ) ;
#138213 = CARTESIAN_POINT ( 'NONE',  ( 3.877287848637627210, -0.1385928533646582361, 1.855967808809717789 ) ) ;
#138214 = CARTESIAN_POINT ( 'NONE',  ( -1.364683531249997417, 4.009375000341424133, 1.214306433183764966E-14 ) ) ;
#138215 = DIRECTION ( 'NONE',  ( -0.000000000000000000, -1.000000000000000000, -0.000000000000000000 ) ) ;
#138216 = CARTESIAN_POINT ( 'NONE',  ( 1.787856894401329333, 1.453325235529376869, 1.524497383921459726 ) ) ;
#138217 = CARTESIAN_POINT ( 'NONE',  ( 3.511198595814932766, 5.119484333249288532, 1.443375672974066548 ) ) ;
#138219 = CARTESIAN_POINT ( 'NONE',  ( 5.045036709957831711, 4.903268083610561767, 0.3063280728123271568 ) ) ;
#138218 = CARTESIAN_POINT ( 'NONE',  ( -0.6823417656250212460, 5.363541667008087543, 1.181850606188767472 ) ) ;
#138220 = CARTESIAN_POINT ( 'NONE',  ( -1.921775512840688371, 9.000000000008071765, -0.7749999999999996891 ) ) ;
#138221 = CARTESIAN_POINT ( 'NONE',  ( 2.883181758455736432, -1.960942133159260692, -0.8077274430827171559 ) ) ;
#138222 = CARTESIAN_POINT ( 'NONE',  ( 5.717509255324652706, 7.006698007003303807, -2.500000000000000444 ) ) ;
#138223 = CARTESIAN_POINT ( 'NONE',  ( 0.9319058833903216543, -1.969584188619889487, 0.4467263836498857055 ) ) ;
#138224 = CARTESIAN_POINT ( 'NONE',  ( 0.6823417656249882723, 0.9260416670080831025, -1.181850606188749264 ) ) ;
#138225 = CARTESIAN_POINT ( 'NONE',  ( -4.622967192579922724, 4.495809267539077503, 1.214306433183764966E-14 ) ) ;
#138226 = CARTESIAN_POINT ( 'NONE',  ( 3.960953433486789521, 7.772862772376584850, -0.7998128361456221525 ) ) ;
#138227 = EDGE_LOOP ( 'NONE', ( #151684, #127052, #116755, #23372, #112771 ) ) ;
#138228 = CARTESIAN_POINT ( 'NONE',  ( 0.8960494714182369869, -0.7788709108395329705, 2.016556642405589184 ) ) ;
#138229 = CARTESIAN_POINT ( 'NONE',  ( 6.610000000000030518, 2.992693383986976041, 2.174209315121559349 ) ) ;
#138231 = CARTESIAN_POINT ( 'NONE',  ( 3.389175213736292047, 5.937492935125556315, 1.082531754730558626 ) ) ;
#138230 = CARTESIAN_POINT ( 'NONE',  ( 5.910428620914669473, 5.860197910680708944, 0.000000000000000000 ) ) ;
#138232 = DIRECTION ( 'NONE',  ( -0.01043841336116912988, 0.000000000000000000, -0.9999455182791217034 ) ) ;
#138233 = CARTESIAN_POINT ( 'NONE',  ( 5.577361344084559747, 1.530155114678043660, 1.313547687611632764 ) ) ;
#138234 = CARTESIAN_POINT ( 'NONE',  ( -8.107412671292051343, 10.48173408797264194, 1.443375672974090751 ) ) ;
#138235 = CARTESIAN_POINT ( 'NONE',  ( -0.1290005225502675879, -0.006633637972621592160, -2.173875058097324064 ) ) ;
#138236 = CARTESIAN_POINT ( 'NONE',  ( 0.000000000000000000, 0.000000000000000000, 11.09999999999999964 ) ) ;
#138238 = CARTESIAN_POINT ( 'NONE',  ( -0.6823417656250039265, 10.81770833367473550, -1.181850606188755259 ) ) ;
#138237 = CARTESIAN_POINT ( 'NONE',  ( 0.4974159974337259427, 1.879172763871908902, -1.259763710243780865 ) ) ;
#138239 = CARTESIAN_POINT ( 'NONE',  ( -7.323375529675950624, 11.69568855126397011, -0.7998128361456291469 ) ) ;
#138240 = EDGE_CURVE ( 'NONE', #110521, #206877, #181471, .T. ) ;
#138242 = CARTESIAN_POINT ( 'NONE',  ( 1.229944743773615956, 1.913488753162166045, 0.09234796458578581335 ) ) ;
#138241 = CARTESIAN_POINT ( 'NONE',  ( -4.894130264408858899, 8.653643041878236630, -0.7216878364870207285 ) ) ;
#138243 = CARTESIAN_POINT ( 'NONE',  ( -1.364683531250012516, 2.342708333674752286, 0.7879004041258379498 ) ) ;
#138244 = CARTESIAN_POINT ( 'NONE',  ( 0.3282377607281227738, 2.636164550367435133, 1.224999999999981659 ) ) ;
#138245 = CARTESIAN_POINT ( 'NONE',  ( -6.009258394948636914E-15, 9.687499999999996447, -1.732050807568875195 ) ) ;
#138246 = CARTESIAN_POINT ( 'NONE',  ( 3.404663882806455266, 1.358838683821527393, -1.062305643495575103 ) ) ;
#138247 = CARTESIAN_POINT ( 'NONE',  ( 3.379725431556547477, 7.165039780116438273, -1.734723475976807094E-15 ) ) ;
#138248 = CARTESIAN_POINT ( 'NONE',  ( 1.704008468626088790, -0.6311095051503686770, -1.653581786927365904 ) ) ;
#138249 = CARTESIAN_POINT ( 'NONE',  ( 3.088541981101311507, -1.197259257089001716, 1.618239360019198880 ) ) ;
#138250 = CARTESIAN_POINT ( 'NONE',  ( 8.387690588348714726, 12.93738945304888333, 1.040834085586084257E-14 ) ) ;
#138251 = CARTESIAN_POINT ( 'NONE',  ( 5.649526978565787338, -1.736373965863503122, -1.361823127433124725 ) ) ;
#138252 = EDGE_LOOP ( 'NONE', ( #111438, #71044, #202581 ) ) ;
#138253 = CARTESIAN_POINT ( 'NONE',  ( 4.342060261306793123, -1.245981751006501437, -1.589553384294100091 ) ) ;
#138254 = CARTESIAN_POINT ( 'NONE',  ( -7.923814432544069142, 8.209148024248356990, 0.000000000000000000 ) ) ;
#138256 = CARTESIAN_POINT ( 'NONE',  ( 3.831657784458125882, 0.6766976527424087839, -1.899625577706779422 ) ) ;
#138255 = CARTESIAN_POINT ( 'NONE',  ( 4.037823014030429647, -2.028772383530423884, 0.6168223452112443494 ) ) ;
#138257 = ORIENTED_EDGE ( 'NONE', *, *, #22298, .T. ) ;
#138258 = CARTESIAN_POINT ( 'NONE',  ( 4.712340909201580885, 7.655425606447271214, -1.199719254218452047 ) ) ;
#138259 = ORIENTED_EDGE ( 'NONE', *, *, #176346, .F. ) ;
#138260 = CARTESIAN_POINT ( 'NONE',  ( 1.428351348257720588, 1.801920623737063520, 0.5021531274154652502 ) ) ;
#138261 = CARTESIAN_POINT ( 'NONE',  ( 1.499999999999821032, 7.268077025657388113, -4.207854987879545483 ) ) ;
#138262 = CARTESIAN_POINT ( 'NONE',  ( 6.182253972182746971, 0.9374619682817868505, 1.549891177688822452 ) ) ;
#138263 = CARTESIAN_POINT ( 'NONE',  ( -2.764973262183167968, 5.313220341600567664, 1.199719254218462483 ) ) ;
#138264 = CARTESIAN_POINT ( 'NONE',  ( -9.670366421564544623, 3.035553407718987629, -6.557686755922881972 ) ) ;
#138265 = CARTESIAN_POINT ( 'NONE',  ( -0.6823417656250003738, 2.530208333674753618, -1.181850606188749264 ) ) ;
#138266 = CARTESIAN_POINT ( 'NONE',  ( 6.830415307812257808, -7.246166700180801001, 6.717278222822394618 ) ) ;
#138267 = ORIENTED_EDGE ( 'NONE', *, *, #93452, .T. ) ;
#138268 = CARTESIAN_POINT ( 'NONE',  ( 5.722950238744198614, 8.730506807626655430, 1.082531754730549967 ) ) ;
#138269 = CARTESIAN_POINT ( 'NONE',  ( -3.960390268967665328, 6.674186842887300131, 1.082531754730549967 ) ) ;
#138270 = CARTESIAN_POINT ( 'NONE',  ( -4.586401103172829785, 8.572828063668767484, 0.7998128361456281477 ) ) ;
#138271 = CARTESIAN_POINT ( 'NONE',  ( 4.342108446431157454, -1.306982937058022820, -1.669832246961988176 ) ) ;
#138273 = CARTESIAN_POINT ( 'NONE',  ( -10.78237064342727791, 6.270194388237658956, -4.501389708959286473 ) ) ;
#138272 = CARTESIAN_POINT ( 'NONE',  ( 2.400879090975676089, 3.975933801733734896, -11.29524806062144116 ) ) ;
#138274 = CARTESIAN_POINT ( 'NONE',  ( 4.991463202408453093, 1.458887350482462875, 1.326006969317705009 ) ) ;
#138275 = CARTESIAN_POINT ( 'NONE',  ( -0.6823417656250246877, 0.5510416670080897639, 1.181850606188755259 ) ) ;
#138276 = CARTESIAN_POINT ( 'NONE',  ( 1.318609283782465003, -0.7284450440303428254, -1.876953636963938354 ) ) ;
#138277 = VERTEX_POINT ( 'NONE', #65568 ) ;
#138278 = CARTESIAN_POINT ( 'NONE',  ( -0.05292715583045219663, -1.893440308637056146, -0.9475653277955156106 ) ) ;
#138279 = DIRECTION ( 'NONE',  ( -7.993605777301127091E-15, 0.000000000000000000, -1.000000000000000000 ) ) ;
#138280 = CARTESIAN_POINT ( 'NONE',  ( 1.469279758060073160, 1.824989553406907383, 0.9776941847434923449 ) ) ;
#138281 = ORIENTED_EDGE ( 'NONE', *, *, #211661, .T. ) ;
#138282 = CARTESIAN_POINT ( 'NONE',  ( 6.364626766972446781, 6.390095747748157251, 0.7998128361456352531 ) ) ;
#138283 = CARTESIAN_POINT ( 'NONE',  ( 4.362691568547328202, 8.311833606605697256, -0.7998128361456381397 ) ) ;
#138285 = CARTESIAN_POINT ( 'NONE',  ( 3.832150974156964818, 7.622593236491780999, 1.040834085586084257E-14 ) ) ;
#138284 = CARTESIAN_POINT ( 'NONE',  ( 4.312501488504257630, 1.911392599577836693, 0.8473735431044140398 ) ) ;
#138286 = CARTESIAN_POINT ( 'NONE',  ( 7.374709211190586089, 7.568525266002632534, 0.000000000000000000 ) ) ;
#138289 = ORIENTED_EDGE ( 'NONE', *, *, #131699, .F. ) ;
#138288 = CARTESIAN_POINT ( 'NONE',  ( 1.945701609745503324, -1.183853311710543199, -1.371160031100856935 ) ) ;
#138287 = CARTESIAN_POINT ( 'NONE',  ( 3.381694320706640333, 1.157239582903809128, 1.411935816614327655 ) ) ;
#138290 = CARTESIAN_POINT ( 'NONE',  ( 6.498651167236064730, -0.5841124237929047336, -2.128106146270396071 ) ) ;
#138291 = DIRECTION ( 'NONE',  ( 0.000000000000000000, 0.000000000000000000, -1.000000000000000000 ) ) ;
#138292 = CARTESIAN_POINT ( 'NONE',  ( 4.225739626866775289, -2.112672615930260900, 0.6375689414055001336 ) ) ;
#138293 = CARTESIAN_POINT ( 'NONE',  ( -1.402160292154681736E-14, 9.484375000341398021, 1.575800808251682339 ) ) ;
#138294 = CARTESIAN_POINT ( 'NONE',  ( 2.385291144485178982, 0.09204604084523880514, -1.910175020619097275 ) ) ;
#138295 = MECHANICAL_DESIGN_GEOMETRIC_PRESENTATION_REPRESENTATION (  '', ( #210933 ), #72549 ) ;
#138296 = CARTESIAN_POINT ( 'NONE',  ( 8.880754312151170282, 10.31963377138658089, 1.199719254218453823 ) ) ;
#138297 = CARTESIAN_POINT ( 'NONE',  ( 6.426242046702522082, 1.060841730010402495, 1.777776562702712226 ) ) ;
#138298 = CARTESIAN_POINT ( 'NONE',  ( 1.360316468749973140, 0.5468750003413819227, -2.081668171172168513E-14 ) ) ;
#138299 = CARTESIAN_POINT ( 'NONE',  ( 5.442994344319362021, -1.727133847215430729, -1.348975639928217118 ) ) ;
#138300 = CARTESIAN_POINT ( 'NONE',  ( 5.696489930276292135, 7.416392257432566026, -1.320530921439456273 ) ) ;
#138301 = CARTESIAN_POINT ( 'NONE',  ( -9.473215147174821382, -6.532648913094946330, 0.3561222683123355104 ) ) ;
#138302 = EDGE_LOOP ( 'NONE', ( #21434, #152130 ) ) ;
#138303 = CARTESIAN_POINT ( 'NONE',  ( 1.532410409194677081, -1.041802156240267951, 1.385306760018462313 ) ) ;
#138304 = ADVANCED_FACE ( 'NONE', ( #101283 ), #99175, .T. ) ;
#138305 = CARTESIAN_POINT ( 'NONE',  ( 3.655401173194738007, 0.4573680094964554521, -1.813624142381641491 ) ) ;
#138306 = DIRECTION ( 'NONE',  ( 8.638326563840814399E-31, 0.000000000000000000, 1.000000000000000000 ) ) ;
#138307 = CARTESIAN_POINT ( 'NONE',  ( -0.7500000000000006661, 12.48958333401613352, -1.299038105676657340 ) ) ;
#138308 = CARTESIAN_POINT ( 'NONE',  ( -8.703971430293361067, 9.256980878204810637, 0.7216878364870438212 ) ) ;
#138309 = CARTESIAN_POINT ( 'NONE',  ( 3.725458348705031231, 7.568394850123006279, -1.734723475976807094E-15 ) ) ;
#138310 = CARTESIAN_POINT ( 'NONE',  ( 6.614133338355735248, 2.065126723422955557, -0.1462301744803648496 ) ) ;
#138311 = CARTESIAN_POINT ( 'NONE',  ( 1.651970485933237143, 1.039013645561959853, 1.727991324714774013 ) ) ;
#138312 = CARTESIAN_POINT ( 'NONE',  ( -9.321394304595349567, 10.83371376257142416, 1.199719254218462483 ) ) ;
#138313 = CARTESIAN_POINT ( 'NONE',  ( 5.096939404094710468, 4.911127157724081371, 0.000000000000000000 ) ) ;
#138314 = CARTESIAN_POINT ( 'NONE',  ( 1.306853331985533107, 1.934050699793531836, 1.030479497498619557 ) ) ;
#138315 = CARTESIAN_POINT ( 'NONE',  ( 5.443921307256319508, 0.7362202147598859714, -1.670853202368663082 ) ) ;
#138316 = CARTESIAN_POINT ( 'NONE',  ( -3.737243898861318137, 7.511868315313511069, 0.7998128361456341429 ) ) ;
#138317 = CARTESIAN_POINT ( 'NONE',  ( 6.373741612200171325, 7.569024981389272710, 1.082531754730549967 ) ) ;
#138318 = CARTESIAN_POINT ( 'NONE',  ( 9.585778300061798873, 11.14216175728232550, -1.199719254218440723 ) ) ;
#138319 = CARTESIAN_POINT ( 'NONE',  ( -5.926849427829407269, 6.943687749669614995, -1.199719254218453823 ) ) ;
#138320 = CARTESIAN_POINT ( 'NONE',  ( 4.330940004561544043, 7.140181541042074365, -1.199719254218452047 ) ) ;
#138321 = CARTESIAN_POINT ( 'NONE',  ( 7.241463443474815520, 8.581367117876336437, -1.082531754730548412 ) ) ;
#138322 = VERTEX_POINT ( 'NONE', #150055 ) ;
#138324 = CARTESIAN_POINT ( 'NONE',  ( 0.1002437576986033446, -0.9471954198254585178, 1.776316830230479260 ) ) ;
#138323 = CARTESIAN_POINT ( 'NONE',  ( 2.929072846782492245, -1.238530643895646488, -1.362589426554157157 ) ) ;
#138325 = CARTESIAN_POINT ( 'NONE',  ( 1.458857794315861156, 1.741214688395021470, 1.500301734068248294 ) ) ;
#138327 = CARTESIAN_POINT ( 'NONE',  ( 6.877797714452785982, -1.903667959252927533, 0.4735691183095217527 ) ) ;
#138326 = CARTESIAN_POINT ( 'NONE',  ( 3.063779527008304360, 6.518233848244248563, 0.7216878364870317197 ) ) ;
#138328 = CARTESIAN_POINT ( 'NONE',  ( -5.413783410558481002, 5.210502155273325720, -0.7998128361456221525 ) ) ;
#138329 = CARTESIAN_POINT ( 'NONE',  ( -4.016220928916872879, 7.677703825520077352, -0.2262283546238970933 ) ) ;
#138330 = CARTESIAN_POINT ( 'NONE',  ( 3.164218664783400747, 1.912571728330178855, -0.004505864839042527346 ) ) ;
#138331 = CARTESIAN_POINT ( 'NONE',  ( -9.429859533504656000, 10.96025652963230534, -1.199719254218441611 ) ) ;
#138332 = CARTESIAN_POINT ( 'NONE',  ( 6.353009478083933459, 6.838182937092724956, 0.6209923359970755952 ) ) ;
#138333 = CARTESIAN_POINT ( 'NONE',  ( -5.966997003790217136, 9.975597247814986801, -0.7216878364870338292 ) ) ;
#138335 = CARTESIAN_POINT ( 'NONE',  ( 1.358040219746913024, 0.7549631825471068147, 1.711723683848711985 ) ) ;
#138334 = CARTESIAN_POINT ( 'NONE',  ( 2.191069407410517478, 1.617985365078830950, 1.324160459713573879 ) ) ;
#138336 = CARTESIAN_POINT ( 'NONE',  ( 2.266953675890924558, -2.015725231744563306, 0.04666741021024794350 ) ) ;
#138337 = CARTESIAN_POINT ( 'NONE',  ( 7.863365906246055914, 10.19701286208565705, -1.443375672974057666 ) ) ;
#138338 = CARTESIAN_POINT ( 'NONE',  ( -1.201851678989727383E-14, 3.509375000341421469, -1.575800808251660134 ) ) ;
#138339 = CARTESIAN_POINT ( 'NONE',  ( 3.157457554155696844, 0.7852445609939761040, 1.553317506218002464 ) ) ;
#138340 = MECHANICAL_DESIGN_GEOMETRIC_PRESENTATION_REPRESENTATION (  '', ( #155498 ), #172827 ) ;
#138341 = CARTESIAN_POINT ( 'NONE',  ( 4.253507506385319381, 5.985511395581417204, 1.599625672291267398 ) ) ;
#138343 = CYLINDRICAL_SURFACE ( 'NONE', #203373, 1.500000000000000222 ) ;
#138342 = CARTESIAN_POINT ( 'NONE',  ( 1.734723475976807094E-15, 15.42691958146951414, 11.91973154060106665 ) ) ;
#138344 = CARTESIAN_POINT ( 'NONE',  ( 3.228823373612188519, 0.04322303627742052345, 1.724510841617853840 ) ) ;
#138345 = CARTESIAN_POINT ( 'NONE',  ( 2.964592600559623037, -2.025863808726846127, -0.8364240203130177687 ) ) ;
#138346 = CARTESIAN_POINT ( 'NONE',  ( 5.654950187766193181, -1.741821662664808867, 1.355018943897445149 ) ) ;
#138347 = CARTESIAN_POINT ( 'NONE',  ( -9.348526197514022584, 4.999985930147239799, -7.001887667968696327 ) ) ;
#138348 = CARTESIAN_POINT ( 'NONE',  ( 3.327178260015594802, -2.004142704238300876, -0.8352945444606455494 ) ) ;
#138349 = CARTESIAN_POINT ( 'NONE',  ( 2.473051018021198200, 0.08991741065280876855, -1.823594477012622228 ) ) ;
#138350 = DIRECTION ( 'NONE',  ( 0.7592566023653004592, -0.6507913734559641616, -1.725633230170963105E-31 ) ) ;
#138351 = CARTESIAN_POINT ( 'NONE',  ( 4.821547164884887771, -1.499609098395672246, -1.495007082409164356 ) ) ;
#138352 = CARTESIAN_POINT ( 'NONE',  ( 6.639320575229248789, 2.444019389566108647, 2.379739370560208567 ) ) ;
#138353 = EDGE_CURVE ( 'NONE', #77951, #66179, #167912, .T. ) ;
#138354 = ORIENTED_EDGE ( 'NONE', *, *, #147573, .T. ) ;
#138356 = CARTESIAN_POINT ( 'NONE',  ( -1.364683531249997417, 2.821875000341422801, 1.214306433183764966E-14 ) ) ;
#138355 = CARTESIAN_POINT ( 'NONE',  ( 4.529038776287770851, -2.096192991274762996, 0.9282860960324219590 ) ) ;
#138357 = CARTESIAN_POINT ( 'NONE',  ( 0.6124999999999655165, 0.08333333333334497217, 1.060881119635885828 ) ) ;
#138358 = CARTESIAN_POINT ( 'NONE',  ( 8.866142388332804103, 12.43125098877526113, -1.199719254218446718 ) ) ;
#138359 = CARTESIAN_POINT ( 'NONE',  ( 0.1004478525090373164, -0.9956121213324088393, 1.872212410442177344 ) ) ;
#138360 = CARTESIAN_POINT ( 'NONE',  ( -6.249945626219832739, 6.393950773452325542, 1.040834085586084257E-14 ) ) ;
#138361 = CARTESIAN_POINT ( 'NONE',  ( 4.541618270897912701, 4.400902192243413502, 1.214306433183764966E-14 ) ) ;
#138362 = CARTESIAN_POINT ( 'NONE',  ( -4.704316113817535339, 8.432193199521691440, 0.7216878364870458196 ) ) ;
#138363 =( BOUNDED_SURFACE ( )  B_SPLINE_SURFACE ( 3, 2, ( 
 ( #181988, #80244, #213416 ),
 ( #16278, #1094, #67155 ),
 ( #49876, #212355, #163642 ),
 ( #13096, #199297, #130147 ),
 ( #96527, #179885, #197183 ),
 ( #111749, #148453, #23 ),
 ( #145292, #195061, #162576 ),
 ( #146342, #47777, #31509 ),
 ( #97584, #15223, #147389 ),
 ( #48820, #114936, #55206 ) ),
 .UNSPECIFIED., .F., .F., .T. ) 
 B_SPLINE_SURFACE_WITH_KNOTS ( ( 4, 2, 2, 2, 4 ),
 ( 3, 3 ),
 ( 0.001504998634567469764, 0.001881248293209337313, 0.002257497951851204863, 0.002633747610493072412, 0.003009997269134939962 ),
 ( 0.000000000000000000, 1.000000000000000000 ),
 .UNSPECIFIED. ) 
 GEOMETRIC_REPRESENTATION_ITEM ( )  RATIONAL_B_SPLINE_SURFACE ( (
 ( 1.000000000000000000, 0.7127552757490021040, 1.000000000000000000),
 ( 1.000000000000000000, 0.7006570731214798453, 1.000000000000000000),
 ( 1.000000000000000000, 0.7089665949506331888, 1.000000000000000000),
 ( 1.000000000000000000, 0.7450337546129037758, 1.000000000000000000),
 ( 1.000000000000000000, 0.7695313365922599180, 1.000000000000000000),
 ( 1.000000000000000000, 0.7891799723974980418, 1.000000000000000000),
 ( 1.000000000000000000, 0.7830193708541549613, 1.000000000000000000),
 ( 1.000000000000000000, 0.7491666546211300792, 1.000000000000000000),
 ( 1.000000000000000000, 0.7234076953912167429, 1.000000000000000000),
 ( 1.000000000000000000, 0.7127558927793078425, 1.000000000000000000) ) ) 
 REPRESENTATION_ITEM ( '' )  SURFACE ( )  );
#138364 = CARTESIAN_POINT ( 'NONE',  ( -6.773846765317340868, -7.246166700180801001, -6.773846765317301788 ) ) ;
#138365 = VERTEX_POINT ( 'NONE', #68765 ) ;
#138366 = CARTESIAN_POINT ( 'NONE',  ( 5.291638762709002464, 1.525045427759319727, -1.319226660814104335 ) ) ;
#138368 = CARTESIAN_POINT ( 'NONE',  ( 3.098538415137185531, 2.046439989356943823, 0.2571918767454490773 ) ) ;
#138367 = CARTESIAN_POINT ( 'NONE',  ( 5.996784015946103885, 5.890669528225568996, 1.040834085586084257E-14 ) ) ;
#138370 = CARTESIAN_POINT ( 'NONE',  ( -0.2409995289980003397, 4.087843961663322645, -2.555282842491034323 ) ) ;
#138369 = CARTESIAN_POINT ( 'NONE',  ( 6.535912570239620578, 9.782925877658371405, 1.199719254218452047 ) ) ;
#138371 = CARTESIAN_POINT ( 'NONE',  ( 6.550524494058025837, 7.671308660269694712, -1.199719254218452047 ) ) ;
#138372 = CARTESIAN_POINT ( 'NONE',  ( -1.642778471875000035, -1.217708332855376607, -2.845375778867859751 ) ) ;
#138373 = DIRECTION ( 'NONE',  ( 0.000000000000000000, 1.000000000000000000, 0.000000000000000000 ) ) ;
#138374 = CARTESIAN_POINT ( 'NONE',  ( 6.667925998804712151, -1.351855065013835455, 1.725503752137508284 ) ) ;
#138375 = CARTESIAN_POINT ( 'NONE',  ( 3.516250148862578584, -1.862017090670412767, 0.7743150488077471527 ) ) ;
#138376 = CARTESIAN_POINT ( 'NONE',  ( 3.087279721815265443, -0.7436087841871074078, 1.684586988852328160 ) ) ;
#138377 = EDGE_CURVE ( 'NONE', #190177, #58907, #208600, .T. ) ;
#138378 = CARTESIAN_POINT ( 'NONE',  ( 5.575427483717746213, 7.527751369135936343, 1.599625672291267398 ) ) ;
#138379 = SURFACE_STYLE_USAGE ( .BOTH. , #6201 ) ;
#138380 = CARTESIAN_POINT ( 'NONE',  ( 0.6742806677700216023, -1.621663110835226629, -0.5878086553270861492 ) ) ;
#138381 = CARTESIAN_POINT ( 'NONE',  ( -3.440018289565379028, 5.036440642624797626, 1.599625672291267398 ) ) ;
#138382 = CARTESIAN_POINT ( 'NONE',  ( 0.4757056697715462690, -2.282288811291408148, -0.2737132658124728501 ) ) ;
#138383 = CARTESIAN_POINT ( 'NONE',  ( -5.540478329478883524, 9.615641817700700145, 0.000000000000000000 ) ) ;
#138384 = CARTESIAN_POINT ( 'NONE',  ( 0.5622849326936694148, 2.237558834470813274, -0.3334926475991057959 ) ) ;
#138385 = CARTESIAN_POINT ( 'NONE',  ( 3.563196004013529983, -1.857486927118640718, -0.9925908497740908443 ) ) ;
#138386 = CARTESIAN_POINT ( 'NONE',  ( -5.152980901645737077, 8.169505597632108262, -1.199719254218453823 ) ) ;
#138387 = CARTESIAN_POINT ( 'NONE',  ( 8.437251666405968464, 8.737881787095446384, 1.040834085586084257E-14 ) ) ;
#138388 = CARTESIAN_POINT ( 'NONE',  ( 5.180624093753221970, 9.058162186105164437, 0.000000000000000000 ) ) ;
#138389 =( NAMED_UNIT ( * ) SI_UNIT ( $, .STERADIAN. ) SOLID_ANGLE_UNIT ( ) );
#138390 = CARTESIAN_POINT ( 'NONE',  ( -7.172426956829277778, 8.326585190177668849, -1.199719254218452935 ) ) ;
#138391 = CARTESIAN_POINT ( 'NONE',  ( 7.253248993186731219, 8.524840582548424806, 1.082531754730558626 ) ) ;
#138392 = CARTESIAN_POINT ( 'NONE',  ( 4.145277420728366025, 7.638539262984231470, 0.7997124044470202975 ) ) ;
#138393 = CARTESIAN_POINT ( 'NONE',  ( -5.596818484342970912, 5.424043074688562172, -0.7998128361456221525 ) ) ;
#138394 = CARTESIAN_POINT ( 'NONE',  ( 3.674281580191523400, 2.204306621758029383, -0.2748671541705596799 ) ) ;
#138395 = CARTESIAN_POINT ( 'NONE',  ( 2.431793384409334902, 1.031818167245980744, -1.933333044699905079 ) ) ;
#138396 = CARTESIAN_POINT ( 'NONE',  ( -6.063521013809733518, 8.097193820909906137, 1.599625672291283607 ) ) ;
#138397 = CARTESIAN_POINT ( 'NONE',  ( -4.098307573080856692, 8.003385611894792362, 0.7998128361456352531 ) ) ;
#138398 = CARTESIAN_POINT ( 'NONE',  ( 5.037533845850875380, 1.831247050742194515, -0.7043679133837479345 ) ) ;
#138399 = CARTESIAN_POINT ( 'NONE',  ( 1.734723475976807094E-15, -3.469446951953614189E-15, -0.2913868168252300994 ) ) ;
#138400 = CARTESIAN_POINT ( 'NONE',  ( 1.364683531249988535, 1.363541667008083769, 0.7879004041258500513 ) ) ;
#138401 = CARTESIAN_POINT ( 'NONE',  ( -4.990809943606294929, 4.995235487061662205, -0.7216878364870338292 ) ) ;
#138402 = CARTESIAN_POINT ( 'NONE',  ( -5.246642258808529746, 9.064907035344523578, 0.000000000000000000 ) ) ;
#138403 = CARTESIAN_POINT ( 'NONE',  ( 4.219064148821600746, 1.637239594409030330, -1.347683705884415106 ) ) ;
#138404 = CARTESIAN_POINT ( 'NONE',  ( -4.065465959251405081, 5.836405933916976707, -1.599625672291271394 ) ) ;
#138405 = ORIENTED_EDGE ( 'NONE', *, *, #65245, .T. ) ;
#138406 = CARTESIAN_POINT ( 'NONE',  ( 5.577088068215094729, -0.04877400797019536272, -2.161318155665878038 ) ) ;
#138407 = CARTESIAN_POINT ( 'NONE',  ( 6.063521013809720195, 8.097193820909906137, 1.599625672291281386 ) ) ;
#138408 = CARTESIAN_POINT ( 'NONE',  ( 5.144037045698616417, 0.5398437887287730330, 1.760322748975438500 ) ) ;
#138409 = CARTESIAN_POINT ( 'NONE',  ( -5.903030530102264528, 6.005529115149156993, -0.1628943571830038795 ) ) ;
#138410 = CARTESIAN_POINT ( 'NONE',  ( -1.201851678989727383E-14, 0.8843750003414173610, 1.575800808251672791 ) ) ;
#138411 = CARTESIAN_POINT ( 'NONE',  ( 0.3095773630682343569, 1.202386210327820004, -1.258585571321766627 ) ) ;
#138412 = CARTESIAN_POINT ( 'NONE',  ( 6.727182134110202050, 7.629137130509070275, 2.410944104600750038 ) ) ;
#138413 = CARTESIAN_POINT ( 'NONE',  ( 0.3633361122992279646, 3.192526366011316341, 2.035233858735807644 ) ) ;
#138414 = CARTESIAN_POINT ( 'NONE',  ( -0.4379653042624916948, 3.065656782498161537, 0.4195809500673950421 ) ) ;
#138415 = PRESENTATION_LAYER_ASSIGNMENT (  '', '', ( #83029 ) ) ;
#138416 = CARTESIAN_POINT ( 'NONE',  ( 4.170900312159072421, -2.016029151617684256, -0.7805680927704603533 ) ) ;
#138417 = CARTESIAN_POINT ( 'NONE',  ( -3.100010679019018500, 6.768429558830820980, 1.040834085586084257E-14 ) ) ;
#138418 = CARTESIAN_POINT ( 'NONE',  ( -5.870317324592805086, 9.792527945426188651, -0.7216878364870197293 ) ) ;
#138419 = CARTESIAN_POINT ( 'NONE',  ( 3.045950098598048328, 0.7793912989166664751, -2.016482303682599841 ) ) ;
#138420 = CARTESIAN_POINT ( 'NONE',  ( 4.657473197611246896, 0.4347632249906174806, -1.922659379041303129 ) ) ;
#138421 = CARTESIAN_POINT ( 'NONE',  ( 3.426783358884141428, 0.7772304037446680081, 1.549921577765429825 ) ) ;
#138422 = EDGE_CURVE ( 'NONE', #159827, #121606, #53805, .T. ) ;
#138423 = CARTESIAN_POINT ( 'NONE',  ( 0.4334776158547505864, -1.553986563932317377, -1.545601477622601472 ) ) ;
#138424 = CARTESIAN_POINT ( 'NONE',  ( 1.642099192286674336, -1.672607260348612845, -1.589979871525433408 ) ) ;
#138425 = CARTESIAN_POINT ( 'NONE',  ( 3.251298195952691206, -1.682652751511631850, -1.189445392860078110 ) ) ;
#138426 = CARTESIAN_POINT ( 'NONE',  ( 6.075724011240296818, -1.035248994944122369, 1.642949693582099302 ) ) ;
#138427 = CARTESIAN_POINT ( 'NONE',  ( -7.334597914868727919, 10.54048608644677465, -1.082531754730543083 ) ) ;
#138429 = ADVANCED_FACE ( 'NONE', ( #118672 ), #184655, .T. ) ;
#138428 = CARTESIAN_POINT ( 'NONE',  ( -6.140917232347002042, 6.129101290685087911, -0.7998128361456362523 ) ) ;
#138430 = DIRECTION ( 'NONE',  ( 0.6507913734559640506, -0.7592566023653004592, 0.000000000000000000 ) ) ;
#138432 = ORIENTED_EDGE ( 'NONE', *, *, #200474, .F. ) ;
#138431 = CARTESIAN_POINT ( 'NONE',  ( -1.299038105676632915, 5.999999999999998224, -0.7500000000000006661 ) ) ;
#138433 = CARTESIAN_POINT ( 'NONE',  ( -6.331294547457448019, 10.33033470543493770, 0.7216878364870458196 ) ) ;
#138434 = CARTESIAN_POINT ( 'NONE',  ( 3.294164632606086940, -0.8960083017303889230, 2.016869484631748310 ) ) ;
#138435 = CARTESIAN_POINT ( 'NONE',  ( 1.642778471875000035, -3.463541666188708845, -2.845375778867859751 ) ) ;
#138436 = EDGE_LOOP ( 'NONE', ( #169192, #61891 ) ) ;
#138437 = CARTESIAN_POINT ( 'NONE',  ( 0.3560157238547481118, -1.860367465765656814, -0.05377290132800408712 ) ) ;
#138438 = CARTESIAN_POINT ( 'NONE',  ( -0.02900071798685525254, 1.326456003635017922, -2.425894103910302135 ) ) ;
#138439 = CARTESIAN_POINT ( 'NONE',  ( -1.499999999999997780, 5.681250000682820378, 1.214306433183764966E-14 ) ) ;
#138440 = CARTESIAN_POINT ( 'NONE',  ( 4.232984923718338344, 7.533997312158466464, -0.9744250676351111640 ) ) ;
#138442 = CARTESIAN_POINT ( 'NONE',  ( 6.620655732516647518, 0.007553340620044743381, 1.826407896915738238 ) ) ;
#138441 = CARTESIAN_POINT ( 'NONE',  ( -6.529347706211431124, 6.814240946220119000, -0.5220719126654594922 ) ) ;
#138443 = CARTESIAN_POINT ( 'NONE',  ( 6.263598714517844002, 0.9507720431706817577, 1.576509192756641475 ) ) ;
#138444 = EDGE_LOOP ( 'NONE', ( #114129, #157312, #39236 ) ) ;
#138445 = CARTESIAN_POINT ( 'NONE',  ( 1.973578683463860672, 1.972434364383905292, -0.5973212362519930707 ) ) ;
#138446 = CARTESIAN_POINT ( 'NONE',  ( -0.6801582343750161019, 0.6822916670080614310, 1.178068619123810334 ) ) ;
#138447 = CARTESIAN_POINT ( 'NONE',  ( -6.989391883044787868, 8.113044270762433285, -1.199719254218446718 ) ) ;
#138448 = CARTESIAN_POINT ( 'NONE',  ( 4.955668840994886359, 5.740367388370866131, 1.199719254218462483 ) ) ;
#138449 = CARTESIAN_POINT ( 'NONE',  ( 1.323197370116558469, -0.05141181009169673577, 2.060424651611890479 ) ) ;
#138450 = CARTESIAN_POINT ( 'NONE',  ( 4.845164456061270997, 0.5726227986864868003, -1.750029900461601340 ) ) ;
#138451 = CARTESIAN_POINT ( 'NONE',  ( 6.494519276145969577, 7.535692896047149425, -1.199719254218446718 ) ) ;
#138452 =( BOUNDED_SURFACE ( )  B_SPLINE_SURFACE ( 3, 2, ( 
 ( #202360, #54010, #203426 ),
 ( #3089, #37760, #36677 ),
 ( #205578, #86506, #172036 ),
 ( #103833, #169881, #39905 ),
 ( #21471, #71295, #121230 ),
 ( #107092, #19356, #187200 ),
 ( #56146, #38828, #104912 ),
 ( #69160, #22552, #88658 ) ),
 .UNSPECIFIED., .F., .F., .T. ) 
 B_SPLINE_SURFACE_WITH_KNOTS ( ( 4, 2, 2, 4 ),
 ( 3, 3 ),
 ( 0.000000000000000000, 0.0002204160392919284333, 0.0004408320785838568665, 0.0008816641571677137331 ),
 ( 0.000000000000000000, 1.000000000000000000 ),
 .UNSPECIFIED. ) 
 GEOMETRIC_REPRESENTATION_ITEM ( )  RATIONAL_B_SPLINE_SURFACE ( (
 ( 1.000000000000000000, 0.4127341956165090364, 1.000000000000000000),
 ( 1.000000000000000000, 0.4103180386331816698, 1.000000000000000000),
 ( 1.000000000000000000, 0.4223234233957802730, 1.000000000000000000),
 ( 1.000000000000000000, 0.4613847219399360156, 1.000000000000000000),
 ( 1.000000000000000000, 0.4878744032655297769, 1.000000000000000000),
 ( 1.000000000000000000, 0.5702658980235773001, 1.000000000000000000),
 ( 1.000000000000000000, 0.6280001242509168913, 1.000000000000000000),
 ( 1.000000000000000000, 0.6787756258918240526, 1.000000000000000000) ) ) 
 REPRESENTATION_ITEM ( '' )  SURFACE ( )  );
#138453 = AXIS2_PLACEMENT_3D ( 'NONE', #79505, #209480, #194321 ) ;
#138454 = CARTESIAN_POINT ( 'NONE',  ( -6.493429226302317225, 6.540365283632955773, 0.7998128361456341429 ) ) ;
#138455 = PRESENTATION_STYLE_ASSIGNMENT (( #73428 ) ) ;
#138456 = CARTESIAN_POINT ( 'NONE',  ( 4.864015066594513215, 2.183220759563545776, -0.3215228633955333759 ) ) ;
#138457 = CARTESIAN_POINT ( 'NONE',  ( 6.784454189598811524, -2.216766238704069636, -0.4514476129710183194 ) ) ;
#138458 = CARTESIAN_POINT ( 'NONE',  ( -3.904385051055635270, 6.538571078664754843, 1.082531754730560403 ) ) ;
#138459 = CARTESIAN_POINT ( 'NONE',  ( 0.2285749388857594433, 1.317234250586714284, -1.386657971642536014 ) ) ;
#138460 = CARTESIAN_POINT ( 'NONE',  ( 1.130092623156966347, 2.014433208573155110, 0.09411304420373775570 ) ) ;
#138461 = CARTESIAN_POINT ( 'NONE',  ( 5.668717623845194176, 9.627604637879139560, 0.000000000000000000 ) ) ;
#138462 = CARTESIAN_POINT ( 'NONE',  ( 6.807498166657679484, -0.4075194142965676836, 1.832415718333743282 ) ) ;
#138463 = CARTESIAN_POINT ( 'NONE',  ( 6.410809557875646547, -0.5148348048229570706, -1.841598127471068658 ) ) ;
#138464 = FACE_OUTER_BOUND ( 'NONE', #206267, .T. ) ;
#138465 = CARTESIAN_POINT ( 'NONE',  ( 1.569004590881704075, 0.1408476687595125731, -1.865417194689425795 ) ) ;
#138466 = CARTESIAN_POINT ( 'NONE',  ( 2.255092540634635156, 0.09411513195021348199, -2.014433103604281960 ) ) ;
#138468 = CARTESIAN_POINT ( 'NONE',  ( -5.984739259312381598, 6.154819375939016624, 0.1731420012108849660 ) ) ;
#138467 = CARTESIAN_POINT ( 'NONE',  ( -0.6823417656250212460, 1.301041667008083547, 1.181850606188755259 ) ) ;
#138470 = CARTESIAN_POINT ( 'NONE',  ( 5.127606433170654121, -2.000101594804974514, 0.6598296307055817600 ) ) ;
#138469 = CARTESIAN_POINT ( 'NONE',  ( -7.828943636887387925, 11.22118577875556156, 1.199719254218453823 ) ) ;
#138471 = CARTESIAN_POINT ( 'NONE',  ( 6.259060471003163428, 10.45398764947904624, -0.7998128361456291469 ) ) ;
#138473 = CARTESIAN_POINT ( 'NONE',  ( -6.503107236049161521, 10.73870887536603291, 0.7998128361456481317 ) ) ;
#138472 = CARTESIAN_POINT ( 'NONE',  ( 3.237364818613055473, 6.998952398349030268, -1.734723475976807094E-15 ) ) ;
#138474 = FILL_AREA_STYLE_COLOUR ( '', #85819 ) ;
#138475 = CARTESIAN_POINT ( 'NONE',  ( 4.183856667257361828, 1.958065582907195568, -0.4948979464895820191 ) ) ;
#138476 = CARTESIAN_POINT ( 'NONE',  ( -1.001543065824772872E-14, 5.071875000341421469, 1.575800808251672791 ) ) ;
#138477 = CARTESIAN_POINT ( 'NONE',  ( 5.916483495826922123, 0.8326555988564422472, 1.887315221659194631 ) ) ;
#138478 = CARTESIAN_POINT ( 'NONE',  ( 9.897088948295946764, 10.64895131587453569, 0.7216878364870438212 ) ) ;
#138479 = CARTESIAN_POINT ( 'NONE',  ( 4.587301040747738590, 1.933109172225886185, -0.9673573668882375909 ) ) ;
#138480 = CARTESIAN_POINT ( 'NONE',  ( 5.027041095616958444, 9.086908054853605421, 0.000000000000000000 ) ) ;
#138481 = CARTESIAN_POINT ( 'NONE',  ( -0.6823417656250246877, -1.136458332991911790, 1.181850606188755259 ) ) ;
#138483 = CARTESIAN_POINT ( 'NONE',  ( 9.452953987210896969, 3.481541100950246381, -7.393264229718174541 ) ) ;
#138482 = CARTESIAN_POINT ( 'NONE',  ( 4.681308178468477799, 8.683552984847038303, 0.000000000000000000 ) ) ;
#138484 = CARTESIAN_POINT ( 'NONE',  ( 7.931156673870037643, 8.355363662377600420, -0.7216878364870267237 ) ) ;
#138486 = CARTESIAN_POINT ( 'NONE',  ( 0.000000000000000000, 6.999999999999999112, -11.00000000000000000 ) ) ;
#138485 = CARTESIAN_POINT ( 'NONE',  ( 1.768284035615394600, -2.154879749829127444, 0.2648707735025003229 ) ) ;
#138488 = CARTESIAN_POINT ( 'NONE',  ( 1.804012939494209267, 1.363607186100148638, -1.237405090928713092 ) ) ;
#138487 = CARTESIAN_POINT ( 'NONE',  ( -4.555176424511596878, 7.297827681030051750, 1.082531754730560403 ) ) ;
#138489 = B_SPLINE_CURVE_WITH_KNOTS ( 'NONE', 3,
 ( #17342, #138595, #141827, #204618 ),
 .UNSPECIFIED., .F., .F.,
 ( 4, 4 ),
 ( 0.000000000000000000, 7.241384396098642291E-05 ),
 .UNSPECIFIED. ) ;
#138490 = CARTESIAN_POINT ( 'NONE',  ( 1.364683531249990311, 3.884375000341417028, 1.214306433183764966E-14 ) ) ;
#138491 = CARTESIAN_POINT ( 'NONE',  ( 3.052458795248469414, -1.657928338269051505, 1.433322580492613296 ) ) ;
#138492 = CARTESIAN_POINT ( 'NONE',  ( 6.983263157960349687, 0.5706719223780298833, 2.105707282093812083 ) ) ;
#138493 = CARTESIAN_POINT ( 'NONE',  ( 3.749113412367131914, -1.851274732041636950, 1.300436299091920045 ) ) ;
#138494 = CARTESIAN_POINT ( 'NONE',  ( -4.720210035852093533, 8.658662141802762946, -0.7998128361456281477 ) ) ;
#138495 = CARTESIAN_POINT ( 'NONE',  ( -1.474414414893459258, 7.826756755319736136, -10.64843978026285320 ) ) ;
#138496 = CARTESIAN_POINT ( 'NONE',  ( 6.491225937077876651, 6.748298437306541331, 0.07656069123261090292 ) ) ;
#138497 = CARTESIAN_POINT ( 'NONE',  ( -1.500000000000015099, 13.97916666666666607, -0.8660254037844309360 ) ) ;
#138498 = CARTESIAN_POINT ( 'NONE',  ( 4.421367491832258523, 8.172362817197399210, 0.7216878364870257245 ) ) ;
#138499 = CARTESIAN_POINT ( 'NONE',  ( 5.800005483916761406, -1.769921774263127912, 0.001416880316495658159 ) ) ;
#138500 = CARTESIAN_POINT ( 'NONE',  ( 8.932124273304774320, 9.315233161810734686, 0.7998128361456462443 ) ) ;
#138501 = CARTESIAN_POINT ( 'NONE',  ( 2.415183150638998466, 1.880743233677120818, 0.9477269459148714992 ) ) ;
#138503 = CARTESIAN_POINT ( 'NONE',  ( -0.7500000000000215383, 0.6916666666666876351, 1.299038105676659116 ) ) ;
#138502 = CARTESIAN_POINT ( 'NONE',  ( 1.364683531249997417, 9.984375000341398021, 2.602085213965210642E-15 ) ) ;
#138504 = CARTESIAN_POINT ( 'NONE',  ( 1.363649640492822668, -0.4818474322187695780, 1.909556114072549882 ) ) ;
#138505 = CARTESIAN_POINT ( 'NONE',  ( -5.307090785106547415, 5.156303768904543894, -0.7998128361456362523 ) ) ;
#138506 = CARTESIAN_POINT ( 'NONE',  ( 0.1858947801188018389, -1.204007190563995078, -1.549573762531175625 ) ) ;
#138508 = ORIENTED_EDGE ( 'NONE', *, *, #208007, .T. ) ;
#138507 = CARTESIAN_POINT ( 'NONE',  ( 5.800986464141828058, -0.2745434460682676936, -1.790553645544520345 ) ) ;
#138509 = CARTESIAN_POINT ( 'NONE',  ( 6.534666852106798096, 7.686494751288491578, -1.082531754730543083 ) ) ;
#138510 = CARTESIAN_POINT ( 'NONE',  ( -1.364683531250014514, -0.9072916663252470482, 0.7879004041258379498 ) ) ;
#138511 = CARTESIAN_POINT ( 'NONE',  ( 4.926551758443063811, 1.790249073151507275, 0.5424879929923772659 ) ) ;
#138512 = CARTESIAN_POINT ( 'NONE',  ( 2.381428537494710618, 5.930083727052461562, 0.7998128361456462443 ) ) ;
#138513 = VERTEX_POINT ( 'NONE', #74136 ) ;
#138514 = CARTESIAN_POINT ( 'NONE',  ( 5.049704560591026237, 1.530381825397047812, 1.394388655583590042 ) ) ;
#138515 = CARTESIAN_POINT ( 'NONE',  ( -0.6125000000000349054, 2.208333333333325932, -1.060881119635983083 ) ) ;
#138516 = CARTESIAN_POINT ( 'NONE',  ( -4.624739795592931912, 8.409630504918133909, -0.7216878364870338292 ) ) ;
#138517 = CARTESIAN_POINT ( 'NONE',  ( 3.278550485571194439, -0.9336338327896769318, -0.8199742731213923719 ) ) ;
#138518 = CARTESIAN_POINT ( 'NONE',  ( 6.968000882419564945, 10.21675256520979858, 1.199719254218460707 ) ) ;
#138519 = CARTESIAN_POINT ( 'NONE',  ( -10.17947440576205054, 10.77047498301088346, 0.7998128361456462443 ) ) ;
#138520 = CARTESIAN_POINT ( 'NONE',  ( 7.452141709366786770, 8.723195411463290583, 1.199719254218452047 ) ) ;
#138521 = B_SPLINE_CURVE_WITH_KNOTS ( 'NONE', 3,
 ( #10925, #77000, #209121, #60759 ),
 .UNSPECIFIED., .F., .F.,
 ( 4, 4 ),
 ( 0.003703980837549441640, 0.004484133753724313387 ),
 .UNSPECIFIED. ) ;
#138522 = CARTESIAN_POINT ( 'NONE',  ( 1.364683531249988757, 0.1343750003414204142, 0.000000000000000000 ) ) ;
#138523 = CARTESIAN_POINT ( 'NONE',  ( -1.402160292154681736E-14, 1.337500000000025446, -1.732050807568863648 ) ) ;
#138525 = CARTESIAN_POINT ( 'NONE',  ( 4.137209430464448445, 7.978494768850520558, 1.040834085586084257E-14 ) ) ;
#138524 = CARTESIAN_POINT ( 'NONE',  ( 4.721123852359588646, -1.751549048416237486, -0.8839179009662299080 ) ) ;
#138526 = CARTESIAN_POINT ( 'NONE',  ( 2.565779641467882399, 1.620934753846922982, -1.198676126143098486 ) ) ;
#138527 = CARTESIAN_POINT ( 'NONE',  ( -6.966220764712148572, 6.002124920821316323, 2.420000000000000373 ) ) ;
#138528 = CARTESIAN_POINT ( 'NONE',  ( 0.5389544483674936215, -1.876709678404146153, 1.131566444868239874 ) ) ;
#138529 = CARTESIAN_POINT ( 'NONE',  ( -11.92619526913700057, 10.19999999999998153, 1.328859060402682868 ) ) ;
#138530 = CARTESIAN_POINT ( 'NONE',  ( 1.844777716111935861, -1.582881869529973562, 0.9963996312925410548 ) ) ;
#138531 = CARTESIAN_POINT ( 'NONE',  ( -1.500000000000001332, -1.318749999317178734, 0.000000000000000000 ) ) ;
#138532 = CARTESIAN_POINT ( 'NONE',  ( 3.779544948098710666, 0.2423517821111692006, -1.998478243804775900 ) ) ;
#138533 = CARTESIAN_POINT ( 'NONE',  ( -7.995557903757128493, 10.35123685918189729, 1.599625672291295375 ) ) ;
#138535 = CARTESIAN_POINT ( 'NONE',  ( 3.128620947210249970, 0.5168888077675163339, 2.053037424179054327 ) ) ;
#138534 = CARTESIAN_POINT ( 'NONE',  ( -5.761852096127856981, 5.824508321678349532, 0.000000000000000000 ) ) ;
#138536 = CARTESIAN_POINT ( 'NONE',  ( 4.562978833902987752, 1.602482145440896399, -1.310924660355553106 ) ) ;
#138537 = CARTESIAN_POINT ( 'NONE',  ( 6.099189001301251523, 8.209082816308541197, 1.599625672291268286 ) ) ;
#138539 = CARTESIAN_POINT ( 'NONE',  ( 6.620655732516618208, 1.260995252412312251, 2.189931766300906801 ) ) ;
#138538 = CARTESIAN_POINT ( 'NONE',  ( 1.312182373965790072, 1.401635355298202379, -1.551525349546636123 ) ) ;
#138541 = EDGE_LOOP ( 'NONE', ( #7151, #14458, #35793, #2797 ) ) ;
#138540 = CARTESIAN_POINT ( 'NONE',  ( 6.422862827026682098, 1.704596635199370880, 0.6539724957527744964 ) ) ;
#138542 = CARTESIAN_POINT ( 'NONE',  ( 7.938462636001388795, 9.220293482545153907, -1.199719254218441611 ) ) ;
#138543 = CARTESIAN_POINT ( 'NONE',  ( 4.000000000000012434, 6.499999999999999112, 0.7500000000000006661 ) ) ;
#138544 = CARTESIAN_POINT ( 'NONE',  ( -11.89204169242383102, 13.79999999999999893, 0.8046421800351404308 ) ) ;
#138545 = AXIS2_PLACEMENT_3D ( 'NONE', #195033, #162549, #28269 ) ;
#138546 = CARTESIAN_POINT ( 'NONE',  ( -9.645001968711920171, 4.042125922905831281, 6.587946042608958663 ) ) ;
#138547 = CARTESIAN_POINT ( 'NONE',  ( 8.093854517234030155, 8.545177812968924869, -0.7216878364870267237 ) ) ;
#138548 = CARTESIAN_POINT ( 'NONE',  ( 1.347111479062088405E-15, 2.000000000000001776, 11.00000000000000000 ) ) ;
#138549 = CARTESIAN_POINT ( 'NONE',  ( 5.901015568784107934, -0.2851453878830525479, -1.890788771128081969 ) ) ;
#138550 = CARTESIAN_POINT ( 'NONE',  ( -6.995117189646935962, 10.24838825697502109, 1.199719254218453823 ) ) ;
#138551 = CARTESIAN_POINT ( 'NONE',  ( 4.632082037363250748, 8.555846143565791095, -0.7998128361456231517 ) ) ;
#138552 = DIRECTION ( 'NONE',  ( 0.7592566023653005702, -0.6507913734559639396, 0.000000000000000000 ) ) ;
#138553 = LINE ( 'NONE', #42130, #82362 ) ;
#138554 = CARTESIAN_POINT ( 'NONE',  ( 4.304877467538922531, 4.981110786005563007, 1.199719254218464037 ) ) ;
#138555 = VERTEX_POINT ( 'NONE', #37353 ) ;
#138556 = ADVANCED_FACE ( 'NONE', ( #185720 ), #124038, .T. ) ;
#138557 = CIRCLE ( 'NONE', #62480, 10.99999999999999112 ) ;
#138558 = EDGE_CURVE ( 'NONE', #19519, #106155, #203613, .T. ) ;
#138559 = CARTESIAN_POINT ( 'NONE',  ( 6.239861269555550649, 2.010826412442122013, -0.1511553674920090573 ) ) ;
#138560 = CARTESIAN_POINT ( 'NONE',  ( -0.07933194154488883154, -9.746166700180788567, -9.499668754385620417 ) ) ;
#138561 = CARTESIAN_POINT ( 'NONE',  ( 0.9630212455657579662, -7.887518224194900737E-15, -0.8538729164882093992 ) ) ;
#138562 = CARTESIAN_POINT ( 'NONE',  ( -6.482157434489847603, 6.770256554395555959, 0.2388210531332583819 ) ) ;
#138563 = CARTESIAN_POINT ( 'NONE',  ( -6.249945626219832739, 6.393950773452325542, 1.040834085586084257E-14 ) ) ;
#138564 = CARTESIAN_POINT ( 'NONE',  ( 4.356247428692526569, 3.976710176429713250, 0.7998128361456341429 ) ) ;
#138565 = CARTESIAN_POINT ( 'NONE',  ( 3.239063133055252841, -0.1400698962470778297, -1.964493882382233991 ) ) ;
#138566 = CARTESIAN_POINT ( 'NONE',  ( 4.816029892389546596, 1.034148959857810190, -1.730877356967218894 ) ) ;
#138567 = CARTESIAN_POINT ( 'NONE',  ( -7.528855374290365887, 7.678086112960552434, -0.7998128361456291469 ) ) ;
#138568 = CARTESIAN_POINT ( 'NONE',  ( -10.96384327792182134, -7.754568858751050620, 0.4817895937885991464 ) ) ;
#138569 = CARTESIAN_POINT ( 'NONE',  ( 4.523480939507462217, -1.347072049868164978, -1.728447516733351952 ) ) ;
#138570 = CARTESIAN_POINT ( 'NONE',  ( 2.872000511136533873, 1.029149822700244465, 1.628267440728261573 ) ) ;
#138571 = CARTESIAN_POINT ( 'NONE',  ( -9.169391961543940539, 9.592045464756413509, 1.040834085586084257E-14 ) ) ;
#138572 = CARTESIAN_POINT ( 'NONE',  ( -0.02968770228137588424, 4.095675376368371090, -2.381331788581673159 ) ) ;
#138573 = CARTESIAN_POINT ( 'NONE',  ( 0.03028722099337673168, -1.361824662662258767, -1.737358624739212321 ) ) ;
#138574 =( NAMED_UNIT ( * ) SI_UNIT ( $, .STERADIAN. ) SOLID_ANGLE_UNIT ( ) );
#138575 = CARTESIAN_POINT ( 'NONE',  ( 0.6823417656249969321, 13.27604166700806232, -1.181850606188757036 ) ) ;
#138576 = CARTESIAN_POINT ( 'NONE',  ( 4.462605117192430804, 8.358123070033169455, 1.040834085586084257E-14 ) ) ;
#138577 = ORIENTED_EDGE ( 'NONE', *, *, #141509, .T. ) ;
#138578 = CARTESIAN_POINT ( 'NONE',  ( 5.736508392357904107, 5.865217010605237924, 0.000000000000000000 ) ) ;
#138579 = ORIENTED_EDGE ( 'NONE', *, *, #168152, .T. ) ;
#138580 = EDGE_LOOP ( 'NONE', ( #103059, #72594, #115040, #2616 ) ) ;
#138582 = CARTESIAN_POINT ( 'NONE',  ( 2.526041439118778431, -1.990860190764773829, 0.2976642988744558904 ) ) ;
#138581 = CARTESIAN_POINT ( 'NONE',  ( 0.8021671156859496721, 1.469769370800941166, -1.269469122775281456 ) ) ;
#138583 = CARTESIAN_POINT ( 'NONE',  ( 5.132278277959533064, 0.2326997901972542582, -2.286600633956968220 ) ) ;
#138585 = CARTESIAN_POINT ( 'NONE',  ( 3.291705155655884951, -1.246473628130102762, -1.382024748694546501 ) ) ;
#138584 = CARTESIAN_POINT ( 'NONE',  ( -7.014364370223741929, 9.276787413384745662, -1.599625672291271394 ) ) ;
#138586 = CARTESIAN_POINT ( 'NONE',  ( 7.095713291905693332, 9.371694488680407886, 1.599625672291268286 ) ) ;
#138587 = FACE_BOUND ( 'NONE', #59827, .T. ) ;
#138588 = CARTESIAN_POINT ( 'NONE',  ( 6.222915752822945734, 1.412394824171304908, -1.289504995239741714 ) ) ;
#138589 = CARTESIAN_POINT ( 'NONE',  ( -7.691553217654356622, 7.867900263551875994, -0.7998128361456291469 ) ) ;
#138590 = CARTESIAN_POINT ( 'NONE',  ( -5.506019780925599960, 5.596313630600862510, 0.7216878364870257245 ) ) ;
#138591 = CARTESIAN_POINT ( 'NONE',  ( 5.513254163946260000, -2.039523011555996579, 0.4591751592910776614 ) ) ;
#138592 = CARTESIAN_POINT ( 'NONE',  ( 6.155038550924155416, 6.283225852274053835, 0.7216878364870317197 ) ) ;
#138593 = VERTEX_POINT ( 'NONE', #203031 ) ;
#138594 = EDGE_CURVE ( 'NONE', #21883, #87431, #141213, .T. ) ;
#138595 = CARTESIAN_POINT ( 'NONE',  ( 3.046854503059200248, 2.800000000000017586, -2.499999999999995115 ) ) ;
#138596 = CARTESIAN_POINT ( 'NONE',  ( 0.9436603434208358232, 0.7422609627109194586, -1.668170528445270140 ) ) ;
#138597 = CARTESIAN_POINT ( 'NONE',  ( -5.922214171070950606, 5.803671375871217286, -0.7998128361456291469 ) ) ;
#138598 =( GEOMETRIC_REPRESENTATION_CONTEXT ( 3 ) GLOBAL_UNCERTAINTY_ASSIGNED_CONTEXT ( ( #167343 ) ) GLOBAL_UNIT_ASSIGNED_CONTEXT ( ( #171423, #73927, #6765 ) ) REPRESENTATION_CONTEXT ( 'NONE', 'WORKASPACE' ) );
#138599 = CARTESIAN_POINT ( 'NONE',  ( 2.162404540820038967, 1.068076967457934012, 1.366050734290222834 ) ) ;
#138600 =( NAMED_UNIT ( * ) PLANE_ANGLE_UNIT ( ) SI_UNIT ( $, .RADIAN. ) );
#138601 = CARTESIAN_POINT ( 'NONE',  ( -7.203459687562382641, 7.298457811777897319, -0.7998128361456291469 ) ) ;
#138602 = CARTESIAN_POINT ( 'NONE',  ( -5.805552323418545768, 6.064174366559389462, -0.5408148663509839693 ) ) ;
#138603 = CARTESIAN_POINT ( 'NONE',  ( 0.4267348894952603944, -1.354911996285239617, 1.565345633960464111 ) ) ;
#138604 = CARTESIAN_POINT ( 'NONE',  ( 5.092344371507952161, -1.812320225013038133, -0.2200062734805732223 ) ) ;
#138605 = CARTESIAN_POINT ( 'NONE',  ( 3.151168776707893748, 1.684956273983062580, -1.004420888743910334 ) ) ;
#138606 = CARTESIAN_POINT ( 'NONE',  ( 1.224999999999974998, -0.3333333326504774874, 0.7072540797572697269 ) ) ;
#138607 = CARTESIAN_POINT ( 'NONE',  ( -9.612894607289142357, 11.17379744904754801, -1.199719254218441611 ) ) ;
#138608 = CARTESIAN_POINT ( 'NONE',  ( 6.262976894508937242, 9.394224579314053969, -1.199719254218440723 ) ) ;
#138609 = CARTESIAN_POINT ( 'NONE',  ( 4.213620120093874988, 1.703795446819071691, 1.262174061880352083 ) ) ;
#138610 = CARTESIAN_POINT ( 'NONE',  ( -0.3000000000000097589, 3.214163249644239606, 0.5238375172406791735 ) ) ;
#138611 = CARTESIAN_POINT ( 'NONE',  ( -9.541187415715041809, 12.15447128979948310, -1.599625672291263179 ) ) ;
#138612 = CARTESIAN_POINT ( 'NONE',  ( 2.149362472714404504, 1.803301116200561882, -1.016697834320609894 ) ) ;
#138614 = CARTESIAN_POINT ( 'NONE',  ( -1.402160292154681736E-14, -1.115624999658584082, 1.575800808251672791 ) ) ;
#138613 = CARTESIAN_POINT ( 'NONE',  ( -11.96212011828584210, 11.32812445049947669, 0.9569185076417884295 ) ) ;
#138616 = VERTEX_POINT ( 'NONE', #154316 ) ;
#138615 = CARTESIAN_POINT ( 'NONE',  ( 4.143395664610330265, 0.1093779850947790705, 2.218736840405158173 ) ) ;
#138617 = CARTESIAN_POINT ( 'NONE',  ( 1.899501351379283554, -1.088314401552924249, -2.024763765589305820 ) ) ;
#138619 = CARTESIAN_POINT ( 'NONE',  ( 6.192244813941197634, 1.021713635409545073, -1.791695130993501417 ) ) ;
#138618 = CARTESIAN_POINT ( 'NONE',  ( 8.256552361042350796, 12.57646882128404187, 1.040834085586084257E-14 ) ) ;
#138621 = CARTESIAN_POINT ( 'NONE',  ( -1.737499999999997824, -0.2916666666666657415, 3.009438278150925683 ) ) ;
#138620 = CARTESIAN_POINT ( 'NONE',  ( 4.146814880933355596, 5.931313009212638931, 1.599625672291261402 ) ) ;
#138622 = CARTESIAN_POINT ( 'NONE',  ( 6.269096963164666469, 1.759884223096353173, -0.5412972069449849544 ) ) ;
#138623 = VERTEX_POINT ( 'NONE', #173794 ) ;
#138624 = CARTESIAN_POINT ( 'NONE',  ( 0.000000000000000000, -0.9200000000000041478, 0.000000000000000000 ) ) ;
#138625 = EDGE_CURVE ( 'NONE', #113056, #183752, #5370, .T. ) ;
#138626 = CARTESIAN_POINT ( 'NONE',  ( 3.269685606991072468, 0.4601866041431811327, -1.856093204100267124 ) ) ;
#138627 = CARTESIAN_POINT ( 'NONE',  ( -0.1106727585415837045, 2.018984206239351042, -2.418200238751634146 ) ) ;
#138628 = CARTESIAN_POINT ( 'NONE',  ( 3.627714610788032701, -1.027129601966117134, -1.385419451709940519 ) ) ;
#138629 = CARTESIAN_POINT ( 'NONE',  ( 2.694546298722868549, 1.457235452327232395, -1.394086077981852911 ) ) ;
#138630 =( BOUNDED_CURVE ( )  B_SPLINE_CURVE ( 2, ( #32849, #134645, #102112, #130434, #149808, #166048, #180171, #131467, #168182 ),
 .UNSPECIFIED., .F., .T. ) 
 B_SPLINE_CURVE_WITH_KNOTS ( ( 3, 2, 2, 2, 3 ),
 ( 0.4732142857142856984, 0.4761904761904761640, 0.4821428571428571508, 0.4880952380952380820, 0.4910714285714285476 ),
 .UNSPECIFIED. ) 
 CURVE ( )  GEOMETRIC_REPRESENTATION_ITEM ( )  RATIONAL_B_SPLINE_CURVE ( ( 0.9330127018922194093, 0.9330127018922194093, 1.000000000000000000, 0.8660254037844387076, 1.000000000000000000, 0.8660254037844387076, 1.000000000000000000, 0.9330127018922199644, 0.9330127018922194093 ) ) 
 REPRESENTATION_ITEM ( '' )  );
#138631 = CARTESIAN_POINT ( 'NONE',  ( 3.551692777231782561, -1.542557649656286944, 1.704429084079077006 ) ) ;
#138632 = CARTESIAN_POINT ( 'NONE',  ( 3.603020308667020277, 1.786206176199186535, -1.388445577547703369 ) ) ;
#138633 = CARTESIAN_POINT ( 'NONE',  ( 0.06543086261080394150, -1.973449318085427340, -0.9880335165917543128 ) ) ;
#138634 = CARTESIAN_POINT ( 'NONE',  ( -4.800995793014949165, 8.615262501910491366, 0.7216878364870267237 ) ) ;
#138635 = ORIENTED_EDGE ( 'NONE', *, *, #118861, .T. ) ;
#138636 = CARTESIAN_POINT ( 'NONE',  ( 4.692510491889085422, -0.3870912556891945577, -1.726709192852653230 ) ) ;
#138638 = CARTESIAN_POINT ( 'NONE',  ( 1.025772235718758196, -1.457823864038493733, -1.768965695191491827 ) ) ;
#138637 = CARTESIAN_POINT ( 'NONE',  ( 6.933015448541703485, 9.181880338089085214, 1.599625672291268286 ) ) ;
#138639 = CARTESIAN_POINT ( 'NONE',  ( 5.419803763747102821, 1.093575605593154920, -1.481025086994464113 ) ) ;
#138640 = CARTESIAN_POINT ( 'NONE',  ( -2.788173145904702555, 6.404619103530779789, -0.7998128361456281477 ) ) ;
#138641 = CARTESIAN_POINT ( 'NONE',  ( 5.507841377412062478, -0.9828142975771281264, -1.958786091674463714 ) ) ;
#138642 = CARTESIAN_POINT ( 'NONE',  ( -4.980641328173854632, 6.904110530993182948, 1.599625672291263179 ) ) ;
#138643 = CARTESIAN_POINT ( 'NONE',  ( -4.810445574750349174, 4.506608013497163334, 0.7998128361456341429 ) ) ;
#138644 = CARTESIAN_POINT ( 'NONE',  ( -5.577069096748362043, 15.51842150349689042, 10.63472584745987426 ) ) ;
#138645 = EDGE_CURVE ( 'NONE', #4590, #13599, #126249, .T. ) ;
#138646 = CARTESIAN_POINT ( 'NONE',  ( 6.232888004217203459, -1.964670499678453197, -0.6532144590316590893 ) ) ;
#138647 = CARTESIAN_POINT ( 'NONE',  ( 0.4269707148552639997, -1.727061408318403712, 1.040797348915108111 ) ) ;
#138648 = CARTESIAN_POINT ( 'NONE',  ( 0.6823417656249899377, 5.676041667008087543, -1.181850606188754593 ) ) ;
#138649 = CARTESIAN_POINT ( 'NONE',  ( 4.072816532378962684, -1.798017144868354178, -0.6922151418781684606 ) ) ;
#138650 = CARTESIAN_POINT ( 'NONE',  ( -1.364683531250000748, 10.35937500034139802, 0.000000000000000000 ) ) ;
#138651 = CARTESIAN_POINT ( 'NONE',  ( -3.958617665510283601, 4.681104033592509595, -1.082531754730549967 ) ) ;
#138652 = CARTESIAN_POINT ( 'NONE',  ( 0.6861347341944658007, 2.138861475627896080, -0.5996866306409093239 ) ) ;
#138654 = ORIENTED_EDGE ( 'NONE', *, *, #68346, .F. ) ;
#138653 = CARTESIAN_POINT ( 'NONE',  ( 0.000000000000000000, -7.666862915010147717, 0.000000000000000000 ) ) ;
#138656 = CARTESIAN_POINT ( 'NONE',  ( 0.000000000000000000, 11.29999999999999893, 0.000000000000000000 ) ) ;
#138655 = CARTESIAN_POINT ( 'NONE',  ( 1.451998047839290207, 7.315968950356647404, -4.301760722583974683 ) ) ;
#138657 = CARTESIAN_POINT ( 'NONE',  ( 10.53876547652418338, 11.18964789890005918, 0.7998128361456462443 ) ) ;
#138658 = CARTESIAN_POINT ( 'NONE',  ( -3.917943204224914933, 6.554388924028945240, -1.082531754730548412 ) ) ;
#138659 = CARTESIAN_POINT ( 'NONE',  ( 11.86239285000045740, 11.37999999999999901, -1.812080536912752837 ) ) ;
#138660 = LINE ( 'NONE', #203612, #92404 ) ;
#138661 = CARTESIAN_POINT ( 'NONE',  ( 8.527715432871318058, 12.89282573841782664, -0.7216878364870338292 ) ) ;
#138662 = CARTESIAN_POINT ( 'NONE',  ( 0.9593383959572501229, 1.601786533887459507, 1.132500672181527168 ) ) ;
#138663 = CARTESIAN_POINT ( 'NONE',  ( -1.364683531250000748, 2.321875000341422357, 1.214306433183764966E-14 ) ) ;
#138664 = CARTESIAN_POINT ( 'NONE',  ( 11.89835103415199313, 12.27106914167532103, 1.561208891256346876 ) ) ;
#138665 = CARTESIAN_POINT ( 'NONE',  ( 6.654749070045313353, -0.5220710138904552933, -1.891073168474053823 ) ) ;
#138666 = CARTESIAN_POINT ( 'NONE',  ( -9.481229494658258261, 9.955855920056455588, -0.7998128361456291469 ) ) ;
#138667 =( GEOMETRIC_REPRESENTATION_CONTEXT ( 3 ) GLOBAL_UNCERTAINTY_ASSIGNED_CONTEXT ( ( #147173 ) ) GLOBAL_UNIT_ASSIGNED_CONTEXT ( ( #131230, #68265, #33653 ) ) REPRESENTATION_CONTEXT ( 'NONE', 'WORKASPACE' ) );
#138668 = CARTESIAN_POINT ( 'NONE',  ( -4.894130264408866893, 6.732904613275549899, -1.443375672974051449 ) ) ;
#138669 = B_SPLINE_CURVE_WITH_KNOTS ( 'NONE', 3,
 ( #158825, #191298, #189184, #76493 ),
 .UNSPECIFIED., .F., .F.,
 ( 4, 4 ),
 ( 0.000000000000000000, 0.0003110688635154432429 ),
 .UNSPECIFIED. ) ;
#138670 = CARTESIAN_POINT ( 'NONE',  ( 0.1107634673921135821, -0.9696846621911526798, -2.041722876818732324 ) ) ;
#138672 = EDGE_LOOP ( 'NONE', ( #125311, #25745, #49560, #190794 ) ) ;
#138671 = CARTESIAN_POINT ( 'NONE',  ( -4.543954038874438162, 8.453030145328826350, 1.040834085586084257E-14 ) ) ;
#138673 = CARTESIAN_POINT ( 'NONE',  ( -1.500000000000015099, -0.7979166659838445863, 0.8660254037844403729 ) ) ;
#138674 = CARTESIAN_POINT ( 'NONE',  ( 1.211929638205839765, -0.8359089839212189288, -1.673436591668895579 ) ) ;
#138675 = CARTESIAN_POINT ( 'NONE',  ( -0.1347034368660744441, -0.1421164721313403212, -1.704521202080215847 ) ) ;
#138676 = EDGE_CURVE ( 'NONE', #30492, #204725, #19680, .T. ) ;
#138678 = CARTESIAN_POINT ( 'NONE',  ( 4.423480980095358284, -1.348712413769267426, -1.727291790683552541 ) ) ;
#138677 = CARTESIAN_POINT ( 'NONE',  ( 1.360316468749943608, 1.494791667008105174, 0.7853790794158439503 ) ) ;
#138679 = CARTESIAN_POINT ( 'NONE',  ( 4.559805550777903171, 0.5102292677348593264, -2.250327227043275702 ) ) ;
#138680 = CARTESIAN_POINT ( 'NONE',  ( 6.538362368396775537, 2.037695317216736246, 0.3068575337649599444 ) ) ;
#138681 = CARTESIAN_POINT ( 'NONE',  ( 1.921723552510564259, 1.118073055411296313, -1.587613466820477992 ) ) ;
#138682 = CARTESIAN_POINT ( 'NONE',  ( -5.056828107772860292, 6.922718763866881453, -1.443375672974051449 ) ) ;
#138683 = EDGE_CURVE ( 'NONE', #146171, #190376, #154161, .T. ) ;
#138684 = SURFACE_STYLE_USAGE ( .BOTH. , #41189 ) ;
#138685 = CARTESIAN_POINT ( 'NONE',  ( 3.716343503921665459, 6.389465617000312569, -1.082531754730549967 ) ) ;
#138686 = CARTESIAN_POINT ( 'NONE',  ( 1.249999999999822364, 10.00000000000000178, 4.154462424328221104 ) ) ;
#138687 = CARTESIAN_POINT ( 'NONE',  ( 3.270157880292836605, 1.821742160604752137, -0.8647241845514613834 ) ) ;
#138688 = CARTESIAN_POINT ( 'NONE',  ( -5.382223794500852421, 5.381608636446842731, -0.7216878364870197293 ) ) ;
#138689 = CARTESIAN_POINT ( 'NONE',  ( 4.540400682753764627, 6.905156770093001661, -1.249999994511372448 ) ) ;
#138690 = CARTESIAN_POINT ( 'NONE',  ( 11.86145016429272836, 13.40000000000000036, 1.179999999999997051 ) ) ;
#138691 = CARTESIAN_POINT ( 'NONE',  ( 1.013953575274041619, -0.8186894766500467657, -1.631917417583013341 ) ) ;
#138692 = CARTESIAN_POINT ( 'NONE',  ( -7.123883369337781879, 7.275895117174344229, 0.7998128361456341429 ) ) ;
#138693 = CARTESIAN_POINT ( 'NONE',  ( -4.468294144155606773, 7.370704380560280100, 1.199719254218452935 ) ) ;
#138694 = CARTESIAN_POINT ( 'NONE',  ( -11.25552992593869206, 3.531787801817266370, 5.933966561491729408 ) ) ;
#138695 = EDGE_LOOP ( 'NONE', ( #31744, #178847, #100176, #29057 ) ) ;
#138696 = CARTESIAN_POINT ( 'NONE',  ( 5.559468503951485729, 0.4043298029084033685, -2.020654889403751486 ) ) ;
#138697 = CARTESIAN_POINT ( 'NONE',  ( -6.631346530415505036, 7.869564052640446228, 1.082531754730549078 ) ) ;
#138698 = CARTESIAN_POINT ( 'NONE',  ( 7.146556367734764770, 9.431011410480991231, 1.443375672974063439 ) ) ;
#138699 = CARTESIAN_POINT ( 'NONE',  ( -4.253507506385335368, 5.985511395581417204, 1.599625672291267398 ) ) ;
#138700 = CARTESIAN_POINT ( 'NONE',  ( -8.272446282632566650, 12.80293776304669962, 0.7998128361456481317 ) ) ;
#138701 = CARTESIAN_POINT ( 'NONE',  ( 5.936196224836090884, -1.123750473735840361, -1.677956830082157236 ) ) ;
#138703 = VERTEX_POINT ( 'NONE', #188938 ) ;
#138702 = CARTESIAN_POINT ( 'NONE',  ( 5.619863295618399590, -0.5416267994347803150, 2.154155341088887177 ) ) ;
#138704 = CARTESIAN_POINT ( 'NONE',  ( -5.015590482412729756, 4.816220082428420923, 0.000000000000000000 ) ) ;
#138705 = CARTESIAN_POINT ( 'NONE',  ( 5.120175567455225618, 9.125288595339771547, -0.7998128361456281477 ) ) ;
#138706 = AXIS2_PLACEMENT_3D ( 'NONE', #115413, #51419, #99109 ) ;
#138707 = CARTESIAN_POINT ( 'NONE',  ( 4.346593572148568896, 0.5479209435249388083, 1.986652789453833057 ) ) ;
#138708 = CARTESIAN_POINT ( 'NONE',  ( 3.621720349255663773, 0.2986264320336135536, 1.994071497604548382 ) ) ;
#138709 = ORIENTED_EDGE ( 'NONE', *, *, #11469, .T. ) ;
#138710 = CARTESIAN_POINT ( 'NONE',  ( -15.75000000000000000, 13.79999999999998295, 3.199999999999997957 ) ) ;
#138711 = CARTESIAN_POINT ( 'NONE',  ( 2.205172540517054802, 5.724451730578533848, 1.040834085586084257E-14 ) ) ;
#138713 = VERTEX_POINT ( 'NONE', #106683 ) ;
#138712 = CARTESIAN_POINT ( 'NONE',  ( -6.363572996767778100, 8.517530811019446091, -1.599625672291271394 ) ) ;
#138714 = CARTESIAN_POINT ( 'NONE',  ( 4.893454165248502186, 8.027304163657891678, -0.9628252682179049282 ) ) ;
#138715 = CARTESIAN_POINT ( 'NONE',  ( 3.778672575519220977, -1.986742196792599335, 0.3418835855632795795 ) ) ;
#138716 = CARTESIAN_POINT ( 'NONE',  ( 3.837712106225504183, 1.832433245109680531, 0.1787696065849928018 ) ) ;
#138717 = CARTESIAN_POINT ( 'NONE',  ( 6.392116398765105956, 6.567141947924169720, 2.438447736777272112 ) ) ;
#138718 = CARTESIAN_POINT ( 'NONE',  ( 1.840857126529979126, 2.283052885565831858, 0.3356036407394235033 ) ) ;
#138719 = CARTESIAN_POINT ( 'NONE',  ( 5.083381250481017410, 4.895309311841474553, 0.7998128361456352531 ) ) ;
#138720 = CARTESIAN_POINT ( 'NONE',  ( 3.304151629394710632, -2.159270932758147854, 0.1024373671053082913 ) ) ;
#138721 = CARTESIAN_POINT ( 'NONE',  ( 7.099665995050449041, 11.43469409420089455, 0.7998128361456462443 ) ) ;
#138722 = CARTESIAN_POINT ( 'NONE',  ( -5.250031796989778066, 7.148123067953287446, 1.599625672291267398 ) ) ;
#138723 = AXIS2_PLACEMENT_3D ( 'NONE', #161471, #209109, #157200 ) ;
#138724 = CARTESIAN_POINT ( 'NONE',  ( 3.567963868821962592, 1.814363981409074844, -1.410851157308941506 ) ) ;
#138725 = CARTESIAN_POINT ( 'NONE',  ( 8.014278199453780616, 8.522615118883788199, 0.000000000000000000 ) ) ;
#138726 = CARTESIAN_POINT ( 'NONE',  ( 2.078771448894382701, -0.08914341469279044028, -1.868647664167771616 ) ) ;
#138727 = CARTESIAN_POINT ( 'NONE',  ( 6.368046306259418365, 1.013251383440600284, 1.691012432383535602 ) ) ;
#138729 = CARTESIAN_POINT ( 'NONE',  ( -5.887983850084758330, 10.09134126839936840, 0.7998128361456291469 ) ) ;
#138728 = CARTESIAN_POINT ( 'NONE',  ( -1.364683531249997417, 4.259375000341424133, 1.214306433183764966E-14 ) ) ;
#138731 = CARTESIAN_POINT ( 'NONE',  ( 1.805583701156989518, 1.836052299496168771, 1.224139149458243425 ) ) ;
#138730 = CARTESIAN_POINT ( 'NONE',  ( -4.550733115681270036, 8.460939068270139529, 0.7998128361456481317 ) ) ;
#138732 = CARTESIAN_POINT ( 'NONE',  ( -2.680403734648525216, 0.4910177078054965838, -0.09999999999832666353 ) ) ;
#138733 = CARTESIAN_POINT ( 'NONE',  ( 4.656335691289526402, 7.519809842224722374, -1.199719254218452047 ) ) ;
#138734 = CARTESIAN_POINT ( 'NONE',  ( -5.271422797614987665, 5.044414773505913274, -0.7998128361456221525 ) ) ;
#138735 = CARTESIAN_POINT ( 'NONE',  ( -1.298432343300637860E-14, 2.519999999999999130, -2.000000000000000000 ) ) ;
#138736 = CARTESIAN_POINT ( 'NONE',  ( 6.297732458894883756, -0.6644727202288897017, 1.856229495857963263 ) ) ;
#138737 = CARTESIAN_POINT ( 'NONE',  ( 6.182281242350501138, -1.240197753460486663, 1.945954285860839850 ) ) ;
#138738 = CARTESIAN_POINT ( 'NONE',  ( 0.2913577194270203785, -1.795273245208812485, 0.7915465721433642132 ) ) ;
#138739 = CARTESIAN_POINT ( 'NONE',  ( 2.536046341495324707, 1.265347977242038402, 1.628790341535201636 ) ) ;
#138740 = CARTESIAN_POINT ( 'NONE',  ( 5.992340707560151358, 8.014150130285418783, 1.443375672974062551 ) ) ;
#138741 = CARTESIAN_POINT ( 'NONE',  ( 5.996449078994045223, 10.21788403546024782, 0.7998128361456331437 ) ) ;
#138742 = CARTESIAN_POINT ( 'NONE',  ( 7.090551149822735155, 9.295395646258437949, 1.443375672974076540 ) ) ;
#138743 = CARTESIAN_POINT ( 'NONE',  ( -0.6823417656250212460, 3.363541667008085323, 1.181850606188767472 ) ) ;
#138744 = CARTESIAN_POINT ( 'NONE',  ( -9.367496997647986490, 14.53091781611831834, 7.499999999937057460 ) ) ;
#138745 = CARTESIAN_POINT ( 'NONE',  ( 4.867013957181530515, 5.740899707208986236, -1.082531754730548412 ) ) ;
#138746 = CARTESIAN_POINT ( 'NONE',  ( 5.107971825378077924, 0.6857059611327814830, -2.060108355502160649 ) ) ;
#138748 = CARTESIAN_POINT ( 'NONE',  ( 4.634224865634020141, 0.3196297827482602050, 1.813140464320086132 ) ) ;
#138747 = CARTESIAN_POINT ( 'NONE',  ( 6.539320575229249144, 0.007148032025052972194, 1.896977914940492393 ) ) ;
#138749 = CARTESIAN_POINT ( 'NONE',  ( 9.521443730523927229, -8.144690279336728622, -0.3123298761244219790 ) ) ;
#138750 = CARTESIAN_POINT ( 'NONE',  ( 1.981451431469405389, 3.479816182765795851, 0.4617787996151190288 ) ) ;
#138751 = DIRECTION ( 'NONE',  ( 0.000000000000000000, 0.000000000000000000, 1.000000000000000000 ) ) ;
#138752 = CARTESIAN_POINT ( 'NONE',  ( 0.4041009963523278237, -0.6015683965250936405, 2.180870993196832419 ) ) ;
#138753 = CARTESIAN_POINT ( 'NONE',  ( -4.849785647588779725, 6.920107565692508622, 1.442884047295606820 ) ) ;
#138754 = CARTESIAN_POINT ( 'NONE',  ( -0.1054627972275519465, 3.385846599571567417, -2.076146368081344118 ) ) ;
#138755 = CARTESIAN_POINT ( 'NONE',  ( 6.410638904775656677, 6.895589754593423493, 0.7569561588358000304 ) ) ;
#138756 = CARTESIAN_POINT ( 'NONE',  ( 0.2055213853429035953, 1.417038256915002181, 1.284265443176696442 ) ) ;
#138757 = AXIS2_PLACEMENT_3D ( 'NONE', #80844, #161026, #129679 ) ;
#138758 = CARTESIAN_POINT ( 'NONE',  ( 2.008344819247428248, 1.313797796480600244, -1.186068062872788209 ) ) ;
#138759 = AXIS2_PLACEMENT_3D ( 'NONE', #32406, #33463, #149353 ) ;
#138760 = CARTESIAN_POINT ( 'NONE',  ( 0.1000639402851908749, -0.9014739813196898099, 1.686438745833309438 ) ) ;
#138762 = CARTESIAN_POINT ( 'NONE',  ( 3.603066768525709396, -0.1374138116273740384, 1.910719597520103896 ) ) ;
#138761 = CARTESIAN_POINT ( 'NONE',  ( -10.49131193887636826, 11.13428543831092909, 1.040834085586084257E-14 ) ) ;
#138763 = VECTOR ( 'NONE', #127813, 1000.000000000000000 ) ;
#138764 = CARTESIAN_POINT ( 'NONE',  ( 4.316829372628319561, -1.460888098903726728, 1.321172513512254065 ) ) ;
#138765 = CARTESIAN_POINT ( 'NONE',  ( -0.03470293633787284449, -1.699275230904277789, 1.268407768021381221 ) ) ;
#138766 = CARTESIAN_POINT ( 'NONE',  ( -1.500000000000015099, 10.97916666666666785, -0.8660254037844309360 ) ) ;
#138767 = CARTESIAN_POINT ( 'NONE',  ( 2.641296366799699147, -1.384790685969448099, -1.257831364775918503 ) ) ;
#138769 = VERTEX_POINT ( 'NONE', #87171 ) ;
#138768 = CARTESIAN_POINT ( 'NONE',  ( 6.322847717702526182, 1.612277268089978621, 0.6135241758537502976 ) ) ;
#138771 = CARTESIAN_POINT ( 'NONE',  ( 3.334942599281629949, 5.874221551595115720, -1.082531754730543083 ) ) ;
#138770 = CARTESIAN_POINT ( 'NONE',  ( 2.825073394047578734, 2.078234123670623212, 0.7428476018367863309 ) ) ;
#138772 = CARTESIAN_POINT ( 'NONE',  ( -1.201851678989727383E-14, 3.759375000341422801, -1.575800808251660134 ) ) ;
#138773 = CARTESIAN_POINT ( 'NONE',  ( 6.877413162628407406, -0.1429737755889188000, 1.930079329684093237 ) ) ;
#138774 = CARTESIAN_POINT ( 'NONE',  ( 6.740374924288304648, 11.01552117831172062, 1.040834085586084257E-14 ) ) ;
#138775 = CARTESIAN_POINT ( 'NONE',  ( -9.561524646135538319, 12.17819805862340310, -1.599625672291263179 ) ) ;
#138776 = CARTESIAN_POINT ( 'NONE',  ( 0.1747926744264660381, 0.006858446013176254172, -1.855468577918440776 ) ) ;
#138777 = CARTESIAN_POINT ( 'NONE',  ( -4.475070042639309520, 5.445751865460756846, 1.284222742053057642 ) ) ;
#138778 = CARTESIAN_POINT ( 'NONE',  ( -7.721398836998401016, -6.134628647623487474, -7.721398836998358384 ) ) ;
#138779 = VERTEX_POINT ( 'NONE', #157532 ) ;
#138780 = CARTESIAN_POINT ( 'NONE',  ( 3.332542965736586371, -1.235447621225284509, 1.661183390374972424 ) ) ;
#138781 = CARTESIAN_POINT ( 'NONE',  ( -1.201851678989727383E-14, 3.337500000000019007, -1.732050807568863648 ) ) ;
#138782 = CARTESIAN_POINT ( 'NONE',  ( 4.985647801523278133, 6.839675073242382553, -1.599625672291256295 ) ) ;
#138783 = CARTESIAN_POINT ( 'NONE',  ( -6.605427497552981642, 6.764401258476403278, 0.1916688254133581959 ) ) ;
#138784 = CARTESIAN_POINT ( 'NONE',  ( 0.3990893844944528590, -0.2493554465154389221, -2.004162882155545056 ) ) ;
#138785 =( LENGTH_UNIT ( ) NAMED_UNIT ( * ) SI_UNIT ( .MILLI., .METRE. ) );
#138786 = CARTESIAN_POINT ( 'NONE',  ( 0.6823417656249899377, 3.676041667008085767, -1.181850606188754593 ) ) ;
#138788 = CARTESIAN_POINT ( 'NONE',  ( 8.595506201384008449, 11.05117653974661529, 1.443375672974076540 ) ) ;
#138787 = CARTESIAN_POINT ( 'NONE',  ( 0.1749903794560384862, 2.035240947854660920, -2.372290655319588382 ) ) ;
#138789 = CARTESIAN_POINT ( 'NONE',  ( 5.729842239849809893, -1.821464125411855983, -0.8645900286049985617 ) ) ;
#138790 = CARTESIAN_POINT ( 'NONE',  ( 5.419116407314492179, -1.729028094342921706, 0.8252531017051125684 ) ) ;
#138791 = CARTESIAN_POINT ( 'NONE',  ( 6.539320575229280230, 7.629137130509070275, 2.703262396134015866 ) ) ;
#138792 = CARTESIAN_POINT ( 'NONE',  ( 3.702820756938397295, 1.880440254450808757, 1.125299312022425280 ) ) ;
#138793 = CARTESIAN_POINT ( 'NONE',  ( 1.499999999999989120, 2.285416667349482012, 0.8660254037844524744 ) ) ;
#138794 = CARTESIAN_POINT ( 'NONE',  ( 2.461071540317420148, -1.587761714688112002, 1.065645112462119570 ) ) ;
#138795 = CARTESIAN_POINT ( 'NONE',  ( -4.367698041896780126, 8.247398148854895084, 0.7998128361456481317 ) ) ;
#138796 = CARTESIAN_POINT ( 'NONE',  ( 3.999292125906899198, 6.649295999324608353, 1.082531754730558626 ) ) ;
#138798 = CARTESIAN_POINT ( 'NONE',  ( 1.441030037510174777, -1.730879250949714843, -1.034145807338890277 ) ) ;
#138797 = CARTESIAN_POINT ( 'NONE',  ( 3.553238514845298734, 7.337208092372121904, -0.2327671511505452484 ) ) ;
#138799 = CARTESIAN_POINT ( 'NONE',  ( 1.364683531250000303, 11.06770833367473550, -0.7879004041258355073 ) ) ;
#138801 = CARTESIAN_POINT ( 'NONE',  ( -4.796552484184649856, 8.818004674849227342, -0.7998128361456362523 ) ) ;
#138800 = CARTESIAN_POINT ( 'NONE',  ( -0.1288028175206907822, -0.008968661790493319408, -2.273875003271645934 ) ) ;
#138803 = VERTEX_POINT ( 'NONE', #107768 ) ;
#138802 = CARTESIAN_POINT ( 'NONE',  ( 3.135487559415173653, -1.157359333423061409, -1.278988843622446137 ) ) ;
#138804 = CARTESIAN_POINT ( 'NONE',  ( 6.328397690248316110, -1.000878058022572903, -1.869571840794107986 ) ) ;
#138805 = CARTESIAN_POINT ( 'NONE',  ( 6.096362627639171805, 10.26417349888772179, -0.7998128361456291469 ) ) ;
#138806 = CARTESIAN_POINT ( 'NONE',  ( 5.606460214450851964, 6.499623990736163037, 1.199719254218462483 ) ) ;
#138807 = ADVANCED_FACE ( 'NONE', ( #172706 ), #94370, .T. ) ;
#138808 = PLANE ( 'NONE',  #182088 ) ;
#138809 = CARTESIAN_POINT ( 'NONE',  ( 0.5901948623465642640, 1.011764341257429978, -1.680720577067334354 ) ) ;
#138810 = CARTESIAN_POINT ( 'NONE',  ( 6.922777049148924000, -8.203199116536602276, -6.506163559800166141 ) ) ;
#138811 = CARTESIAN_POINT ( 'NONE',  ( 6.844168616800228477, 6.879284895888727824, -0.7998128361456281477 ) ) ;
#138812 = ORIENTED_EDGE ( 'NONE', *, *, #103518, .T. ) ;
#138813 = CARTESIAN_POINT ( 'NONE',  ( 9.499771961674738918, -7.051679281653861153, 0.06642998979260432424 ) ) ;
#138814 = VERTEX_POINT ( 'NONE', #46988 ) ;
#138815 = CARTESIAN_POINT ( 'NONE',  ( 3.088311256162243446, -1.077087438943722164, 1.456314016777765286 ) ) ;
#138816 = ORIENTED_EDGE ( 'NONE', *, *, #59430, .T. ) ;
#138817 = CARTESIAN_POINT ( 'NONE',  ( 8.380911511541880188, 12.92948053010758258, 0.7998128361456462443 ) ) ;
#138818 = CARTESIAN_POINT ( 'NONE',  ( 3.549202351727371862, 7.362762853649070571, -0.7998128361456362523 ) ) ;
#138819 = CARTESIAN_POINT ( 'NONE',  ( 3.598146505595464006, -0.8898571075792599538, 1.577739831003275084 ) ) ;
#138820 = CARTESIAN_POINT ( 'NONE',  ( 0.4841233049523195886, 3.595619050313132448, 0.4351758553768796944 ) ) ;
#138821 = CARTESIAN_POINT ( 'NONE',  ( 0.000000000000000000, 3.499999999999989342, 0.000000000000000000 ) ) ;
#138822 = CARTESIAN_POINT ( 'NONE',  ( 5.364345920411571100, 6.316227854031381206, 1.080878399565273540 ) ) ;
#138823 = EDGE_CURVE ( 'NONE', #34023, #75994, #86100, .T. ) ;
#138825 = CARTESIAN_POINT ( 'NONE',  ( -1.364683531250010295, 14.63020833367473550, 0.7879004041258445001 ) ) ;
#138824 = CARTESIAN_POINT ( 'NONE',  ( 5.248444859377932481, -1.846993913715170077, -0.2278608691909170259 ) ) ;
#138826 = EDGE_CURVE ( 'NONE', #181742, #121570, #55924, .T. ) ;
#138827 = CARTESIAN_POINT ( 'NONE',  ( 2.196773704658647297, 1.712196953037805613, 0.8591283806286521552 ) ) ;
#138828 =( LENGTH_UNIT ( ) NAMED_UNIT ( * ) SI_UNIT ( .MILLI., .METRE. ) );
#138829 = CARTESIAN_POINT ( 'NONE',  ( -11.52570357830391323, 8.091488070261075194, -2.173620758456770830 ) ) ;
#138830 = AXIS2_PLACEMENT_3D ( 'NONE', #213011, #117731, #1746 ) ;
#138831 = CARTESIAN_POINT ( 'NONE',  ( 6.086061792568233209, 7.019478939793144967, 0.9900148145245997178 ) ) ;
#138832 = CARTESIAN_POINT ( 'NONE',  ( 8.302289836269501677, 14.87052365979419655, 9.588395110663297416 ) ) ;
#138833 = DIRECTION ( 'NONE',  ( 0.000000000000000000, 0.000000000000000000, 1.000000000000000000 ) ) ;
#138834 = DIRECTION ( 'NONE',  ( 1.000000000000000000, 0.000000000000000000, -3.491481338843133355E-15 ) ) ;
#138835 = CARTESIAN_POINT ( 'NONE',  ( 7.456621297836082185, 7.801739057004660971, 0.7216878364870317197 ) ) ;
#138836 = CARTESIAN_POINT ( 'NONE',  ( -3.415764635639130020, 6.072476943965863683, 1.199719254218462483 ) ) ;
#138837 = CARTESIAN_POINT ( 'NONE',  ( -9.586610838029432813, -7.161464053357567749, 0.003376046620578128550 ) ) ;
#138838 = CARTESIAN_POINT ( 'NONE',  ( 1.746151220907150359, 0.6571888886500141247, 1.984721739902342019 ) ) ;
#138839 = CARTESIAN_POINT ( 'NONE',  ( 6.721714886968523928, -1.868385559882647318, 0.4688378381374983528 ) ) ;
#138840 = CARTESIAN_POINT ( 'NONE',  ( -5.590039407536138150, 5.416134151747256986, 0.000000000000000000 ) ) ;
#138841 = CARTESIAN_POINT ( 'NONE',  ( 2.063248287022978467, 0.3151258922809499485, -1.798016661460503984 ) ) ;
#138842 = CARTESIAN_POINT ( 'NONE',  ( 3.123846942790895920, -2.126788776302591888, 0.5888931905130635469 ) ) ;
#138843 = CARTESIAN_POINT ( 'NONE',  ( 1.499999999999996891, 9.927083334016131744, -0.8660254037844378194 ) ) ;
#138844 = CARTESIAN_POINT ( 'NONE',  ( 1.160255710619631397, 1.910328232974867868, 0.09094507755665059978 ) ) ;
#138845 = CARTESIAN_POINT ( 'NONE',  ( 1.697640821309716497, -1.424308401971938975, -1.360563176039381261 ) ) ;
#138846 = CARTESIAN_POINT ( 'NONE',  ( 4.229980187955574067, 1.905242447948073403, 0.3755566216582290617 ) ) ;
#138847 = VERTEX_POINT ( 'NONE', #117359 ) ;
#138848 = DIRECTION ( 'NONE',  ( 0.000000000000000000, -1.000000000000000000, 0.000000000000000000 ) ) ;
#138850 = CARTESIAN_POINT ( 'NONE',  ( 6.719592977537645062, 0.3186052404706584129, -1.833303987817246794 ) ) ;
#138849 = CARTESIAN_POINT ( 'NONE',  ( -3.318713740295064163, 7.093859473644694269, 0.000000000000000000 ) ) ;
#138851 = CARTESIAN_POINT ( 'NONE',  ( 4.061549535745618833, 6.896169004081968090, -1.199719254218452047 ) ) ;
#138852 = CARTESIAN_POINT ( 'NONE',  ( 0.3123298761244165389, -8.144690279336737504, 9.521443730523929005 ) ) ;
#138853 = CARTESIAN_POINT ( 'NONE',  ( 9.317477881089539338, 11.89347683273640932, 1.599625672291279388 ) ) ;
#138854 = CARTESIAN_POINT ( 'NONE',  ( -7.259464905474441565, 7.434073576000447048, -0.7998128361456362523 ) ) ;
#138855 = CARTESIAN_POINT ( 'NONE',  ( 2.788834510562918645, 1.878274557074947948, -1.128960604485473862 ) ) ;
#138856 = CARTESIAN_POINT ( 'NONE',  ( 3.714570900464285064, 4.396382807705524698, 1.082531754730560403 ) ) ;
#138857 = ORIENTED_EDGE ( 'NONE', *, *, #36800, .F. ) ;
#138858 = CIRCLE ( 'NONE', #166504, 2.400000000000000799 ) ;
#138859 = CARTESIAN_POINT ( 'NONE',  ( 6.821687566331318564, 7.987665577921906568, 1.199719254218452935 ) ) ;
#138860 = DIRECTION ( 'NONE',  ( 5.578174157656880098E-15, 1.000000000000000000, 7.437565543542506798E-15 ) ) ;
#138861 = CARTESIAN_POINT ( 'NONE',  ( 3.633261591126951018, -1.686358373764598406, 0.7000054678709469735 ) ) ;
#138862 = FACE_OUTER_BOUND ( 'NONE', #117113, .T. ) ;
#138863 = CARTESIAN_POINT ( 'NONE',  ( -3.195971524519394702, 4.751719416737803847, -1.599625672291262513 ) ) ;
#138864 = CARTESIAN_POINT ( 'NONE',  ( -5.066182726705734218, 7.967045547422810792, 1.194666625917781611 ) ) ;
#138865 = DIRECTION ( 'NONE',  ( 1.040834085586084257E-15, 1.000000000000000000, -4.622230424712076367E-32 ) ) ;
#138866 = CARTESIAN_POINT ( 'NONE',  ( 4.100366707588389836, -0.5864361863821172527, -1.776433678864146382 ) ) ;
#138867 = CARTESIAN_POINT ( 'NONE',  ( 9.413438726589914651, 9.876766690643398405, 0.000000000000000000 ) ) ;
#138868 = CARTESIAN_POINT ( 'NONE',  ( 2.455585946167909928, 0.5135756288857267204, -1.856723504524477875 ) ) ;
#138869 = CARTESIAN_POINT ( 'NONE',  ( 6.368018226480639754, -1.947316962026977682, 0.2367824842242904348 ) ) ;
#138870 = TOROIDAL_SURFACE ( 'NONE', #145850, 0.8299999999999999600, 0.08000000000000000167 ) ;
#138871 = CARTESIAN_POINT ( 'NONE',  ( 1.364683531250000303, 9.067708333674733723, -0.7879004041258355073 ) ) ;
#138872 = CARTESIAN_POINT ( 'NONE',  ( -5.554036483092550824, 9.631459663583308739, -0.7998128361456231517 ) ) ;
#138873 = CARTESIAN_POINT ( 'NONE',  ( 5.495132332240461714, 5.305409230568988832, 0.7998128361456341429 ) ) ;
#138874 = CARTESIAN_POINT ( 'NONE',  ( -5.939880696118548187, 6.102484698325975288, 0.000000000000000000 ) ) ;
#138875 = CARTESIAN_POINT ( 'NONE',  ( 0.5798918133415768006, -0.7576680531077238934, 1.977200763303339714 ) ) ;
#138876 = CARTESIAN_POINT ( 'NONE',  ( 10.56588178375152864, 11.22128359066528169, -0.7998128361456281477 ) ) ;
#138877 = CARTESIAN_POINT ( 'NONE',  ( -1.378881877344243945, 4.087185210397143109, 0.5904953584335903560 ) ) ;
#138878 = CARTESIAN_POINT ( 'NONE',  ( 4.926661076633905623, -1.356332079400805135, 1.564123780295342492 ) ) ;
#138880 = CARTESIAN_POINT ( 'NONE',  ( -0.6823417656250212460, 2.863541667008084879, 1.181850606188767472 ) ) ;
#138879 = CARTESIAN_POINT ( 'NONE',  ( 0.3976880421775743635, -0.6195963491163231085, -1.733980255833282191 ) ) ;
#138881 = ORIENTED_EDGE ( 'NONE', *, *, #187841, .T. ) ;
#138882 = CARTESIAN_POINT ( 'NONE',  ( 5.098365541279441082, -0.3395090112114571013, 2.273368781073564993 ) ) ;
#138883 = CARTESIAN_POINT ( 'NONE',  ( 7.456621297836082185, 7.801739057004660971, 0.7216878364870317197 ) ) ;
#138885 = CARTESIAN_POINT ( 'NONE',  ( 0.3282377607281121712, 1.426335450315397102, -1.225000000000027400 ) ) ;
#138884 = CARTESIAN_POINT ( 'NONE',  ( 5.126391479742934187, 6.113783160189109722, -1.082531754730548412 ) ) ;
#138886 = CARTESIAN_POINT ( 'NONE',  ( 0.4458144982435990888, 0.7132466706018144587, -2.178543642160748917 ) ) ;
#138887 = CARTESIAN_POINT ( 'NONE',  ( 0.3282377607281144472, 0.3236645496846485281, 1.224999999999966116 ) ) ;
#138888 = CARTESIAN_POINT ( 'NONE',  ( -5.074494633264801990, 9.142270515442742607, 0.7998128361456291469 ) ) ;
#138889 = CARTESIAN_POINT ( 'NONE',  ( 5.103436805131417842, -1.932407887632971555, 0.1922973783335303055 ) ) ;
#138890 = EDGE_LOOP ( 'NONE', ( #60711, #159566, #68857, #146826 ) ) ;
#138891 = CARTESIAN_POINT ( 'NONE',  ( 9.205623113554624481, 10.80261038964432707, 1.082531754730549967 ) ) ;
#138892 = EDGE_CURVE ( 'NONE', #15383, #170783, #83718, .T. ) ;
#138893 = VERTEX_POINT ( 'NONE', #197468 ) ;
#138894 = CARTESIAN_POINT ( 'NONE',  ( -0.2106854629475244378, -0.004120941679102134263, -1.996958217618934661 ) ) ;
#138895 = CARTESIAN_POINT ( 'NONE',  ( 6.069546051295944267, 1.394081536189459847, 1.457239770841619375 ) ) ;
#138897 =( NAMED_UNIT ( * ) PLANE_ANGLE_UNIT ( ) SI_UNIT ( $, .RADIAN. ) );
#138896 = CARTESIAN_POINT ( 'NONE',  ( -7.330154606482786050, 11.70359747420527619, 0.000000000000000000 ) ) ;
#138898 = CARTESIAN_POINT ( 'NONE',  ( -3.285556943749998737, -2.617708332855374298, 1.896917185911908499 ) ) ;
#138900 = CARTESIAN_POINT ( 'NONE',  ( 1.375481398426938284, 1.050436561215197351, 1.424246879149461797 ) ) ;
#138899 = CARTESIAN_POINT ( 'NONE',  ( 3.082061393860520138, -2.059794914563463308, -0.3567947225071969042 ) ) ;
#138901 = CARTESIAN_POINT ( 'NONE',  ( 2.550000000000000266, 1.000000000000000888, 1.849324200890695824 ) ) ;
#138903 = CARTESIAN_POINT ( 'NONE',  ( 4.119262515598776098, -2.194098707595509623, 0.6636001952689452033 ) ) ;
#138902 = CARTESIAN_POINT ( 'NONE',  ( 3.464990776744291345, 6.200183785247111778, 1.199719254218452047 ) ) ;
#138904 = B_SPLINE_CURVE_WITH_KNOTS ( 'NONE', 3,
 ( #188540, #156051, #205851, #123643 ),
 .UNSPECIFIED., .F., .F.,
 ( 4, 4 ),
 ( 0.000000000000000000, 1.835777882413431832E-05 ),
 .UNSPECIFIED. ) ;
#138905 = CARTESIAN_POINT ( 'NONE',  ( 2.273056812072488775, 1.069988629298643579, 1.372433606717870846 ) ) ;
#138906 = CARTESIAN_POINT ( 'NONE',  ( 3.867100128395839942, 5.534702787927018974, -1.599625672291255185 ) ) ;
#138907 = CARTESIAN_POINT ( 'NONE',  ( -2.681339180781858289, -0.4790681834518588644, -0.1012129971987970750 ) ) ;
#138908 = CARTESIAN_POINT ( 'NONE',  ( 2.020412548985677681, 1.729603159991144556, -0.1218859752038989053 ) ) ;
#138909 = CARTESIAN_POINT ( 'NONE',  ( -0.6801582343750125492, 2.213541667008059211, 1.178068619123818994 ) ) ;
#138910 = CARTESIAN_POINT ( 'NONE',  ( 1.293147247811817779, -1.684623093139308025, 0.7912131235938785201 ) ) ;
#138911 = CARTESIAN_POINT ( 'NONE',  ( 2.383468162319524630, -0.001743713053406481962, 2.171350059665664300 ) ) ;
#138912 = CARTESIAN_POINT ( 'NONE',  ( 4.150767584078112193, 7.994312614733129152, 0.7998128361456321445 ) ) ;
#138913 = CARTESIAN_POINT ( 'NONE',  ( 3.591030000661588062, 1.731995077137841843, 1.032480907900306111 ) ) ;
#138914 = CARTESIAN_POINT ( 'NONE',  ( 1.781250000000001332, 0.7852924748300815772, 1.895863743164048154 ) ) ;
#138915 = CIRCLE ( 'NONE', #45527, 0.08000000000000015432 ) ;
#138916 = CARTESIAN_POINT ( 'NONE',  ( -1.201851678989727383E-14, 3.118750000682814161, -1.732050807568863648 ) ) ;
#138917 = CARTESIAN_POINT ( 'NONE',  ( 0.5340448022827409824, 0.9932739084477918423, -1.650449964952714454 ) ) ;
#138918 = CARTESIAN_POINT ( 'NONE',  ( 0.6823417656249969321, 14.77604166700806410, -1.181850606188757036 ) ) ;
#138919 = CARTESIAN_POINT ( 'NONE',  ( 4.535507215201760367, -0.1075840215562298280, 2.218897223943790742 ) ) ;
#138920 = ORIENTED_EDGE ( 'NONE', *, *, #164541, .F. ) ;
#138922 = CIRCLE ( 'NONE', #11013, 0.08000000000000025147 ) ;
#138921 = SURFACE_STYLE_FILL_AREA ( #206019 ) ;
#138923 = CARTESIAN_POINT ( 'NONE',  ( -1.402160292154681736E-14, -0.1624999999999815481, -1.732050807568870754 ) ) ;
#138924 = CARTESIAN_POINT ( 'NONE',  ( 6.805303039055573322, 10.02693841461847057, 1.199719254218460707 ) ) ;
#138925 = CARTESIAN_POINT ( 'NONE',  ( -0.6823417656250003738, -0.7822916663252423852, -1.181850606188749264 ) ) ;
#138926 = CARTESIAN_POINT ( 'NONE',  ( 1.032228388637240313, -2.166051452891520679, 0.4916964420428306948 ) ) ;
#138927 = CARTESIAN_POINT ( 'NONE',  ( 6.215287892896892430, -1.681934637451238279, -1.009743211781432670 ) ) ;
#138928 = CARTESIAN_POINT ( 'NONE',  ( 7.768458830950378591, 12.00702636951006497, 1.040834085586084257E-14 ) ) ;
#138929 = CARTESIAN_POINT ( 'NONE',  ( 5.466221857368295467, 1.108383815247836690, 1.972225493889906867 ) ) ;
#138930 = CARTESIAN_POINT ( 'NONE',  ( -3.662110889467009578, 7.286563447771212232, 0.7216878364870338292 ) ) ;
#138931 = CARTESIAN_POINT ( 'NONE',  ( 3.719230382982277927, -1.817711772858042751, -0.9750064267827946995 ) ) ;
#138932 = CARTESIAN_POINT ( 'NONE',  ( -6.555530967407501741, 7.606873202518897870, 1.199719254218450271 ) ) ;
#138933 = CARTESIAN_POINT ( 'NONE',  ( 1.499999999999987121, 2.827083334016148530, -0.8660254037844262731 ) ) ;
#138934 = CARTESIAN_POINT ( 'NONE',  ( -0.6823417656249969321, 5.030208333674755394, -1.181850606188749264 ) ) ;
#138935 = CARTESIAN_POINT ( 'NONE',  ( 4.323419078940895943, -1.790677508454678657, 0.5408235849187342792 ) ) ;
#138936 = CARTESIAN_POINT ( 'NONE',  ( 3.674194220352343443, 1.259077133501560697, 1.192749331401379731 ) ) ;
#138937 = CARTESIAN_POINT ( 'NONE',  ( 3.579424886596099586, -0.8542006638617373193, 1.516299650553302181 ) ) ;
#138938 = EDGE_CURVE ( 'NONE', #142721, #111346, #24825, .T. ) ;
#138939 = CARTESIAN_POINT ( 'NONE',  ( 0.3106431952284515741, 1.574884954006963600, -1.665989127006389126 ) ) ;
#138940 = CARTESIAN_POINT ( 'NONE',  ( 1.364683531249988535, 4.217708333674752730, -0.7879004041258239610 ) ) ;
#138941 = CARTESIAN_POINT ( 'NONE',  ( 4.915614241032515430, -1.119620181645267776, -1.765504464341709934 ) ) ;
#138942 = CARTESIAN_POINT ( 'NONE',  ( 5.824156380204161820, 1.872177270857039000, 0.5156464658115608168 ) ) ;
#138944 = ORIENTED_EDGE ( 'NONE', *, *, #160078, .F. ) ;
#138943 = CARTESIAN_POINT ( 'NONE',  ( 9.348381460497192208, 13.52536904890506619, 7.450314784081279562 ) ) ;
#138945 = CARTESIAN_POINT ( 'NONE',  ( 0.5982800022500452952, -0.2930678230431381648, 1.994870242743536304 ) ) ;
#138946 = CARTESIAN_POINT ( 'NONE',  ( 0.3871773095200456982, -1.998849835692744659, -0.7086421328065874992 ) ) ;
#138947 = CARTESIAN_POINT ( 'NONE',  ( 0.000000000000000000, -13.99999999999999822, 0.000000000000000000 ) ) ;
#138948 = CARTESIAN_POINT ( 'NONE',  ( -1.249999999999997558, 10.00000000000000178, -4.154462424328202452 ) ) ;
#138949 = CARTESIAN_POINT ( 'NONE',  ( -8.479735010343349089, 11.98044238112085758, 1.199719254218453823 ) ) ;
#138950 = CARTESIAN_POINT ( 'NONE',  ( 6.632963465583686435, 8.761543347979550589, -1.599625672291262513 ) ) ;
#138951 = CARTESIAN_POINT ( 'NONE',  ( -6.773846765307970585, -7.473374494058216300, 6.773846765307992790 ) ) ;
#138953 = ADVANCED_FACE ( 'NONE', ( #116289 ), #97872, .T. ) ;
#138952 = CARTESIAN_POINT ( 'NONE',  ( 4.723181480036696023, -0.08661695748878039947, 1.823760500460340550 ) ) ;
#138954 = ORIENTED_EDGE ( 'NONE', *, *, #13614, .F. ) ;
#138955 = CARTESIAN_POINT ( 'NONE',  ( -5.935437387732586778, 10.14670372898850381, -0.7998128361456362523 ) ) ;
#138956 = CARTESIAN_POINT ( 'NONE',  ( 9.512045263456263555, -8.176568542494905500, -0.4655551865852067817 ) ) ;
#138957 = CARTESIAN_POINT ( 'NONE',  ( -3.285556943749998737, -2.617708332855374298, 1.896917185911908499 ) ) ;
#138958 = CARTESIAN_POINT ( 'NONE',  ( -7.477485413136760073, 8.682486722536401302, -1.199719254218446718 ) ) ;
#138959 = CARTESIAN_POINT ( 'NONE',  ( 2.232681213900446160, 1.316219961256912763, -1.532148775131780383 ) ) ;
#138960 = CARTESIAN_POINT ( 'NONE',  ( 6.159228477734898455, -1.889628185881117695, -1.139594184263223120 ) ) ;
#138961 = CARTESIAN_POINT ( 'NONE',  ( -3.122120512896910505, 6.864500708346841229, 0.7998128361456352531 ) ) ;
#138962 = CARTESIAN_POINT ( 'NONE',  ( 3.115880741807099508, 1.852434257297396858, -0.1774315261868253668 ) ) ;
#138963 = CARTESIAN_POINT ( 'NONE',  ( 2.381428537494710618, 5.930083727052461562, 0.7998128361456462443 ) ) ;
#138964 = DIRECTION ( 'NONE',  ( -1.000000000000000000, 6.505213034913026604E-16, 0.000000000000000000 ) ) ;
#138965 = ORIENTED_EDGE ( 'NONE', *, *, #191143, .T. ) ;
#138966 = ORIENTED_EDGE ( 'NONE', *, *, #130414, .F. ) ;
#138967 = CARTESIAN_POINT ( 'NONE',  ( -4.660252114795309097, 6.460046772059735432, -1.599625672291256295 ) ) ;
#138968 = CARTESIAN_POINT ( 'NONE',  ( -8.134002093194872884, 11.57708731111429401, 1.199719254218453823 ) ) ;
#138969 = CARTESIAN_POINT ( 'NONE',  ( 5.391160240453525709, 1.608232483172780558, -0.8641324296934371763 ) ) ;
#138971 = CARTESIAN_POINT ( 'NONE',  ( -4.014048110574687911, 7.796590492392542870, 0.4333429611983550256 ) ) ;
#138970 = CARTESIAN_POINT ( 'NONE',  ( -4.329849954717889915, 6.144853928627882489, 1.599625672291270506 ) ) ;
#138972 = CARTESIAN_POINT ( 'NONE',  ( 6.328358748234019338, 6.951510624437585939, -0.8854765018257749754 ) ) ;
#138973 = CARTESIAN_POINT ( 'NONE',  ( 0.8953158854557360380, 0.1194439997053517860, 1.729786500971510765 ) ) ;
#138974 = CARTESIAN_POINT ( 'NONE',  ( 0.005214030526056419486, -0.7400075616556491820, -1.574097848898856622 ) ) ;
#138975 = CARTESIAN_POINT ( 'NONE',  ( 5.901056178406707708, 1.890114102979102650, -1.323741089068092958 ) ) ;
#138976 = CARTESIAN_POINT ( 'NONE',  ( 4.016958651398847557, 7.908478536599129249, -0.7998128361456362523 ) ) ;
#138977 = CARTESIAN_POINT ( 'NONE',  ( 0.5267265402719328860, 1.971218143044730420, 0.6008300406652696823 ) ) ;
#138978 = CARTESIAN_POINT ( 'NONE',  ( 6.657217119509961201, 7.725507046638470321, -1.199719254218446718 ) ) ;
#138979 = CARTESIAN_POINT ( 'NONE',  ( 5.747524558462486333, -2.240600987983232262, -0.5116226552598357458 ) ) ;
#138980 = CARTESIAN_POINT ( 'NONE',  ( 5.951324661306437669, 4.742844146916157300, 2.438848701820569786 ) ) ;
#138981 = CARTESIAN_POINT ( 'NONE',  ( -7.099629715411508890, 8.311931418515415615, 1.199719254218452047 ) ) ;
#138983 = EDGE_CURVE ( 'NONE', #197365, #702, #140429, .T. ) ;
#138982 = COLOUR_RGB ( '', 0.08235294, 0.09019608, 0.10196078) ;
#138984 = CARTESIAN_POINT ( 'NONE',  ( 6.051601594667258333, 0.5412791183288803154, -1.790613848972313571 ) ) ;
#138986 = CARTESIAN_POINT ( 'NONE',  ( -2.972980823146582186, 6.690504403638126263, 0.000000000000000000 ) ) ;
#138985 = CARTESIAN_POINT ( 'NONE',  ( 3.252119977711815491, 0.8557668478980616777, -1.710280963351323846 ) ) ;
#138987 = CARTESIAN_POINT ( 'NONE',  ( 4.811249113497881424, 1.919052844561389692, 1.089612025192594258 ) ) ;
#138988 = CARTESIAN_POINT ( 'NONE',  ( 4.786377933101198856, -0.7163331637287263520, -1.992584184115009149 ) ) ;
#138989 = CARTESIAN_POINT ( 'NONE',  ( 1.224999999999989875, 0.4375000006828014265, -4.510281037539698445E-14 ) ) ;
#138990 = CARTESIAN_POINT ( 'NONE',  ( 6.883263157960393563, 4.695771316066229772, 2.508818740863460572 ) ) ;
#138991 = CARTESIAN_POINT ( 'NONE',  ( -0.2108831679770960255, -0.001785917861228669690, -1.896958272444612792 ) ) ;
#138992 = CARTESIAN_POINT ( 'NONE',  ( 6.183927461164522299, 6.387205924212962849, 0.000000000000000000 ) ) ;
#138993 = CARTESIAN_POINT ( 'NONE',  ( -6.116136693096208887, 6.308116694799912771, 0.7216878364870257245 ) ) ;
#138994 = CARTESIAN_POINT ( 'NONE',  ( 5.426475896148662770, -0.9536019125786737716, -1.894055658958586852 ) ) ;
#138995 = CARTESIAN_POINT ( 'NONE',  ( 2.591229953566904776, -0.3941274307956154077, -2.273529888306951019 ) ) ;
#138996 = CARTESIAN_POINT ( 'NONE',  ( 4.193769882565239193, -1.351282707657221582, -1.422545440481419510 ) ) ;
#138997 = CARTESIAN_POINT ( 'NONE',  ( 6.297729475711208558, -1.489980986158835119, -1.426453875638087343 ) ) ;
#138998 = CARTESIAN_POINT ( 'NONE',  ( 3.063779527008311021, 5.557864633942907417, 1.082531754730546636 ) ) ;
#138999 = CARTESIAN_POINT ( 'NONE',  ( 4.228163802615382494, 6.026220084508304708, -1.599625672291269396 ) ) ;
#139000 = ORIENTED_EDGE ( 'NONE', *, *, #22500, .F. ) ;
#139001 = CARTESIAN_POINT ( 'NONE',  ( 5.717982508692024624, 0.9896897593998502662, -1.756851901128737348 ) ) ;
#139002 = CARTESIAN_POINT ( 'NONE',  ( -9.592557376868645846, 11.15007068022363157, -1.199719254218441611 ) ) ;
#139003 = CARTESIAN_POINT ( 'NONE',  ( 11.81900460097218186, 13.75757134874136334, 1.592493057836596115 ) ) ;
#139004 = CARTESIAN_POINT ( 'NONE',  ( -10.48267169704037727, 5.268073273308885973, 5.153989745587932880 ) ) ;
#139005 = CARTESIAN_POINT ( 'NONE',  ( 2.905323041198346612, -1.807408099546173208, 1.202558989554833646 ) ) ;
#139006 = CARTESIAN_POINT ( 'NONE',  ( 3.867818961648523235, 7.734482231890414283, 1.040834085586084257E-14 ) ) ;
#139007 = CARTESIAN_POINT ( 'NONE',  ( 1.143014088299774578, 2.045220145331683614, 0.5602274146137007360 ) ) ;
#139008 = CARTESIAN_POINT ( 'NONE',  ( 0.7499999999999902300, 1.264583334016147642, 1.299038105676657340 ) ) ;
#139009 = CARTESIAN_POINT ( 'NONE',  ( -5.995491887707443013, 14.48115541362584402, -10.40458799691657532 ) ) ;
#139010 = CARTESIAN_POINT ( 'NONE',  ( 6.059925523928845870, 7.140772946495586915, 1.155538509043469997 ) ) ;
#139011 = CARTESIAN_POINT ( 'NONE',  ( 0.8079727292511580394, -2.051105382888893658, 0.1991618667988598601 ) ) ;
#139012 = VECTOR ( 'NONE', #118027, 1000.000000000000000 ) ;
#139014 = CARTESIAN_POINT ( 'NONE',  ( 6.727182134110231360, 6.039168392632435989, 2.405853653942995773 ) ) ;
#139013 = CARTESIAN_POINT ( 'NONE',  ( -9.612894607289142357, 11.17379744904754801, -1.199719254218441611 ) ) ;
#139015 = CARTESIAN_POINT ( 'NONE',  ( 0.6823417656249882723, 0.6760416670080898749, -1.181850606188749264 ) ) ;
#139016 = CARTESIAN_POINT ( 'NONE',  ( -0.4640281877397542942, 3.122791860410086606, 2.027579305719746205 ) ) ;
#139017 = ORIENTED_EDGE ( 'NONE', *, *, #25165, .F. ) ;
#139018 = CARTESIAN_POINT ( 'NONE',  ( 3.826736342760712173, 1.350229473097919630, -1.354399478966497483 ) ) ;
#139019 = CARTESIAN_POINT ( 'NONE',  ( 5.137463350450376609, -1.253266684191740810, -1.249936613051380485 ) ) ;
#139020 = CARTESIAN_POINT ( 'NONE',  ( 5.027041095616958444, 9.086908054853605421, 0.000000000000000000 ) ) ;
#139021 = CARTESIAN_POINT ( 'NONE',  ( -5.590039407536138150, 5.416134151747256986, 0.000000000000000000 ) ) ;
#139022 = CARTESIAN_POINT ( 'NONE',  ( 0.01741795466771427214, -0.4834593703179098645, 1.745828368453090418 ) ) ;
#139024 = CARTESIAN_POINT ( 'NONE',  ( 6.327746003090493510, 0.7280626223893000848, -1.772066133663487530 ) ) ;
#139023 = CARTESIAN_POINT ( 'NONE',  ( 1.499999999999990896, 8.673756432004010364, -2.614717076620595826 ) ) ;
#139025 = CARTESIAN_POINT ( 'NONE',  ( 1.188034388246852480, -1.312013912954514971, -1.601590607232979524 ) ) ;
#139026 = CARTESIAN_POINT ( 'NONE',  ( -1.402160292154681736E-14, 0.2593750003414224681, -1.575800808251665908 ) ) ;
#139027 = AXIS2_PLACEMENT_3D ( 'NONE', #113332, #46147, #162022 ) ;
#139028 = CARTESIAN_POINT ( 'NONE',  ( 5.840666405660361882, 0.3664468388623157158, 1.834233659845653897 ) ) ;
#139029 = CARTESIAN_POINT ( 'NONE',  ( 2.314841291766779108, 1.630546960418734148, 0.8213866120303781049 ) ) ;
#139031 = CARTESIAN_POINT ( 'NONE',  ( 5.324837791525375508, 7.612559486139466536, 1.234112182050936646 ) ) ;
#139030 = CARTESIAN_POINT ( 'NONE',  ( 5.162800556355915838, -1.600310254184673431, 1.519886962452212664 ) ) ;
#139032 = CARTESIAN_POINT ( 'NONE',  ( 0.6823417656249882723, 0.4260416670080896528, -1.181850606188749264 ) ) ;
#139033 = CARTESIAN_POINT ( 'NONE',  ( 3.842276591979614242, -1.019319043456867524, 1.793165911747495844 ) ) ;
#139034 = CARTESIAN_POINT ( 'NONE',  ( -6.906989191158078079, 10.14557225873805812, -1.199719254218440723 ) ) ;
#139035 = CARTESIAN_POINT ( 'NONE',  ( 9.023114925094663619, 10.48572115315399245, 1.199719254218453823 ) ) ;
#139036 = DIRECTION ( 'NONE',  ( 0.6762880771785568790, 0.000000000000000000, 0.7366372490351884572 ) ) ;
#139037 = CARTESIAN_POINT ( 'NONE',  ( 6.215297738502283842, -1.773692237561547147, -1.067698627785176768 ) ) ;
#139038 = CARTESIAN_POINT ( 'NONE',  ( -0.6823417656250212460, 0.8635416670080899859, 1.181850606188755259 ) ) ;
#139039 = CARTESIAN_POINT ( 'NONE',  ( 4.112696061561730509, 1.531809107248631507, -1.525399859652858847 ) ) ;
#139041 = CARTESIAN_POINT ( 'NONE',  ( 1.662477996687723669, -0.7030478115006146833, -1.831755296705489977 ) ) ;
#139040 = CARTESIAN_POINT ( 'NONE',  ( 4.617835026475571425, -0.5366920026289195844, 1.946999912814169287 ) ) ;
#139042 = CARTESIAN_POINT ( 'NONE',  ( 4.892487020634524342, 4.880525410245029505, -1.277330582746047388E-09 ) ) ;
#139045 = CARTESIAN_POINT ( 'NONE',  ( 5.477130870240836558, 9.333810415348903433, -0.7216878364870267237 ) ) ;
#139044 = CARTESIAN_POINT ( 'NONE',  ( -3.285556943750000070, -3.959374999522043304, 0.000000000000000000 ) ) ;
#139043 = DIRECTION ( 'NONE',  ( 0.000000000000000000, 0.2128498979015776560, 0.9770849098022587054 ) ) ;
#139046 = CARTESIAN_POINT ( 'NONE',  ( -5.610041701004606196, 9.767075427805856691, -0.7998128361456362523 ) ) ;
#139047 = CARTESIAN_POINT ( 'NONE',  ( 2.413296319342159713, -1.879803466158457059, 0.7303082167480907660 ) ) ;
#139048 = CARTESIAN_POINT ( 'NONE',  ( -4.548924232584923288, 5.265832011892554121, -1.199719254218446718 ) ) ;
#139049 = CARTESIAN_POINT ( 'NONE',  ( 1.499999999999822586, 7.388542872122531691, 4.154462424328221104 ) ) ;
#139050 = CARTESIAN_POINT ( 'NONE',  ( 6.187759705938407073, 1.828009178079874841, -0.5617473972939349691 ) ) ;
#139051 = CARTESIAN_POINT ( 'NONE',  ( -4.434768960748669997, 5.005376996850392501, -0.9481656214291103169 ) ) ;
#139052 = CARTESIAN_POINT ( 'NONE',  ( 4.595850884908202261, 7.345281218159464665, -1.082531754730549078 ) ) ;
#139054 = CARTESIAN_POINT ( 'NONE',  ( 4.060172857048785389, -1.158672032380179573, 1.650094836768666084 ) ) ;
#139053 = CARTESIAN_POINT ( 'NONE',  ( -9.300530188850304469, 9.952966096521256745, 1.040834085586084257E-14 ) ) ;
#139055 = CARTESIAN_POINT ( 'NONE',  ( -0.7499999999999972244, 4.108333333333360038, -1.299038105676652011 ) ) ;
#139056 = CARTESIAN_POINT ( 'NONE',  ( -0.6823417656250039265, 8.567708333674733723, -1.181850606188755259 ) ) ;
#139057 = CARTESIAN_POINT ( 'NONE',  ( 6.809587843971872445, -0.3681478646948634914, 1.690922663601742038 ) ) ;
#139058 = CARTESIAN_POINT ( 'NONE',  ( 6.398522151006641678, 6.429640362454684954, 0.000000000000000000 ) ) ;
#139059 = CARTESIAN_POINT ( 'NONE',  ( 7.944714827928033962, 12.21265836598400689, 0.7216878364870438212 ) ) ;
#139060 = CARTESIAN_POINT ( 'NONE',  ( -6.773376349083142678, -7.246166700180801001, -6.661184041420939117 ) ) ;
#139061 = CARTESIAN_POINT ( 'NONE',  ( 4.516781199771729760, 1.709404882366181377, 0.7599583452636837766 ) ) ;
#139062 =( BOUNDED_CURVE ( )  B_SPLINE_CURVE ( 2, ( #88490, #6130, #201128, #72199, #23453, #1855, #138307, #171859, #52766 ),
 .UNSPECIFIED., .F., .T. ) 
 B_SPLINE_CURVE_WITH_KNOTS ( ( 3, 2, 2, 2, 3 ),
 ( 0.3839285714285713969, 0.3869047619047619180, 0.3928571428571428492, 0.3988095238095238360, 0.4017857142857143016 ),
 .UNSPECIFIED. ) 
 CURVE ( )  GEOMETRIC_REPRESENTATION_ITEM ( )  RATIONAL_B_SPLINE_CURVE ( ( 0.9330127018922194093, 0.9330127018922187432, 1.000000000000000000, 0.8660254037844387076, 1.000000000000000000, 0.8660254037844387076, 1.000000000000000000, 0.9330127018922194093, 0.9330127018922194093 ) ) 
 REPRESENTATION_ITEM ( '' )  );
#139063 = DIRECTION ( 'NONE',  ( 0.000000000000000000, -1.000000000000000000, -0.000000000000000000 ) ) ;
#139065 = AXIS2_PLACEMENT_3D ( 'NONE', #33668, #134413, #167943 ) ;
#139064 = CARTESIAN_POINT ( 'NONE',  ( 2.553653463975919635, 1.597511423921485818, 1.316731848974454833 ) ) ;
#139066 = CARTESIAN_POINT ( 'NONE',  ( -8.054952659850432184, 8.570068656013202002, 0.000000000000000000 ) ) ;
#139067 = EDGE_LOOP ( 'NONE', ( #12879, #22652, #110766 ) ) ;
#139069 = CARTESIAN_POINT ( 'NONE',  ( 3.878514461961128479, 6.682628084666728085, -1.199719254218448494 ) ) ;
#139068 = CIRCLE ( 'NONE', #45688, 0.08000000000000032085 ) ;
#139070 = CARTESIAN_POINT ( 'NONE',  ( 0.2808753465170962249, 1.674874268995883320, -1.122520385770639839 ) ) ;
#139071 = CARTESIAN_POINT ( 'NONE',  ( -0.1935108285373255133, -0.3924519521045151671, -1.774502223569380144 ) ) ;
#139072 = CARTESIAN_POINT ( 'NONE',  ( 5.709392084686216506, 5.833581318321598985, -0.7216878364870458196 ) ) ;
#139073 = CARTESIAN_POINT ( 'NONE',  ( -2.432941034296860483, 5.235517099077979353, -0.8783347955927902628 ) ) ;
#139074 = EDGE_CURVE ( 'NONE', #202980, #183045, #78080, .T. ) ;
#139075 = CARTESIAN_POINT ( 'NONE',  ( 7.524412065460039933, 10.76193592880331984, -1.082531754730537976 ) ) ;
#139076 = CARTESIAN_POINT ( 'NONE',  ( 6.428537391173986038, 10.65171072301167854, 0.7998128361456462443 ) ) ;
#139078 = CARTESIAN_POINT ( 'NONE',  ( 6.362892188913578551, -0.09940890854263698118, -1.913169475778592865 ) ) ;
#139077 = CARTESIAN_POINT ( 'NONE',  ( -6.728924311084075960, 6.744833205886536120, 1.040834085586084257E-14 ) ) ;
#139079 = CARTESIAN_POINT ( 'NONE',  ( -5.409340101728189687, 5.413244328212059031, 0.7216878364870288332 ) ) ;
#139081 = ORIENTED_EDGE ( 'NONE', *, *, #183120, .F. ) ;
#139080 = CARTESIAN_POINT ( 'NONE',  ( 4.528060117284232966, 6.305822774963486310, 1.443375672974062551 ) ) ;
#139082 = CARTESIAN_POINT ( 'NONE',  ( -8.676855123066030018, 9.225345186439589895, -0.7216878364870267237 ) ) ;
#139083 = CARTESIAN_POINT ( 'NONE',  ( 3.485389320157119553, 1.955090977548096687, -0.9225387301767663528 ) ) ;
#139084 = CARTESIAN_POINT ( 'NONE',  ( -7.593975437430151132, 8.032261896522864930, -0.7216878364870338292 ) ) ;
#139085 = CARTESIAN_POINT ( 'NONE',  ( 6.211043768836181478, 7.379210830797944709, 1.082531754730549967 ) ) ;
#139086 = CARTESIAN_POINT ( 'NONE',  ( 1.336355901170083849, -1.182550835430173919, -1.760063440837428272 ) ) ;
#139087 = CARTESIAN_POINT ( 'NONE',  ( 5.860330175037710809, 0.7421476303169189936, 1.668095884353037128 ) ) ;
#139088 = EDGE_CURVE ( 'NONE', #83814, #49203, #8966, .T. ) ;
#139089 = CARTESIAN_POINT ( 'NONE',  ( 1.669145487688096896, 0.1492116152736686074, -1.965789094590511654 ) ) ;
#139090 = CARTESIAN_POINT ( 'NONE',  ( 3.340010735810138520, -1.142844047782382466, -1.533173144288489276 ) ) ;
#139091 = EDGE_LOOP ( 'NONE', ( #92207, #173493 ) ) ;
#139092 = CARTESIAN_POINT ( 'NONE',  ( 5.283641479639247684, -1.870778298764510961, 0.6161543930274359093 ) ) ;
#139093 = CARTESIAN_POINT ( 'NONE',  ( -0.02948999725180690215, 0.001137248348246927814, -1.926291057026579656 ) ) ;
#139094 = ORIENTED_EDGE ( 'NONE', *, *, #57012, .F. ) ;
#139095 = CARTESIAN_POINT ( 'NONE',  ( -4.125423880308188629, 8.035021303660014880, -0.7998128361456481317 ) ) ;
#139096 = CARTESIAN_POINT ( 'NONE',  ( -5.953438850176548947, 9.959779401932374654, 0.000000000000000000 ) ) ;
#139097 = CARTESIAN_POINT ( 'NONE',  ( 6.170369307550815030, 8.292126506933040986, 1.443375672974064550 ) ) ;
#139099 = ORIENTED_EDGE ( 'NONE', *, *, #158166, .T. ) ;
#139098 = CARTESIAN_POINT ( 'NONE',  ( 4.758414378865199801, 1.907420806491459064, 0.1369992607160031295 ) ) ;
#139100 = CARTESIAN_POINT ( 'NONE',  ( 1.290363523627102049, -0.9912053058820712304, 1.971723787660728977 ) ) ;
#139101 = AXIS2_PLACEMENT_3D ( 'NONE', #188327, #24756, #160100 ) ;
#139102 = CARTESIAN_POINT ( 'NONE',  ( 7.772296586883624236, -5.601927612791787858, 7.784592198500461357 ) ) ;
#139103 = CARTESIAN_POINT ( 'NONE',  ( 5.988937038716908745, -1.912324646158647168, -0.6291777902352905238 ) ) ;
#139104 = CARTESIAN_POINT ( 'NONE',  ( 0.5221183067616939066, 7.970647359861179559, 1.933437843119054866 ) ) ;
#139105 = CARTESIAN_POINT ( 'NONE',  ( -3.035961785846409301E-14, 2.999999999999988454, -1.857347330825986687 ) ) ;
#139106 = CARTESIAN_POINT ( 'NONE',  ( 1.873570696236816158, -0.2555354716398828274, 2.054483085851127377 ) ) ;
#139107 = CARTESIAN_POINT ( 'NONE',  ( -5.038826645773246682, 9.030381520044109322, 0.7998128361456481317 ) ) ;
#139108 = CARTESIAN_POINT ( 'NONE',  ( -4.736138090107036902, 8.221507128720061175, -0.6901939221467829899 ) ) ;
#139109 = CARTESIAN_POINT ( 'NONE',  ( 0.2687375195599971400, -1.410744835756465365, 1.637978619736128127 ) ) ;
#139110 = PRESENTATION_STYLE_ASSIGNMENT (( #172678 ) ) ;
#139111 = CARTESIAN_POINT ( 'NONE',  ( 3.445180431648313224, 7.033477913649446300, 0.7216878364870257245 ) ) ;
#139112 = CYLINDRICAL_SURFACE ( 'NONE', #75228, 9.499999999999992895 ) ;
#139113 = CARTESIAN_POINT ( 'NONE',  ( 4.390142812726693045, 4.016254791136236513, 1.214306433183764966E-14 ) ) ;
#139114 = CARTESIAN_POINT ( 'NONE',  ( -1.402160292154681736E-14, 12.48437500034139624, 1.575800808251682339 ) ) ;
#139116 = CARTESIAN_POINT ( 'NONE',  ( -5.284646014276622950, 9.387447126623207794, -0.7998128361456362523 ) ) ;
#139115 = CARTESIAN_POINT ( 'NONE',  ( 6.825078400183573812, 7.629137130509070275, 2.455651831298297338 ) ) ;
#139117 = CARTESIAN_POINT ( 'NONE',  ( 4.570818470097482766, -0.8114142876072638622, 1.532583664885181607 ) ) ;
#139118 = AXIS2_PLACEMENT_3D ( 'NONE', #154963, #72626, #48156 ) ;
#139119 = CARTESIAN_POINT ( 'NONE',  ( -4.603156847039612920, 5.329103395422994716, 1.199719254218462483 ) ) ;
#139120 = CARTESIAN_POINT ( 'NONE',  ( 2.254815949590884827, -0.5480598642870064818, -1.996355599893632649 ) ) ;
#139121 = CARTESIAN_POINT ( 'NONE',  ( 3.409862312649377003, -1.263030510572001885, -1.699084664797428479 ) ) ;
#139122 = CARTESIAN_POINT ( 'NONE',  ( 7.396136491454752715, 8.587579647240744407, 1.199719254218462483 ) ) ;
#139123 = CARTESIAN_POINT ( 'NONE',  ( 0.6823417656249899377, 3.676041667008085767, -1.181850606188754593 ) ) ;
#139124 = CARTESIAN_POINT ( 'NONE',  ( 1.990998161727207449, 0.1877779126488627881, 1.960439330322023999 ) ) ;
#139125 = CARTESIAN_POINT ( 'NONE',  ( 5.497327176576959573, 6.424397595302826502, 1.252573174869066941 ) ) ;
#139126 = CARTESIAN_POINT ( 'NONE',  ( 6.411931881972196610E-05, -0.8997486769052507327, 1.687471195204979457 ) ) ;
#139127 = CARTESIAN_POINT ( 'NONE',  ( 4.048992419199006321, -1.904907007256863904, -1.274792539085588539 ) ) ;
#139128 = CARTESIAN_POINT ( 'NONE',  ( 1.260069262837599791, 0.7379878962356714034, 1.670071910705408946 ) ) ;
#139129 = CARTESIAN_POINT ( 'NONE',  ( 6.378184920586140727, 6.405913593630768510, 0.000000000000000000 ) ) ;
#139130 = CARTESIAN_POINT ( 'NONE',  ( 6.114364089638798738, 6.235772314107808079, 0.7216878364870317197 ) ) ;
#139131 = CARTESIAN_POINT ( 'NONE',  ( -8.369460898337653276, 8.658792557682392754, 0.7998128361456462443 ) ) ;
#139132 = CARTESIAN_POINT ( 'NONE',  ( 2.636979257498579088, 1.897111442976556317, 0.6741904779793208569 ) ) ;
#139133 = CARTESIAN_POINT ( 'NONE',  ( 3.344534541303633368, -1.931932779036081183, -0.3399374921491463142 ) ) ;
#139134 = CARTESIAN_POINT ( 'NONE',  ( -7.133561379084627063, 11.47423870890741782, 0.7998128361456481317 ) ) ;
#139135 = CARTESIAN_POINT ( 'NONE',  ( -6.738566041191992539, 7.820414121934134322, 1.199719254218450271 ) ) ;
#139136 = CARTESIAN_POINT ( 'NONE',  ( -10.95308175811721085, 12.29999999999998295, 1.799999999999999600 ) ) ;
#139138 = CARTESIAN_POINT ( 'NONE',  ( 4.205725695155067889, -1.765064932122958785, 0.1306522685067777467 ) ) ;
#139137 = CARTESIAN_POINT ( 'NONE',  ( 6.439408583351804438, 0.8014019654560710082, -1.931139719275380084 ) ) ;
#139139 = CARTESIAN_POINT ( 'NONE',  ( -1.499999999999981126, 3.410416667349486897, -0.8660254037844499209 ) ) ;
#139140 = CARTESIAN_POINT ( 'NONE',  ( 0.8322822162843239724, 2.159637434087835928, 0.3711470721824081109 ) ) ;
#139141 = CARTESIAN_POINT ( 'NONE',  ( 5.771390581163715616, 1.041905927170128754, 1.393825671036960534 ) ) ;
#139142 = CIRCLE ( 'NONE', #7703, 0.04999999999999929501 ) ;
#139143 = CARTESIAN_POINT ( 'NONE',  ( 7.293396569147545527, 10.59638086639245280, 1.199719254218460707 ) ) ;
#139144 = CARTESIAN_POINT ( 'NONE',  ( 0.1331715793776418189, 2.029267568408019695, -2.369146612602909041 ) ) ;
#139145 = CARTESIAN_POINT ( 'NONE',  ( 6.434253291069976122, -1.843495385113643525, -1.373021106398547131 ) ) ;
#139146 = FACE_OUTER_BOUND ( 'NONE', #129481, .T. ) ;
#139147 = CARTESIAN_POINT ( 'NONE',  ( 5.466046595369183692, 1.418568314722228996, 0.9965602304959333413 ) ) ;
#139148 = CARTESIAN_POINT ( 'NONE',  ( 1.489210700298746692, -0.3264265768355456010, -2.182489157894373033 ) ) ;
#139149 = CARTESIAN_POINT ( 'NONE',  ( 5.459503713743925069, 1.771904602436706222, 1.254488129281390751 ) ) ;
#139150 = CARTESIAN_POINT ( 'NONE',  ( 2.737856954955798727, 5.281584649835344258, 1.199719254218452047 ) ) ;
#139151 = CARTESIAN_POINT ( 'NONE',  ( 0.8138397394129359697, -1.348031465540124207, -1.632742428372506049 ) ) ;
#139152 = CARTESIAN_POINT ( 'NONE',  ( 4.468750000000002665, 0.7852924748297492874, -1.895863743164178494 ) ) ;
#139153 = CARTESIAN_POINT ( 'NONE',  ( 6.827182134110223011, 1.235230467647760788, 2.302354205009625954 ) ) ;
#139154 = CARTESIAN_POINT ( 'NONE',  ( 4.436495903120683870, 1.889097993355067562, 0.3764034397915373975 ) ) ;
#139155 = CARTESIAN_POINT ( 'NONE',  ( 1.506789913206330489, -2.211016841974380309, -0.2134033219785695379 ) ) ;
#139156 = ORIENTED_EDGE ( 'NONE', *, *, #139088, .F. ) ;
#139157 = CARTESIAN_POINT ( 'NONE',  ( -0.7500000000000215383, 4.941666666666684193, 1.299038105676671107 ) ) ;
#139158 = CARTESIAN_POINT ( 'NONE',  ( 3.974511587100456822, 7.788680618259193444, 1.040834085586084257E-14 ) ) ;
#139159 = CARTESIAN_POINT ( 'NONE',  ( 6.551614543901692400, 8.666636272683888365, 1.599625672291281386 ) ) ;
#139160 = CARTESIAN_POINT ( 'NONE',  ( 4.002737143027909283, -2.197200394838841664, -0.3254818186308478523 ) ) ;
#139161 = CARTESIAN_POINT ( 'NONE',  ( -7.361714222540411967, 11.53249099303175385, 0.000000000000000000 ) ) ;
#139162 = CARTESIAN_POINT ( 'NONE',  ( -0.6681007961528204753, -4.204658361604701966, 0.8428154764861340853 ) ) ;
#139163 = CARTESIAN_POINT ( 'NONE',  ( 7.456621297836082185, 7.801739057004660971, 0.7216878364870317197 ) ) ;
#139164 = CARTESIAN_POINT ( 'NONE',  ( -7.985389288324685531, 12.26011190311341537, -0.7216878364870267237 ) ) ;
#139165 = CARTESIAN_POINT ( 'NONE',  ( 6.048345925472183637, 8.149765894507963182, 1.443375672974065660 ) ) ;
#139166 = CARTESIAN_POINT ( 'NONE',  ( 2.004529941291322448, -1.955172360644286789, 0.4926429297785542283 ) ) ;
#139168 = CARTESIAN_POINT ( 'NONE',  ( 6.795384964414455276, -1.844194740592384196, 0.9240657454356243639 ) ) ;
#139167 = CARTESIAN_POINT ( 'NONE',  ( 8.762647353133951711, 9.117510088278095282, 1.040834085586084257E-14 ) ) ;
#139169 = FACE_OUTER_BOUND ( 'NONE', #123494, .T. ) ;
#139170 = CARTESIAN_POINT ( 'NONE',  ( 5.790741006368192778, 8.809596036521288198, -1.082531754730548412 ) ) ;
#139171 = CARTESIAN_POINT ( 'NONE',  ( 6.198757988109700356, 1.452298656357524864, 0.9588401209737663633 ) ) ;
#139172 = DIRECTION ( 'NONE',  ( 1.000000000000000000, 0.000000000000000000, 0.000000000000000000 ) ) ;
#139173 = CARTESIAN_POINT ( 'NONE',  ( 1.364683531249988535, 1.863541667008086211, 0.7879004041258500513 ) ) ;
#139174 = CARTESIAN_POINT ( 'NONE',  ( 1.528175773270981308, 1.703719318302211683, 0.4785495757857262666 ) ) ;
#139175 = CARTESIAN_POINT ( 'NONE',  ( 0.4225002777262388265, -1.427939226333583500, -1.423959630194884696 ) ) ;
#139176 = CARTESIAN_POINT ( 'NONE',  ( 6.198757988109700356, 1.452298656357524864, 0.9588401209737663633 ) ) ;
#139177 = CARTESIAN_POINT ( 'NONE',  ( 4.230218865515364968, 2.248128804489764043, 0.4474220685124987162 ) ) ;
#139178 = CARTESIAN_POINT ( 'NONE',  ( 2.132514540308296791, -1.644867172388216003, 0.8273176719292076875 ) ) ;
#139179 = CARTESIAN_POINT ( 'NONE',  ( 10.58621901417202515, 11.24501035948919991, -0.7998128361456281477 ) ) ;
#139180 = CARTESIAN_POINT ( 'NONE',  ( 9.086253353280449474, 13.40000000000000036, 7.838367176906169576 ) ) ;
#139181 = CARTESIAN_POINT ( 'NONE',  ( 3.381694320706640333, 1.157239582903809128, 1.411935816614327655 ) ) ;
#139182 = CARTESIAN_POINT ( 'NONE',  ( 3.850232551101365086, 0.2440307281281335616, -2.001511205109906655 ) ) ;
#139183 = CARTESIAN_POINT ( 'NONE',  ( -7.967387826325084355, 12.44703623068796361, 0.7998128361456481317 ) ) ;
#139185 = CYLINDRICAL_SURFACE ( 'NONE', #152111, 1.500000000000000222 ) ;
#139184 = CARTESIAN_POINT ( 'NONE',  ( 3.801889278938491934, -0.6593813483589389124, 2.164292034026161549 ) ) ;
#139186 = CARTESIAN_POINT ( 'NONE',  ( 5.174884205284945082, -1.981925234046210571, -0.7124256662833851061 ) ) ;
#139187 = CARTESIAN_POINT ( 'NONE',  ( 9.410656278130334229, 14.12788591601509758, 8.484697815724119963 ) ) ;
#139188 = CARTESIAN_POINT ( 'NONE',  ( 2.611853368047814872, 0.5545374748289233491, -1.994631108499920646 ) ) ;
#139189 = CARTESIAN_POINT ( 'NONE',  ( 3.999819011231439347, 4.625209253646830554, 1.199719254218464037 ) ) ;
#139190 = CARTESIAN_POINT ( 'NONE',  ( 1.360316468749980023, 0.7968750003414099004, -3.122502256758252770E-14 ) ) ;
#139191 = CARTESIAN_POINT ( 'NONE',  ( 5.496778590849229040, -2.068848325035842706, -0.4644329061709790429 ) ) ;
#139194 = EDGE_CURVE ( 'NONE', #162079, #185175, #15507, .T. ) ;
#139193 = CARTESIAN_POINT ( 'NONE',  ( 1.066875820281657949, -1.741210523058086324, -0.8246449397346886645 ) ) ;
#139192 = CARTESIAN_POINT ( 'NONE',  ( -9.236128959407555072, 11.79856975744075598, -1.599625672291263179 ) ) ;
#139195 = CARTESIAN_POINT ( 'NONE',  ( -4.329849954717889915, 6.144853928627882489, 1.599625672291270506 ) ) ;
#139196 = CARTESIAN_POINT ( 'NONE',  ( 7.801827329660018684, 11.18955008699033726, 1.199719254218460707 ) ) ;
#139197 = CARTESIAN_POINT ( 'NONE',  ( 6.224601922005513543, 7.395028676162137771, -1.082531754730548412 ) ) ;
#139198 = CARTESIAN_POINT ( 'NONE',  ( 4.464323212750023195, 7.049731028713583925, 1.131627047429624167 ) ) ;
#139199 = DIRECTION ( 'NONE',  ( 0.000000000000000000, -1.000000000000000000, 0.000000000000000000 ) ) ;
#139200 = CARTESIAN_POINT ( 'NONE',  ( -3.741160322367112379, 6.452105245148518797, 1.199719254218464037 ) ) ;
#139201 = CARTESIAN_POINT ( 'NONE',  ( 0.7564555125054818197, 0.8934716743186126298, -2.033981271184843731 ) ) ;
#139202 = CARTESIAN_POINT ( 'NONE',  ( 1.940588816512535120, 2.082954711654343427, 0.3096100588686269695 ) ) ;
#139203 = CARTESIAN_POINT ( 'NONE',  ( -7.587723245503481095, 8.881373870289390737, 1.199719254218452047 ) ) ;
#139204 = CARTESIAN_POINT ( 'NONE',  ( 7.564559641420864899, 10.91273778404466199, -1.199719254218446718 ) ) ;
#139205 = CARTESIAN_POINT ( 'NONE',  ( 6.174622966819019787, 1.250768081284852951, -1.378062710742117059 ) ) ;
#139206 = CARTESIAN_POINT ( 'NONE',  ( 7.019370843573166319, 9.212351955633947043, 1.599625672291281386 ) ) ;
#139207 = CARTESIAN_POINT ( 'NONE',  ( -7.322812365156824654, 8.676274193172000437, 1.082531754730549078 ) ) ;
#139208 = AXIS2_PLACEMENT_3D ( 'NONE', #111541, #127824, #129941 ) ;
#139209 = CARTESIAN_POINT ( 'NONE',  ( 0.3344391967911933272, -1.139684030083350841, -1.788147294700337397 ) ) ;
#139210 = CARTESIAN_POINT ( 'NONE',  ( -5.912237504011027767, 9.055304967058290799, 1.199719254218454489 ) ) ;
#139212 = CARTESIAN_POINT ( 'NONE',  ( 3.174217076811707727, -0.9646401420641316227, -1.708233030250068785 ) ) ;
#139211 = CARTESIAN_POINT ( 'NONE',  ( -7.761958760141988650E-14, -0.3124999999999614197, -1.414508159514597407 ) ) ;
#139213 = CARTESIAN_POINT ( 'NONE',  ( 2.501032641837992454, 1.736685530831501456, -1.287010829427559289 ) ) ;
#139214 = CARTESIAN_POINT ( 'NONE',  ( 1.012948470060770934, -1.796336717620912626, 0.4034172393945419377 ) ) ;
#139215 = CIRCLE ( 'NONE', #45842, 0.2000000000000005107 ) ;
#139217 = CARTESIAN_POINT ( 'NONE',  ( -4.744851797206062649, 6.824086272657805985, -1.238183395270262999 ) ) ;
#139216 = CARTESIAN_POINT ( 'NONE',  ( -5.632486471834530661, 5.535932070087196344, -0.7998128361456362523 ) ) ;
#139218 = CARTESIAN_POINT ( 'NONE',  ( 3.081702191724482454, -1.714667182045168214, -0.2967042344550906985 ) ) ;
#139219 = CARTESIAN_POINT ( 'NONE',  ( 6.480434237652132445, 7.623223367758051872, 1.082531754730558626 ) ) ;
#139220 = CARTESIAN_POINT ( 'NONE',  ( -11.31087111570240467, 5.182330806778288057, -5.726608797552268371 ) ) ;
#139221 = CARTESIAN_POINT ( 'NONE',  ( 1.235488887756378551, -1.954010380348418119, 0.9248176494114216384 ) ) ;
#139222 = CARTESIAN_POINT ( 'NONE',  ( 2.214220036344019871, -1.617569417291262690, -1.203170845901546215 ) ) ;
#139223 = CARTESIAN_POINT ( 'NONE',  ( -3.022498986271275001, 2.800000000000024691, 2.500000000000011102 ) ) ;
#139224 = CARTESIAN_POINT ( 'NONE',  ( 0.6378455412261313517, -1.529572671500577297, -1.527792216034072670 ) ) ;
#139225 = EDGE_CURVE ( 'NONE', #92745, #148246, #157723, .T. ) ;
#139226 = CARTESIAN_POINT ( 'NONE',  ( 2.307442625383813617, -0.4335913300187159702, 1.923040929009907973 ) ) ;
#139227 = CARTESIAN_POINT ( 'NONE',  ( 2.993041990875914493, 6.420974562437304911, 0.3677586026352899218 ) ) ;
#139230 = ORIENTED_EDGE ( 'NONE', *, *, #112332, .T. ) ;
#139229 = CARTESIAN_POINT ( 'NONE',  ( -4.014622883422322985, 7.697827440719083647, -0.7216878364870458196 ) ) ;
#139228 = CARTESIAN_POINT ( 'NONE',  ( 11.01135777277262306, 11.00632581993708570, 1.399999999999998579 ) ) ;
#139231 = CARTESIAN_POINT ( 'NONE',  ( -6.414416072596857532, 6.656109304217339151, -0.7216878364870338292 ) ) ;
#139232 = CARTESIAN_POINT ( 'NONE',  ( -0.2108831679770926115, 5.723481173670196043, -2.491210874135452613 ) ) ;
#139233 = CARTESIAN_POINT ( 'NONE',  ( 6.384963997392946844, 6.413822516572072807, 0.7998128361456352531 ) ) ;
#139234 = CARTESIAN_POINT ( 'NONE',  ( -5.336015975430226099, 8.383046517047350932, -1.199719254218453823 ) ) ;
#139235 = CARTESIAN_POINT ( 'NONE',  ( 2.684245096118286877, 1.082265567382127758, 1.705031398228576078 ) ) ;
#139236 = CARTESIAN_POINT ( 'NONE',  ( -6.740338644649361832, 7.892758502626242567, -1.199719254218452047 ) ) ;
#139237 = CARTESIAN_POINT ( 'NONE',  ( -10.10046125205658463, 11.84658821789661509, -1.082531754730537976 ) ) ;
#139238 = CARTESIAN_POINT ( 'NONE',  ( 5.737451576302465384, -2.089288847444936259, 0.9800045452074584995 ) ) ;
#139239 = CARTESIAN_POINT ( 'NONE',  ( 6.654749070045313353, -0.5220710138904552933, -1.891073168474053823 ) ) ;
#139240 = CARTESIAN_POINT ( 'NONE',  ( 4.188298518248589453, 1.053080760608171129, -1.654974388233184657 ) ) ;
#139241 =( BOUNDED_SURFACE ( )  B_SPLINE_SURFACE ( 3, 2, ( 
 ( #158383, #27291, #174650 ),
 ( #156256, #175701, #11033 ),
 ( #91263, #24088, #26226 ),
 ( #92342, #141102, #93399 ),
 ( #189798, #142155, #73926 ),
 ( #59801, #43578, #106475 ),
 ( #127030, #172502, #39287 ),
 ( #143235, #89126, #105382 ),
 ( #171421, #109698, #155180 ),
 ( #90193, #6764, #190855 ),
 ( #42516, #125958, #72839 ),
 ( #138943, #204964, #7835 ) ),
 .UNSPECIFIED., .F., .F., .T. ) 
 B_SPLINE_SURFACE_WITH_KNOTS ( ( 4, 2, 2, 2, 2, 4 ),
 ( 3, 3 ),
 ( 6.288372600415925717E-18, 0.001066554601603806208, 0.001599831902405706276, 0.002133109203207606344, 0.003199663804811406480, 0.004266218406415206617 ),
 ( 0.000000000000000000, 1.000000000000000000 ),
 .UNSPECIFIED. ) 
 GEOMETRIC_REPRESENTATION_ITEM ( )  RATIONAL_B_SPLINE_SURFACE ( (
 ( 1.000000000000000000, 0.8509626965198142656, 1.000000000000000000),
 ( 1.000000000000000000, 0.8509149327537995910, 1.000000000000000000),
 ( 1.000000000000000000, 0.8506374068021691492, 1.000000000000000000),
 ( 1.000000000000000000, 0.8504793255920759520, 1.000000000000000000),
 ( 1.000000000000000000, 0.8504520640024009204, 1.000000000000000000),
 ( 1.000000000000000000, 0.8502690826081933384, 1.000000000000000000),
 ( 1.000000000000000000, 0.8502072942086275065, 1.000000000000000000),
 ( 1.000000000000000000, 0.8489325510347147663, 1.000000000000000000),
 ( 1.000000000000000000, 0.8474238666478376425, 1.000000000000000000),
 ( 1.000000000000000000, 0.8452420265713719294, 1.000000000000000000),
 ( 1.000000000000000000, 0.8443493681871490075, 1.000000000000000000),
 ( 1.000000000000000000, 0.8435444081809017058, 1.000000000000000000) ) ) 
 REPRESENTATION_ITEM ( '' )  SURFACE ( )  );
#139242 = CARTESIAN_POINT ( 'NONE',  ( 8.121497709785879593, 9.433834401960398353, -1.199719254218445830 ) ) ;
#139243 = CARTESIAN_POINT ( 'NONE',  ( 0.1060925565549031974, -0.09613213100253051313, 2.014232862735332308 ) ) ;
#139244 = ORIENTED_EDGE ( 'NONE', *, *, #100257, .T. ) ;
#139245 = CARTESIAN_POINT ( 'NONE',  ( 1.973964399615803389, -0.9004667817871301327, 1.916432390954267984 ) ) ;
#139246 = CARTESIAN_POINT ( 'NONE',  ( -1.500000000000015099, 1.160416667349484898, -0.8660254037844313801 ) ) ;
#139248 = CARTESIAN_POINT ( 'NONE',  ( -7.043624497499477499, 8.176315654292865887, 1.199719254218450271 ) ) ;
#139247 = CARTESIAN_POINT ( 'NONE',  ( -10.30923643716943872, 0.9706168436483918471, 5.952040432139342307 ) ) ;
#139249 = CARTESIAN_POINT ( 'NONE',  ( 2.413779523973126118, 1.202770565240804279, -1.394052804434331216 ) ) ;
#139250 = ORIENTED_EDGE ( 'NONE', *, *, #79113, .T. ) ;
#139251 = CARTESIAN_POINT ( 'NONE',  ( -8.611400122974211868, 13.19838391011195888, 1.040834085586084257E-14 ) ) ;
#139252 = CARTESIAN_POINT ( 'NONE',  ( 9.527611255715328298, 12.67370358187078239, 7.222190795531108876 ) ) ;
#139253 = CARTESIAN_POINT ( 'NONE',  ( 3.726904977748810133, 1.497142547446396410, -1.502090761940577002 ) ) ;
#139254 = CARTESIAN_POINT ( 'NONE',  ( 0.09336763325077861164, -1.840659761701424646, -0.04852334659839750014 ) ) ;
#139255 = CARTESIAN_POINT ( 'NONE',  ( 1.499999999999990896, 5.306250000682820378, 1.214306433183764966E-14 ) ) ;
#139256 = B_SPLINE_CURVE_WITH_KNOTS ( 'NONE', 3,
 ( #63938, #198185, #199241, #50888, #165704, #83368 ),
 .UNSPECIFIED., .F., .F.,
 ( 4, 2, 4 ),
 ( 5.135960789614000585E-18, 0.001422024648551338099, 0.002844049297102670994 ),
 .UNSPECIFIED. ) ;
#139257 = CARTESIAN_POINT ( 'NONE',  ( 6.428537391173986038, 10.65171072301167854, 0.7998128361456462443 ) ) ;
#139258 = CARTESIAN_POINT ( 'NONE',  ( 5.528692779322568640, 9.672168352510192690, 0.7998128361456341429 ) ) ;
#139259 = CARTESIAN_POINT ( 'NONE',  ( 4.604794268142059721, 1.595455460008918580, -1.304385708662815002 ) ) ;
#139260 = AXIS2_PLACEMENT_3D ( 'NONE', #212326, #165730, #179856 ) ;
#139262 = CARTESIAN_POINT ( 'NONE',  ( 1.522747961674526085, -1.733470594775164075, 0.6210259959333885860 ) ) ;
#139261 = CARTESIAN_POINT ( 'NONE',  ( -7.725448601688521322, 7.907444878258402809, 1.040834085586084257E-14 ) ) ;
#139263 = CARTESIAN_POINT ( 'NONE',  ( 1.364683531249988535, 5.155208333674749177, -0.7879004041258300672 ) ) ;
#139264 = FILL_AREA_STYLE ('',( #186920 ) ) ;
#139265 = CARTESIAN_POINT ( 'NONE',  ( 0.000000000000000000, 3.499999999999989342, 0.000000000000000000 ) ) ;
#139266 = DIRECTION ( 'NONE',  ( 0.000000000000000000, 1.000000000000000000, 0.000000000000000000 ) ) ;
#139267 = CARTESIAN_POINT ( 'NONE',  ( 0.6278963055918493907, -2.094311335337955882, 0.6960538111202837497 ) ) ;
#139268 = CARTESIAN_POINT ( 'NONE',  ( 3.251526197659323270, -1.847530484110882387, -1.305540666510462078 ) ) ;
#139269 = CARTESIAN_POINT ( 'NONE',  ( -6.860062538834774237, 10.94723069537516302, 0.7216878364870458196 ) ) ;
#139270 = CARTESIAN_POINT ( 'NONE',  ( 3.287185820011778947, 0.03942761580559561718, -1.811315726287704431 ) ) ;
#139271 = CARTESIAN_POINT ( 'NONE',  ( 3.731564767512856040, 0.6402975007456043199, -1.805710188498848456 ) ) ;
#139272 = CARTESIAN_POINT ( 'NONE',  ( 5.477033855465498924, 1.911541192706748715, 0.7957256658025002594 ) ) ;
#139273 = CARTESIAN_POINT ( 'NONE',  ( -1.364683531250012516, 4.551041667008082214, -0.7879004041258300672 ) ) ;
#139274 = CARTESIAN_POINT ( 'NONE',  ( 2.360178788647437464, 0.8414710005770206225, 1.782988266942896693 ) ) ;
#139275 = CARTESIAN_POINT ( 'NONE',  ( 0.7449895426413064570, -1.653788825565579046, 0.9876836116205435223 ) ) ;
#139276 = CARTESIAN_POINT ( 'NONE',  ( 3.485083742438867649, 1.691615344724434200, -0.7988839237506044633 ) ) ;
#139277 = CARTESIAN_POINT ( 'NONE',  ( 1.946342613620454243, 0.8805590942474375016, -2.133279852835685109 ) ) ;
#139278 = CARTESIAN_POINT ( 'NONE',  ( 3.648742529127374734, -0.3609857515115758586, -1.825517407628447053 ) ) ;
#139279 = CARTESIAN_POINT ( 'NONE',  ( 0.6823417656249917140, 3.842708333674754506, 1.181850606188765695 ) ) ;
#139280 = COLOUR_RGB ( '', 0.08235294, 0.09019608, 0.10196078) ;
#139282 = CARTESIAN_POINT ( 'NONE',  ( -3.262708522383007903, 6.958243709422141876, 1.040834085586084257E-14 ) ) ;
#139281 = AXIS2_PLACEMENT_3D ( 'NONE', #82505, #116142, #35890 ) ;
#139283 = CARTESIAN_POINT ( 'NONE',  ( 6.745345117998789775, 7.828323044875442172, 1.199719254218462483 ) ) ;
#139284 = CARTESIAN_POINT ( 'NONE',  ( 11.04536101718726293, 10.09537905954598180, 1.099999999999999201 ) ) ;
#139285 = CARTESIAN_POINT ( 'NONE',  ( 0.4871192430246041316, -0.2598372338927424918, -2.089908867234680834 ) ) ;
#139286 = CARTESIAN_POINT ( 'NONE',  ( 3.917943204224906939, 5.594019709727598766, -1.443375672974051449 ) ) ;
#139288 = LINE ( 'NONE', #170695, #18101 ) ;
#139287 = CARTESIAN_POINT ( 'NONE',  ( -1.364683531250010295, 5.342708333674750953, 0.7879004041258379498 ) ) ;
#139289 = CARTESIAN_POINT ( 'NONE',  ( 1.705496241919310707, 1.842552997918958768, -1.049655202612943095 ) ) ;
#139290 = CYLINDRICAL_SURFACE ( 'NONE', #9898, 1.500000000000000222 ) ;
#139291 = CARTESIAN_POINT ( 'NONE',  ( 0.3869806665078223129, -1.903265420633104332, -0.6765555904410057719 ) ) ;
#139292 = CARTESIAN_POINT ( 'NONE',  ( 0.6823417656249882723, 0.6760416670080898749, -1.181850606188749264 ) ) ;
#139293 = CARTESIAN_POINT ( 'NONE',  ( -2.629918611371007575, 6.012062780000711371, 0.7216878364870317197 ) ) ;
#139294 = CARTESIAN_POINT ( 'NONE',  ( 4.150767584078112193, 7.994312614733129152, 0.7998128361456321445 ) ) ;
#139295 = ORIENTED_EDGE ( 'NONE', *, *, #52572, .F. ) ;
#139296 = CARTESIAN_POINT ( 'NONE',  ( 1.493687833870473325, 1.635750924671933282, 1.413141523588061776 ) ) ;
#139297 = DIRECTION ( 'NONE',  ( 0.000000000000000000, 0.000000000000000000, 1.000000000000000000 ) ) ;
#139300 = CARTESIAN_POINT ( 'NONE',  ( 3.660338286009610975, 6.253849852777763729, -1.082531754730543083 ) ) ;
#139299 = DIRECTION ( 'NONE',  ( 1.000000000000000000, -0.000000000000000000, 1.779758311459929752E-16 ) ) ;
#139298 = CARTESIAN_POINT ( 'NONE',  ( 5.899733120602060232, 6.912052057904395141, -1.199719254218452047 ) ) ;
#139301 = CARTESIAN_POINT ( 'NONE',  ( -3.654804927335652209, 6.421633627603656080, 1.199719254218452935 ) ) ;
#139302 = CARTESIAN_POINT ( 'NONE',  ( 5.876185452347599814, -2.007255679753978228, -0.1928398672442974138 ) ) ;
#139303 = CARTESIAN_POINT ( 'NONE',  ( -8.866669273657352690, 9.446795028796142191, 0.7216878364870438212 ) ) ;
#139304 = CARTESIAN_POINT ( 'NONE',  ( 0.1874131419884322858, 1.628132678060219884, 1.467219630700428157 ) ) ;
#139305 = DIRECTION ( 'NONE',  ( -1.276756478318932585E-15, 1.000000000000000000, -1.665334536937738262E-16 ) ) ;
#139307 = CARTESIAN_POINT ( 'NONE',  ( -1.402160292154681736E-14, 10.92187500034139802, 1.575800808251682339 ) ) ;
#139306 = CARTESIAN_POINT ( 'NONE',  ( 6.825078400183575589, -0.005632053428735600553, 2.144262460745151255 ) ) ;
#139308 = CARTESIAN_POINT ( 'NONE',  ( -8.136864746495904299, 12.64475930422059768, -0.7998128361456281477 ) ) ;
#139310 = CARTESIAN_POINT ( 'NONE',  ( 0.8783700953360704666, -0.4667435877003899836, -1.857722024819864037 ) ) ;
#139309 = CARTESIAN_POINT ( 'NONE',  ( -5.056828107772860292, 6.922718763866881453, -1.443375672974051449 ) ) ;
#139311 = CARTESIAN_POINT ( 'NONE',  ( -1.364683531250014514, 0.3427083336747508424, 0.7879004041258379498 ) ) ;
#139312 = CARTESIAN_POINT ( 'NONE',  ( -0.4694063952341946955, -6.893137084989842123, -10.98997987423602751 ) ) ;
#139313 = VECTOR ( 'NONE', #11204, 1000.000000000000000 ) ;
#139314 = CARTESIAN_POINT ( 'NONE',  ( 0.000000000000000000, 0.000000000000000000, 0.000000000000000000 ) ) ;
#139315 = CARTESIAN_POINT ( 'NONE',  ( 2.965164839364425653, 0.2526306750327989015, -1.706137528056344888 ) ) ;
#139316 = CARTESIAN_POINT ( 'NONE',  ( 4.583538449871731757, 7.505156070562471804, 1.199719254218451159 ) ) ;
#139317 = CARTESIAN_POINT ( 'NONE',  ( 1.493014682725684938, 1.335586794047480153, 1.161194053514543745 ) ) ;
#139318 = CARTESIAN_POINT ( 'NONE',  ( 1.664698924820615433, 0.6334283372178346472, 1.910891431425953302 ) ) ;
#139319 = FILL_AREA_STYLE ('',( #207491 ) ) ;
#139320 = CARTESIAN_POINT ( 'NONE',  ( 3.733602637680955461, -2.039903990487580643, 0.8422819887162477093 ) ) ;
#139321 = ORIENTED_EDGE ( 'NONE', *, *, #73148, .F. ) ;
#139322 = CARTESIAN_POINT ( 'NONE',  ( 9.070041577417981671, 9.684062716516882219, -0.7216878364870197293 ) ) ;
#139323 = CARTESIAN_POINT ( 'NONE',  ( -6.912678218121246942, 9.158153569265168770, 1.599625672291269396 ) ) ;
#139325 = CARTESIAN_POINT ( 'NONE',  ( 4.394157760337158436, -0.8647400765994192051, -1.821735888681835336 ) ) ;
#139324 = CARTESIAN_POINT ( 'NONE',  ( 3.897227946829431300, -0.2092540311423168320, -2.110150122182581356 ) ) ;
#139327 = ORIENTED_EDGE ( 'NONE', *, *, #66049, .T. ) ;
#139326 = CARTESIAN_POINT ( 'NONE',  ( 4.464998409566146798, -1.450835031669978292, 1.084616504919968305 ) ) ;
#139328 = CARTESIAN_POINT ( 'NONE',  ( 5.899733120602060232, 6.912052057904395141, -1.199719254218452047 ) ) ;
#139329 = ORIENTED_EDGE ( 'NONE', *, *, #38831, .T. ) ;
#139330 = EDGE_CURVE ( 'NONE', #27240, #128202, #68518, .T. ) ;
#139331 = CARTESIAN_POINT ( 'NONE',  ( 1.111929834214450796, -0.8377583890188080584, -1.672643128629976772 ) ) ;
#139332 = CARTESIAN_POINT ( 'NONE',  ( -10.39230484541323740, 3.447199233515621408, 6.000000000000048850 ) ) ;
#139333 = CARTESIAN_POINT ( 'NONE',  ( -2.117044542028253318, 5.621635732341564662, -0.7998128361456281477 ) ) ;
#139334 = LINE ( 'NONE', #171816, #16695 ) ;
#139335 = CARTESIAN_POINT ( 'NONE',  ( -3.602337597214539753E-15, 11.84375000068279604, 1.500000000000001554 ) ) ;
#139336 = CARTESIAN_POINT ( 'NONE',  ( 1.364683531249988535, 3.467708333674749621, -0.7879004041258239610 ) ) ;
#139337 = DIRECTION ( 'NONE',  ( 0.6483454320283800199, 0.000000000000000000, -0.7613463080411787542 ) ) ;
#139338 = B_SPLINE_CURVE_WITH_KNOTS ( 'NONE', 3,
 ( #143453, #62169, #208391, #212657, #79476, #194291 ),
 .UNSPECIFIED., .F., .F.,
 ( 4, 2, 4 ),
 ( 1.685978275629812889E-15, 0.0001724549256341273700, 0.0003449098512665687514 ),
 .UNSPECIFIED. ) ;
#139339 = CARTESIAN_POINT ( 'NONE',  ( 6.319508997745523438, 9.426492026461511742, -1.082531754730548412 ) ) ;
#139340 = CARTESIAN_POINT ( 'NONE',  ( -4.014622883422329203, 6.737458226417744278, -1.082531754730546636 ) ) ;
#139341 = CARTESIAN_POINT ( 'NONE',  ( -5.936491157937300756, 8.019268665717216749, 1.599625672291263179 ) ) ;
#139342 = CARTESIAN_POINT ( 'NONE',  ( 4.676102344489991403, 2.097148071331572439, -0.3138259731317455392 ) ) ;
#139344 = CARTESIAN_POINT ( 'NONE',  ( -10.12885446735897510, 6.153639267710001803, -5.673676530672286944 ) ) ;
#139343 = CARTESIAN_POINT ( 'NONE',  ( -0.1294898018152201291, 4.092224548688067287, -2.481517387982924649 ) ) ;
#139345 = CARTESIAN_POINT ( 'NONE',  ( 5.817641553194794035, -1.923906765362886961, 0.4292884390787749527 ) ) ;
#139346 = CARTESIAN_POINT ( 'NONE',  ( -1.364683531250000748, 1.759375000341421913, 0.000000000000000000 ) ) ;
#139347 = CARTESIAN_POINT ( 'NONE',  ( 0.9143154035033382865, -2.013376230895477903, 0.004183558276700528357 ) ) ;
#139348 = EDGE_LOOP ( 'NONE', ( #27683, #129031, #148546, #98698 ) ) ;
#139349 = CARTESIAN_POINT ( 'NONE',  ( 6.503150284217945831, -0.1439854277452867481, 2.084527530714448407 ) ) ;
#139350 = CARTESIAN_POINT ( 'NONE',  ( 8.868224039976556838, 12.79319246706557678, 8.085344725444658209 ) ) ;
#139351 = CARTESIAN_POINT ( 'NONE',  ( 1.047426762419433777, 1.826728496382063582, -0.9743617655595809834 ) ) ;
#139352 = ORIENTED_EDGE ( 'NONE', *, *, #55232, .F. ) ;
#139353 = CARTESIAN_POINT ( 'NONE',  ( 4.420840606507738357, 7.315341919971147355, 1.199719254218451159 ) ) ;
#139354 = CARTESIAN_POINT ( 'NONE',  ( 5.200434439293556643, 8.224868058221247225, -1.199719254218452047 ) ) ;
#139356 = CARTESIAN_POINT ( 'NONE',  ( 6.017121246366603060, 5.914396297049491658, 1.040834085586084257E-14 ) ) ;
#139355 = CARTESIAN_POINT ( 'NONE',  ( 3.046908718545093819, -1.709425224762064266, -1.203301715110078662 ) ) ;
#139357 = CARTESIAN_POINT ( 'NONE',  ( 7.038618024149998043, 8.240751112043669835, -1.199719254218452047 ) ) ;
#139360 = VERTEX_POINT ( 'NONE', #305 ) ;
#139359 = CARTESIAN_POINT ( 'NONE',  ( 1.664434086620687703, 0.5685959063129341073, 1.719966406682835958 ) ) ;
#139358 = CARTESIAN_POINT ( 'NONE',  ( 2.221465439867484903, -1.771451409125622600, 0.4407646962370226351 ) ) ;
#139361 = CARTESIAN_POINT ( 'NONE',  ( 5.022202109028018668, -1.178465353167540197, -1.865713892744431446 ) ) ;
#139362 = CARTESIAN_POINT ( 'NONE',  ( 0.000000000000000000, 0.000000000000000000, 0.000000000000000000 ) ) ;
#139363 = CARTESIAN_POINT ( 'NONE',  ( 3.874219531129017291, 1.223701582695544632, 1.836212042189053761 ) ) ;
#139364 = CARTESIAN_POINT ( 'NONE',  ( -0.6823417656250003738, 8.463541667008064096, 1.181850606188754593 ) ) ;
#139365 = CARTESIAN_POINT ( 'NONE',  ( 2.895058368816882499, -0.1428820475998151818, -1.907012587803847303 ) ) ;
#139366 = CARTESIAN_POINT ( 'NONE',  ( 7.262363838414439776, 11.62450824479221900, 0.7998128361456462443 ) ) ;
#139367 = CARTESIAN_POINT ( 'NONE',  ( 5.371561628297467195, -0.3073141173523045167, 2.047320497149993646 ) ) ;
#139368 =( GEOMETRIC_REPRESENTATION_CONTEXT ( 3 ) GLOBAL_UNCERTAINTY_ASSIGNED_CONTEXT ( ( #170606 ) ) GLOBAL_UNIT_ASSIGNED_CONTEXT ( ( #138785, #136651, #39140 ) ) REPRESENTATION_CONTEXT ( 'NONE', 'WORKASPACE' ) );
#139369 = CARTESIAN_POINT ( 'NONE',  ( 1.546240757466833093, 8.694816975860053532, -2.507471980975701342 ) ) ;
#139370 = CARTESIAN_POINT ( 'NONE',  ( 5.548420995840112724, -1.728225626343689925, 1.347513067664840358 ) ) ;
#139371 = CARTESIAN_POINT ( 'NONE',  ( 5.461903044330952639, 7.609029316319980474, -1.335476589331906494 ) ) ;
#139372 = EDGE_LOOP ( 'NONE', ( #169601, #6145, #45082, #29397 ) ) ;
#139373 = DIRECTION ( 'NONE',  ( 0.000000000000000000, 0.000000000000000000, 1.000000000000000000 ) ) ;
#139374 = CARTESIAN_POINT ( 'NONE',  ( 3.739016502318667445, 7.584212696005614873, 0.7998128361456271485 ) ) ;
#139375 = CARTESIAN_POINT ( 'NONE',  ( 3.285556943749998737, -2.092708332855377051, -1.896917185911906722 ) ) ;
#139376 = DIRECTION ( 'NONE',  ( -0.000000000000000000, -1.000000000000000000, -0.000000000000000000 ) ) ;
#139377 = CARTESIAN_POINT ( 'NONE',  ( -7.212574532790092974, 10.39812547402169862, -1.082531754730543971 ) ) ;
#139378 = CARTESIAN_POINT ( 'NONE',  ( 4.411198876399872404, 6.239761003923544713, -1.599625672291273171 ) ) ;
#139379 = CARTESIAN_POINT ( 'NONE',  ( 6.350451050988413115, -2.059726887988411637, -0.2088473404622398499 ) ) ;
#139381 = EDGE_CURVE ( 'NONE', #79131, #139750, #82653, .T. ) ;
#139380 = CARTESIAN_POINT ( 'NONE',  ( 4.934167778409569216, 0.9889366926784399769, -1.653171546959011140 ) ) ;
#139382 = CARTESIAN_POINT ( 'NONE',  ( 1.282827611874960416, 1.646826022920354848, -1.163289555428485667 ) ) ;
#139383 = CARTESIAN_POINT ( 'NONE',  ( -9.996439331977562404, 10.55693406359564790, 0.7998128361456462443 ) ) ;
#139384 = CARTESIAN_POINT ( 'NONE',  ( 5.820193082016415609, 10.01225203898631655, 0.000000000000000000 ) ) ;
#139385 = CARTESIAN_POINT ( 'NONE',  ( 0.7500000000000006661, 13.16666666666666607, -1.299038105676657340 ) ) ;
#139386 = CARTESIAN_POINT ( 'NONE',  ( 1.834175572193702530, 2.167931929539984814, 0.3193665180123914094 ) ) ;
#139387 = CARTESIAN_POINT ( 'NONE',  ( 5.268108045213575785, 0.9031548532531764595, 1.586571422427636824 ) ) ;
#139388 = CARTESIAN_POINT ( 'NONE',  ( 5.804299160426222848, 7.865044668620976509, -1.443375672974078761 ) ) ;
#139389 = CARTESIAN_POINT ( 'NONE',  ( 9.856941372335116469, 11.45851867493453291, 1.199719254218450271 ) ) ;
#139390 = CARTESIAN_POINT ( 'NONE',  ( -5.336015975430226099, 8.383046517047350932, -1.199719254218453823 ) ) ;
#139391 = CARTESIAN_POINT ( 'NONE',  ( 4.599240423533799138, 6.388866465587984322, 1.599625672291267398 ) ) ;
#139392 = CARTESIAN_POINT ( 'NONE',  ( 6.021229618244865023, 10.03886863134542828, -0.7216878364870458196 ) ) ;
#139393 = VERTEX_POINT ( 'NONE', #65318 ) ;
#139395 = CARTESIAN_POINT ( 'NONE',  ( 6.152595719530761009, 1.991896818749523845, 0.2912318779872117847 ) ) ;
#139394 = CARTESIAN_POINT ( 'NONE',  ( 2.384105128782065819, -0.3166398734758494315, -1.813660976904336808 ) ) ;
#139396 = CARTESIAN_POINT ( 'NONE',  ( 1.863111423135884293, -0.7740270289045609875, 2.164224664766948525 ) ) ;
#139397 = CARTESIAN_POINT ( 'NONE',  ( 6.297705697576845729, -1.418553083497756884, -1.355282376159852475 ) ) ;
#139398 = CARTESIAN_POINT ( 'NONE',  ( -6.905180308061733996, 6.950465202360470052, 0.7998128361456341429 ) ) ;
#139399 = LINE ( 'NONE', #205432, #8815 ) ;
#139400 = CARTESIAN_POINT ( 'NONE',  ( 3.410326831400651404, -1.910418641682644969, -0.08914582809275289899 ) ) ;
#139401 = CARTESIAN_POINT ( 'NONE',  ( -2.449219305563052895, 6.009172956465517856, 1.040834085586084257E-14 ) ) ;
#139402 = CARTESIAN_POINT ( 'NONE',  ( -1.580000000000025828, -1.099999999999976108, 2.579999999999999183 ) ) ;
#139403 = CARTESIAN_POINT ( 'NONE',  ( -2.810282979782591006, 6.500690253046801814, 0.000000000000000000 ) ) ;
#139405 = CARTESIAN_POINT ( 'NONE',  ( 1.709613803025863188, -1.856884215550944850, 0.2259493607114013147 ) ) ;
#139404 = CARTESIAN_POINT ( 'NONE',  ( 2.648082478619179003, 0.7070732986501033768, 1.967675578925948354 ) ) ;
#139406 = CARTESIAN_POINT ( 'NONE',  ( 2.056017322730230301, 1.755501262438976751, -0.9912458455646618871 ) ) ;
#139407 = CARTESIAN_POINT ( 'NONE',  ( 8.975134502566660899, 10.53370701015836275, -1.082531754730543083 ) ) ;
#139408 = ORIENTED_EDGE ( 'NONE', *, *, #41681, .F. ) ;
#139409 = CARTESIAN_POINT ( 'NONE',  ( -1.001543065824772872E-14, 4.634375000341418804, 1.575800808251672791 ) ) ;
#139410 = CARTESIAN_POINT ( 'NONE',  ( 2.594910355399903334, -0.5442454861351472273, 1.653239653166445278 ) ) ;
#139411 = CIRCLE ( 'NONE', #4530, 3.971937515251341644 ) ;
#139412 = CARTESIAN_POINT ( 'NONE',  ( 6.173040012923759257, 6.096301524699504704, -0.7998128361456281477 ) ) ;
#139414 = CARTESIAN_POINT ( 'NONE',  ( 0.1083990404229777937, 3.398882113126670657, -2.078799743937121303 ) ) ;
#139413 = FACE_OUTER_BOUND ( 'NONE', #35945, .T. ) ;
#139415 = CARTESIAN_POINT ( 'NONE',  ( 3.351896425306086336, 1.725068445106912707, -0.001234800371389954687 ) ) ;
#139416 = CARTESIAN_POINT ( 'NONE',  ( 2.489988787850425656, -2.185901284972164405, -0.1580625509675498419 ) ) ;
#139417 = CARTESIAN_POINT ( 'NONE',  ( 5.760442859251142522, 0.8911043219209063837, 2.019162844794204048 ) ) ;
#139418 = CARTESIAN_POINT ( 'NONE',  ( -10.30104275384242740, 4.689840931292195592, -5.506867539468097483 ) ) ;
#139419 = CARTESIAN_POINT ( 'NONE',  ( 2.131898410887596906, 2.078612851201648404, -0.6269345663092191767 ) ) ;
#139420 = CARTESIAN_POINT ( 'NONE',  ( 1.488595654847742145, -0.2661386877833261111, -1.806066791206423439 ) ) ;
#139421 = SURFACE_STYLE_FILL_AREA ( #94678 ) ;
#139422 = CARTESIAN_POINT ( 'NONE',  ( 4.012992375354424546, 0.1078809898697324771, 2.114737393012538824 ) ) ;
#139423 = CARTESIAN_POINT ( 'NONE',  ( 0.000000000000000000, 0.000000000000000000, 7.049999999999999822 ) ) ;
#139424 = ORIENTED_EDGE ( 'NONE', *, *, #48451, .T. ) ;
#139426 = CARTESIAN_POINT ( 'NONE',  ( -1.364683531250014514, 0.8010416670080889867, -0.7879004041258289570 ) ) ;
#139425 = CARTESIAN_POINT ( 'NONE',  ( 4.687240393977892161, 1.697883010200517129, 1.540384229137826466 ) ) ;
#139427 = CARTESIAN_POINT ( 'NONE',  ( 1.224999999999943023, 2.645833333333332593, -0.7072540797573158011 ) ) ;
#139428 = CARTESIAN_POINT ( 'NONE',  ( 10.37606763316019531, 10.99983374830873650, 0.7998128361456462443 ) ) ;
#139429 = CARTESIAN_POINT ( 'NONE',  ( 0.3465379015402513252, 1.086389676674501148, -1.820904993421072371 ) ) ;
#139430 = CARTESIAN_POINT ( 'NONE',  ( -5.829642864196175722, 7.824335979694092558, 1.443375672974064550 ) ) ;
#139431 = CARTESIAN_POINT ( 'NONE',  ( 4.744990575102895569, 5.598539094783909320, -1.082531754730548412 ) ) ;
#139432 = CARTESIAN_POINT ( 'NONE',  ( -6.114364089638801403, 8.156510742710487705, 1.443375672974078761 ) ) ;
#139433 = AXIS2_PLACEMENT_3D ( 'NONE', #193197, #129364, #145567 ) ;
#139434 = CARTESIAN_POINT ( 'NONE',  ( 0.001932293024931841172, -9.922538603026485049, 10.91970414279959378 ) ) ;
#139435 = ORIENTED_EDGE ( 'NONE', *, *, #104201, .T. ) ;
#139436 = CARTESIAN_POINT ( 'NONE',  ( 5.608046130584797950, -0.04667949407829303371, 2.016033753796213635 ) ) ;
#139438 = CARTESIAN_POINT ( 'NONE',  ( 2.922777048086916629, -1.425580663919909563, 1.490811266603887963 ) ) ;
#139437 = CARTESIAN_POINT ( 'NONE',  ( 3.988069740714122791, 7.804498464141805592, 0.7998128361456321445 ) ) ;
#139440 = CARTESIAN_POINT ( 'NONE',  ( 6.883263157960369583, 7.629137130509070275, 2.546189081643289942 ) ) ;
#139439 = CARTESIAN_POINT ( 'NONE',  ( 1.841222038795635206E-16, 1.899999999999999023, 2.750000000000000000 ) ) ;
#139441 = CARTESIAN_POINT ( 'NONE',  ( 4.380693030546916944, 6.204170850428461392, 1.443375672974058777 ) ) ;
#139442 = CARTESIAN_POINT ( 'NONE',  ( -3.285556943750000070, -2.559374999522041172, 0.000000000000000000 ) ) ;
#139443 = CARTESIAN_POINT ( 'NONE',  ( 6.972266317189433020E-16, 0.5000000006828014820, -1.225000000000012745 ) ) ;
#139444 = CARTESIAN_POINT ( 'NONE',  ( 5.718738293430368991, -0.05686238728638653983, 2.190873718245327506 ) ) ;
#139445 = CARTESIAN_POINT ( 'NONE',  ( 3.586564705785996843, -0.5826563296015655480, 1.930417576838711957 ) ) ;
#139446 = CARTESIAN_POINT ( 'NONE',  ( 3.403688466941825475, -0.7492148395099357261, -1.682118234477212537 ) ) ;
#139447 = CARTESIAN_POINT ( 'NONE',  ( 4.971035877704902184, 8.951292290631053916, 1.040834085586084257E-14 ) ) ;
#139448 =( NAMED_UNIT ( * ) SI_UNIT ( $, .STERADIAN. ) SOLID_ANGLE_UNIT ( ) );
#139449 = CARTESIAN_POINT ( 'NONE',  ( 6.036143291503483610, 0.8974207610169572247, -1.589712159477923992 ) ) ;
#139450 = AXIS2_PLACEMENT_3D ( 'NONE', #49228, #132630, #16688 ) ;
#139451 = CARTESIAN_POINT ( 'NONE',  ( 0.1242335807666505171, 0.4018034787525020524, 2.263199520926823638 ) ) ;
#139452 = CARTESIAN_POINT ( 'NONE',  ( -7.576308911938196999, 7.733448573549685179, 0.7998128361456462443 ) ) ;
#139453 = CARTESIAN_POINT ( 'NONE',  ( 0.1755611466353265426, -0.002217706044388422469, -2.244164702216360219 ) ) ;
#139454 = CARTESIAN_POINT ( 'NONE',  ( 2.403073576612833939, 1.690916729301103594, -1.255302274246564043 ) ) ;
#139455 = CARTESIAN_POINT ( 'NONE',  ( -4.274563570058511175, 8.209017608368725405, 0.000000000000000000 ) ) ;
#139456 = CARTESIAN_POINT ( 'NONE',  ( 6.913768267964901071, 10.15348118167935709, -1.199719254218441611 ) ) ;
#139457 = CARTESIAN_POINT ( 'NONE',  ( 7.634649897826745857, 8.079715433652276957, 0.7216878364870267237 ) ) ;
#139458 = SURFACE_STYLE_FILL_AREA ( #141617 ) ;
#139460 = EDGE_CURVE ( 'NONE', #209493, #178739, #138630, .T. ) ;
#139459 = CARTESIAN_POINT ( 'NONE',  ( -5.038826645773246682, 9.030381520044109322, 0.7998128361456481317 ) ) ;
#139461 = CARTESIAN_POINT ( 'NONE',  ( 5.951666246274792016, 8.927065806420504401, 1.082531754730558626 ) ) ;
#139462 = CARTESIAN_POINT ( 'NONE',  ( 5.291954866116698852, 6.573566887673666592, 1.361072633976003310 ) ) ;
#139463 = AXIS2_PLACEMENT_3D ( 'NONE', #4623, #6770, #58747 ) ;
#139464 = CARTESIAN_POINT ( 'NONE',  ( -4.629219384062206011, 7.488174150459498968, -1.199719254218452047 ) ) ;
#139466 = CARTESIAN_POINT ( 'NONE',  ( 4.307018013452124983, -0.4884699388765164074, -2.166881332863872522 ) ) ;
#139465 = CARTESIAN_POINT ( 'NONE',  ( 2.144932638433934002, 2.058100890041581810, 0.5106320605416380110 ) ) ;
#139467 = CARTESIAN_POINT ( 'NONE',  ( 2.730644157659181559, 0.2691629481662433099, 2.174792594416566249 ) ) ;
#139468 = CARTESIAN_POINT ( 'NONE',  ( -6.735703387890906946, 6.752742128827836865, -0.7998128361456291469 ) ) ;
#139469 = CARTESIAN_POINT ( 'NONE',  ( 0.3115100037339203487, 1.922317768103290803, 1.083863418116323807 ) ) ;
#139470 = CARTESIAN_POINT ( 'NONE',  ( -4.878955176071358757, 6.785476686873604280, -1.599625672291271394 ) ) ;
#139471 = CARTESIAN_POINT ( 'NONE',  ( 4.967221142815226642, 1.706001049663580460, 0.9686458024478412643 ) ) ;
#139472 = CARTESIAN_POINT ( 'NONE',  ( 8.703444544968814256, 12.24143683818393313, -1.199719254218446718 ) ) ;
#139473 = CARTESIAN_POINT ( 'NONE',  ( 2.324088772396477673E-16, 0.6875000000000069944, -1.225000000000008749 ) ) ;
#139474 = CARTESIAN_POINT ( 'NONE',  ( -0.6823417656250003738, 1.717708333674752730, -1.181850606188749264 ) ) ;
#139475 = CARTESIAN_POINT ( 'NONE',  ( -3.336715202739028552, 6.906935146588564223, 0.7216878364870338292 ) ) ;
#139477 = VERTEX_POINT ( 'NONE', #164978 ) ;
#139476 = CARTESIAN_POINT ( 'NONE',  ( -6.426201623197489887, 6.599582769926260362, 0.7216878364870317197 ) ) ;
#139478 = CARTESIAN_POINT ( 'NONE',  ( 3.199588043238619228, 1.915454767000431602, -0.9102714984489732597 ) ) ;
#139479 = CARTESIAN_POINT ( 'NONE',  ( -4.472210567661380587, 6.310941310395290493, 1.599625672291270506 ) ) ;
#139480 = CARTESIAN_POINT ( 'NONE',  ( 5.647404790089923132, -1.701416311724871067, -1.333359258283283166 ) ) ;
#139481 = CARTESIAN_POINT ( 'NONE',  ( 5.632522751473472589, 8.658694745772667289, -1.199719254218440723 ) ) ;
#139482 = CARTESIAN_POINT ( 'NONE',  ( 3.456447201099471123, -1.625387274077850996, -0.8650149607793490292 ) ) ;
#139483 = UNCERTAINTY_MEASURE_WITH_UNIT (LENGTH_MEASURE( 1.000000000000000082E-05 ), #111266, 'distance_accuracy_value', 'NONE');
#139484 = CARTESIAN_POINT ( 'NONE',  ( -5.899175937014327076, 6.007822909898694164, -0.1935691424272238670 ) ) ;
#139485 = CARTESIAN_POINT ( 'NONE',  ( 1.364683531249988757, 1.446875000341421469, 0.000000000000000000 ) ) ;
#139486 = CARTESIAN_POINT ( 'NONE',  ( 6.667905886031927132, -1.063982290101581185, 1.377602455597818132 ) ) ;
#139487 = CARTESIAN_POINT ( 'NONE',  ( 6.727182134110193168, 4.701113012587437190, 2.373661997258198486 ) ) ;
#139488 = CARTESIAN_POINT ( 'NONE',  ( 3.497640442645619796, 6.064035702186436616, -1.082531754730543083 ) ) ;
#139489 = FILL_AREA_STYLE ('',( #92876 ) ) ;
#139490 = CARTESIAN_POINT ( 'NONE',  ( 4.276362541559985075, -1.246951984143488623, 1.765614359104182629 ) ) ;
#139491 = CARTESIAN_POINT ( 'NONE',  ( -5.786632634934295361, 5.645492917045106473, 0.7998128361456341429 ) ) ;
#139492 = CARTESIAN_POINT ( 'NONE',  ( 6.749375321999433908, -1.976647572034227140, -0.3960365597561604778 ) ) ;
#139493 = CARTESIAN_POINT ( 'NONE',  ( -8.473482818416675499, 9.948446711983361723, -1.082531754730543083 ) ) ;
#139494 = CARTESIAN_POINT ( 'NONE',  ( 3.977527890101069996, 2.036293384626610248, -0.7259696361804208742 ) ) ;
#139495 = CARTESIAN_POINT ( 'NONE',  ( 5.044191579798307679, 1.965876612296811654, 0.1480472272742116568 ) ) ;
#139496 = CARTESIAN_POINT ( 'NONE',  ( 4.270605845326081784, -1.729236537505800086, 0.1267691526786636214 ) ) ;
#139497 = CARTESIAN_POINT ( 'NONE',  ( 1.154151856878969928, 0.8927059368322427524, 2.001694687108931170 ) ) ;
#139498 = CARTESIAN_POINT ( 'NONE',  ( 0.7632353006940760798, -1.668858575275869116, 1.593938313602519363 ) ) ;
#139499 = CARTESIAN_POINT ( 'NONE',  ( 3.620434630758031069, 1.310268768930487937, -1.590567769477232662 ) ) ;
#139500 = CARTESIAN_POINT ( 'NONE',  ( 5.565949569975685129, -1.228723311412585950, 1.503964349303931192 ) ) ;
#139501 = CARTESIAN_POINT ( 'NONE',  ( -8.365017589507372620, 9.821903944922480534, 1.082531754730558626 ) ) ;
#139502 = CARTESIAN_POINT ( 'NONE',  ( -5.492988512192097161, 6.437516681426083132, 1.199719254218452935 ) ) ;
#139503 = FILL_AREA_STYLE ('',( #71252 ) ) ;
#139505 = ORIENTED_EDGE ( 'NONE', *, *, #39637, .T. ) ;
#139504 = CARTESIAN_POINT ( 'NONE',  ( -3.546339698426324460, 6.295090860542775779, -1.199719254218450271 ) ) ;
#139506 = CARTESIAN_POINT ( 'NONE',  ( -6.168596704093453731, 10.14052055484361325, 0.7216878364870458196 ) ) ;
#139507 = CARTESIAN_POINT ( 'NONE',  ( 2.151677955860908487, -1.772288797910109404, -1.314638326115322053 ) ) ;
#139508 = CARTESIAN_POINT ( 'NONE',  ( -3.285556943750000514, -4.076041666188709556, -1.896917185911906500 ) ) ;
#139509 = VERTEX_POINT ( 'NONE', #1382 ) ;
#139510 = CARTESIAN_POINT ( 'NONE',  ( 0.5318007479364270651, 1.064995724915913433, 1.525891442952797439 ) ) ;
#139511 = CARTESIAN_POINT ( 'NONE',  ( -0.02880301295722554472, 4.079423595021631321, -2.828475351696632778 ) ) ;
#139512 = CARTESIAN_POINT ( 'NONE',  ( -0.7499999999999972244, 5.139583334016151639, -1.299038105676652899 ) ) ;
#139513 = CARTESIAN_POINT ( 'NONE',  ( 4.774589472192324102, 6.991777125168484375, -1.402305405395011251 ) ) ;
#139515 = CARTESIAN_POINT ( 'NONE',  ( -1.436716030283634371, 7.421837552815579109, -4.237608343040895953 ) ) ;
#139514 = CARTESIAN_POINT ( 'NONE',  ( -6.581660514134937578, 6.779899958900003298, -0.3344319070191399401 ) ) ;
#139516 = CARTESIAN_POINT ( 'NONE',  ( 6.210883717528068892, -0.2205035313364057392, 1.827825250963102333 ) ) ;
#139517 = ORIENTED_EDGE ( 'NONE', *, *, #59579, .F. ) ;
#139518 = CARTESIAN_POINT ( 'NONE',  ( 2.325137485922982084, -0.001238304602014379070, 2.061077815622249343 ) ) ;
#139519 = CARTESIAN_POINT ( 'NONE',  ( 1.360316468749980023, 0.01562500034139879812, -2.255140518769849223E-14 ) ) ;
#139520 = CARTESIAN_POINT ( 'NONE',  ( -5.669280788808708671, 9.765911353585494226, 0.7998128361456481317 ) ) ;
#139521 = CARTESIAN_POINT ( 'NONE',  ( -0.4000000000000218936, 2.999999999999988898, 0.3999999999999819811 ) ) ;
#139522 = CARTESIAN_POINT ( 'NONE',  ( 11.86145017354087372, 11.00485634456124018, 1.099999999999996980 ) ) ;
#139523 = CARTESIAN_POINT ( 'NONE',  ( 5.183294799126148433, 4.941598775268944976, 1.040834085586084257E-14 ) ) ;
#139524 = CARTESIAN_POINT ( 'NONE',  ( 0.9716393833266089297, 1.986344416073432484, -0.5490401152750885583 ) ) ;
#139526 = CARTESIAN_POINT ( 'NONE',  ( 5.144037045698616417, 0.5398437887287730330, 1.760322748975438500 ) ) ;
#139525 = CARTESIAN_POINT ( 'NONE',  ( -0.7500000000000006661, 12.45833333333333570, -1.299038105676657340 ) ) ;
#139527 = CARTESIAN_POINT ( 'NONE',  ( 7.657657833620182153, 7.828355648845348291, -0.7998128361456281477 ) ) ;
#139528 = VECTOR ( 'NONE', #77350, 1000.000000000000000 ) ;
#139529 = CARTESIAN_POINT ( 'NONE',  ( -4.633854640820660009, 8.628190524257904670, -0.7998128361456362523 ) ) ;
#139530 = EDGE_LOOP ( 'NONE', ( #91252, #200304, #98571, #15050, #17445 ) ) ;
#139531 = AXIS2_PLACEMENT_3D ( 'NONE', #139895, #3443, #69510 ) ;
#139532 = CARTESIAN_POINT ( 'NONE',  ( 4.389439674793148782, 1.972019932058775016, -0.9908447712502415072 ) ) ;
#139533 = CARTESIAN_POINT ( 'NONE',  ( 0.2632415847364302786, -1.930764589519979424, -0.9721467891136772455 ) ) ;
#139534 = CARTESIAN_POINT ( 'NONE',  ( -6.426201623197489887, 6.599582769926260362, 0.7216878364870317197 ) ) ;
#139535 = CARTESIAN_POINT ( 'NONE',  ( -0.01753026575586694516, -1.247696154478775021, 1.449428981083925150 ) ) ;
#139536 = CARTESIAN_POINT ( 'NONE',  ( 0.6203277878081385754, 1.987498645412737908, 0.3399528957561820386 ) ) ;
#139537 = CARTESIAN_POINT ( 'NONE',  ( 5.682275777458829502, 9.643422483761748154, 0.7216878364870317197 ) ) ;
#139538 = DIRECTION ( 'NONE',  ( -0.000000000000000000, -1.000000000000000000, -0.000000000000000000 ) ) ;
#139539 = CARTESIAN_POINT ( 'NONE',  ( -0.1263102688159843945, 6.363441598446243574, 3.117922131261606999 ) ) ;
#139540 = DIRECTION ( 'NONE',  ( 0.000000000000000000, 8.546850786086437571E-32, 1.000000000000000000 ) ) ;
#139542 = STYLED_ITEM ( 'NONE', ( #14789 ), #1742 ) ;
#139541 = CARTESIAN_POINT ( 'NONE',  ( 0.4966798268824790252, 1.557709316500059726, -1.035497600327957235 ) ) ;
#139543 = CARTESIAN_POINT ( 'NONE',  ( 1.991423064788412800, -0.4370762659771566527, 1.968445590580846893 ) ) ;
#139545 = DIRECTION ( 'NONE',  ( 0.000000000000000000, 1.000000000000000000, -8.546850786086437571E-32 ) ) ;
#139544 = CARTESIAN_POINT ( 'NONE',  ( -0.6823417656250246877, 0.3010416670080895418, 1.181850606188755259 ) ) ;
#139547 = CARTESIAN_POINT ( 'NONE',  ( 4.108114811375044084, -2.100464006233178083, 0.1544923775467464122 ) ) ;
#139546 = CARTESIAN_POINT ( 'NONE',  ( -9.013473194986783454, 9.410140237106395134, -0.7998128361456291469 ) ) ;
#139548 = CARTESIAN_POINT ( 'NONE',  ( 8.555358625423188812, 9.940005470203933768, 1.199719254218462483 ) ) ;
#139550 = CARTESIAN_POINT ( 'NONE',  ( -8.864333505236459132, 9.236143932397675727, 1.040834085586084257E-14 ) ) ;
#139549 = CARTESIAN_POINT ( 'NONE',  ( 4.573896719763862251, 6.429575154514868274, -1.599625672291273171 ) ) ;
#139551 = CARTESIAN_POINT ( 'NONE',  ( 5.510910596163088569E-16, 2.499999999999998668, 4.500000000000000000 ) ) ;
#139552 = CARTESIAN_POINT ( 'NONE',  ( 4.588152005245718534, 1.166368207181975869, 1.648760302449885584 ) ) ;
#139553 = CARTESIAN_POINT ( 'NONE',  ( -0.6823417656250212460, 5.051041667008086655, 1.181850606188767472 ) ) ;
#139554 = CARTESIAN_POINT ( 'NONE',  ( 6.180145878880094479, -1.142753862412404509, -1.717008129757614077 ) ) ;
#139555 = CARTESIAN_POINT ( 'NONE',  ( 7.917598520700710019, 12.18102267421877727, -0.7216878364870328300 ) ) ;
#139556 = CARTESIAN_POINT ( 'NONE',  ( 4.956408742875526130, 0.8222144862577386304, 1.999314050312686053 ) ) ;
#139557 = CARTESIAN_POINT ( 'NONE',  ( 7.686546744304875389, 7.932335721302671949, 0.7998128361456291469 ) ) ;
#139558 = CARTESIAN_POINT ( 'NONE',  ( 0.6823417656249882723, -0.3447916663252489911, 1.181850606188755259 ) ) ;
#139560 = CARTESIAN_POINT ( 'NONE',  ( -9.499606442108964544, -9.746166700193986898, 0.08647222121513808979 ) ) ;
#139559 = CARTESIAN_POINT ( 'NONE',  ( 6.180537922983273091, 8.303989891604203422, -1.599625672291281386 ) ) ;
#139561 = CARTESIAN_POINT ( 'NONE',  ( 7.497295758232718654, 9.769931022736756177, -1.443375672974058777 ) ) ;
#139563 = CARTESIAN_POINT ( 'NONE',  ( -0.3656762941044116033, -7.723177556212100114, 10.97096416026169052 ) ) ;
#139562 = CARTESIAN_POINT ( 'NONE',  ( 2.084662720398474001, 1.251192046665784208, -1.774223565721672724 ) ) ;
#139565 = CARTESIAN_POINT ( 'NONE',  ( 2.120424178990498731, 0.001545453418709194504, 1.841430844159386293 ) ) ;
#139564 = CARTESIAN_POINT ( 'NONE',  ( -5.422898255786198440, 7.349800603215774331, -1.443375672974052559 ) ) ;
#139566 = CARTESIAN_POINT ( 'NONE',  ( 0.6823417656249882723, 2.176041667008084435, -1.181850606188749264 ) ) ;
#139567 = CARTESIAN_POINT ( 'NONE',  ( 3.790727848299980440, 1.850687065220711469, -1.173560875862532660 ) ) ;
#139568 = CARTESIAN_POINT ( 'NONE',  ( 6.983263157960404754, 0.5601148359399975574, 2.204851038219941106 ) ) ;
#139569 = CARTESIAN_POINT ( 'NONE',  ( 3.854571047428239527, 0.8115417623771915556, 2.112135835510853710 ) ) ;
#139570 = CARTESIAN_POINT ( 'NONE',  ( -6.669721502918952716, 9.868759955792373972, 1.199719254218452047 ) ) ;
#139571 = CARTESIAN_POINT ( 'NONE',  ( -1.364683531250012516, 4.551041667008082214, -0.7879004041258300672 ) ) ;
#139572 = CARTESIAN_POINT ( 'NONE',  ( 6.151318917739748038, 6.974181327834800825, -0.9227930848511676221 ) ) ;
#139573 = CARTESIAN_POINT ( 'NONE',  ( -1.402160292154681736E-14, 14.06250000000000355, 1.732050807568881190 ) ) ;
#139574 = CARTESIAN_POINT ( 'NONE',  ( 4.882344714696929877, 8.710169577206153591, -0.7216878364870458196 ) ) ;
#139575 = CARTESIAN_POINT ( 'NONE',  ( 5.448444396454582339, 0.5145788473605721336, 1.693291817928108234 ) ) ;
#139576 = CARTESIAN_POINT ( 'NONE',  ( 3.334638158648925099, 1.275257586908218110, -1.557663628481553264 ) ) ;
#139577 = CARTESIAN_POINT ( 'NONE',  ( 9.108380270282433244, 9.520865158284665952, 1.040834085586084257E-14 ) ) ;
#139578 = CARTESIAN_POINT ( 'NONE',  ( 1.764816150188710298, -1.489710805432680418, 1.488830988054674620 ) ) ;
#139580 = CARTESIAN_POINT ( 'NONE',  ( 1.499999999999987121, 1.545833333333354487, -0.8660254037844253849 ) ) ;
#139579 = CARTESIAN_POINT ( 'NONE',  ( -0.6823417656250039265, 10.56770833367473550, -1.181850606188755259 ) ) ;
#139581 = CARTESIAN_POINT ( 'NONE',  ( 0.5726248362980547180, 1.360856580973464069, -1.424029402571887148 ) ) ;
#139582 = CARTESIAN_POINT ( 'NONE',  ( -4.065465959251405081, 5.836405933916976707, -1.599625672291271394 ) ) ;
#139583 = CARTESIAN_POINT ( 'NONE',  ( 3.588273936444265289, 7.344317902764286643, -0.3372145678562175064 ) ) ;
#139585 = ORIENTED_EDGE ( 'NONE', *, *, #191715, .T. ) ;
#139584 = CARTESIAN_POINT ( 'NONE',  ( 5.326340473083292615, -0.8217345736999382977, -1.614601580891014354 ) ) ;
#139586 = CARTESIAN_POINT ( 'NONE',  ( 7.782016984564060103, 9.141736572488651902, 1.082531754730558626 ) ) ;
#139587 = EDGE_CURVE ( 'NONE', #137371, #201176, #198073, .T. ) ;
#139588 = CARTESIAN_POINT ( 'NONE',  ( 5.225416543158964977, -1.776039340814106637, 0.5876355328483380269 ) ) ;
#139589 = VECTOR ( 'NONE', #98783, 1000.000000000000000 ) ;
#139590 = VERTEX_POINT ( 'NONE', #67443 ) ;
#139591 = CARTESIAN_POINT ( 'NONE',  ( 4.135645376760338721, 1.951069878921590561, -0.6927527371542246959 ) ) ;
#139592 = VECTOR ( 'NONE', #107501, 1000.000000000000000 ) ;
#139593 = CARTESIAN_POINT ( 'NONE',  ( -1.225000000000038058, 2.270833333333394766, 0.7072540797572857141 ) ) ;
#139594 = CARTESIAN_POINT ( 'NONE',  ( -6.265276382846530545, 6.482112999508623297, 0.000000000000000000 ) ) ;
#139595 = FACE_OUTER_BOUND ( 'NONE', #92365, .T. ) ;
#139596 = CARTESIAN_POINT ( 'NONE',  ( 9.426996880203592610, 9.892584536526015881, -0.7998128361456281477 ) ) ;
#139597 = CARTESIAN_POINT ( 'NONE',  ( -8.130085669689073313, 12.63685038127928806, 0.7998128361456481317 ) ) ;
#139598 = CARTESIAN_POINT ( 'NONE',  ( 6.373214726875630731, 9.593111727067046957, 1.199719254218452047 ) ) ;
#139599 = CIRCLE ( 'NONE', #156907, 6.200000000000000178 ) ;
#139600 = DIRECTION ( 'NONE',  ( -5.578564026256491869E-16, -1.000000000000000000, -9.066213480720160632E-32 ) ) ;
#139601 = CARTESIAN_POINT ( 'NONE',  ( -1.364683531250012516, 0.5302083336747518416, 0.7879004041258379498 ) ) ;
#139602 = CARTESIAN_POINT ( 'NONE',  ( 1.499999999999987121, 1.754166666666691521, 0.8660254037844524744 ) ) ;
#139604 = CARTESIAN_POINT ( 'NONE',  ( 6.484877546038077867, 6.460111979999551224, 1.040834085586084257E-14 ) ) ;
#139603 = CARTESIAN_POINT ( 'NONE',  ( 4.158614545834369736, -0.6132839004606009947, -1.863630207987923004 ) ) ;
#139605 = CARTESIAN_POINT ( 'NONE',  ( 2.319685276966905629, -1.560262528187049025, 1.276846253076675541 ) ) ;
#139606 = DIRECTION ( 'NONE',  ( -0.6029061840396265914, -0.7978120914393163066, 0.000000000000000000 ) ) ;
#139607 = CIRCLE ( 'NONE', #205271, 0.08000000000000004330 ) ;
#139608 = DIRECTION ( 'NONE',  ( -8.638326563840814399E-31, 0.000000000000000000, -1.000000000000000000 ) ) ;
#139609 = CARTESIAN_POINT ( 'NONE',  ( -11.78331023100045627, 9.799999999999982947, 1.799999999999999600 ) ) ;
#139610 = CARTESIAN_POINT ( 'NONE',  ( 2.512791842090915218, 1.668957736969980621, 0.8448945032545759348 ) ) ;
#139611 = CARTESIAN_POINT ( 'NONE',  ( 1.364683531249990311, 4.863541667008084879, 0.7879004041258500513 ) ) ;
#139612 = CARTESIAN_POINT ( 'NONE',  ( 4.236591777569945982, 1.235091891264840314, -1.589779643154372701 ) ) ;
#139613 = CARTESIAN_POINT ( 'NONE',  ( -9.508345801885592863, 9.987491611821676329, 0.7998128361456462443 ) ) ;
#139615 = CARTESIAN_POINT ( 'NONE',  ( 3.058335788041772307, -1.258934183635691095, 1.702155058717010672 ) ) ;
#139614 = CARTESIAN_POINT ( 'NONE',  ( -6.236387472606166327, 6.378132927569716060, -0.7216878364870278340 ) ) ;
#139616 = CARTESIAN_POINT ( 'NONE',  ( 4.826661161267837841, -1.354893614093263254, 1.565527137264411728 ) ) ;
#139617 = CARTESIAN_POINT ( 'NONE',  ( 5.342795052237045539, 8.390955439988655229, -1.199719254218450271 ) ) ;
#139619 = CARTESIAN_POINT ( 'NONE',  ( 6.620655732516651071, 1.241313378043694238, 2.288056600130850882 ) ) ;
#139618 = CARTESIAN_POINT ( 'NONE',  ( 0.9430502156211654219, -1.650385480578796749, -1.283440319295367615 ) ) ;
#139621 = ORIENTED_EDGE ( 'NONE', *, *, #85474, .T. ) ;
#139620 = CARTESIAN_POINT ( 'NONE',  ( 0.1820471141361617307, -1.670984272841398832, -0.4269972090983116253 ) ) ;
#139622 = CARTESIAN_POINT ( 'NONE',  ( 6.642605195691581699, 9.837124264027149678, 1.199719254218462483 ) ) ;
#139623 = CARTESIAN_POINT ( 'NONE',  ( 8.103009739378183696, -6.700000000000002842, -7.439168848973796599 ) ) ;
#139624 = FACE_OUTER_BOUND ( 'NONE', #22374, .T. ) ;
#139625 = CARTESIAN_POINT ( 'NONE',  ( -11.05071387823260487, 4.509444648491869323, 6.218574854545789066 ) ) ;
#139626 = CARTESIAN_POINT ( 'NONE',  ( 7.415946836550714849, 9.675023947441092176, 1.443375672974076540 ) ) ;
#139627 = CARTESIAN_POINT ( 'NONE',  ( 1.364683531249996529, 12.02604166700806587, 0.7879004041258403923 ) ) ;
#139628 = CARTESIAN_POINT ( 'NONE',  ( 5.988906256519173077, -1.817303134770717588, -0.5954205699960082310 ) ) ;
#139629 = CARTESIAN_POINT ( 'NONE',  ( -9.494787648271923786, 9.971673765939062406, 1.040834085586084257E-14 ) ) ;
#139630 = CARTESIAN_POINT ( 'NONE',  ( 5.198661835836162481, 8.152523677529138979, 1.199719254218462483 ) ) ;
#139631 = CARTESIAN_POINT ( 'NONE',  ( -11.92050416151432835, 11.15205375279624178, -1.381922468431411088 ) ) ;
#139632 = EDGE_CURVE ( 'NONE', #12663, #10241, #95436, .T. ) ;
#139633 = FACE_OUTER_BOUND ( 'NONE', #89481, .T. ) ;
#139634 = CARTESIAN_POINT ( 'NONE',  ( 2.361091307074211887, 5.906356958228550447, 0.7998128361456462443 ) ) ;
#139635 = ORIENTED_EDGE ( 'NONE', *, *, #64317, .F. ) ;
#139636 = CARTESIAN_POINT ( 'NONE',  ( -5.641074431737709283, 8.738948049406083385, -1.199719254218452047 ) ) ;
#139637 = CARTESIAN_POINT ( 'NONE',  ( 5.870720304489429608, -0.2986452421533461465, -1.994069804803912049 ) ) ;
#139638 = LINE ( 'NONE', #175326, #97473 ) ;
#139639 = CARTESIAN_POINT ( 'NONE',  ( 1.347111479062088405E-15, 2.999999999999999112, 11.00000000000000000 ) ) ;
#139640 = CARTESIAN_POINT ( 'NONE',  ( -0.1399997263889820043, 5.722209607272843002, -2.594334538518060729 ) ) ;
#139641 =( BOUNDED_CURVE ( )  B_SPLINE_CURVE ( 2, ( #152701, #186251, #37886, #103964, #41108, #123501, #206770 ),
 .UNSPECIFIED., .F., .T. ) 
 B_SPLINE_CURVE_WITH_KNOTS ( ( 3, 2, 2, 3 ),
 ( 0.4499999999999996780, 0.4583333333333332038, 0.4666666666666668406, 0.4750000000000003664 ),
 .UNSPECIFIED. ) 
 CURVE ( )  GEOMETRIC_REPRESENTATION_ITEM ( )  RATIONAL_B_SPLINE_CURVE ( ( 1.000000000000005329, 0.8660254037844333785, 1.000000000000000000, 0.8660254037844387076, 1.000000000000000000, 0.8660254037844324904, 1.000000000000006217 ) ) 
 REPRESENTATION_ITEM ( '' )  );
#139642 = CARTESIAN_POINT ( 'NONE',  ( -4.717874267875590277, 7.487641831621378863, 1.082531754730560403 ) ) ;
#139643 = CARTESIAN_POINT ( 'NONE',  ( 3.440018289565364817, 5.036440642624797626, 1.599625672291267398 ) ) ;
#139644 = CARTESIAN_POINT ( 'NONE',  ( 2.131642331222316500, 1.886095724437972798, -0.5669754052412961931 ) ) ;
#139645 = EDGE_CURVE ( 'NONE', #111396, #84144, #133453, .T. ) ;
#139646 = CARTESIAN_POINT ( 'NONE',  ( 3.989861366179075386, -2.010826228832915508, 0.1511578083489423796 ) ) ;
#139647 = CARTESIAN_POINT ( 'NONE',  ( -6.344325816190970357, 9.489131654609717970, 1.199719254218452047 ) ) ;
#139648 = CARTESIAN_POINT ( 'NONE',  ( 6.727182134110167411, 4.690976314540481695, 2.651619508270358416 ) ) ;
#139649 = CARTESIAN_POINT ( 'NONE',  ( 4.804715953495782621, 1.905792977913090214, 1.081705336968781239 ) ) ;
#139650 = DIRECTION ( 'NONE',  ( 0.000000000000000000, 1.000000000000000000, 0.000000000000000000 ) ) ;
#139651 = CARTESIAN_POINT ( 'NONE',  ( 3.311465173828963326, -0.3771673786017637475, 1.888946036755128288 ) ) ;
#139652 = CARTESIAN_POINT ( 'NONE',  ( -8.076906825439122528, 10.44614393447756129, -1.599625672291263179 ) ) ;
#139653 = EDGE_CURVE ( 'NONE', #104013, #211691, #201718, .T. ) ;
#139654 = CARTESIAN_POINT ( 'NONE',  ( -0.1296875068448159474, 0.7431874094961619104, -1.910093690679348200 ) ) ;
#139655 = CARTESIAN_POINT ( 'NONE',  ( -0.01666059994226073634, -0.1612322585618740090, -2.171656592459797253 ) ) ;
#139656 = CARTESIAN_POINT ( 'NONE',  ( -1.792254920982459199, 15.51967661332317050, -11.87386578584006358 ) ) ;
#139657 = CARTESIAN_POINT ( 'NONE',  ( -3.110356790690614215, 14.48006632018288542, 11.59859428470667453 ) ) ;
#139658 = CARTESIAN_POINT ( 'NONE',  ( 5.823390672269506574, 6.752709524857930745, -1.199719254218446718 ) ) ;
#139659 = CARTESIAN_POINT ( 'NONE',  ( -3.697672731464866747, 7.367968498737385019, -2.499999999999995115 ) ) ;
#139660 = CARTESIAN_POINT ( 'NONE',  ( 3.282482588284323821, 6.843663763058119187, 0.7216878364870257245 ) ) ;
#139662 = CARTESIAN_POINT ( 'NONE',  ( 3.264317399697822530, 2.013265973121576291, -0.002229150246490021157 ) ) ;
#139661 = CARTESIAN_POINT ( 'NONE',  ( 6.497600353373155002, -1.840680978339729545, 0.05264081064878384231 ) ) ;
#139663 = CARTESIAN_POINT ( 'NONE',  ( 5.413504136812340661, 0.6594720349357428013, 2.201770641885878899 ) ) ;
#139665 = CARTESIAN_POINT ( 'NONE',  ( 3.572968443166994579, 1.680613686130405515, 0.7995154651666557255 ) ) ;
#139664 = SURFACE_SIDE_STYLE ('',( #202473 ) ) ;
#139666 = CARTESIAN_POINT ( 'NONE',  ( 8.011942431032855083, 8.311964022485323511, 0.7998128361456291469 ) ) ;
#139667 = DIRECTION ( 'NONE',  ( -0.9999980456341538426, 0.000000000000000000, -0.001977050295949953074 ) ) ;
#139668 = CARTESIAN_POINT ( 'NONE',  ( -15.75000000000000000, 13.40000000000000036, 0.6999999999999992895 ) ) ;
#139669 = CARTESIAN_POINT ( 'NONE',  ( -6.018930129462987999, 9.109503353427070849, 1.199719254218452047 ) ) ;
#139670 = CARTESIAN_POINT ( 'NONE',  ( -3.526529353330350336, 7.128384988945109413, -0.7216878364870458196 ) ) ;
#139671 = CARTESIAN_POINT ( 'NONE',  ( 5.952696063536119908, -1.793662432779649540, -1.073965677532197072 ) ) ;
#139672 = CARTESIAN_POINT ( 'NONE',  ( 6.317736394288147039, 6.473040002865377396, 0.7216878364870317197 ) ) ;
#139673 = ORIENTED_EDGE ( 'NONE', *, *, #122982, .F. ) ;
#139675 = CARTESIAN_POINT ( 'NONE',  ( 4.111146893441827821, 5.819424013814004759, 1.599625672291267398 ) ) ;
#139674 = CARTESIAN_POINT ( 'NONE',  ( -11.07790593930098311, 12.30000000000000071, 0.6999999999999992895 ) ) ;
#139676 = CARTESIAN_POINT ( 'NONE',  ( 5.988827324695590981, -0.2600698726980456010, -1.705031240916178525 ) ) ;
#139677 = CARTESIAN_POINT ( 'NONE',  ( -3.764360206088648297, 7.543504007078730922, -0.7998128361456281477 ) ) ;
#139678 = AXIS2_PLACEMENT_3D ( 'NONE', #58848, #92451, #23118 ) ;
#139679 = CARTESIAN_POINT ( 'NONE',  ( 1.881130407182354469, -0.4634198587198985475, -1.670964061236743348 ) ) ;
#139680 =( LENGTH_UNIT ( ) NAMED_UNIT ( * ) SI_UNIT ( .MILLI., .METRE. ) );
#139681 = CARTESIAN_POINT ( 'NONE',  ( 0.7499999999999920064, 5.514583334016151639, 1.299038105676669330 ) ) ;
#139682 = CARTESIAN_POINT ( 'NONE',  ( -5.032047568966410367, 9.022472597102808578, 1.214306433183764966E-14 ) ) ;
#139683 = CARTESIAN_POINT ( 'NONE',  ( -1.201851678989727383E-14, 3.337500000000019007, -1.732050807568863648 ) ) ;
#139685 = AXIS2_PLACEMENT_3D ( 'NONE', #22004, #171492, #172573 ) ;
#139684 = CARTESIAN_POINT ( 'NONE',  ( 0.7079804021624566124, 0.6528548590773940452, -1.964656565413371414 ) ) ;
#139686 = CARTESIAN_POINT ( 'NONE',  ( 5.356004772612798170, 1.823420152956479523, -0.09349780940721279243 ) ) ;
#139687 = CARTESIAN_POINT ( 'NONE',  ( 2.149198318390078910, 1.709348667602617500, -0.9624241554767108964 ) ) ;
#139688 = CARTESIAN_POINT ( 'NONE',  ( -10.66756793585402363, 11.33991743478486391, 0.7998128361456462443 ) ) ;
#139689 = CARTESIAN_POINT ( 'NONE',  ( 6.154511665599609493, 9.267681812253174556, 1.199719254218462483 ) ) ;
#139690 = CARTESIAN_POINT ( 'NONE',  ( 3.405043383231837417, -0.4154483767263848493, -2.079220720149973278 ) ) ;
#139691 = CARTESIAN_POINT ( 'NONE',  ( -11.92619526913699879, 13.39999999999998259, 1.328859060402684644 ) ) ;
#139692 = CARTESIAN_POINT ( 'NONE',  ( -5.639314450680645407, 6.167449467472198243, -0.8320033040390877321 ) ) ;
#139693 = CARTESIAN_POINT ( 'NONE',  ( 1.604436975501881468, 2.067711310959176707, 0.1055696395834623824 ) ) ;
#139695 = CARTESIAN_POINT ( 'NONE',  ( -6.009258394948636914E-15, 15.21875000068279782, -1.732050807568875195 ) ) ;
#139694 = DIRECTION ( 'NONE',  ( 0.000000000000000000, 3.252606517456504467E-14, -1.000000000000000000 ) ) ;
#139697 = EDGE_LOOP ( 'NONE', ( #171394, #60859, #136749, #184137 ) ) ;
#139696 = CARTESIAN_POINT ( 'NONE',  ( 3.264521566599550173, 2.221473416772083098, -0.001674386450213962828 ) ) ;
#139698 = CARTESIAN_POINT ( 'NONE',  ( 1.758794133653733827, 2.198278648980501515, -0.6719540409268388581 ) ) ;
#139700 = CARTESIAN_POINT ( 'NONE',  ( 0.3386216902839487841, -1.901412053528793722, -0.4823507731460881520 ) ) ;
#139699 = CARTESIAN_POINT ( 'NONE',  ( 10.38518247838791986, 11.21839376764850726, 0.7216878364870438212 ) ) ;
#139702 = CARTESIAN_POINT ( 'NONE',  ( -1.642778471874998480, -3.901041666188709289, 2.845375778867863303 ) ) ;
#139701 = CARTESIAN_POINT ( 'NONE',  ( 5.890091390494168522, 5.836471141856793388, 0.000000000000000000 ) ) ;
#139703 = DIRECTION ( 'NONE',  ( -1.000000000000000000, 7.771561172376097755E-16, 4.440892098500627148E-16 ) ) ;
#139704 = CARTESIAN_POINT ( 'NONE',  ( 6.444863656277017405, -1.483217659742748218, -1.090817886357238198 ) ) ;
#139705 = CARTESIAN_POINT ( 'NONE',  ( -1.715332513650474455, -0.7127186716553509660, 0.8729729531562419043 ) ) ;
#139706 = CARTESIAN_POINT ( 'NONE',  ( -0.1104750535120268828, 4.084583917300320444, -2.658209514912849514 ) ) ;
#139707 = CARTESIAN_POINT ( 'NONE',  ( 3.311258828109595154, -0.3375135790737812114, 1.691226829923969666 ) ) ;
#139708 = CARTESIAN_POINT ( 'NONE',  ( 2.132046339962359038, 2.016188815772378629, 0.04465230659478347519 ) ) ;
#139709 = CARTESIAN_POINT ( 'NONE',  ( 2.584987504963653038, -0.7174396784795608051, 2.183947998982360250 ) ) ;
#139710 = CARTESIAN_POINT ( 'NONE',  ( 3.128476345081227628, 1.259638568860393493, -1.879123747193896632 ) ) ;
#139711 = CARTESIAN_POINT ( 'NONE',  ( 5.514326386059018148, -0.9456761151771397866, -1.881892731060728519 ) ) ;
#139712 = CARTESIAN_POINT ( 'NONE',  ( -5.912764389335557702, 8.951956649983198844, 1.082531754730550855 ) ) ;
#139713 = ORIENTED_EDGE ( 'NONE', *, *, #204566, .T. ) ;
#139714 = CARTESIAN_POINT ( 'NONE',  ( 5.114393831954183511, 1.220379059178023695, -1.281870188591783588 ) ) ;
#139716 = CARTESIAN_POINT ( 'NONE',  ( 0.4809653258567511691, -0.2865729554843428062, -2.274222260372929405 ) ) ;
#139715 = CARTESIAN_POINT ( 'NONE',  ( 6.393551957296131683, 9.616838495890963401, 1.199719254218452047 ) ) ;
#139717 = CARTESIAN_POINT ( 'NONE',  ( 5.736236344406846932, 0.3633543575551900773, 1.804753862313414281 ) ) ;
#139719 = ADVANCED_FACE ( 'NONE', ( #21891 ), #136758, .T. ) ;
#139718 = CARTESIAN_POINT ( 'NONE',  ( -4.243865776277440993, 4.909930479533815451, -1.199719254218446718 ) ) ;
#139720 = B_SPLINE_CURVE_WITH_KNOTS ( 'NONE', 3,
 ( #140603, #205542, #105978, #189305, #173077, #124400, #190358, #42020 ),
 .UNSPECIFIED., .F., .F.,
 ( 4, 2, 2, 4 ),
 ( 0.000000000000000000, 0.0004970278158210322947, 0.0007455417237315461109, 0.0009940556316420600357 ),
 .UNSPECIFIED. ) ;
#139721 = CARTESIAN_POINT ( 'NONE',  ( 6.246043798300164873, 0.6838514278588082584, 2.082077653496945402 ) ) ;
#139722 = CARTESIAN_POINT ( 'NONE',  ( -4.620631424159025613, 4.285158171140619032, -0.7998128361456221525 ) ) ;
#139723 = CARTESIAN_POINT ( 'NONE',  ( -5.951577129995881954, 15.44725960769734208, 10.37887709679271175 ) ) ;
#139724 = CARTESIAN_POINT ( 'NONE',  ( 5.951642636407409093, 1.565221049572671719, 1.355249363302114318 ) ) ;
#139725 = CARTESIAN_POINT ( 'NONE',  ( -0.1179535434602772825, -2.016182236903838465, -0.04464881524945257807 ) ) ;
#139726 =( BOUNDED_SURFACE ( )  B_SPLINE_SURFACE ( 3, 2, ( 
 ( #155288, #57784, #26339 ),
 ( #172615, #109810, #11148 ),
 ( #189913, #91377, #41558 ),
 ( #89237, #175819, #205078 ),
 ( #25275, #42628, #59912 ),
 ( #23120, #24191, #6870 ) ),
 .UNSPECIFIED., .F., .F., .T. ) 
 B_SPLINE_SURFACE_WITH_KNOTS ( ( 4, 2, 4 ),
 ( 3, 3 ),
 ( 0.000000000000000000, 0.0003754691837024766443, 0.0007509383674049532886 ),
 ( 0.000000000000000000, 1.000000000000000000 ),
 .UNSPECIFIED. ) 
 GEOMETRIC_REPRESENTATION_ITEM ( )  RATIONAL_B_SPLINE_SURFACE ( (
 ( 1.000000000000000000, 0.6711954675835484219, 1.000000000000000000),
 ( 1.000000000000000000, 0.6709646295267468474, 1.000000000000000000),
 ( 1.000000000000000000, 0.6771840716659200954, 1.000000000000000000),
 ( 1.000000000000000000, 0.6927481755867312962, 1.000000000000000000),
 ( 1.000000000000000000, 0.7017972101310044897, 1.000000000000000000),
 ( 1.000000000000000000, 0.7071067811865475727, 1.000000000000000000) ) ) 
 REPRESENTATION_ITEM ( '' )  SURFACE ( )  );
#139727 = CARTESIAN_POINT ( 'NONE',  ( -1.402160292154681736E-14, -0.7562499993171803991, 1.732050807568877637 ) ) ;
#139728 = CARTESIAN_POINT ( 'NONE',  ( 3.967344596728016093, 0.2348649212099394590, -1.912067515532820838 ) ) ;
#139729 = CARTESIAN_POINT ( 'NONE',  ( -0.6823417656250003738, 10.65104166700806765, 1.181850606188754593 ) ) ;
#139730 = CARTESIAN_POINT ( 'NONE',  ( 1.224646799147353059E-15, 1.000000000000000888, 9.999999999999998224 ) ) ;
#139731 = CARTESIAN_POINT ( 'NONE',  ( 1.441950287000768771, -2.089521377041357653, 0.7543469697938051111 ) ) ;
#139733 = ORIENTED_EDGE ( 'NONE', *, *, #177164, .T. ) ;
#139732 = CARTESIAN_POINT ( 'NONE',  ( 3.390420931869152721, 6.113185632892752075, -1.199719254218452047 ) ) ;
#139735 =( NAMED_UNIT ( * ) SI_UNIT ( $, .STERADIAN. ) SOLID_ANGLE_UNIT ( ) );
#139734 = CARTESIAN_POINT ( 'NONE',  ( -2.875737979874388284, 6.369128386579808954, -0.7216878364870458196 ) ) ;
#139736 = CARTESIAN_POINT ( 'NONE',  ( 2.693266070609028784, 6.293894182352508970, 0.000000000000000000 ) ) ;
#139737 = LINE ( 'NONE', #104018, #108138 ) ;
#139738 = DIRECTION ( 'NONE',  ( -0.6507913734559650498, -0.7592566023652995710, 0.000000000000000000 ) ) ;
#139739 = CARTESIAN_POINT ( 'NONE',  ( 11.92078253488439721, 7.617083250100837866, -0.8769071248199897806 ) ) ;
#139740 = CARTESIAN_POINT ( 'NONE',  ( 8.554831740098642001, 12.92446143018304916, 0.7216878364870438212 ) ) ;
#139741 = CARTESIAN_POINT ( 'NONE',  ( 1.082386330805637398, 1.171445227557347923, -1.573568114121715933 ) ) ;
#139742 = CARTESIAN_POINT ( 'NONE',  ( 0.6823417656249882723, 0.9885416670080832136, -1.181850606188749264 ) ) ;
#139743 = DIRECTION ( 'NONE',  ( -0.000000000000000000, -1.000000000000000000, -0.000000000000000000 ) ) ;
#139744 = TOROIDAL_SURFACE ( 'NONE', #115642, 9.580000000000003624, 0.08000000000000000167 ) ;
#139745 = CARTESIAN_POINT ( 'NONE',  ( 6.461383593301071926, 1.630371061775518271, 1.090930979547571456 ) ) ;
#139746 = CARTESIAN_POINT ( 'NONE',  ( -9.820183334999905256, 10.35130206712171130, 1.040834085586084257E-14 ) ) ;
#139747 = CARTESIAN_POINT ( 'NONE',  ( -4.392478580703220281, 8.068382744221649361, 1.040834085586084257E-14 ) ) ;
#139748 = CARTESIAN_POINT ( 'NONE',  ( 6.737200384369169903, -1.933438233944267060, 0.9670071574134844195 ) ) ;
#139750 = VERTEX_POINT ( 'NONE', #138901 ) ;
#139749 = CARTESIAN_POINT ( 'NONE',  ( -4.855791571988752331, 8.816840600628864877, 0.7998128361456481317 ) ) ;
#139751 = CARTESIAN_POINT ( 'NONE',  ( 1.499999999999987566, -1.193749999317185395, 0.000000000000000000 ) ) ;
#139752 = CARTESIAN_POINT ( 'NONE',  ( 0.8779421195594695471, -1.044212112285093585, 1.551753832453220294 ) ) ;
#139753 = CARTESIAN_POINT ( 'NONE',  ( 0.7560338623246564138, 1.671613681001963281, -0.4610611789691662632 ) ) ;
#139754 = VECTOR ( 'NONE', #122914, 1000.000000000000000 ) ;
#139756 = CARTESIAN_POINT ( 'NONE',  ( 4.511385190476093321, -2.149204750630455241, 0.4279282578087198474 ) ) ;
#139755 = CARTESIAN_POINT ( 'NONE',  ( 1.360316468749953600, 1.786458333674746601, -0.7853790794159161148 ) ) ;
#139757 = CARTESIAN_POINT ( 'NONE',  ( 4.155530545730415248, -1.916392541607782496, -1.285185436265631642 ) ) ;
#139758 = CARTESIAN_POINT ( 'NONE',  ( 6.889916301919797981, -0.8861221739737500380, 1.859037482098152338 ) ) ;
#139759 = CARTESIAN_POINT ( 'NONE',  ( 2.853385946047338084, 1.932536089888321040, -0.1910151464093560736 ) ) ;
#139760 = CARTESIAN_POINT ( 'NONE',  ( -5.056828107772852299, 7.883087978168217269, -1.082531754730548412 ) ) ;
#139761 = CARTESIAN_POINT ( 'NONE',  ( 5.150683391976684788, 2.089615912265533559, 0.3601871064465370087 ) ) ;
#139762 = DIRECTION ( 'NONE',  ( 0.000000000000000000, 0.000000000000000000, -1.000000000000000000 ) ) ;
#139763 = CARTESIAN_POINT ( 'NONE',  ( 3.217422812353257555, 1.967887761762876941, 0.4390297752325384995 ) ) ;
#139764 = CARTESIAN_POINT ( 'NONE',  ( -5.544921637864838715, 6.531792001339513654, -1.082531754730543971 ) ) ;
#139765 = CARTESIAN_POINT ( 'NONE',  ( -7.618755976236585958, 7.853246491889623648, 0.000000000000000000 ) ) ;
#139766 = CARTESIAN_POINT ( 'NONE',  ( 8.723781775389312543, 12.26516360700784958, -1.199719254218446718 ) ) ;
#139767 = CARTESIAN_POINT ( 'NONE',  ( 1.260069262837599791, 0.7379878962356714034, 1.670071910705408946 ) ) ;
#139768 = CARTESIAN_POINT ( 'NONE',  ( -5.529746549527323474, 7.544733289238903851, -1.599625672291271394 ) ) ;
#139769 = CARTESIAN_POINT ( 'NONE',  ( 0.000000000000000000, 1.000000000000000888, 8.049999999999993605 ) ) ;
#139770 = CARTESIAN_POINT ( 'NONE',  ( -11.60067993250125262, 4.148157162114866736, 5.314938114050354656 ) ) ;
#139771 = ORIENTED_EDGE ( 'NONE', *, *, #72931, .T. ) ;
#139772 = CARTESIAN_POINT ( 'NONE',  ( 5.032131441678504125, 1.061211460345131252, -1.766520746938464947 ) ) ;
#139773 = CARTESIAN_POINT ( 'NONE',  ( -6.089020385868856522, 9.157588645938716354, -1.082531754730549967 ) ) ;
#139774 = CARTESIAN_POINT ( 'NONE',  ( -2.903417451620861289, 6.539070793532962611, 0.7998128361456341429 ) ) ;
#139775 = CARTESIAN_POINT ( 'NONE',  ( -9.001723924469462901, 12.58942944760136484, -1.199719254218446718 ) ) ;
#139776 = CARTESIAN_POINT ( 'NONE',  ( 5.092447094119275874, -1.120170962321866082, 1.680348583886650315 ) ) ;
#139778 = ORIENTED_EDGE ( 'NONE', *, *, #124029, .T. ) ;
#139777 = CARTESIAN_POINT ( 'NONE',  ( 5.584718243131947091, -1.410645330893144589, 1.715908544892131626 ) ) ;
#139780 = CARTESIAN_POINT ( 'NONE',  ( 8.270110514656026979, 10.67154823856396817, 1.443375672974076540 ) ) ;
#139779 = CARTESIAN_POINT ( 'NONE',  ( -7.937372586157736443, 8.224965870130965584, 0.7998128361456341429 ) ) ;
#139781 = CARTESIAN_POINT ( 'NONE',  ( 5.307127064745490230, 8.279066444590018392, -1.199719254218452935 ) ) ;
#139782 = CARTESIAN_POINT ( 'NONE',  ( 4.030192151223922714, 1.103973922444676070, -1.740068238149700353 ) ) ;
#139783 = CARTESIAN_POINT ( 'NONE',  ( 4.078750125433938223, -0.7691220382576718917, 1.864168106189521890 ) ) ;
#139784 = VERTEX_POINT ( 'NONE', #154073 ) ;
#139785 = DIRECTION ( 'NONE',  ( -0.000000000000000000, 1.000000000000000000, 9.023263958591317418E-17 ) ) ;
#139786 = CARTESIAN_POINT ( 'NONE',  ( 3.683011284406639607, 7.448596931783069586, 0.7998128361456321445 ) ) ;
#139788 = EDGE_LOOP ( 'NONE', ( #128592, #143941, #181212, #51106 ) ) ;
#139787 = CARTESIAN_POINT ( 'NONE',  ( -6.770317605177755382, 8.992066187497757213, 1.599625672291269396 ) ) ;
#139789 = CARTESIAN_POINT ( 'NONE',  ( 5.318333368960210805, 7.618274611128187601, -1.232678415538956518 ) ) ;
#139790 = CARTESIAN_POINT ( 'NONE',  ( 3.602888598310006074, 0.9090057795711030675, -1.799647124144133858 ) ) ;
#139791 = CARTESIAN_POINT ( 'NONE',  ( 4.048646477676579813, -1.531818510360350327, -1.021117339664041834 ) ) ;
#139792 = CARTESIAN_POINT ( 'NONE',  ( 0.000000000000000000, -9.999999999999994671, 0.000000000000000000 ) ) ;
#139793 = CARTESIAN_POINT ( 'NONE',  ( 1.542099375240197245, -1.674077152000338797, -1.588604925253054745 ) ) ;
#139794 = CARTESIAN_POINT ( 'NONE',  ( 3.223806664999388172, 6.983134552466421674, -0.7998128361456362523 ) ) ;
#139795 = CARTESIAN_POINT ( 'NONE',  ( 4.235729478701364847, -1.487246874726022128, -1.568870776130903089 ) ) ;
#139796 = CARTESIAN_POINT ( 'NONE',  ( -5.052384799386910430, 9.046199365926717917, 1.214306433183764966E-14 ) ) ;
#139797 = EDGE_CURVE ( 'NONE', #48021, #9929, #139979, .T. ) ;
#139798 = CARTESIAN_POINT ( 'NONE',  ( 3.111036021816812713, 0.8295677418227834776, -2.143598788741421401 ) ) ;
#139799 = DIRECTION ( 'NONE',  ( 0.000000000000000000, 0.000000000000000000, 1.000000000000000000 ) ) ;
#139800 = CARTESIAN_POINT ( 'NONE',  ( 1.990876257202532695, 1.628914321797021669, -0.9196232060951770038 ) ) ;
#139801 = CARTESIAN_POINT ( 'NONE',  ( 0.2628735715076990220, -1.758816568047173234, -0.8906303152973747972 ) ) ;
#139802 = VECTOR ( 'NONE', #98474, 1000.000000000000000 ) ;
#139804 = FILL_AREA_STYLE_COLOUR ( '', #22113 ) ;
#139803 = CARTESIAN_POINT ( 'NONE',  ( 1.364683531249988535, 5.155208333674749177, -0.7879004041258300672 ) ) ;
#139806 = CARTESIAN_POINT ( 'NONE',  ( 1.331021600797330118, 2.127646391749141941, 0.5858054460900484761 ) ) ;
#139805 = CARTESIAN_POINT ( 'NONE',  ( -6.423865854776591000, 6.388931673527803667, 1.040834085586084257E-14 ) ) ;
#139807 = CARTESIAN_POINT ( 'NONE',  ( 11.84668730067608600, 10.90000000000000036, -1.400000000000001910 ) ) ;
#139808 = CARTESIAN_POINT ( 'NONE',  ( 6.166260936116925606, 6.088392601758203071, 0.7998128361456341429 ) ) ;
#139809 = CARTESIAN_POINT ( 'NONE',  ( -4.401593425930945713, 8.286942763561420122, 1.040834085586084257E-14 ) ) ;
#139810 = CARTESIAN_POINT ( 'NONE',  ( -7.770158002573702483, -5.767087321559040802, 7.786489011996849285 ) ) ;
#139811 = CARTESIAN_POINT ( 'NONE',  ( 6.666873957964818409, -1.802346848367493592, -0.7993007979140465125 ) ) ;
#139812 = CARTESIAN_POINT ( 'NONE',  ( 5.813149116883928436, 2.032396105517704221, 1.093072976444838362 ) ) ;
#139813 = CARTESIAN_POINT ( 'NONE',  ( 6.883263157960402445, 0.001763689368145578400, 1.846037217754380011 ) ) ;
#139814 = CARTESIAN_POINT ( 'NONE',  ( 3.344635507851092981, -2.031254381041375456, -0.3572892473815546532 ) ) ;
#139815 = CARTESIAN_POINT ( 'NONE',  ( 6.317736394288135493, 8.393778431468064127, 1.443375672974076540 ) ) ;
#139816 = CARTESIAN_POINT ( 'NONE',  ( 6.047819040147648373, 9.213483425884394507, 1.199719254218452047 ) ) ;
#139817 = CARTESIAN_POINT ( 'NONE',  ( 7.144783764277405247, 8.398297815487545392, -1.082531754730543971 ) ) ;
#139818 = CARTESIAN_POINT ( 'NONE',  ( -0.6823417656250212460, 2.863541667008084879, 1.181850606188767472 ) ) ;
#139819 = CARTESIAN_POINT ( 'NONE',  ( 3.836594282542902246, 7.419851063034623273, 0.7216878364870317197 ) ) ;
#139820 = CARTESIAN_POINT ( 'NONE',  ( 5.881339278728036746, -0.05926448915108929044, 2.170540009233146606 ) ) ;
#139821 = DIRECTION ( 'NONE',  ( 0.7592566023652994600, -0.6507913734559651608, -0.000000000000000000 ) ) ;
#139823 = CARTESIAN_POINT ( 'NONE',  ( 4.792441439910442469, 1.527937338083688923, -1.027124420945781935 ) ) ;
#139822 = CARTESIAN_POINT ( 'NONE',  ( -3.145128448690323264, 4.692402494937224056, -1.443375672974059665 ) ) ;
#139825 = DIRECTION ( 'NONE',  ( 0.7592566023653005702, -0.6507913734559639396, 0.000000000000000000 ) ) ;
#139824 = CARTESIAN_POINT ( 'NONE',  ( -10.04733898909035794, 1.529612873802629780, -6.247711339171014622 ) ) ;
#139826 = CARTESIAN_POINT ( 'NONE',  ( 6.620655732516649294, -0.002413161512292843602, 2.173887093218459743 ) ) ;
#139827 = CARTESIAN_POINT ( 'NONE',  ( 0.2802489257003986101, -1.812731005579379051, -0.4610361243657657981 ) ) ;
#139828 = CARTESIAN_POINT ( 'NONE',  ( 6.719576162335838099, -2.196678875378419882, 0.5415391501680610897 ) ) ;
#139829 = EDGE_CURVE ( 'NONE', #121570, #73222, #1976, .T. ) ;
#139830 = CARTESIAN_POINT ( 'NONE',  ( -4.645415345243833372, 7.101964347008438594, 1.385782282575825919 ) ) ;
#139831 = DIRECTION ( 'NONE',  ( 0.000000000000000000, 0.000000000000000000, 1.000000000000000000 ) ) ;
#139832 = CARTESIAN_POINT ( 'NONE',  ( 5.644368669187761256, 7.458116220610145675, 1.329639117314229235 ) ) ;
#139833 = CARTESIAN_POINT ( 'NONE',  ( -5.275531169048922386, 5.327410250078064458, -0.7216878364870338292 ) ) ;
#139834 = CARTESIAN_POINT ( 'NONE',  ( 11.48243876534946217, 13.79999999999999893, -3.200000000000001510 ) ) ;
#139835 = CARTESIAN_POINT ( 'NONE',  ( 2.447821898584545242, 1.769419436591600725, 0.04612135499031978086 ) ) ;
#139836 = CARTESIAN_POINT ( 'NONE',  ( 6.252595736715376162, 1.991502868314236174, 0.2931975281106109499 ) ) ;
#139838 = CARTESIAN_POINT ( 'NONE',  ( 3.743669890235715947, 1.900728030520698830, -0.2378226680747745625 ) ) ;
#139837 = CARTESIAN_POINT ( 'NONE',  ( -9.073431116043565225, 11.60875560684942265, -1.599625672291263179 ) ) ;
#139839 = CARTESIAN_POINT ( 'NONE',  ( 4.422284282497963126, 0.9263432559908044706, 1.738082477136545956 ) ) ;
#139840 = CARTESIAN_POINT ( 'NONE',  ( 6.275650217586050239, 0.3411474428106214263, -1.990588700022011714 ) ) ;
#139841 = CARTESIAN_POINT ( 'NONE',  ( -2.137381772448751605, 5.645362501165475777, -0.7998128361456281477 ) ) ;
#139842 = CARTESIAN_POINT ( 'NONE',  ( 2.571000202304725590, 0.09389976206976291540, -1.868427151830873267 ) ) ;
#139844 = ORIENTED_EDGE ( 'NONE', *, *, #165066, .T. ) ;
#139843 = CARTESIAN_POINT ( 'NONE',  ( 5.988827324695590981, -0.2600698726980456010, -1.705031240916178525 ) ) ;
#139846 = CARTESIAN_POINT ( 'NONE',  ( 3.714570900464274850, 6.317121236308204324, 1.082531754730558626 ) ) ;
#139845 = CARTESIAN_POINT ( 'NONE',  ( 2.245003380770736801, 0.4850519687749441644, 2.152760086278446394 ) ) ;
#139847 = CARTESIAN_POINT ( 'NONE',  ( 1.364683531249990311, 3.446875000341416584, 1.214306433183764966E-14 ) ) ;
#139848 = CARTESIAN_POINT ( 'NONE',  ( 6.127397123722368555, 0.1457569626216181913, -1.956525209266091192 ) ) ;
#139849 = CARTESIAN_POINT ( 'NONE',  ( 7.052212457402625922, 11.37933163361175382, -0.7998128361456291469 ) ) ;
#139850 = DIRECTION ( 'NONE',  ( -0.6507913734559640506, -0.7592566023653004592, 0.000000000000000000 ) ) ;
#139851 = DIRECTION ( 'NONE',  ( 0.000000000000000000, 1.000000000000000000, 0.000000000000000000 ) ) ;
#139852 = CARTESIAN_POINT ( 'NONE',  ( -3.242371291962510504, 6.934516940598226320, 1.040834085586084257E-14 ) ) ;
#139853 = FACE_OUTER_BOUND ( 'NONE', #180271, .T. ) ;
#139854 = VERTEX_POINT ( 'NONE', #156217 ) ;
#139855 = CARTESIAN_POINT ( 'NONE',  ( 2.506376218629560171, 2.069854378281150709, 0.05321039126485183068 ) ) ;
#139856 = CARTESIAN_POINT ( 'NONE',  ( -1.500000000000013101, 3.379166666666691299, -0.8660254037844313801 ) ) ;
#139857 = CARTESIAN_POINT ( 'NONE',  ( 5.834086172582112262, 5.700855377634248100, 1.040834085586084257E-14 ) ) ;
#139858 = CARTESIAN_POINT ( 'NONE',  ( 5.415556014015861841, 5.282846535965431300, -0.7998128361456481317 ) ) ;
#139859 = CARTESIAN_POINT ( 'NONE',  ( -0.07552420640595960966, -0.8660980012666683603, -1.823048286210580793 ) ) ;
#139860 = DIRECTION ( 'NONE',  ( -0.9998476951563912696, 0.000000000000000000, 0.01745240643728004568 ) ) ;
#139861 = CARTESIAN_POINT ( 'NONE',  ( -1.364683531250012516, 3.530208333674758059, 0.7879004041258379498 ) ) ;
#139862 = EDGE_CURVE ( 'NONE', #116385, #142909, #4095, .T. ) ;
#139864 = CARTESIAN_POINT ( 'NONE',  ( 10.22248463502393001, 11.02857961705718282, 0.7216878364870438212 ) ) ;
#139863 = CARTESIAN_POINT ( 'NONE',  ( 0.07479286986305544449, 2.046156589154801253, -2.272744413733415403 ) ) ;
#139865 = CARTESIAN_POINT ( 'NONE',  ( 5.483749906247235906, 1.861732415968733401, 0.7741956105717237024 ) ) ;
#139866 = CARTESIAN_POINT ( 'NONE',  ( 5.225768846659354594, 0.7701814094057590765, -1.754262016157917881 ) ) ;
#139867 = CARTESIAN_POINT ( 'NONE',  ( 6.539320575229278454, 3.689604457162498630, 2.617406275049142916 ) ) ;
#139868 = CARTESIAN_POINT ( 'NONE',  ( 2.507599501126521524, -2.167277876680247850, 0.3246147914140809498 ) ) ;
#139869 = CARTESIAN_POINT ( 'NONE',  ( -1.500000000000013101, 2.702083334016155636, 0.8660254037844403729 ) ) ;
#139870 = CARTESIAN_POINT ( 'NONE',  ( 1.986440140746603911, -1.173720106059353396, 1.509789020923378189 ) ) ;
#139871 = CARTESIAN_POINT ( 'NONE',  ( -6.552668314106420588, 6.539201209412602189, -0.7998128361456291469 ) ) ;
#139873 = CARTESIAN_POINT ( 'NONE',  ( 6.187133403942106646, 1.760427041935657799, 1.175965560660442444 ) ) ;
#139872 = FACE_OUTER_BOUND ( 'NONE', #197346, .T. ) ;
#139874 = CARTESIAN_POINT ( 'NONE',  ( 0.6823417656249969321, 9.588541667008065872, -1.181850606188757036 ) ) ;
#139876 = CARTESIAN_POINT ( 'NONE',  ( -5.712781623311813384, 7.758274208654143855, -1.599625672291271394 ) ) ;
#139875 = CARTESIAN_POINT ( 'NONE',  ( 6.409741707328596938, -1.031184584194230647, -1.933826218581576439 ) ) ;
#139878 = VERTEX_POINT ( 'NONE', #103185 ) ;
#139877 = CARTESIAN_POINT ( 'NONE',  ( 3.029983902540707152, 0.9595516922606081023, -1.432977992855663185 ) ) ;
#139879 = CARTESIAN_POINT ( 'NONE',  ( 5.924112389714111693, -2.104401743431310923, 0.2612745606217213856 ) ) ;
#139880 = CARTESIAN_POINT ( 'NONE',  ( 6.923409998072794558, 11.22906209772695618, 1.040834085586084257E-14 ) ) ;
#139881 = CARTESIAN_POINT ( 'NONE',  ( 5.497994985541524215, 6.373081223675282736, -1.199719254218445830 ) ) ;
#139882 = CARTESIAN_POINT ( 'NONE',  ( 0.1331565106231328843, 0.003911343561965873426, -1.946049565259087455 ) ) ;
#139883 = EDGE_CURVE ( 'NONE', #190021, #44750, #206001, .T. ) ;
#139884 = FACE_OUTER_BOUND ( 'NONE', #155963, .T. ) ;
#139885 = CARTESIAN_POINT ( 'NONE',  ( 6.654354466208897811, 6.657835053532175529, 0.7998128361456341429 ) ) ;
#139886 = CARTESIAN_POINT ( 'NONE',  ( 0.1399997263886003374, 0.002789056014650820314, -1.999853399661279063 ) ) ;
#139887 = ORIENTED_EDGE ( 'NONE', *, *, #98482, .F. ) ;
#139888 = CARTESIAN_POINT ( 'NONE',  ( -11.86239285000045918, 13.88000000000000078, -1.812080536912753059 ) ) ;
#139889 = VERTEX_POINT ( 'NONE', #39247 ) ;
#139890 = CARTESIAN_POINT ( 'NONE',  ( 2.508236654460756387, -1.806733793710820324, -0.1315605372460958433 ) ) ;
#139891 = ORIENTED_EDGE ( 'NONE', *, *, #207315, .F. ) ;
#139892 = CARTESIAN_POINT ( 'NONE',  ( 10.71502147350184231, 11.39527989537399755, 0.000000000000000000 ) ) ;
#139893 = CARTESIAN_POINT ( 'NONE',  ( 5.411639590510088027, 6.342609606130419131, -1.199719254218452047 ) ) ;
#139894 = CARTESIAN_POINT ( 'NONE',  ( 3.721195823539941827, 1.555462818066039254, 0.9281401003491447366 ) ) ;
#139895 = CARTESIAN_POINT ( 'NONE',  ( 0.000000000000000000, 14.48195938056239385, 0.000000000000000000 ) ) ;
#139896 = CARTESIAN_POINT ( 'NONE',  ( 1.499999999999996891, 9.177083334016128191, -0.8660254037844378194 ) ) ;
#139897 = CARTESIAN_POINT ( 'NONE',  ( 5.849510849484250485, 6.002983934024645585, 0.3487602046992159810 ) ) ;
#139899 = CARTESIAN_POINT ( 'NONE',  ( 1.364683531249996529, 14.71354166700806410, 0.7879004041258405033 ) ) ;
#139898 = CARTESIAN_POINT ( 'NONE',  ( 4.791365544089026152, -1.701862485369805000, 0.7535167838805619800 ) ) ;
#139900 = CARTESIAN_POINT ( 'NONE',  ( 3.005391328865916645, -1.845313015785840172, 0.5138285116655214591 ) ) ;
#139901 = CARTESIAN_POINT ( 'NONE',  ( 1.131563826228650038, -1.154680578942975044, -1.414029504508321100 ) ) ;
#139902 = VECTOR ( 'NONE', #22933, 1000.000000000000000 ) ;
#139903 = CARTESIAN_POINT ( 'NONE',  ( 1.499999999999985789, -1.099999999999976108, 2.579999999999999183 ) ) ;
#139904 = CARTESIAN_POINT ( 'NONE',  ( -10.92046113480654768, 4.688422163420479016, 4.459782501114215592 ) ) ;
#139905 = CARTESIAN_POINT ( 'NONE',  ( 5.794989345469916842, 7.230977472937116346, 1.182549002416101835 ) ) ;
#139906 = CARTESIAN_POINT ( 'NONE',  ( -11.48767021851170078, 9.769957725361562595, 3.470194894594595070 ) ) ;
#139907 = CARTESIAN_POINT ( 'NONE',  ( -6.329050364910258075, 6.923295760524523779, 0.8374253472341108839 ) ) ;
#139908 = AXIS2_PLACEMENT_3D ( 'NONE', #134055, #51715, #164384 ) ;
#139909 = CARTESIAN_POINT ( 'NONE',  ( 7.348156068926750883, 8.635565504245116486, -1.082531754730537976 ) ) ;
#139910 = EDGE_CURVE ( 'NONE', #1117, #210323, #66243, .T. ) ;
#139911 = CARTESIAN_POINT ( 'NONE',  ( -3.253066792275140173, 5.882662793374543675, 1.199719254218462483 ) ) ;
#139912 = CARTESIAN_POINT ( 'NONE',  ( 0.1632417891470130944, -1.931755829615459996, -0.9703963252955111196 ) ) ;
#139913 = CARTESIAN_POINT ( 'NONE',  ( 1.482492212676550070, -0.3080716119066116421, -2.067685480015791111 ) ) ;
#139914 = CARTESIAN_POINT ( 'NONE',  ( 6.651400849050447484, -1.547811450530303778, -1.146644766597894938 ) ) ;
#139915 = CARTESIAN_POINT ( 'NONE',  ( -6.715366157470410435, 6.729015360003925750, -0.7998128361456291469 ) ) ;
#139916 = EDGE_CURVE ( 'NONE', #153986, #54700, #85026, .T. ) ;
#139917 = CARTESIAN_POINT ( 'NONE',  ( 2.485134345765506847, 1.670108983700506977, -0.7376146046164518966 ) ) ;
#139918 = CARTESIAN_POINT ( 'NONE',  ( 2.965657822035951963, 0.3232568108629539361, -2.182957019552448141 ) ) ;
#139919 = CARTESIAN_POINT ( 'NONE',  ( 11.95360554405576714, 12.49555003497412464, 1.059413164304728872 ) ) ;
#139920 = CARTESIAN_POINT ( 'NONE',  ( 1.248149539447914735, 0.9399939672071171426, -1.665319807275446706 ) ) ;
#139921 =( BOUNDED_SURFACE ( )  B_SPLINE_SURFACE ( 3, 2, ( 
 ( #165930, #69467, #135572 ),
 ( #184293, #20717, #168062 ),
 ( #35918, #87878, #117238 ),
 ( #182158, #68401, #101994 ) ),
 .UNSPECIFIED., .F., .F., .F. ) 
 B_SPLINE_SURFACE_WITH_KNOTS ( ( 4, 4 ),
 ( 3, 3 ),
 ( 0.005313560486515473899, 0.008339948430246690511 ),
 ( 0.000000000000000000, 1.000000000000000000 ),
 .UNSPECIFIED. ) 
 GEOMETRIC_REPRESENTATION_ITEM ( )  RATIONAL_B_SPLINE_SURFACE ( (
 ( 1.000000000000000000, 0.7184380228464071205, 1.000000000000000000),
 ( 1.000000000000000000, 0.7185467277397555863, 1.000000000000000000),
 ( 1.000000000000000000, 0.7186585579881037411, 1.000000000000000000),
 ( 1.000000000000000000, 0.7187737999613683648, 1.000000000000000000) ) ) 
 REPRESENTATION_ITEM ( '' )  SURFACE ( )  );
#139922 = EDGE_LOOP ( 'NONE', ( #123712, #190109, #147087, #83832 ) ) ;
#139923 = AXIS2_PLACEMENT_3D ( 'NONE', #88040, #166087, #135736 ) ;
#139924 = CARTESIAN_POINT ( 'NONE',  ( 1.680066331807037905, -1.091455746017004014, -1.639250758224161775 ) ) ;
#139925 = CARTESIAN_POINT ( 'NONE',  ( 2.946749062660087848, -1.589232290113586910, -1.115973732403415131 ) ) ;
#139926 = ORIENTED_EDGE ( 'NONE', *, *, #3121, .T. ) ;
#139927 = DIRECTION ( 'NONE',  ( -5.828670879282089587E-16, 0.8656921114426507913, -0.5005768354468322912 ) ) ;
#139929 = CARTESIAN_POINT ( 'NONE',  ( 6.403157621081472683, -1.572583794901558862, 0.9946829920960180704 ) ) ;
#139928 = CARTESIAN_POINT ( 'NONE',  ( -3.467853430045390706, 7.267855778353407459, 0.7998128361456352531 ) ) ;
#139930 = CARTESIAN_POINT ( 'NONE',  ( 5.682802662783380754, 6.658966523782627434, 1.199719254218452935 ) ) ;
#139931 = DIRECTION ( 'NONE',  ( 0.000000000000000000, 1.000000000000000000, 0.000000000000000000 ) ) ;
#139932 = CARTESIAN_POINT ( 'NONE',  ( 10.01963921569910632, 11.64833282552586091, 1.199719254218450271 ) ) ;
#139933 = CARTESIAN_POINT ( 'NONE',  ( -6.771371375382467583, 6.864631124226471037, -0.7998128361456362523 ) ) ;
#139934 = CARTESIAN_POINT ( 'NONE',  ( 2.191216702865448784, 1.696344223602393786, 1.387594652289561248 ) ) ;
#139935 = CARTESIAN_POINT ( 'NONE',  ( 2.223174002961016082, 5.537527403522402025, -0.7216878364870267237 ) ) ;
#139936 = CARTESIAN_POINT ( 'NONE',  ( 5.203297092594585393, 9.292540051327542017, 0.7998128361456341429 ) ) ;
#139937 = DIRECTION ( 'NONE',  ( 1.276756478318932585E-15, -1.000000000000000000, 1.665334536937738262E-16 ) ) ;
#139938 = CARTESIAN_POINT ( 'NONE',  ( 3.053144290054691901, -1.492835736363471888, -1.050712463094093385 ) ) ;
#139939 = CARTESIAN_POINT ( 'NONE',  ( 2.550000000000000266, 2.499999999999998668, -1.849324200890695824 ) ) ;
#139940 = CARTESIAN_POINT ( 'NONE',  ( -9.707274797704657843, 11.38787068781932987, 1.082531754730558626 ) ) ;
#139941 = CARTESIAN_POINT ( 'NONE',  ( -5.543378919943204863, 7.538303290789565736, -1.349654061105177050 ) ) ;
#139942 = DIRECTION ( 'NONE',  ( 0.000000000000000000, 8.546850786086437571E-32, 1.000000000000000000 ) ) ;
#139943 = PRESENTATION_LAYER_ASSIGNMENT (  '', '', ( #112307 ) ) ;
#139944 = CARTESIAN_POINT ( 'NONE',  ( 9.088043039861931405, 9.497138389460751284, 1.040834085586084257E-14 ) ) ;
#139945 = CARTESIAN_POINT ( 'NONE',  ( 2.350114058346234547, 1.926077408352431464, 0.04734757869597795016 ) ) ;
#139946 = CARTESIAN_POINT ( 'NONE',  ( 6.280128941539553367, -1.086961472313338284, -1.632890767417946032 ) ) ;
#139947 = CARTESIAN_POINT ( 'NONE',  ( 1.500000000000001332, 14.37499999999999822, 0.000000000000000000 ) ) ;
#139948 = CARTESIAN_POINT ( 'NONE',  ( -7.660520486921249983, 8.896027641951645748, -1.199719254218446718 ) ) ;
#139949 = CARTESIAN_POINT ( 'NONE',  ( 4.147904930777053245, 6.926640621626830807, -1.199719254218452047 ) ) ;
#139950 = CARTESIAN_POINT ( 'NONE',  ( -5.777182852754558340, 5.912670547734647286, 0.000000000000000000 ) ) ;
#139951 = AXIS2_PLACEMENT_3D ( 'NONE', #16102, #200189, #198068 ) ;
#139952 = CARTESIAN_POINT ( 'NONE',  ( 9.999301985278609806, 11.62460605670194447, 1.199719254218452047 ) ) ;
#139953 = CARTESIAN_POINT ( 'NONE',  ( 11.88168509644349058, 13.87999999999997947, 1.685788023084328513 ) ) ;
#139954 = CARTESIAN_POINT ( 'NONE',  ( 5.647352632913819726, 1.828451368696734747, -0.9708816006866529680 ) ) ;
#139956 = CARTESIAN_POINT ( 'NONE',  ( 0.6823417656249899377, 2.655208333674753618, 1.181850606188767472 ) ) ;
#139955 = CARTESIAN_POINT ( 'NONE',  ( -0.1237769027084348328, -0.1346504581853508187, -1.811164470923332104 ) ) ;
#139957 = VERTEX_POINT ( 'NONE', #90149 ) ;
#139958 = EDGE_LOOP ( 'NONE', ( #178218, #65309, #50184, #91391, #132330, #123343, #35812, #20393, #81373, #29199, #155674, #53903, #91264, #47942, #47523, #142198, #140598, #68293, #97010, #29552, #105146, #95018, #45488, #86947, #193013 ) ) ;
#139959 = CARTESIAN_POINT ( 'NONE',  ( 5.590575961319281362, -0.5612465257360791382, 2.229044676911738687 ) ) ;
#139960 = CARTESIAN_POINT ( 'NONE',  ( 6.697364695470787943, 7.876308901879812474, -1.082531754730543083 ) ) ;
#139962 = DIRECTION ( 'NONE',  ( 0.000000000000000000, 1.000000000000000000, 0.000000000000000000 ) ) ;
#139961 = CARTESIAN_POINT ( 'NONE',  ( 4.746763178560254204, 6.631252689777363152, 1.443375672974065660 ) ) ;
#139963 = CARTESIAN_POINT ( 'NONE',  ( -0.02880301295727759683, -0.006976478922920535501, -2.273770288744044521 ) ) ;
#139964 = CARTESIAN_POINT ( 'NONE',  ( 1.225000000000010747, 0.3749999999999864553, -2.081668171172168513E-14 ) ) ;
#139965 = CARTESIAN_POINT ( 'NONE',  ( -5.641074431737709283, 8.738948049406083385, -1.199719254218452047 ) ) ;
#139966 = CARTESIAN_POINT ( 'NONE',  ( 4.839755972451986743, 1.936857930295164065, 0.1413805851513943446 ) ) ;
#139967 = ORIENTED_EDGE ( 'NONE', *, *, #8949, .T. ) ;
#139969 = CARTESIAN_POINT ( 'NONE',  ( 9.544576953896278582, 10.23768732240824164, 0.000000000000000000 ) ) ;
#139968 = CIRCLE ( 'NONE', #122722, 9.499999999999991118 ) ;
#139970 = ORIENTED_EDGE ( 'NONE', *, *, #19832, .F. ) ;
#139971 = CARTESIAN_POINT ( 'NONE',  ( 6.416268857797894576, -1.911816439625917852, 0.05404522429636184067 ) ) ;
#139972 = CARTESIAN_POINT ( 'NONE',  ( 0.3458015845922198239, 1.719860733928044949, 0.1322621976239789499 ) ) ;
#139973 = CARTESIAN_POINT ( 'NONE',  ( 5.454314652423888354, -1.275559214091715354, 1.561879324423600890 ) ) ;
#139975 = CARTESIAN_POINT ( 'NONE',  ( -4.556949027968976829, 5.449433633119473264, 1.082531754730549078 ) ) ;
#139974 = CARTESIAN_POINT ( 'NONE',  ( -9.664264568442742842, 10.16939683947169115, -0.7998128361456291469 ) ) ;
#139976 = CARTESIAN_POINT ( 'NONE',  ( 3.285556943750000514, -1.451041666188708890, 1.896917185911906500 ) ) ;
#139978 = CARTESIAN_POINT ( 'NONE',  ( 1.006321374186702311, 1.343689884961623227, -1.152001066587736267 ) ) ;
#139977 = CARTESIAN_POINT ( 'NONE',  ( 2.466838723508807174, 0.1015857406408589014, -2.088290385120465498 ) ) ;
#139979 = LINE ( 'NONE', #72801, #64326 ) ;
#139981 = CARTESIAN_POINT ( 'NONE',  ( 4.189605479905995189, -0.8790709274306067744, 2.117190895528203498 ) ) ;
#139980 = CARTESIAN_POINT ( 'NONE',  ( 4.543917759235442944, 5.330267469643351852, 1.199719254218452935 ) ) ;
#139982 = CARTESIAN_POINT ( 'NONE',  ( 2.483973769465233961, -0.2969572910719043279, -1.714626640263767543 ) ) ;
#139983 = CARTESIAN_POINT ( 'NONE',  ( 3.842846474469570062, 6.570739089268092137, -1.199719254218452047 ) ) ;
#139984 = CARTESIAN_POINT ( 'NONE',  ( 2.953504815971871977, -1.868289524550557523, 1.003269902519101864 ) ) ;
#139985 = CARTESIAN_POINT ( 'NONE',  ( 1.854049621773927514, 4.999999999999997335, -0.7500000000000006661 ) ) ;
#139986 = CARTESIAN_POINT ( 'NONE',  ( 1.721629994271107744, -1.484111423267266527, -0.8961763045370867431 ) ) ;
#139987 = CARTESIAN_POINT ( 'NONE',  ( -1.360316468750036645, 2.151041667008108060, -0.7853790794159301036 ) ) ;
#139988 = CARTESIAN_POINT ( 'NONE',  ( 1.117373073715557164, 0.3680575366376471758, -1.824110739772739631 ) ) ;
#139989 = CARTESIAN_POINT ( 'NONE',  ( 2.664704904736223234, -0.8290184881076659851, -2.006861667775594160 ) ) ;
#139990 = CARTESIAN_POINT ( 'NONE',  ( 5.769158057814842699, 6.689438141327490150, 1.199719254218462483 ) ) ;
#139991 = CARTESIAN_POINT ( 'NONE',  ( 3.450407915430803385, -1.350735839785843773, 1.497501794165828626 ) ) ;
#139992 = CARTESIAN_POINT ( 'NONE',  ( 2.312500000000001776, 1.451031289061216478, 1.451031289061020857 ) ) ;
#139993 = CARTESIAN_POINT ( 'NONE',  ( -1.201851678989727383E-14, 3.368750000682815049, -1.732050807568863648 ) ) ;
#139994 = CARTESIAN_POINT ( 'NONE',  ( 1.325083149161108365, -0.05013198271685941065, 1.925904219417676089 ) ) ;
#139995 = CARTESIAN_POINT ( 'NONE',  ( 1.364683531250000303, 14.50520833367473372, -0.7879004041258355073 ) ) ;
#139996 = CARTESIAN_POINT ( 'NONE',  ( 4.816739660502834752, -0.7493216981008001820, -2.091313736985983773 ) ) ;
#139997 = ORIENTED_EDGE ( 'NONE', *, *, #3680, .F. ) ;
#139998 = CARTESIAN_POINT ( 'NONE',  ( -0.2108831679771203116, 0.7314853703891763814, -1.979988191570913880 ) ) ;
#139999 = CARTESIAN_POINT ( 'NONE',  ( -1.402160292154681736E-14, 0.3375000000000208389, -1.732050807568870754 ) ) ;
#140000 = CARTESIAN_POINT ( 'NONE',  ( 6.401421083946654100, 10.62007503124645957, -0.7998128361456291469 ) ) ;
#140001 = CARTESIAN_POINT ( 'NONE',  ( -1.402160292154681736E-14, -0.3031249996585801965, -1.575800808251665908 ) ) ;
#140002 = CARTESIAN_POINT ( 'NONE',  ( 6.170221320256972675, 2.215557125880045053, -0.1624646739342323065 ) ) ;
#140003 = CARTESIAN_POINT ( 'NONE',  ( 4.615648854252428102, 0.4318217149890530848, -1.913582009320368371 ) ) ;
#140004 = CARTESIAN_POINT ( 'NONE',  ( 9.327646496521982300, 11.90534021740758064, -1.443375672974057666 ) ) ;
#140005 = CARTESIAN_POINT ( 'NONE',  ( -1.424698021954212912, 3.957288782964809570, -0.4926413923218403434 ) ) ;
#140006 = CARTESIAN_POINT ( 'NONE',  ( 5.729810862507367375, -1.428767958649424408, -1.754208347296302373 ) ) ;
#140007 = CARTESIAN_POINT ( 'NONE',  ( -5.560252395380252288, 7.580323442733986283, 1.443375672974058777 ) ) ;
#140008 = CARTESIAN_POINT ( 'NONE',  ( 2.822777196768213592, -1.424206252425799679, 1.492280444834346520 ) ) ;
#140009 = CARTESIAN_POINT ( 'NONE',  ( -5.961834861707238531, 7.978559976790334574, -1.599625672291263179 ) ) ;
#140010 = CARTESIAN_POINT ( 'NONE',  ( -1.500000000000013101, 2.452083334016154748, 0.8660254037844403729 ) ) ;
#140011 = CARTESIAN_POINT ( 'NONE',  ( -0.6823417656249969321, 5.780208333674756283, -1.181850606188749264 ) ) ;
#140012 = CARTESIAN_POINT ( 'NONE',  ( 4.604681543780857034, 1.447206075137374759, -1.185162884121161442 ) ) ;
#140013 = CARTESIAN_POINT ( 'NONE',  ( 3.656634503061773067, 0.9670403524725273980, 1.439223064172075350 ) ) ;
#140014 = CARTESIAN_POINT ( 'NONE',  ( 1.751089554790756342, 1.735802523247106377, -0.1280615824842730732 ) ) ;
#140015 = CARTESIAN_POINT ( 'NONE',  ( 1.136728594277321980, 0.4534141614637792195, 2.246936901365268913 ) ) ;
#140016 = CARTESIAN_POINT ( 'NONE',  ( 0.6048602812970468312, -0.7454967350204610987, -2.077179305122120123 ) ) ;
#140017 = CARTESIAN_POINT ( 'NONE',  ( 4.300388110500093397, 1.614917507917512207, -1.327843252744983049 ) ) ;
#140018 = CARTESIAN_POINT ( 'NONE',  ( 5.402268692527759875, 1.469326413266746956, -1.269838510729433212 ) ) ;
#140019 = ORIENTED_EDGE ( 'NONE', *, *, #67872, .T. ) ;
#140020 = CARTESIAN_POINT ( 'NONE',  ( 0.2818752512256904597, 1.674885806461807958, -1.122501178855893400 ) ) ;
#140021 = CARTESIAN_POINT ( 'NONE',  ( -0.1225938595818750754, -1.897163925677572305, -0.9476133185889324961 ) ) ;
#140022 = CYLINDRICAL_SURFACE ( 'NONE', #59169, 6.249999999999995559 ) ;
#140023 = CARTESIAN_POINT ( 'NONE',  ( 6.451795992440088057, -1.844709169062180409, -0.8146298745319994206 ) ) ;
#140024 = CARTESIAN_POINT ( 'NONE',  ( -8.853638004923878313, 10.28799807962136548, 1.199719254218462483 ) ) ;
#140025 = CARTESIAN_POINT ( 'NONE',  ( 5.849453209292126310, 8.911780279894442103, 1.199719254218462483 ) ) ;
#140026 =( LENGTH_UNIT ( ) NAMED_UNIT ( * ) SI_UNIT ( .MILLI., .METRE. ) );
#140027 = CARTESIAN_POINT ( 'NONE',  ( 4.143042835627613663, -1.587387879459275286, 0.9017181768668989239 ) ) ;
#140028 = CARTESIAN_POINT ( 'NONE',  ( 2.696532018272995490, -2.200798769047443759, -0.1632673417703081331 ) ) ;
#140029 = VERTEX_POINT ( 'NONE', #22969 ) ;
#140030 = CARTESIAN_POINT ( 'NONE',  ( -5.759181390754928742, 9.941071732514568993, 0.000000000000000000 ) ) ;
#140031 = CARTESIAN_POINT ( 'NONE',  ( -5.002032328799064231, 4.800402236545811441, -0.7998128361456362523 ) ) ;
#140032 = CARTESIAN_POINT ( 'NONE',  ( -3.285556943749998737, -2.267708332855375986, 1.896917185911908499 ) ) ;
#140033 = CARTESIAN_POINT ( 'NONE',  ( -5.831978632172702071, 9.955725504176825780, 0.7998128361456481317 ) ) ;
#140034 = CARTESIAN_POINT ( 'NONE',  ( 2.689718276569666333, 1.916506935140523726, -0.6377304922457660563 ) ) ;
#140035 = ADVANCED_FACE ( 'NONE', ( #203853 ), #144367, .T. ) ;
#140036 = CARTESIAN_POINT ( 'NONE',  ( -4.553559489343377287, 6.405848385690952718, -1.599625672291271394 ) ) ;
#140037 = CARTESIAN_POINT ( 'NONE',  ( 2.904952611580268851, -1.549997479519327648, 1.029535618745812675 ) ) ;
#140038 = CARTESIAN_POINT ( 'NONE',  ( 8.516493047678546091, 13.08765898893368629, -0.7998128361456352531 ) ) ;
#140039 = CARTESIAN_POINT ( 'NONE',  ( 1.252085211431710698, 2.800000000000024691, 0.7750000000000152323 ) ) ;
#140040 = ORIENTED_EDGE ( 'NONE', *, *, #23441, .T. ) ;
#140041 = CARTESIAN_POINT ( 'NONE',  ( -5.362413449404877852, 6.214902764849178141, -1.199719254218446718 ) ) ;
#140042 = CARTESIAN_POINT ( 'NONE',  ( -7.700141177557535244, 11.07091624287075859, -1.199719254218446718 ) ) ;
#140043 = CARTESIAN_POINT ( 'NONE',  ( 5.039593146249602640, -1.293522693445446015, -1.288650932716684849 ) ) ;
#140045 = CARTESIAN_POINT ( 'NONE',  ( -4.550628574872730425, 7.191434026324334816, -1.338276217581878980 ) ) ;
#140044 = CARTESIAN_POINT ( 'NONE',  ( -3.871735385154307263, 6.674719161725423788, -1.199719254218450271 ) ) ;
#140046 = CARTESIAN_POINT ( 'NONE',  ( 5.620636616140949116, 7.477306742562066511, -1.332712173395997013 ) ) ;
#140047 = CARTESIAN_POINT ( 'NONE',  ( 0.4031117941524774984, 0.2875473383168804520, 1.709643368666772467 ) ) ;
#140048 = CARTESIAN_POINT ( 'NONE',  ( 6.685540632719009224, -0.7820230359689305244, 1.665195522482863399 ) ) ;
#140049 = CARTESIAN_POINT ( 'NONE',  ( 3.914918041407587257, 1.633027907263858491, -1.630791690553441420 ) ) ;
#140050 = CARTESIAN_POINT ( 'NONE',  ( 6.066347387471824781, 6.042103138330730872, -0.7998128361456481317 ) ) ;
#140051 = CARTESIAN_POINT ( 'NONE',  ( 0.6849272659917711170, -0.2494827685093256309, -2.045528899044207982 ) ) ;
#140052 = CARTESIAN_POINT ( 'NONE',  ( 5.412729640353754590, 7.337937218544611895, 1.599625672291267398 ) ) ;
#140053 = ADVANCED_FACE ( 'NONE', ( #179136 ), #145631, .T. ) ;
#140054 = EDGE_CURVE ( 'NONE', #107579, #92970, #155450, .T. ) ;
#140055 = CARTESIAN_POINT ( 'NONE',  ( 6.274848118712046841, -2.282167594539401101, 0.2721878479114477334 ) ) ;
#140056 = CARTESIAN_POINT ( 'NONE',  ( 3.028993686180013079, 2.741750000184217217, 2.499999999999997335 ) ) ;
#140058 = AXIS2_PLACEMENT_3D ( 'NONE', #143717, #127513, #45127 ) ;
#140057 = CARTESIAN_POINT ( 'NONE',  ( -6.668631453075260396, 8.873432343378178544, -1.599625672291271394 ) ) ;
#140059 = CARTESIAN_POINT ( 'NONE',  ( 5.418772907935071714, 1.728844841293469159, 0.7149302089985640762 ) ) ;
#140060 = VECTOR ( 'NONE', #130123, 1000.000000000000000 ) ;
#140062 = CARTESIAN_POINT ( 'NONE',  ( -3.688700311369816909, 6.461178242310183784, -1.199719254218450271 ) ) ;
#140061 = CARTESIAN_POINT ( 'NONE',  ( 3.146637304467227558, 1.866760668956708447, 0.4145885930168375921 ) ) ;
#140063 = CARTESIAN_POINT ( 'NONE',  ( 5.233140740401229785, 0.1595256157847015632, 2.201181388321731269 ) ) ;
#140064 = CARTESIAN_POINT ( 'NONE',  ( 4.505136581001433882, -0.1005046246093168893, 2.115047560132724325 ) ) ;
#140065 = CARTESIAN_POINT ( 'NONE',  ( -0.6125000000000296874, 1.020833334016133076, -1.060881119635955327 ) ) ;
#140066 = CARTESIAN_POINT ( 'NONE',  ( 6.983263157960366563, 2.056882910316945701, 2.252511522010155698 ) ) ;
#140067 = CARTESIAN_POINT ( 'NONE',  ( 6.672020991256494504, 6.956648375986938859, 0.000000000000000000 ) ) ;
#140068 = CARTESIAN_POINT ( 'NONE',  ( -5.939880696118548187, 6.102484698325975288, 0.000000000000000000 ) ) ;
#140069 = CARTESIAN_POINT ( 'NONE',  ( 1.888135564707097425, 1.592107727680527329, 1.670599446388189913 ) ) ;
#140070 = CARTESIAN_POINT ( 'NONE',  ( 3.877359892829432386, -0.1466975079335990917, 1.956454564409334296 ) ) ;
#140071 = CARTESIAN_POINT ( 'NONE',  ( -4.339491684825780737, 7.220434844675483355, -1.199719254218455378 ) ) ;
#140072 = CARTESIAN_POINT ( 'NONE',  ( 6.280145880020024052, -1.141028152120068917, -1.718028578259041872 ) ) ;
#140073 = CARTESIAN_POINT ( 'NONE',  ( 2.575685996916329046, 5.948791396470269888, 0.7216878364870438212 ) ) ;
#140074 = CARTESIAN_POINT ( 'NONE',  ( 3.217027588192558074, 6.975225629525113824, -1.734723475976807094E-15 ) ) ;
#140075 = ORIENTED_EDGE ( 'NONE', *, *, #132078, .T. ) ;
#140076 = CARTESIAN_POINT ( 'NONE',  ( 5.296111364736042937, -0.9110065213352031011, -1.799124599017036585 ) ) ;
#140077 = CARTESIAN_POINT ( 'NONE',  ( -7.648771216403934758, 12.07531685244661723, -0.7998128361456291469 ) ) ;
#140079 = CARTESIAN_POINT ( 'NONE',  ( -10.17567228521069467, -0.02076350362892331880, -2.420000000000000373 ) ) ;
#140078 = VECTOR ( 'NONE', #202826, 1000.000000000000000 ) ;
#140080 = CARTESIAN_POINT ( 'NONE',  ( -10.52284959769361805, 5.420271152154175986, 5.071911021504272199 ) ) ;
#140081 = CARTESIAN_POINT ( 'NONE',  ( 1.587047119190465594, 2.091647000433814352, 0.5815059253076891865 ) ) ;
#140082 = DIRECTION ( 'NONE',  ( 0.000000000000000000, 0.000000000000000000, 1.000000000000000000 ) ) ;
#140083 = CARTESIAN_POINT ( 'NONE',  ( -0.7500000000000215383, 0.7229166673494852313, 1.299038105676659116 ) ) ;
#140084 = CARTESIAN_POINT ( 'NONE',  ( -9.367496997694898297, 14.53091781612142697, -7.499999999878477652 ) ) ;
#140085 = CARTESIAN_POINT ( 'NONE',  ( 6.044612043767858545, 7.151903759757407109, 1.166429756139725660 ) ) ;
#140086 = CARTESIAN_POINT ( 'NONE',  ( 1.106794710556399997, 1.562239816646590285, -1.344093658231941824 ) ) ;
#140088 = CARTESIAN_POINT ( 'NONE',  ( 4.350813900535696277, 4.000456626940672500, 0.2320863031703649382 ) ) ;
#140087 = CARTESIAN_POINT ( 'NONE',  ( -0.02244404828160086532, 2.859736408857795009, -2.677210243787793598 ) ) ;
#140089 = CARTESIAN_POINT ( 'NONE',  ( -1.364683531250014514, 0.2385416670080863499, -0.7879004041258359514 ) ) ;
#140090 = CARTESIAN_POINT ( 'NONE',  ( -1.355377658251182726, 3.766337118550212359, 0.6426130056881884656 ) ) ;
#140091 = VERTEX_POINT ( 'NONE', #73110 ) ;
#140092 = CARTESIAN_POINT ( 'NONE',  ( 3.861887077619485797, 0.6414691495152945455, -1.801623935260010079 ) ) ;
#140093 = CARTESIAN_POINT ( 'NONE',  ( 5.330810035471644781, 0.1327828994084866154, 1.764904742964703122 ) ) ;
#140094 = CARTESIAN_POINT ( 'NONE',  ( 6.496291879603339758, 7.608037276739255006, 1.199719254218452935 ) ) ;
#140095 = CARTESIAN_POINT ( 'NONE',  ( -4.172158584703340445, 5.890604320285754980, -1.599625672291256295 ) ) ;
#140097 = CARTESIAN_POINT ( 'NONE',  ( -0.04785004733596533166, -1.249461711056678803, 1.452303129844798590 ) ) ;
#140096 = CARTESIAN_POINT ( 'NONE',  ( -0.2497763946155639181, 6.515865096501928910, -3.141954037565825253 ) ) ;
#140098 = CARTESIAN_POINT ( 'NONE',  ( -0.7500000000000006661, 0.1083333333333560966, -1.299038105676652011 ) ) ;
#140099 = CARTESIAN_POINT ( 'NONE',  ( 0.3267351109269465148, -1.353470794461093973, 1.566751113397255812 ) ) ;
#140100 = CARTESIAN_POINT ( 'NONE',  ( 1.364683531249986537, -0.5322916663252452718, -0.7879004041258309554 ) ) ;
#140101 = CARTESIAN_POINT ( 'NONE',  ( 5.664887262500884368, -1.691755685069219695, -0.7986314380193232365 ) ) ;
#140102 = CARTESIAN_POINT ( 'NONE',  ( 3.246530741642670304, 0.4443377543969920795, 1.770662692542070538 ) ) ;
#140104 = CARTESIAN_POINT ( 'NONE',  ( 6.244837129360077732, 6.910362811036335096, 0.8058565020967979331 ) ) ;
#140103 = CARTESIAN_POINT ( 'NONE',  ( 5.971336403843030105, 0.1662174427981797931, -2.200672837095698497 ) ) ;
#140105 = CARTESIAN_POINT ( 'NONE',  ( -1.402160292154681736E-14, 0.9468750003414176941, -1.575800808251659024 ) ) ;
#140106 = CARTESIAN_POINT ( 'NONE',  ( 3.314939881033797331, -1.563807569242671613, 1.345168064507019423 ) ) ;
#140107 = CARTESIAN_POINT ( 'NONE',  ( -7.389357414647957256, 8.579670724299436557, 1.199719254218450271 ) ) ;
#140108 = CARTESIAN_POINT ( 'NONE',  ( 8.432281472695482449, 11.92507992053172572, 1.199719254218450271 ) ) ;
#140109 = CARTESIAN_POINT ( 'NONE',  ( 4.059776932288224671, 6.823824623389866950, 1.199719254218462483 ) ) ;
#140111 = CARTESIAN_POINT ( 'NONE',  ( 0.2280961430754513408, -1.329988288769240024, -1.704746276402234528 ) ) ;
#140110 = PRESENTATION_LAYER_ASSIGNMENT (  '', '', ( #64005 ) ) ;
#140112 = CARTESIAN_POINT ( 'NONE',  ( 5.740704066448026666, -2.019076491677873619, -0.4572469816465085657 ) ) ;
#140113 = CARTESIAN_POINT ( 'NONE',  ( 1.364683531249986537, -0.5322916663252452718, -0.7879004041258309554 ) ) ;
#140114 = CARTESIAN_POINT ( 'NONE',  ( 3.479894426560462328, 1.368377867093536482, 1.673357603396708360 ) ) ;
#140115 = CARTESIAN_POINT ( 'NONE',  ( -5.012700657095048307, 7.921469694614043711, 1.075264880722737182 ) ) ;
#140117 = CARTESIAN_POINT ( 'NONE',  ( 1.855835942623608181, -0.6640040153468586004, 1.846199708051485811 ) ) ;
#140116 = CARTESIAN_POINT ( 'NONE',  ( 4.494788958170754078, -1.959534436568559190, -0.4887017053271830447 ) ) ;
#140118 = CARTESIAN_POINT ( 'NONE',  ( 6.620655732516668834, 7.629137130509086262, 2.873739711112702544 ) ) ;
#140119 = STYLED_ITEM ( 'NONE', ( #213143 ), #136503 ) ;
#140120 = ADVANCED_FACE ( 'NONE', ( #205241 ), #90466, .T. ) ;
#140123 = CARTESIAN_POINT ( 'NONE',  ( 5.829642864196157070, 8.784705193995428374, 1.082531754730558626 ) ) ;
#140122 = CARTESIAN_POINT ( 'NONE',  ( -3.475000000000000533, -0.3499999999999996447, 0.000000000000000000 ) ) ;
#140121 = CARTESIAN_POINT ( 'NONE',  ( -0.3282377607281349308, 1.448664549684643310, -1.225000000000014522 ) ) ;
#140124 = CARTESIAN_POINT ( 'NONE',  ( -5.759181390754928742, 9.941071732514568993, 0.000000000000000000 ) ) ;
#140125 = CARTESIAN_POINT ( 'NONE',  ( 1.938685741270998797, -1.555697844595272716, 1.282991390469834458 ) ) ;
#140127 = CARTESIAN_POINT ( 'NONE',  ( -11.00029519899100450, -5.907420853759283830, 6.708500942254059474E-15 ) ) ;
#140126 = CARTESIAN_POINT ( 'NONE',  ( -4.717347382551060342, 7.590990148696470818, 1.199719254218464037 ) ) ;
#140128 = CARTESIAN_POINT ( 'NONE',  ( 3.929058411375439874, 5.499999999999998224, -0.7500000000000006661 ) ) ;
#140129 = CARTESIAN_POINT ( 'NONE',  ( 6.047114369478562956, 0.1942372860762129894, 1.902532258075719351 ) ) ;
#140130 = CARTESIAN_POINT ( 'NONE',  ( -4.288456660624211381, 3.897620947016656956, 1.214306433183764966E-14 ) ) ;
#140131 = CARTESIAN_POINT ( 'NONE',  ( 5.463572716182829581, 6.436884926043849653, 1.082531754730560403 ) ) ;
#140133 = CARTESIAN_POINT ( 'NONE',  ( 3.638296137631126914, 0.7283958097016438593, 1.880429543521966007 ) ) ;
#140132 = CARTESIAN_POINT ( 'NONE',  ( -6.846504384776750385, 10.93141284897413890, -0.7216878364870267237 ) ) ;
#140134 = CARTESIAN_POINT ( 'NONE',  ( -1.500000000000013101, 3.629166666666692187, -0.8660254037844313801 ) ) ;
#140135 = CARTESIAN_POINT ( 'NONE',  ( -1.364683531250014514, 14.65104166700806410, -0.7879004041258335089 ) ) ;
#140136 = CARTESIAN_POINT ( 'NONE',  ( 5.913083851878619512, 1.523424462977729599, 0.8087443918367646090 ) ) ;
#140137 = CARTESIAN_POINT ( 'NONE',  ( 5.691390622686558487, 9.861982503101517139, 0.7998128361456341429 ) ) ;
#140138 = CARTESIAN_POINT ( 'NONE',  ( 7.931156674314368438, 12.19684052010138586, 1.040834085586084257E-14 ) ) ;
#140139 = CARTESIAN_POINT ( 'NONE',  ( -11.41381675112453209, 10.90000000000000036, -3.704697986577182078 ) ) ;
#140140 = CARTESIAN_POINT ( 'NONE',  ( 4.815616550699190590, -1.834762568278673900, 0.3632225495420540184 ) ) ;
#140141 = ADVANCED_FACE ( 'NONE', ( #124113 ), #59015, .F. ) ;
#140142 = CARTESIAN_POINT ( 'NONE',  ( -5.608664280835665927, 5.616119181489428236, -0.4078810573515170845 ) ) ;
#140143 = CARTESIAN_POINT ( 'NONE',  ( 1.973570569994816060, -0.2575147360633044391, 2.054139978358980656 ) ) ;
#140144 = CARTESIAN_POINT ( 'NONE',  ( 0.7500000000000006661, 12.44791666734946389, -1.299038105676657340 ) ) ;
#140145 = EDGE_LOOP ( 'NONE', ( #22005, #148785, #94407, #50920 ) ) ;
#140146 = CARTESIAN_POINT ( 'NONE',  ( 3.607351389687783794, 6.366271167014519783, 1.199719254218451159 ) ) ;
#140147 = CARTESIAN_POINT ( 'NONE',  ( -0.1058464554703278104, -0.8645191204341062807, -1.819937883007181512 ) ) ;
#140148 = CARTESIAN_POINT ( 'NONE',  ( 0.8085208021518180965, -0.4412475195509023562, -1.756857618417038358 ) ) ;
#140149 = CARTESIAN_POINT ( 'NONE',  ( 4.706088717274895750, 6.583799151611112954, 1.443375672974065660 ) ) ;
#140150 = CYLINDRICAL_SURFACE ( 'NONE', #3835, 0.08000000000000012657 ) ;
#140151 = ORIENTED_EDGE ( 'NONE', *, *, #181542, .T. ) ;
#140152 = CARTESIAN_POINT ( 'NONE',  ( 8.581948047326003248, 9.114620264742901767, -0.7216878364870197293 ) ) ;
#140153 = CARTESIAN_POINT ( 'NONE',  ( 7.456094412511537151, 10.78619501698377370, 1.199719254218460707 ) ) ;
#140154 = CLOSED_SHELL ( 'NONE', ( #114959, #7847, #54872, #178428, #138429, #113040, #36985, #8539 ) ) ;
#140155 = CARTESIAN_POINT ( 'NONE',  ( 6.116788041597909675, 0.1929307199614685164, 1.905880049602140636 ) ) ;
#140156 = CARTESIAN_POINT ( 'NONE',  ( -11.48243876534946040, 13.79999999999998295, 3.199999999999997957 ) ) ;
#140157 = CARTESIAN_POINT ( 'NONE',  ( -6.492003545397249553, 6.763960095814848472, -0.1687977717132038147 ) ) ;
#140158 = FACE_OUTER_BOUND ( 'NONE', #86213, .T. ) ;
#140160 = ORIENTED_EDGE ( 'NONE', *, *, #93332, .F. ) ;
#140159 = CARTESIAN_POINT ( 'NONE',  ( 3.538314903486612817, 7.071858454135611538, 1.040834085586084257E-14 ) ) ;
#140161 = ADVANCED_FACE ( 'NONE', ( #91545 ), #208447, .F. ) ;
#140162 = CARTESIAN_POINT ( 'NONE',  ( -9.029367117021344313, 9.636609179387466639, 0.7216878364870438212 ) ) ;
#140163 = CARTESIAN_POINT ( 'NONE',  ( 3.432649856329002880, 2.108609624295390006, 0.4754391814798044069 ) ) ;
#140164 = CARTESIAN_POINT ( 'NONE',  ( -7.458393901293492334, 7.874083437696761223, 0.7216878364870317197 ) ) ;
#140165 = CARTESIAN_POINT ( 'NONE',  ( 3.553118775233146120, 6.302999783484076524, -1.199719254218453823 ) ) ;
#140166 = CARTESIAN_POINT ( 'NONE',  ( -3.789667630219657912, 4.380032642466370696, 1.199719254218462483 ) ) ;
#140167 = ADVANCED_FACE ( 'NONE', ( #60080 ), #175987, .F. ) ;
#140168 = CARTESIAN_POINT ( 'NONE',  ( 5.332948099851452461, 0.1360325894329272867, 1.820554394434070744 ) ) ;
#140169 = CARTESIAN_POINT ( 'NONE',  ( 9.873106300043385630, 9.984546488800495112, -6.331846131734216065 ) ) ;
#140170 = CARTESIAN_POINT ( 'NONE',  ( 0.9132762689940625567, -0.2936195204277583515, 1.949272377766637643 ) ) ;
#140171 = CARTESIAN_POINT ( 'NONE',  ( 3.673993457511487204, 1.897360377298975553, -0.2389773157873422427 ) ) ;
#140172 = ORIENTED_EDGE ( 'NONE', *, *, #118661, .T. ) ;
#140173 = CARTESIAN_POINT ( 'NONE',  ( -11.33772463945043540, 10.19999999999999041, -3.600000000000078693 ) ) ;
#140174 = CARTESIAN_POINT ( 'NONE',  ( 5.195741393986025969, -1.391442517743620710, -1.394189886649561227 ) ) ;
#140175 = ORIENTED_EDGE ( 'NONE', *, *, #124443, .T. ) ;
#140176 = CARTESIAN_POINT ( 'NONE',  ( 0.3396542298245264213, 1.936664667523413152, 0.1439508268369827926 ) ) ;
#140177 = ORIENTED_EDGE ( 'NONE', *, *, #34340, .T. ) ;
#140178 = CARTESIAN_POINT ( 'NONE',  ( -6.445975688654487001, 6.485002823043819475, -0.7998128361456362523 ) ) ;
#140180 = CARTESIAN_POINT ( 'NONE',  ( 6.047156637250688860, 0.2094617991648151656, 2.110256208591613003 ) ) ;
#140179 = CARTESIAN_POINT ( 'NONE',  ( -4.098307573080856692, 8.003385611894792362, 0.7998128361456352531 ) ) ;
#140182 = AXIS2_PLACEMENT_3D ( 'NONE', #86797, #152863, #187487 ) ;
#140181 = CARTESIAN_POINT ( 'NONE',  ( 6.414416072596830887, 8.576847732820027659, -1.443375672974078761 ) ) ;
#140184 = ORIENTED_EDGE ( 'NONE', *, *, #23869, .F. ) ;
#140183 = CARTESIAN_POINT ( 'NONE',  ( 3.686107007616833631, 1.064666855108999721, 1.588282736317746302 ) ) ;
#140185 = CARTESIAN_POINT ( 'NONE',  ( 0.5697015142280477118, 0.2141057807664331902, -2.196374807094509496 ) ) ;
#140186 = CARTESIAN_POINT ( 'NONE',  ( 7.717216217110708598, -5.600320323339623485, 7.761717428875256175 ) ) ;
#140187 = CARTESIAN_POINT ( 'NONE',  ( 6.633470333208185465, -0.1360683555875797923, 1.981904614263108266 ) ) ;
#140188 = DIRECTION ( 'NONE',  ( 0.000000000000000000, -1.000000000000000000, 0.000000000000000000 ) ) ;
#140190 = CARTESIAN_POINT ( 'NONE',  ( 5.612517632836664383, 1.944729323200470095, 0.5331731267440716904 ) ) ;
#140189 = CARTESIAN_POINT ( 'NONE',  ( 6.721331454403435934, -0.1262074967819451221, 1.796610827203233063 ) ) ;
#140191 = CARTESIAN_POINT ( 'NONE',  ( 1.768117254402020277, -2.054967671486531255, 0.2513356459030794410 ) ) ;
#140192 = CARTESIAN_POINT ( 'NONE',  ( -6.521635583373313061, 7.567328587812373719, -1.199719254218446718 ) ) ;
#140193 = CARTESIAN_POINT ( 'NONE',  ( -6.171773824192762881, 6.975641918443353795, -0.9092550976456583722 ) ) ;
#140194 = LINE ( 'NONE', #109871, #32725 ) ;
#140195 = CARTESIAN_POINT ( 'NONE',  ( 4.852928918687680948, 7.749168607522574526, 1.199719254218462483 ) ) ;
#140196 = FACE_OUTER_BOUND ( 'NONE', #116462, .T. ) ;
#140197 = CARTESIAN_POINT ( 'NONE',  ( 4.258669648468278446, 7.022179452304728287, 1.082531754730549078 ) ) ;
#140198 = ADVANCED_FACE ( 'NONE', ( #9199 ), #160792, .F. ) ;
#140199 = CARTESIAN_POINT ( 'NONE',  ( 0.09872732973948897262, -6.896119493545150192, 9.497255425109711879 ) ) ;
#140200 = DIRECTION ( 'NONE',  ( -0.000000000000000000, -1.000000000000000000, -0.000000000000000000 ) ) ;
#140201 = CARTESIAN_POINT ( 'NONE',  ( -0.6823417656250039265, 11.63020833367473017, -1.181850606188755259 ) ) ;
#140203 = CARTESIAN_POINT ( 'NONE',  ( -5.596483547390937119, 9.751257581923240991, 0.000000000000000000 ) ) ;
#140202 = CARTESIAN_POINT ( 'NONE',  ( 6.825078400183544503, 2.075476428726834577, 2.163873318353096931 ) ) ;
#140205 = CARTESIAN_POINT ( 'NONE',  ( 4.711369565069784215, 1.661324788532690500, 0.4972849887868810437 ) ) ;
#140204 = AXIS2_PLACEMENT_3D ( 'NONE', #186845, #102402, #103475 ) ;
#140206 = ADVANCED_FACE ( 'NONE', ( #12384 ), #206090, .F. ) ;
#140207 = CARTESIAN_POINT ( 'NONE',  ( -4.060830702492950195, 4.696389560118578999, -1.199719254218452047 ) ) ;
#140208 = CARTESIAN_POINT ( 'NONE',  ( 2.061466481998303735, 1.718891244229248105, 1.153550331455879707 ) ) ;
#140209 = CARTESIAN_POINT ( 'NONE',  ( 3.673546786387419605, 1.535089753090538078, 1.458380203637131833 ) ) ;
#140210 = TOROIDAL_SURFACE ( 'NONE', #50348, 10.92000000000000171, 0.08000000000000000167 ) ;
#140211 = CARTESIAN_POINT ( 'NONE',  ( 6.103141704446003679, 10.27208242182903142, 0.7998128361456462443 ) ) ;
#140212 = CARTESIAN_POINT ( 'NONE',  ( 1.607015867998825343, 0.9165151389911689872, 1.199999999999999734 ) ) ;
#140213 = CARTESIAN_POINT ( 'NONE',  ( 1.270285106180467416, -0.8805531663822261379, -1.761673308874162069 ) ) ;
#140214 = CARTESIAN_POINT ( 'NONE',  ( 5.447554933476544292, 6.459834866240243834, 1.284201090641323040 ) ) ;
#140216 = CARTESIAN_POINT ( 'NONE',  ( 11.86239285000045740, 12.22000000000000064, -1.812080536912752837 ) ) ;
#140215 = CARTESIAN_POINT ( 'NONE',  ( 3.475000000000000533, -1.195833333333332194, -2.006292185433951047 ) ) ;
#140217 = CARTESIAN_POINT ( 'NONE',  ( 3.398623556838876514, 1.807253594820698250, -1.409964679536945598 ) ) ;
#140218 = CARTESIAN_POINT ( 'NONE',  ( 1.681982107312831154, -0.9779208310041755947, 1.541497997293653555 ) ) ;
#140219 = CARTESIAN_POINT ( 'NONE',  ( 4.369470645354133431, 8.319742529546998000, 0.7998128361456271485 ) ) ;
#140220 = CARTESIAN_POINT ( 'NONE',  ( 7.605760987142057061, 7.975735361194951523, -0.7216878364870267237 ) ) ;
#140221 = CARTESIAN_POINT ( 'NONE',  ( -6.659026002606323047, 10.92061410301605662, 0.000000000000000000 ) ) ;
#140222 = CARTESIAN_POINT ( 'NONE',  ( 2.549090200060105893, 0.2507624435445845457, 1.997490752340509879 ) ) ;
#140223 = CARTESIAN_POINT ( 'NONE',  ( 3.151168776707893748, 1.684956273983062580, -1.004420888743910334 ) ) ;
#140224 = CARTESIAN_POINT ( 'NONE',  ( -7.700141177557535244, 11.07091624287075859, -1.199719254218446718 ) ) ;
#140225 = CARTESIAN_POINT ( 'NONE',  ( -5.930802130974132780, 9.006687355190106103, -1.199719254218440723 ) ) ;
#140226 = DIRECTION ( 'NONE',  ( 0.000000000000000000, 0.000000000000000000, -1.000000000000000000 ) ) ;
#140228 = CARTESIAN_POINT ( 'NONE',  ( 4.979261681649114202, 1.650653357529890730, -0.6390028274257038010 ) ) ;
#140227 = CARTESIAN_POINT ( 'NONE',  ( 6.544877668737552945, -1.678188448499055685, -1.246566921223101865 ) ) ;
#140229 = CARTESIAN_POINT ( 'NONE',  ( 4.899944684240791659, 4.860301720779024670, 0.6505774570350670860 ) ) ;
#140230 = CARTESIAN_POINT ( 'NONE',  ( 1.025618320672251560, -1.392776288830662512, -1.691927514038966907 ) ) ;
#140231 = CARTESIAN_POINT ( 'NONE',  ( 5.999919492459485859, -0.6329648550039753685, -1.621342527780894827 ) ) ;
#140232 = CARTESIAN_POINT ( 'NONE',  ( 6.889514614038635187, 11.18951748302043114, -0.7998128361456291469 ) ) ;
#140233 = CARTESIAN_POINT ( 'NONE',  ( 0.1333692844072559280, 0.001398348041498076455, -2.053671342968105051 ) ) ;
#140234 = CARTESIAN_POINT ( 'NONE',  ( 6.539654151966706408, -1.780142272834178918, 1.453760081647121671 ) ) ;
#140235 = CARTESIAN_POINT ( 'NONE',  ( 2.547265342226494947E-16, 1.016439536705160407E-16, -2.080000000000000071 ) ) ;
#140236 = CARTESIAN_POINT ( 'NONE',  ( 5.887993837006205489, -0.03927123031851989521, 1.733586367271770179 ) ) ;
#140237 = CARTESIAN_POINT ( 'NONE',  ( 5.336453890206420247, -1.210535830701382709, 1.802210774359000567 ) ) ;
#140238 = CARTESIAN_POINT ( 'NONE',  ( 3.195971524519376494, 4.751719416737803847, -1.599625672291262513 ) ) ;
#140239 = CARTESIAN_POINT ( 'NONE',  ( 0.04044418650436896329, 0.8167838292495681607, 1.953657075893009853 ) ) ;
#140241 = VECTOR ( 'NONE', #104166, 1000.000000000000000 ) ;
#140240 = CARTESIAN_POINT ( 'NONE',  ( 2.843750000000001332, 1.895863743164146298, 0.7852924748298368840 ) ) ;
#140242 = CARTESIAN_POINT ( 'NONE',  ( 3.719872605471085336, 6.605953636083950364, 2.499999999999999556 ) ) ;
#140243 = CARTESIAN_POINT ( 'NONE',  ( 3.997031241255116552, 1.627850364849007248, -1.029807644849835890 ) ) ;
#140244 = CARTESIAN_POINT ( 'NONE',  ( -0.7500000000000179856, 11.57291666734946212, 1.299038105676658228 ) ) ;
#140245 = CARTESIAN_POINT ( 'NONE',  ( 1.752877424878969803, 2.197725149470313166, 0.3219655503990859757 ) ) ;
#140246 = ORIENTED_EDGE ( 'NONE', *, *, #127807, .T. ) ;
#140247 = CARTESIAN_POINT ( 'NONE',  ( -1.201851678989727383E-14, 4.587500000000025224, -1.732050807568863648 ) ) ;
#140248 = CARTESIAN_POINT ( 'NONE',  ( 4.792970997630896512, 5.550553237779539018, 1.199719254218464037 ) ) ;
#140249 = CARTESIAN_POINT ( 'NONE',  ( 6.144869935491714230, 8.192100896205568361, -1.599625672291262513 ) ) ;
#140250 = CARTESIAN_POINT ( 'NONE',  ( 2.912952216767932256, -0.6468334258018549887, -2.125021405654815787 ) ) ;
#140251 = CARTESIAN_POINT ( 'NONE',  ( -8.188761592974046266, 10.57664116326830595, -1.443375672974059665 ) ) ;
#140252 = CARTESIAN_POINT ( 'NONE',  ( 4.386855106046934516, 4.010796903234440158, -0.04314253085381029862 ) ) ;
#140253 = CARTESIAN_POINT ( 'NONE',  ( 6.317736394288135493, 8.393778431468064127, 1.443375672974076540 ) ) ;
#140254 = CARTESIAN_POINT ( 'NONE',  ( -7.822691444960696572, 12.07029775252209092, -0.7216878364870267237 ) ) ;
#140255 = CARTESIAN_POINT ( 'NONE',  ( 5.831415467653547680, 8.857049574687536619, -1.082531754730548412 ) ) ;
#140256 = CIRCLE ( 'NONE', #188773, 11.92000000000000171 ) ;
#140257 = CARTESIAN_POINT ( 'NONE',  ( 0.9850002542920628379, -2.016597020373378513, 0.002813405579435435122 ) ) ;
#140259 = CARTESIAN_POINT ( 'NONE',  ( 6.637180544258393766, -0.09741176211745629365, -2.060485520500746848 ) ) ;
#140258 = CARTESIAN_POINT ( 'NONE',  ( 7.553864141108259211, 11.96459193126834464, 1.040834085586084257E-14 ) ) ;
#140260 = CARTESIAN_POINT ( 'NONE',  ( -11.44789321844504215, 11.29999999999998295, 3.303298730975396946 ) ) ;
#140261 = CARTESIAN_POINT ( 'NONE',  ( 6.278834536460164983, 9.379038488295265097, -1.082531754730548412 ) ) ;
#140262 = CARTESIAN_POINT ( 'NONE',  ( 6.146048976554097543, 0.5551056870855082259, 1.649627438850902017 ) ) ;
#140263 = CYLINDRICAL_SURFACE ( 'NONE', #64563, 3.475000000000000089 ) ;
#140264 = CARTESIAN_POINT ( 'NONE',  ( -1.364683531250000748, 1.759375000341421913, 0.000000000000000000 ) ) ;
#140265 = CARTESIAN_POINT ( 'NONE',  ( 0.9656335942268097217, 0.8653965441102560163, 1.543625204253181948 ) ) ;
#140266 = CARTESIAN_POINT ( 'NONE',  ( 6.539718741795587320, -1.333554142906383744, 1.108523769342983689 ) ) ;
#140267 = CARTESIAN_POINT ( 'NONE',  ( -0.1296875068448159751, 0.001480089298542403009, -1.826395826379861864 ) ) ;
#140268 = CARTESIAN_POINT ( 'NONE',  ( 3.896227223837216869, -0.7194467914123764407, -2.176594258899899437 ) ) ;
#140269 = CARTESIAN_POINT ( 'NONE',  ( -1.364683531250014514, 0.03020833367475737191, 0.7879004041258379498 ) ) ;
#140270 = CARTESIAN_POINT ( 'NONE',  ( 2.659893383946440260, -1.269561761542839617, 1.333649727802692198 ) ) ;
#140271 = CIRCLE ( 'NONE', #84880, 0.07999999999999998779 ) ;
#140272 = CARTESIAN_POINT ( 'NONE',  ( 8.452618703115982512, 11.94880668935564216, 1.199719254218450271 ) ) ;
#140273 = CARTESIAN_POINT ( 'NONE',  ( 0.000000000000000000, 15.00000000000000000, 0.000000000000000000 ) ) ;
#140274 = CARTESIAN_POINT ( 'NONE',  ( 3.135583521505393545, -1.224952879796761041, -1.353777129306121818 ) ) ;
#140275 = CARTESIAN_POINT ( 'NONE',  ( 3.938125092175647879, -1.678004675797317713, -1.117833462672225497 ) ) ;
#140276 = CARTESIAN_POINT ( 'NONE',  ( -8.967828540435322182, 12.54988483289483980, 1.199719254218462483 ) ) ;
#140278 = CARTESIAN_POINT ( 'NONE',  ( -11.41381675112460847, 12.56983264508524201, -3.704697986577268232 ) ) ;
#140277 = CARTESIAN_POINT ( 'NONE',  ( 3.133911187764222728, -1.518274094020392706, -1.677614996870570918 ) ) ;
#140279 = CARTESIAN_POINT ( 'NONE',  ( 5.702208657235168232, -2.106147099624333219, -0.003344702849475410765 ) ) ;
#140280 = CARTESIAN_POINT ( 'NONE',  ( -1.906201616980850222, 3.231688558335370054, -0.4612787108932971392 ) ) ;
#140281 = CARTESIAN_POINT ( 'NONE',  ( 2.664580169416390643, -0.7900844611210651180, -1.913877855911281234 ) ) ;
#140282 = CARTESIAN_POINT ( 'NONE',  ( 4.273844736805816780, 6.009238164405336313, 1.599625672291267398 ) ) ;
#140283 = CARTESIAN_POINT ( 'NONE',  ( -1.360316468750032204, 0.6718750003414097893, -2.081668171172168513E-14 ) ) ;
#140284 = CARTESIAN_POINT ( 'NONE',  ( 5.725269513181780567, 1.870077439114096629, 0.9995941271150191598 ) ) ;
#140285 = CONTEXT_DEPENDENT_SHAPE_REPRESENTATION ( #107361, #163104 ) ;
#140287 = CARTESIAN_POINT ( 'NONE',  ( 0.9262474005801927257, 1.148234195015400694, -1.546785173711192840 ) ) ;
#140286 = CARTESIAN_POINT ( 'NONE',  ( -2.453662613948990323, 5.806430783008362795, -0.7216878364870257245 ) ) ;
#140288 = UNCERTAINTY_MEASURE_WITH_UNIT (LENGTH_MEASURE( 1.000000000000000082E-05 ), #112870, 'distance_accuracy_value', 'NONE');
#140289 = CARTESIAN_POINT ( 'NONE',  ( -3.305155586681401303, 7.078041627762083898, 0.7998128361456352531 ) ) ;
#140290 = CARTESIAN_POINT ( 'NONE',  ( 8.422639742587595180, 10.84949900448412130, -1.599625672291268286 ) ) ;
#140291 = CARTESIAN_POINT ( 'NONE',  ( 5.519577934094852978, 7.532869904567736974, 1.443375672974064550 ) ) ;
#140292 = CARTESIAN_POINT ( 'NONE',  ( 4.103641366189806128, 7.455328040159560743, 0.6459977421944228526 ) ) ;
#140293 = CARTESIAN_POINT ( 'NONE',  ( -1.737499999999997824, -1.647916665710749573, 3.009438278150925683 ) ) ;
#140294 = CARTESIAN_POINT ( 'NONE',  ( -3.578462479003122976, 6.262291094557191684, 1.199719254218464037 ) ) ;
#140295 = CARTESIAN_POINT ( 'NONE',  ( 0.1764466950717893667, 2.196028898142581731, -0.3343166089466164115 ) ) ;
#140296 = CARTESIAN_POINT ( 'NONE',  ( 1.799976324648028481, -0.7102278526811952597, 1.982709249334560164 ) ) ;
#140297 = CARTESIAN_POINT ( 'NONE',  ( -7.075376061485238566, 9.347967719856493218, 1.599625672291269396 ) ) ;
#140298 = CARTESIAN_POINT ( 'NONE',  ( 6.564118927310645724, 10.80988918183778225, -0.7998128361456291469 ) ) ;
#140299 = CARTESIAN_POINT ( 'NONE',  ( 5.875803118876519626, -1.815897848738392106, 0.4062362408630160737 ) ) ;
#140300 = CARTESIAN_POINT ( 'NONE',  ( 7.884230021546724920, 9.157022099014721306, 1.199719254218462483 ) ) ;
#140301 = FACE_OUTER_BOUND ( 'NONE', #164103, .T. ) ;
#140302 = CARTESIAN_POINT ( 'NONE',  ( -7.268579750702160780, 8.613002809641560731, -1.082531754730549967 ) ) ;
#140303 = CARTESIAN_POINT ( 'NONE',  ( -8.270110514656041190, 10.67154823856396817, 1.443375672974090751 ) ) ;
#140304 = CARTESIAN_POINT ( 'NONE',  ( -4.495411241332101682, 8.048790631822507535, 2.444653990452268832 ) ) ;
#140305 = CARTESIAN_POINT ( 'NONE',  ( -7.262327558775498737, 8.501745569106741840, 1.199719254218452047 ) ) ;
#140307 = CARTESIAN_POINT ( 'NONE',  ( 3.139059813392345077, -0.1416510307416830594, -1.956792864499560691 ) ) ;
#140306 = CARTESIAN_POINT ( 'NONE',  ( -0.6125000000000262457, -0.7916666666666349883, -1.060881119635962211 ) ) ;
#140308 = CARTESIAN_POINT ( 'NONE',  ( 2.395597313961893349, 1.670541196947441520, 1.371929806955954012 ) ) ;
#140310 = CARTESIAN_POINT ( 'NONE',  ( -5.157125652413038885, 6.495829312680758250, -1.199528311315662510 ) ) ;
#140309 = CARTESIAN_POINT ( 'NONE',  ( -5.984998465789844069, 5.947196063035064206, 0.7998128361456281477 ) ) ;
#140311 = CARTESIAN_POINT ( 'NONE',  ( 0.6823417656249882723, 1.926041667008083991, -1.181850606188749264 ) ) ;
#140312 = CARTESIAN_POINT ( 'NONE',  ( 3.767295573485733851, 0.9686143178696275946, 1.445635114442943348 ) ) ;
#140313 = CARTESIAN_POINT ( 'NONE',  ( 5.327991180490514012, 9.159814110640187579, 1.040834085586084257E-14 ) ) ;
#140314 = CARTESIAN_POINT ( 'NONE',  ( -11.88671056400589521, 6.998741290788587754, 4.405061004403326486 ) ) ;
#140315 = EDGE_CURVE ( 'NONE', #12932, #170920, #130799, .T. ) ;
#140316 = CARTESIAN_POINT ( 'NONE',  ( 1.968124833515383809, 1.674630251985644414, 1.122327857054454814 ) ) ;
#140317 = CARTESIAN_POINT ( 'NONE',  ( -0.09630943990284260292, -9.919512026728389387, -10.99957837791001225 ) ) ;
#140318 = CARTESIAN_POINT ( 'NONE',  ( 0.08116279290028630133, -0.1557560750096824431, -2.127278773206460638 ) ) ;
#140319 = CARTESIAN_POINT ( 'NONE',  ( 2.043765361886350274, 0.7562441204337754241, -1.820841827831324533 ) ) ;
#140322 = VERTEX_POINT ( 'NONE', #54387 ) ;
#140321 = CARTESIAN_POINT ( 'NONE',  ( -3.824808732831001201, 7.476377598362539345, 0.7216878364870338292 ) ) ;
#140320 = CARTESIAN_POINT ( 'NONE',  ( 11.01135777277262306, 10.89999999999998259, 1.399999999999998579 ) ) ;
#140323 = CARTESIAN_POINT ( 'NONE',  ( -6.916067756302494374, 7.241369601873926420, 0.000000000000000000 ) ) ;
#140324 = CARTESIAN_POINT ( 'NONE',  ( 6.737475991348287785, 6.825086509519945999, -0.7998128361456481317 ) ) ;
#140325 = CARTESIAN_POINT ( 'NONE',  ( -7.117104292530948229, 7.267986194233038155, -0.7998128361456362523 ) ) ;
#140326 = CARTESIAN_POINT ( 'NONE',  ( 2.086587641237521495, -1.240871089896943280, 1.593450946908819832 ) ) ;
#140327 = CARTESIAN_POINT ( 'NONE',  ( -9.232739420781982176, 12.75498451001223010, 1.082531754730558626 ) ) ;
#140328 = CARTESIAN_POINT ( 'NONE',  ( 5.561655955723623812, 0.4570820274143985729, -2.261718950934066275 ) ) ;
#140329 = EDGE_CURVE ( 'NONE', #75836, #140322, #188643, .T. ) ;
#140330 = CARTESIAN_POINT ( 'NONE',  ( 2.535929169054650156, 1.202975682259961765, 1.549578550289295586 ) ) ;
#140331 = CARTESIAN_POINT ( 'NONE',  ( 9.423080456697809026, 10.95234760669099749, -1.199719254218446718 ) ) ;
#140332 = CARTESIAN_POINT ( 'NONE',  ( 1.002577532868035526, -1.966644254196001196, 0.4445047019146358691 ) ) ;
#140333 = VERTEX_POINT ( 'NONE', #172407 ) ;
#140334 = CARTESIAN_POINT ( 'NONE',  ( 2.114611820864919611, 2.055121497718506163, 0.5091636546959156240 ) ) ;
#140337 = ORIENTED_EDGE ( 'NONE', *, *, #44262, .F. ) ;
#140336 = CARTESIAN_POINT ( 'NONE',  ( -5.682838942422375084, 9.781729199468104596, 0.000000000000000000 ) ) ;
#140335 = CARTESIAN_POINT ( 'NONE',  ( -4.322352044658376968, 3.937165561723182883, 0.7998128361456341429 ) ) ;
#140338 = CARTESIAN_POINT ( 'NONE',  ( 2.079791654855645877, -1.805462111169679584, -0.3597937517794968509 ) ) ;
#140339 = VERTEX_POINT ( 'NONE', #136711 ) ;
#140340 = CARTESIAN_POINT ( 'NONE',  ( -9.755255220232635693, 11.33988483081495957, -1.199719254218441611 ) ) ;
#140341 = CARTESIAN_POINT ( 'NONE',  ( 9.472186069782596363, 13.10071810221855593, 7.368474063948833752 ) ) ;
#140342 = CARTESIAN_POINT ( 'NONE',  ( 3.058948843759463188, 0.5191580478346514704, 2.055925682384197373 ) ) ;
#140343 = CARTESIAN_POINT ( 'NONE',  ( 6.632770897174698810, -1.733374817101345000, 0.8757406700844807546 ) ) ;
#140344 = CARTESIAN_POINT ( 'NONE',  ( -1.201851678989727383E-14, 5.118750000682815937, -1.732050807568863648 ) ) ;
#140345 = CARTESIAN_POINT ( 'NONE',  ( 6.751070424600909448, 9.963667031088037973, -1.199719254218441611 ) ) ;
#140346 = CARTESIAN_POINT ( 'NONE',  ( 5.365994935958575240, 9.482354201918870018, 0.7998128361456341429 ) ) ;
#140347 = CARTESIAN_POINT ( 'NONE',  ( 4.376282966308748357, -1.189761084491423926, 1.682430632154131578 ) ) ;
#140349 = CARTESIAN_POINT ( 'NONE',  ( 0.9250624443557056154, -1.167992581197497604, -1.423340509374780405 ) ) ;
#140348 = CARTESIAN_POINT ( 'NONE',  ( -6.042130013184518589, 10.20090211535728031, -0.7998128361456291469 ) ) ;
#140350 = CARTESIAN_POINT ( 'NONE',  ( -0.6823417656249969321, 4.967708333674755394, -1.181850606188749264 ) ) ;
#140351 =( BOUNDED_CURVE ( )  B_SPLINE_CURVE ( 2, ( #5198, #55056, #71273, #188239, #170928, #169861, #139525, #37736, #205551 ),
 .UNSPECIFIED., .F., .T. ) 
 B_SPLINE_CURVE_WITH_KNOTS ( ( 3, 2, 2, 2, 3 ),
 ( 0.4196428571428570953, 0.4226190476190476164, 0.4285714285714285476, 0.4345238095238095344, 0.4375000000000000000 ),
 .UNSPECIFIED. ) 
 CURVE ( )  GEOMETRIC_REPRESENTATION_ITEM ( )  RATIONAL_B_SPLINE_CURVE ( ( 0.9330127018922194093, 0.9330127018922180770, 1.000000000000000000, 0.8660254037844387076, 1.000000000000000000, 0.8660254037844387076, 1.000000000000000000, 0.9330127018922194093, 0.9330127018922194093 ) ) 
 REPRESENTATION_ITEM ( '' )  );
#140352 = CARTESIAN_POINT ( 'NONE',  ( -9.499750697158754420, -9.920000000031521381, 0.06885943948997631792 ) ) ;
#140353 = CARTESIAN_POINT ( 'NONE',  ( 1.594636444620714633, -2.196503929104542951, -0.2137616909994101977 ) ) ;
#140354 = CARTESIAN_POINT ( 'NONE',  ( 3.427297576727184047, 0.05164501975941707818, 2.261966552586023749 ) ) ;
#140355 = CARTESIAN_POINT ( 'NONE',  ( -9.015808963407680565, 9.620791333504852716, 1.040834085586084257E-14 ) ) ;
#140356 = CARTESIAN_POINT ( 'NONE',  ( 3.990334445075129466, -1.038098595406260705, 1.484453480236499923 ) ) ;
#140357 = CARTESIAN_POINT ( 'NONE',  ( 2.694441388940031601, 1.384233754937878258, -1.324569364742228972 ) ) ;
#140358 = CARTESIAN_POINT ( 'NONE',  ( 3.754400092289136737, -2.067862582909282487, -0.1045053291982081939 ) ) ;
#140359 = CARTESIAN_POINT ( 'NONE',  ( -1.364683531250012516, 3.051041667008083547, -0.7879004041258289570 ) ) ;
#140360 = CARTESIAN_POINT ( 'NONE',  ( 2.448066223300342514, 1.970991375097268961, 0.05018580263361701460 ) ) ;
#140361 = CARTESIAN_POINT ( 'NONE',  ( 1.008667890995796457, 1.460797969510800876, -1.255919511179462322 ) ) ;
#140362 = CARTESIAN_POINT ( 'NONE',  ( 4.276139911362797363, -1.077190196239918851, 1.529178877381555335 ) ) ;
#140363 = CARTESIAN_POINT ( 'NONE',  ( 2.702171824926146826, -0.7227257407616082263, 2.191671519121952461 ) ) ;
#140364 = CARTESIAN_POINT ( 'NONE',  ( 3.842128478764065047, -0.9187925100661897826, 1.618370328034287597 ) ) ;
#140365 = CARTESIAN_POINT ( 'NONE',  ( 0.6823417656249917140, 4.092708333674755394, 1.181850606188765695 ) ) ;
#140366 = AXIS2_PLACEMENT_3D ( 'NONE', #77393, #143510, #44924 ) ;
#140367 = CARTESIAN_POINT ( 'NONE',  ( -4.680589345215810049, 6.483773540883647435, -1.599625672291256295 ) ) ;
#140368 = CARTESIAN_POINT ( 'NONE',  ( 5.262536180398716290, 9.291375977107183104, -0.7998128361456291469 ) ) ;
#140369 = CARTESIAN_POINT ( 'NONE',  ( 11.31269326259041108, 3.603011019375353730, -3.682594235848559716 ) ) ;
#140370 = CARTESIAN_POINT ( 'NONE',  ( 0.1882882188262140766, -0.9905318517600868455, 1.858590670187587612 ) ) ;
#140371 = AXIS2_PLACEMENT_3D ( 'NONE', #185533, #136812, #68572 ) ;
#140372 = CARTESIAN_POINT ( 'NONE',  ( 4.514501963226220660, 4.369266499959774563, -0.7216878364870197293 ) ) ;
#140374 = CARTESIAN_POINT ( 'NONE',  ( -7.407835137441776574, -5.166862915010159263, -8.023115266309144289 ) ) ;
#140373 = CARTESIAN_POINT ( 'NONE',  ( -1.364683531250010295, 3.842708333674751398, 0.7879004041258379498 ) ) ;
#140375 = CARTESIAN_POINT ( 'NONE',  ( 1.617596980227502756, 1.765956010477184535, 1.173731981927571555 ) ) ;
#140376 = CARTESIAN_POINT ( 'NONE',  ( 0.2990895800742687793, -0.2513629124439535345, -2.004038569727568664 ) ) ;
#140377 = CARTESIAN_POINT ( 'NONE',  ( -0.6823417656250003738, 0.2177083336747515085, -1.181850606188749264 ) ) ;
#140378 = CARTESIAN_POINT ( 'NONE',  ( -4.989037340148921196, 5.883260320670900434, 1.082531754730560403 ) ) ;
#140379 = CARTESIAN_POINT ( 'NONE',  ( 5.392392409933256303, 7.314210449720692786, 1.599625672291267398 ) ) ;
#140380 = CARTESIAN_POINT ( 'NONE',  ( 1.528841242883504981, 2.082761121880230881, 0.5781018612496248155 ) ) ;
#140381 = EDGE_CURVE ( 'NONE', #177962, #213399, #171322, .T. ) ;
#140384 = CARTESIAN_POINT ( 'NONE',  ( 3.714570900464278846, 5.356752022006865843, 1.443375672974062551 ) ) ;
#140383 = CARTESIAN_POINT ( 'NONE',  ( 6.925078400183553029, 7.052683076116534444, 2.553806833665558162 ) ) ;
#140382 = CARTESIAN_POINT ( 'NONE',  ( 6.222266154028957885, 6.224008365980749247, 0.7998128361456352531 ) ) ;
#140385 = CARTESIAN_POINT ( 'NONE',  ( -5.015590482412729756, 4.816220082428420923, 0.000000000000000000 ) ) ;
#140386 = CARTESIAN_POINT ( 'NONE',  ( 5.401577436481666439, -1.966305606708594667, 0.4464985920552416720 ) ) ;
#140388 = CARTESIAN_POINT ( 'NONE',  ( -5.600926855776882540, 8.588146194164741232, -1.082531754730549967 ) ) ;
#140387 = CARTESIAN_POINT ( 'NONE',  ( -6.724481002698115439, 10.78905223654906109, -0.7216878364870267237 ) ) ;
#140389 = TRIMMED_CURVE ( 'NONE', #76129, ( PARAMETER_VALUE ( 0.000000000000000000 ), #186838 ), ( PARAMETER_VALUE ( 0.6154797086703889253 ), #190045 ), .T., .PARAMETER. ) ;
#140390 = CARTESIAN_POINT ( 'NONE',  ( -9.345718720454827988, 14.55697459676220795, -7.452154232107646159 ) ) ;
#140392 = CARTESIAN_POINT ( 'NONE',  ( -1.402160292154681736E-14, 11.17187500034139802, 1.575800808251682339 ) ) ;
#140391 = CARTESIAN_POINT ( 'NONE',  ( 0.6028508490328026159, -0.7652319425662640340, -2.129318446015377120 ) ) ;
#140393 = CARTESIAN_POINT ( 'NONE',  ( -9.622536337397040285, 12.24937836509514710, 1.599625672291281386 ) ) ;
#140395 = CARTESIAN_POINT ( 'NONE',  ( 0.03459428079104728826, -1.538086888106354522, 1.141608027856432450 ) ) ;
#140394 = CARTESIAN_POINT ( 'NONE',  ( -6.358410854684796831, 6.520493539994793863, -0.7216878364870267237 ) ) ;
#140396 = CARTESIAN_POINT ( 'NONE',  ( 0.6823417656249882723, 0.9885416670080832136, -1.181850606188749264 ) ) ;
#140397 = DIRECTION ( 'NONE',  ( -1.000000000000000000, 7.387867266669436732E-31, -0.000000000000000000 ) ) ;
#140398 = CARTESIAN_POINT ( 'NONE',  ( -0.7500000000000179856, 8.541666666666669627, 1.299038105676658228 ) ) ;
#140399 = CARTESIAN_POINT ( 'NONE',  ( 2.349869733406087402, 1.724505987646451688, 0.04327962033413671611 ) ) ;
#140400 = CARTESIAN_POINT ( 'NONE',  ( 5.996449078994045223, 10.21788403546024782, 0.7998128361456331437 ) ) ;
#140401 = CARTESIAN_POINT ( 'NONE',  ( 4.716257332707354699, 6.595662536282280719, -1.599625672291269396 ) ) ;
#140402 = CARTESIAN_POINT ( 'NONE',  ( 1.440303513825416992, 0.3384911870211620988, 1.736878781881325384 ) ) ;
#140403 = CARTESIAN_POINT ( 'NONE',  ( 1.998691314347844417, -1.974684511280549559, -0.3905480285893418446 ) ) ;
#140404 = DIRECTION ( 'NONE',  ( -0.7071067811865462405, 0.000000000000000000, 0.7071067811865489050 ) ) ;
#140405 = CARTESIAN_POINT ( 'NONE',  ( 8.401248741962376698, 12.95320729893149370, 0.7998128361456462443 ) ) ;
#140407 = AXIS2_PLACEMENT_3D ( 'NONE', #77847, #159105, #10708 ) ;
#140406 = CARTESIAN_POINT ( 'NONE',  ( 4.594872931952145301, -0.4798491958124780910, -2.153818993410236970 ) ) ;
#140408 = ORIENTED_EDGE ( 'NONE', *, *, #21416, .T. ) ;
#140409 = CARTESIAN_POINT ( 'NONE',  ( 8.012505595552012139, 11.33137838057728786, -1.082531754730543083 ) ) ;
#140411 = CARTESIAN_POINT ( 'NONE',  ( 2.882435586221145041, -0.5880402899147362250, -1.928746874286999757 ) ) ;
#140410 = CARTESIAN_POINT ( 'NONE',  ( 4.670628115925999246, 0.8122961462209904449, 1.958930372594757330 ) ) ;
#140413 = ORIENTED_EDGE ( 'NONE', *, *, #17921, .F. ) ;
#140412 = CARTESIAN_POINT ( 'NONE',  ( 3.146531925530637430, 1.768428357263505557, 0.3923012617871086682 ) ) ;
#140414 = CARTESIAN_POINT ( 'NONE',  ( 6.235824307642648279, 6.239826211863360506, 0.000000000000000000 ) ) ;
#140415 = ORIENTED_EDGE ( 'NONE', *, *, #200871, .F. ) ;
#140416 = CARTESIAN_POINT ( 'NONE',  ( 1.656895194024514906, -1.602792776363659133, -0.9643473572949824435 ) ) ;
#140417 = CIRCLE ( 'NONE', #130110, 2.000000000000000000 ) ;
#140418 = CARTESIAN_POINT ( 'NONE',  ( 6.498675964634617941, -0.4922777150685350156, -1.758009983081544991 ) ) ;
#140421 = CARTESIAN_POINT ( 'NONE',  ( 2.061615604755413500, 1.182011660234401962, 1.507458768284040129 ) ) ;
#140420 = VECTOR ( 'NONE', #70059, 1000.000000000000114 ) ;
#140419 = CARTESIAN_POINT ( 'NONE',  ( -2.819205876637805641, 5.376491725131008259, -1.199719254218446718 ) ) ;
#140422 = CARTESIAN_POINT ( 'NONE',  ( -9.812680342707254866, 4.108039100808300148, -6.337802944732694677 ) ) ;
#140423 = CARTESIAN_POINT ( 'NONE',  ( -0.4019237886466933696, 8.832585450998172050, 1.500000000000005995 ) ) ;
#140424 = B_SPLINE_CURVE_WITH_KNOTS ( 'NONE', 3,
 ( #170358, #84847, #150937, #186609, #183412 ),
 .UNSPECIFIED., .F., .F.,
 ( 4, 1, 4 ),
 ( 0.001713136426838359665, 0.001716577612580400414, 0.001720018798322440947 ),
 .UNSPECIFIED. ) ;
#140425 = CARTESIAN_POINT ( 'NONE',  ( -1.201851678989727383E-14, 1.384375000341419693, 1.575800808251672791 ) ) ;
#140426 = CARTESIAN_POINT ( 'NONE',  ( 0.000000000000000000, 1.000000000000000888, 0.000000000000000000 ) ) ;
#140427 = ADVANCED_FACE ( 'NONE', ( #108532 ), #23995, .T. ) ;
#140428 = CARTESIAN_POINT ( 'NONE',  ( 4.786342355033275986, -0.6839347017603314427, -1.897111394664739326 ) ) ;
#140429 = CIRCLE ( 'NONE', #47028, 11.95586200173895008 ) ;
#140430 = CARTESIAN_POINT ( 'NONE',  ( 7.539742822975472158, 7.968990512992423447, -0.7216878364870317197 ) ) ;
#140431 = FACE_OUTER_BOUND ( 'NONE', #163034, .T. ) ;
#140432 = CARTESIAN_POINT ( 'NONE',  ( -5.738844160334429567, 9.917344963690652548, 0.000000000000000000 ) ) ;
#140433 = CARTESIAN_POINT ( 'NONE',  ( 4.394861267144759331, -2.057662932662501110, -0.5123870273424437904 ) ) ;
#140435 = CARTESIAN_POINT ( 'NONE',  ( -11.21884318011362147, 9.005685702144777594, -2.479759622982018463 ) ) ;
#140434 = CARTESIAN_POINT ( 'NONE',  ( -0.02968770228137587730, 6.948707269782667062, -2.421356871654921417 ) ) ;
#140437 = EDGE_CURVE ( 'NONE', #191668, #193155, #102342, .T. ) ;
#140436 = CARTESIAN_POINT ( 'NONE',  ( 3.936761750732898690, 0.2861355568666827387, 1.950351509585077858 ) ) ;
#140438 = CARTESIAN_POINT ( 'NONE',  ( -0.1052096654315381741, -1.953846233167291002, -0.4849948655165080558 ) ) ;
#140439 = ORIENTED_EDGE ( 'NONE', *, *, #81935, .F. ) ;
#140440 = CARTESIAN_POINT ( 'NONE',  ( 6.333232048763643540, -1.701881231816049000, -1.259509043995930222 ) ) ;
#140442 = EDGE_CURVE ( 'NONE', #169714, #80718, #119730, .T. ) ;
#140441 = FILL_AREA_STYLE_COLOUR ( '', #76762 ) ;
#140443 = CARTESIAN_POINT ( 'NONE',  ( 1.293514844328220281, -1.872496763586928514, 0.8835221827151735763 ) ) ;
#140444 = CARTESIAN_POINT ( 'NONE',  ( 6.964048179274811012, 8.153752959689313684, 1.199719254218452047 ) ) ;
#140445 = EDGE_LOOP ( 'NONE', ( #143637, #76985 ) ) ;
#140446 = CARTESIAN_POINT ( 'NONE',  ( 4.342354338126830804, 8.288106837781779035, -0.7998128361456381397 ) ) ;
#140447 = CARTESIAN_POINT ( 'NONE',  ( 6.176621499477501054, 9.363752961769195693, -1.199719254218452047 ) ) ;
#140449 = CARTESIAN_POINT ( 'NONE',  ( 4.469384193999260901, 8.366031992974468423, -0.7998128361456231517 ) ) ;
#140448 = CARTESIAN_POINT ( 'NONE',  ( 3.345728622622257564, 2.090823719190892049, -0.0003901280219448939298 ) ) ;
#140450 = CARTESIAN_POINT ( 'NONE',  ( 5.854088466050551887, 10.05179665369283981, 0.7998128361456341429 ) ) ;
#140453 = ORIENTED_EDGE ( 'NONE', *, *, #193237, .F. ) ;
#140452 = CARTESIAN_POINT ( 'NONE',  ( 0.2229362713279548491, 1.575107908988721883, 0.8944890650159162959 ) ) ;
#140451 = CARTESIAN_POINT ( 'NONE',  ( 1.729251940891060713, -1.720190037149814444, 0.6116943438041824166 ) ) ;
#140454 = CARTESIAN_POINT ( 'NONE',  ( 6.006501602161061548, -0.7906231143557164165, -2.060575041408031272 ) ) ;
#140455 = CARTESIAN_POINT ( 'NONE',  ( 0.000000000000000000, 7.980384757729337863, 0.000000000000000000 ) ) ;
#140456 = CARTESIAN_POINT ( 'NONE',  ( 4.717920652503574175, -2.164970738276258189, 0.4266498443898231185 ) ) ;
#140457 = CARTESIAN_POINT ( 'NONE',  ( -11.86239285000045918, 12.21999999999998288, 1.812080536912751283 ) ) ;
#140458 = CARTESIAN_POINT ( 'NONE',  ( 2.736851483355093873, 1.801321139115559244, 0.6423184003811268639 ) ) ;
#140459 = CARTESIAN_POINT ( 'NONE',  ( 9.097684769969825780, 10.57271930550834860, -1.199719254218446718 ) ) ;
#140460 = CARTESIAN_POINT ( 'NONE',  ( 5.318829906782316819, -1.502041817331278173, 1.425132596443792643 ) ) ;
#140462 = CARTESIAN_POINT ( 'NONE',  ( -1.538818179733931313, 8.696032261897956417, -2.511230101280735649 ) ) ;
#140461 = CARTESIAN_POINT ( 'NONE',  ( 1.543624195544782474, 8.695410207106890610, -2.508689898543530639 ) ) ;
#140463 = CARTESIAN_POINT ( 'NONE',  ( 5.513277522340928272, -2.138352208816508782, 0.4792397250529822905 ) ) ;
#140464 = VERTEX_POINT ( 'NONE', #40274 ) ;
#140465 = FILL_AREA_STYLE_COLOUR ( '', #100960 ) ;
#140466 = CARTESIAN_POINT ( 'NONE',  ( -0.1515253745957804432, 3.870538056096192836, 11.62858902121511839 ) ) ;
#140467 = CARTESIAN_POINT ( 'NONE',  ( 5.259637247458703868, 5.100941308315409373, 0.000000000000000000 ) ) ;
#140468 = CARTESIAN_POINT ( 'NONE',  ( 0.000000000000000000, -1.334374999522042859, -3.793834371823813445 ) ) ;
#140469 = CARTESIAN_POINT ( 'NONE',  ( -4.462568837553487100, 5.235360394347691404, -1.199719254218453823 ) ) ;
#140470 = EDGE_CURVE ( 'NONE', #120384, #33125, #81632, .T. ) ;
#140471 = CARTESIAN_POINT ( 'NONE',  ( -6.710922849084449915, 10.77323439066645783, 0.000000000000000000 ) ) ;
#140472 = CARTESIAN_POINT ( 'NONE',  ( 4.199993725183334803, 8.122019456014369254, -0.7998128361456362523 ) ) ;
#140473 = CARTESIAN_POINT ( 'NONE',  ( 6.368043163206878354, -2.055323469740528264, 0.2474699835256082281 ) ) ;
#140474 = CARTESIAN_POINT ( 'NONE',  ( 4.441968003317652958, 0.8225352836801721468, -1.742211325687251788 ) ) ;
#140475 = CARTESIAN_POINT ( 'NONE',  ( 0.5269705342763851830, -1.727990693721896287, 1.039014695730144933 ) ) ;
#140476 = CARTESIAN_POINT ( 'NONE',  ( -10.64723070543352712, 11.31619066596094392, 0.7998128361456462443 ) ) ;
#140477 = CARTESIAN_POINT ( 'NONE',  ( 6.994027139803230320, 9.253060644560830994, -1.599625672291267398 ) ) ;
#140478 = CARTESIAN_POINT ( 'NONE',  ( 11.86145016429272836, 10.19999999999999929, -1.100000000000000311 ) ) ;
#140479 = CARTESIAN_POINT ( 'NONE',  ( 0.5861907285475282947, -2.175377356269320828, -0.2643977408666315365 ) ) ;
#140480 = CARTESIAN_POINT ( 'NONE',  ( 5.672426548614881270, -1.154804106291613675, 1.414059844683832612 ) ) ;
#140481 = CARTESIAN_POINT ( 'NONE',  ( 6.563555762791525972, 6.830105609444471426, -0.7216878364870458196 ) ) ;
#140482 = CARTESIAN_POINT ( 'NONE',  ( 4.487385655998885170, 5.298000022495898520, 1.082531754730560403 ) ) ;
#140483 = CARTESIAN_POINT ( 'NONE',  ( -4.956387674247580755, 7.940146832334256111, 1.199719254218452935 ) ) ;
#140484 = CARTESIAN_POINT ( 'NONE',  ( 4.680589345215795838, 6.483773540883647435, -1.599625672291256295 ) ) ;
#140485 = CARTESIAN_POINT ( 'NONE',  ( 5.740951700743842423, 5.662474837148078421, -0.7998128361456481317 ) ) ;
#140486 = ORIENTED_EDGE ( 'NONE', *, *, #31725, .T. ) ;
#140488 = CARTESIAN_POINT ( 'NONE',  ( 6.099863781956886832, 1.391357071557168146, 1.455236689230124947 ) ) ;
#140487 = CARTESIAN_POINT ( 'NONE',  ( 2.999365392321148516, -1.839032331094083927, 0.09308366406014097205 ) ) ;
#140489 = CARTESIAN_POINT ( 'NONE',  ( 0.9842439076201170423, 2.124318566921878482, 0.8778218499742740377 ) ) ;
#140490 = CARTESIAN_POINT ( 'NONE',  ( 6.772321408939014020, -0.9219223515295159599, -1.731591420108986812 ) ) ;
#140491 = CARTESIAN_POINT ( 'NONE',  ( -6.566226467720086113, 6.555019055295208119, 1.040834085586084257E-14 ) ) ;
#140492 = CARTESIAN_POINT ( 'NONE',  ( -5.853218251105561265, 6.233033923027780254, -0.5979115183833558778 ) ) ;
#140493 = B_SPLINE_CURVE_WITH_KNOTS ( 'NONE', 3,
 ( #65499, #131647, #49297, #115412, #102283, #118602, #54607, #133764, #151062, #132695, #53538, #37288, #183533, #120756, #153175, #149986 ),
 .UNSPECIFIED., .F., .F.,
 ( 4, 3, 3, 3, 3, 4 ),
 ( 0.000000000000000000, 2.533473342638980266E-05, 5.061406379858541306E-05, 7.673069672129149185E-05, 0.0001048028779199227441, 0.0001300696341146172241 ),
 .UNSPECIFIED. ) ;
#140494 = CARTESIAN_POINT ( 'NONE',  ( -4.295235737431041478, 3.905529869957963029, -0.7998128361456221525 ) ) ;
#140495 = CARTESIAN_POINT ( 'NONE',  ( 0.7837444799244470683, -1.966470238067185905, 0.6478734989143407619 ) ) ;
#140496 = CARTESIAN_POINT ( 'NONE',  ( -4.604929450496978660, 5.401447776115099408, -1.199719254218453823 ) ) ;
#140498 = CARTESIAN_POINT ( 'NONE',  ( 1.164687902950040321, -1.689591380799923215, -0.8031939614948147010 ) ) ;
#140497 = CARTESIAN_POINT ( 'NONE',  ( 2.472313036883976078, -2.001511166234470007, -0.6043430715973686640 ) ) ;
#140499 = CARTESIAN_POINT ( 'NONE',  ( 1.774767310740913207, -2.001205085354029301, 0.2439901982170673833 ) ) ;
#140500 = CARTESIAN_POINT ( 'NONE',  ( 9.137832345930652522, 10.72352116074969075, -1.082531754730543083 ) ) ;
#140501 = CARTESIAN_POINT ( 'NONE',  ( 0.6823417656249917140, 3.905208333674754950, 1.181850606188765695 ) ) ;
#140502 = CARTESIAN_POINT ( 'NONE',  ( 1.839017211142121244, 0.6657927772366920571, -1.608260388387482420 ) ) ;
#140503 = CARTESIAN_POINT ( 'NONE',  ( 5.983225862332436584, 5.874851682342960402, 0.7998128361456341429 ) ) ;
#140505 = CARTESIAN_POINT ( 'NONE',  ( 1.538818179733923541, 8.696032261897956417, 2.511230101280747196 ) ) ;
#140504 = CARTESIAN_POINT ( 'NONE',  ( -7.037870247915956945, -8.233137084989836652, 6.381095703207982694 ) ) ;
#140506 = CARTESIAN_POINT ( 'NONE',  ( 3.035487670047633202, -1.158914029964135395, -1.277714875195012700 ) ) ;
#140507 = CARTESIAN_POINT ( 'NONE',  ( 2.771223791512751333, 2.080116120148074010, -0.6901165687889164735 ) ) ;
#140508 = CARTESIAN_POINT ( 'NONE',  ( 4.758537496233657293, 0.8426522330295079799, 2.039869969286691731 ) ) ;
#140509 = CARTESIAN_POINT ( 'NONE',  ( -10.81659741420782872, 5.544487526538591560, -6.534070432124610583 ) ) ;
#140510 = CARTESIAN_POINT ( 'NONE',  ( 2.202231255880624516, 0.8340544509695562159, -2.004656366586863303 ) ) ;
#140511 = CARTESIAN_POINT ( 'NONE',  ( 1.260069262837599791, 0.7379878962356714034, 1.670071910705408946 ) ) ;
#140512 = CARTESIAN_POINT ( 'NONE',  ( 3.889952640533121286, -2.111394073168832097, 0.1598612332101984890 ) ) ;
#140513 = CARTESIAN_POINT ( 'NONE',  ( 11.04536101718726293, 10.19999999999999929, 1.099999999999996758 ) ) ;
#140514 = ORIENTED_EDGE ( 'NONE', *, *, #138983, .F. ) ;
#140516 = CARTESIAN_POINT ( 'NONE',  ( -1.402160292154681736E-14, 1.509375000341420359, -1.575800808251659024 ) ) ;
#140515 = CARTESIAN_POINT ( 'NONE',  ( 3.122906911094673887, 0.05843746759831092152, 2.291794357358638123 ) ) ;
#140517 = DIRECTION ( 'NONE',  ( 3.122502256758252154E-17, 2.602085213965210950E-17, 1.000000000000000000 ) ) ;
#140518 = CARTESIAN_POINT ( 'NONE',  ( 4.542145155778077203, 5.257923088951247159, -1.199719254218452047 ) ) ;
#140519 = CARTESIAN_POINT ( 'NONE',  ( -0.04015575566676531788, -1.641981170221142872, -1.341450104213978589 ) ) ;
#140520 = CARTESIAN_POINT ( 'NONE',  ( -6.399085315970151733, 7.528316292462387871, -1.082531754730544860 ) ) ;
#140521 = AXIS2_PLACEMENT_3D ( 'NONE', #41469, #8934, #190875 ) ;
#140522 = CARTESIAN_POINT ( 'NONE',  ( 4.039966587192267866, 4.776011108888172707, 1.082531754730560403 ) ) ;
#140523 = CARTESIAN_POINT ( 'NONE',  ( -7.361714222096077620, 7.691014135307965738, 0.7216878364870317197 ) ) ;
#140524 = CARTESIAN_POINT ( 'NONE',  ( 4.923019175537949543, 4.916146257648610352, 0.000000000000000000 ) ) ;
#140526 = ORIENTED_EDGE ( 'NONE', *, *, #72682, .F. ) ;
#140525 = CIRCLE ( 'NONE', #109483, 0.08000000000000020983 ) ;
#140527 = CARTESIAN_POINT ( 'NONE',  ( 4.693982515131527755, 1.755768268644173791, 0.9914009648221073778 ) ) ;
#140529 = CARTESIAN_POINT ( 'NONE',  ( 3.291897078901334428, -1.381674118267547602, -1.531590470265832726 ) ) ;
#140528 = CARTESIAN_POINT ( 'NONE',  ( 6.159481859310094620, 6.080483678816896109, 1.040834085586084257E-14 ) ) ;
#140530 = DIRECTION ( 'NONE',  ( 1.000000000000000000, -0.000000000000000000, -0.000000000000000000 ) ) ;
#140531 = CARTESIAN_POINT ( 'NONE',  ( 3.404505970362959655, 6.986024375483197879, 0.7216878364870257245 ) ) ;
#140532 = CARTESIAN_POINT ( 'NONE',  ( -1.642778471875000035, -4.017708332855376874, -2.845375778867859751 ) ) ;
#140533 = FACE_OUTER_BOUND ( 'NONE', #91213, .T. ) ;
#140534 = CARTESIAN_POINT ( 'NONE',  ( 6.597619724345276104, -2.191060131252516641, 0.04951108399064289151 ) ) ;
#140535 = CARTESIAN_POINT ( 'NONE',  ( 4.061172775696818782, -1.158689426361030561, 1.650081270007992318 ) ) ;
#140536 = CARTESIAN_POINT ( 'NONE',  ( 3.245484093776138668, 1.841430844176932480, -0.003062914905635482320 ) ) ;
#140537 = CARTESIAN_POINT ( 'NONE',  ( 5.459129407796876166, 9.520734742405036144, 1.040834085586084257E-14 ) ) ;
#140538 = CARTESIAN_POINT ( 'NONE',  ( 6.545924712158827319, 0.6954503440314525609, -1.688125835592364066 ) ) ;
#140539 =( BOUNDED_CURVE ( )  B_SPLINE_CURVE ( 2, ( #18435, #97592, #47787, #203309, #64006, #130155, #90677, #88536, #92815 ),
 .UNSPECIFIED., .F., .T. ) 
 B_SPLINE_CURVE_WITH_KNOTS ( ( 3, 2, 2, 2, 3 ),
 ( 0.7767857142857143016, 0.7797619047619047672, 0.7857142857142856984, 0.7916666666666666297, 0.7946428571428572063 ),
 .UNSPECIFIED. ) 
 CURVE ( )  GEOMETRIC_REPRESENTATION_ITEM ( )  RATIONAL_B_SPLINE_CURVE ( ( 0.9330127018922194093, 0.9330127018922194093, 1.000000000000000000, 0.8660254037844387076, 1.000000000000000000, 0.8660254037844387076, 1.000000000000000000, 0.9330127018922180770, 0.9330127018922194093 ) ) 
 REPRESENTATION_ITEM ( '' )  );
#140540 = CARTESIAN_POINT ( 'NONE',  ( 0.07143917554365029898, -1.076037094620578616, 2.031297111741585226 ) ) ;
#140541 = CARTESIAN_POINT ( 'NONE',  ( -7.901704598666176693, 8.113076874732334076, 0.7998128361456602331 ) ) ;
#140542 = CARTESIAN_POINT ( 'NONE',  ( 0.4392367245290337840, 0.3885019757292383913, 2.228643277672849976 ) ) ;
#140543 = CARTESIAN_POINT ( 'NONE',  ( 2.332770561069871462, 2.043027141408111813, 0.5109185277013729154 ) ) ;
#140544 = CARTESIAN_POINT ( 'NONE',  ( -6.286140498591554326, 7.362860665558790707, 1.199719254218452047 ) ) ;
#140545 =( REPRESENTATION_RELATIONSHIP ('NONE','NONE', #84563, #63688 ) REPRESENTATION_RELATIONSHIP_WITH_TRANSFORMATION ( #39544 )SHAPE_REPRESENTATION_RELATIONSHIP( ) );
#140546 = CARTESIAN_POINT ( 'NONE',  ( 8.938903350111612411, 9.323142084752035430, -0.7998128361456221525 ) ) ;
#140547 = CARTESIAN_POINT ( 'NONE',  ( 6.658462837642791676, 8.861568958707010779, 1.443375672974063439 ) ) ;
#140548 = DIRECTION ( 'NONE',  ( 0.5241784747566542446, 0.000000000000000000, 0.8516084350226855726 ) ) ;
#140549 = CARTESIAN_POINT ( 'NONE',  ( -6.226218857173722476, 8.287007971501239467, 1.599625672291283607 ) ) ;
#140550 = CARTESIAN_POINT ( 'NONE',  ( -3.789102684798408838, 7.352775819508957866, -0.6979800873464858668 ) ) ;
#140551 = CARTESIAN_POINT ( 'NONE',  ( 7.917598520256366790, 8.339545816494993602, 1.040834085586084257E-14 ) ) ;
#140552 = CARTESIAN_POINT ( 'NONE',  ( 4.291716407524416077, 7.230775179981989709, -0.9765121647202840149 ) ) ;
#140553 = CARTESIAN_POINT ( 'NONE',  ( -3.601662362724658895, 7.353689856487406473, -0.7998128361456281477 ) ) ;
#140554 = CARTESIAN_POINT ( 'NONE',  ( 4.271885190509593144, 0.4847678284230126922, -2.167736239397171083 ) ) ;
#140555 = CARTESIAN_POINT ( 'NONE',  ( 0.9904705247469265394, -0.5356807779838267392, -2.124848333686576662 ) ) ;
#140556 = CARTESIAN_POINT ( 'NONE',  ( 0.3642759247451561322, 2.182245240920151375, -0.3280614795862640820 ) ) ;
#140557 = CARTESIAN_POINT ( 'NONE',  ( -5.255720823952942489, 6.160704378480398979, -1.199719254218453823 ) ) ;
#140558 = CARTESIAN_POINT ( 'NONE',  ( 4.861744986159981075, -0.5251177144562025889, 1.890194517805739771 ) ) ;
#140559 = CARTESIAN_POINT ( 'NONE',  ( 8.866142388332804103, 12.43125098877526113, -1.199719254218446718 ) ) ;
#140560 = DIRECTION ( 'NONE',  ( -0.000000000000000000, -1.000000000000000000, -0.000000000000000000 ) ) ;
#140561 = CARTESIAN_POINT ( 'NONE',  ( -1.364683531250000748, 1.009375000341421247, 0.000000000000000000 ) ) ;
#140562 = CARTESIAN_POINT ( 'NONE',  ( -5.004368097219957789, 5.011053332944274352, 0.000000000000000000 ) ) ;
#140565 = EDGE_LOOP ( 'NONE', ( #19427, #68716, #118, #58964 ) ) ;
#140564 = CARTESIAN_POINT ( 'NONE',  ( -4.907688418466881863, 8.669460888279271416, 0.7216878364870458196 ) ) ;
#140563 =( GEOMETRIC_REPRESENTATION_CONTEXT ( 3 ) GLOBAL_UNCERTAINTY_ASSIGNED_CONTEXT ( ( #157336 ) ) GLOBAL_UNIT_ASSIGNED_CONTEXT ( ( #54350, #72712, #58609 ) ) REPRESENTATION_CONTEXT ( 'NONE', 'WORKASPACE' ) );
#140566 = CARTESIAN_POINT ( 'NONE',  ( 4.008146050417991546, -0.8085630067716749192, 1.960596031080278356 ) ) ;
#140567 = CARTESIAN_POINT ( 'NONE',  ( -3.526002468005825286, 6.271364091718859335, -1.199719254218450271 ) ) ;
#140568 = CARTESIAN_POINT ( 'NONE',  ( 5.875883356151954118, 1.283970044810868849, 1.738936680771227206 ) ) ;
#140569 = CARTESIAN_POINT ( 'NONE',  ( 4.423293856316495187, -1.136390847421838490, -1.448631019334602144 ) ) ;
#140570 = CARTESIAN_POINT ( 'NONE',  ( -5.812277037385564782, 6.060071624232533871, -0.5253754717876522040 ) ) ;
#140571 = CARTESIAN_POINT ( 'NONE',  ( -1.364683531250014514, 0.8010416670080889867, -0.7879004041258289570 ) ) ;
#140572 = CARTESIAN_POINT ( 'NONE',  ( 0.1513755341013711675, 0.6631104863988640519, 1.609371435944781936 ) ) ;
#140573 = CARTESIAN_POINT ( 'NONE',  ( 6.827182134110195477, 0.006757161851597691914, 1.710856279483467413 ) ) ;
#140574 = CARTESIAN_POINT ( 'NONE',  ( 3.714570900464285064, 4.396382807705524698, 1.082531754730560403 ) ) ;
#140575 = CARTESIAN_POINT ( 'NONE',  ( 8.990221719931399846, 12.33023651109059493, 7.951427823052896748 ) ) ;
#140577 = EDGE_CURVE ( 'NONE', #134499, #204806, #202736, .T. ) ;
#140576 =( GEOMETRIC_REPRESENTATION_CONTEXT ( 3 ) GLOBAL_UNCERTAINTY_ASSIGNED_CONTEXT ( ( #3315 ) ) GLOBAL_UNIT_ASSIGNED_CONTEXT ( ( #57416, #152783, #24897 ) ) REPRESENTATION_CONTEXT ( 'NONE', 'WORKASPACE' ) );
#140578 = CARTESIAN_POINT ( 'NONE',  ( 3.784175263432405956, -1.067420458145739826, 1.879713924940962677 ) ) ;
#140579 = CARTESIAN_POINT ( 'NONE',  ( -3.653032323878261600, 6.349289246911547835, -1.199719254218452047 ) ) ;
#140580 = CARTESIAN_POINT ( 'NONE',  ( 5.835314490094169138, -1.281163661392352493, 1.556671411349755285 ) ) ;
#140581 = CARTESIAN_POINT ( 'NONE',  ( -7.009202228140739344, 11.12122699956546334, -0.7216878364870267237 ) ) ;
#140582 = CARTESIAN_POINT ( 'NONE',  ( 3.309602206082487008, -0.4233974974612622066, 2.119663826602156131 ) ) ;
#140584 = CARTESIAN_POINT ( 'NONE',  ( 3.936761750732898690, 0.2861355568666827387, 1.950351509585077858 ) ) ;
#140583 = B_SPLINE_CURVE_WITH_KNOTS ( 'NONE', 3,
 ( #110273, #176282, #96110, #27884 ),
 .UNSPECIFIED., .F., .F.,
 ( 4, 4 ),
 ( 0.002059939351769825289, 0.002341702326271046831 ),
 .UNSPECIFIED. ) ;
#140585 = CARTESIAN_POINT ( 'NONE',  ( 1.483892314354786857, 2.131289638308156320, -0.8850757863276045301 ) ) ;
#140586 = CARTESIAN_POINT ( 'NONE',  ( 4.165347332011271497, 0.2559277237221342371, -2.044777286818760142 ) ) ;
#140587 = CARTESIAN_POINT ( 'NONE',  ( 6.146037779257278011, 0.6132840560482490933, 1.842739892034722882 ) ) ;
#140589 = VERTEX_POINT ( 'NONE', #186504 ) ;
#140588 = CARTESIAN_POINT ( 'NONE',  ( -6.683806541412756985, 10.74159869838281622, -0.7216878364870267237 ) ) ;
#140590 = AXIS2_PLACEMENT_3D ( 'NONE', #206822, #89910, #189514 ) ;
#140591 = CARTESIAN_POINT ( 'NONE',  ( -4.796552484184649856, 8.818004674849227342, -0.7998128361456362523 ) ) ;
#140592 = CARTESIAN_POINT ( 'NONE',  ( 11.86239285000045562, 9.799999999999982947, 1.812080536912751061 ) ) ;
#140594 = VERTEX_POINT ( 'NONE', #7744 ) ;
#140593 = CARTESIAN_POINT ( 'NONE',  ( -5.327428015527048366, 5.180030537728460338, -0.7998128361456362523 ) ) ;
#140595 = CARTESIAN_POINT ( 'NONE',  ( -7.334597914868735025, 9.580116872145431728, -1.443375672974058777 ) ) ;
#140596 = CARTESIAN_POINT ( 'NONE',  ( 2.802037382575186975, -0.6933082239683820980, 2.095089865402133267 ) ) ;
#140597 = CARTESIAN_POINT ( 'NONE',  ( -3.285556943750000070, -3.696874999522044458, 0.000000000000000000 ) ) ;
#140598 = ORIENTED_EDGE ( 'NONE', *, *, #22500, .T. ) ;
#140599 = CARTESIAN_POINT ( 'NONE',  ( 6.051606296966551390, 1.483190043545830505, 1.284043323103729595 ) ) ;
#140600 = CARTESIAN_POINT ( 'NONE',  ( -0.1290005225502432740, 4.081813041011835175, -2.728655865233818201 ) ) ;
#140601 = FACE_OUTER_BOUND ( 'NONE', #112797, .T. ) ;
#140603 = CARTESIAN_POINT ( 'NONE',  ( -10.99943592164172834, -8.407420853759269619, 0.1113975120798846308 ) ) ;
#140602 = DIRECTION ( 'NONE',  ( 0.7592566023653005702, 0.6507913734559639396, 0.000000000000000000 ) ) ;
#140604 = CARTESIAN_POINT ( 'NONE',  ( 5.296754776809613041, 1.507285696749562476, 1.057021923447129197 ) ) ;
#140605 = ORIENTED_EDGE ( 'NONE', *, *, #72682, .T. ) ;
#140606 = CARTESIAN_POINT ( 'NONE',  ( 1.868112839806375325, 1.058416689118582665, 1.768180007894581740 ) ) ;
#140607 = CARTESIAN_POINT ( 'NONE',  ( 1.360316468749969809, 0.7447916670080856338, 0.7853790794158741484 ) ) ;
#140608 = CARTESIAN_POINT ( 'NONE',  ( -6.398558430645608475, 9.552403038140164782, -1.199719254218440723 ) ) ;
#140609 = DIRECTION ( 'NONE',  ( 1.276756478318932191E-15, -1.000000000000000000, 3.330669073875483426E-16 ) ) ;
#140610 = SURFACE_STYLE_USAGE ( .BOTH. , #107059 ) ;
#140611 = CARTESIAN_POINT ( 'NONE',  ( 4.635998460869027227, 7.496083073400806818, -1.199719254218452047 ) ) ;
#140612 = CARTESIAN_POINT ( 'NONE',  ( 1.112264416572866566, -0.9257652390157306010, -1.841317064699917516 ) ) ;
#140614 = CARTESIAN_POINT ( 'NONE',  ( 4.810013364240863787, 1.265987717737980134, -1.337210144835267345 ) ) ;
#140613 = CARTESIAN_POINT ( 'NONE',  ( -10.85954583250327588, 4.658451743348587470, -5.107361846340859657 ) ) ;
#140615 = CARTESIAN_POINT ( 'NONE',  ( 6.012151052656117933, 9.101594430485762999, 1.199719254218460707 ) ) ;
#140616 = CARTESIAN_POINT ( 'NONE',  ( -6.469175572376043348, 7.576401584974034265, 1.199719254218452047 ) ) ;
#140618 = ORIENTED_EDGE ( 'NONE', *, *, #148050, .T. ) ;
#140617 = CARTESIAN_POINT ( 'NONE',  ( 6.610000000000026965, 7.052677709320480659, 2.598153670447616470 ) ) ;
#140619 = CARTESIAN_POINT ( 'NONE',  ( 4.424592250794217030, 1.359014646446855767, -1.738718759629574118 ) ) ;
#140620 = CARTESIAN_POINT ( 'NONE',  ( 0.4566077865506940059, 0.8268718848777978359, 1.997384878126715613 ) ) ;
#140621 = CARTESIAN_POINT ( 'NONE',  ( -4.934804725694220906, 7.740727365743146571, -1.082531754730549967 ) ) ;
#140622 = CARTESIAN_POINT ( 'NONE',  ( -0.1054227091227821350, -1.855472971956134920, -0.4628026090111520552 ) ) ;
#140623 = CARTESIAN_POINT ( 'NONE',  ( -0.1882626618336727398, -1.244567986390752390, -1.587255334073833790 ) ) ;
#140624 = CARTESIAN_POINT ( 'NONE',  ( 7.824464048418096951, 8.301165276008827476, -0.7216878364870317197 ) ) ;
#140625 = CARTESIAN_POINT ( 'NONE',  ( 0.07536363704235826688, -0.001874865094115066300, -2.144269471569634877 ) ) ;
#140626 = CARTESIAN_POINT ( 'NONE',  ( 5.356085673312771966, 0.7711821229579116643, -1.750063228584404440 ) ) ;
#140627 = CARTESIAN_POINT ( 'NONE',  ( -0.008622031262367491067, 15.44736672593548299, 11.95585889282746450 ) ) ;
#140628 = CARTESIAN_POINT ( 'NONE',  ( 1.182252951876180180, -1.824241171369020531, -0.4133900166373091767 ) ) ;
#140629 = CARTESIAN_POINT ( 'NONE',  ( 2.641814858895009444, 2.006371511526034546, -0.2024640970367599380 ) ) ;
#140631 = CARTESIAN_POINT ( 'NONE',  ( 3.475310780013381340, 0.05149396089606420035, -2.105609240523627967 ) ) ;
#140630 = CARTESIAN_POINT ( 'NONE',  ( -7.883176251342026042, 11.28445716228600126, -1.199719254218446718 ) ) ;
#140632 = CARTESIAN_POINT ( 'NONE',  ( 8.945682426918439845, 9.331051007693339727, 1.040834085586084257E-14 ) ) ;
#140634 = CARTESIAN_POINT ( 'NONE',  ( -8.311311860377216476, 9.655284244316948872, -1.199719254218446718 ) ) ;
#140633 = CARTESIAN_POINT ( 'NONE',  ( 3.898851692381625877, 6.706354853490643642, -1.199719254218452047 ) ) ;
#140635 = DIRECTION ( 'NONE',  ( 0.000000000000000000, 1.000000000000000000, 0.000000000000000000 ) ) ;
#140636 = CARTESIAN_POINT ( 'NONE',  ( 4.500263427444707531, -0.9482861330638262531, 1.783302102689677371 ) ) ;
#140637 = B_SPLINE_CURVE_WITH_KNOTS ( 'NONE', 3,
 ( #1055, #119158, #185142, #120239, #19449, #70317, #3181 ),
 .UNSPECIFIED., .F., .F.,
 ( 4, 3, 4 ),
 ( 0.0001135037246152890099, 0.0006245292469112829472, 0.002007692286193829209 ),
 .UNSPECIFIED. ) ;
#140638 = CARTESIAN_POINT ( 'NONE',  ( 0.6823417656249917140, 4.592708333674755394, 1.181850606188765695 ) ) ;
#140639 = CARTESIAN_POINT ( 'NONE',  ( 8.758204044747994743, 12.20135990463928266, 1.082531754730546636 ) ) ;
#140640 = CARTESIAN_POINT ( 'NONE',  ( 4.710339443014814442, -0.9195336665917231977, -1.956380038831563972 ) ) ;
#140641 = CARTESIAN_POINT ( 'NONE',  ( 5.875479466675786355, 7.948088359245467416, -1.599625672291283607 ) ) ;
#140642 = CARTESIAN_POINT ( 'NONE',  ( -1.402160292154681736E-14, 0.009375000341421267647, -1.575800808251665908 ) ) ;
#140643 = CARTESIAN_POINT ( 'NONE',  ( 7.205232291019763480, 7.370802192470005565, -0.7998128361456341429 ) ) ;
#140644 = CARTESIAN_POINT ( 'NONE',  ( 9.070041577417981671, 9.684062716516882219, -0.7216878364870197293 ) ) ;
#140646 = DIRECTION ( 'NONE',  ( -0.000000000000000000, -1.000000000000000000, -0.000000000000000000 ) ) ;
#140645 = CARTESIAN_POINT ( 'NONE',  ( 1.926474581872784420, 1.115185415580312700, 1.862746952601635808 ) ) ;
#140648 = CARTESIAN_POINT ( 'NONE',  ( 0.5207438388301621757, -1.748553680932497745, 0.5769860859521497298 ) ) ;
#140647 = CARTESIAN_POINT ( 'NONE',  ( -4.270455198624581783, 7.926022131796578662, 1.040834085586084257E-14 ) ) ;
#140649 = STYLED_ITEM ( 'NONE', ( #125270 ), #15532 ) ;
#140650 = CARTESIAN_POINT ( 'NONE',  ( -0.6823417656250003738, 2.467708333674753618, -1.181850606188749264 ) ) ;
#140651 = CARTESIAN_POINT ( 'NONE',  ( 3.421585747727782678, -1.306972202059282218, -1.759028276249123168 ) ) ;
#140652 = CARTESIAN_POINT ( 'NONE',  ( 6.983263157960330147, 7.052490050591996962, 2.551961896892048109 ) ) ;
#140653 = CARTESIAN_POINT ( 'NONE',  ( 3.432755235230527280, 2.206939294067700619, 0.4977334550177249795 ) ) ;
#140654 = CARTESIAN_POINT ( 'NONE',  ( -7.152089726408780379, 8.302858421353754181, -1.199719254218446718 ) ) ;
#140655 = CARTESIAN_POINT ( 'NONE',  ( -1.201851678989727383E-14, 4.509375000341417916, -1.575800808251660134 ) ) ;
#140656 = CARTESIAN_POINT ( 'NONE',  ( 6.453003701063230402, 6.772902045581084884, 0.3391303328579304277 ) ) ;
#140657 = CARTESIAN_POINT ( 'NONE',  ( 0.7500000000000006661, 12.66666666666666607, -1.299038105676657340 ) ) ;
#140658 = CARTESIAN_POINT ( 'NONE',  ( 4.095971805104276164, 7.792734516014745871, 0.7216878364870257245 ) ) ;
#140659 = CARTESIAN_POINT ( 'NONE',  ( 4.586996685387556560, 1.581260375356493331, -0.7947977318805318214 ) ) ;
#140660 = CARTESIAN_POINT ( 'NONE',  ( 7.609150525767641504, 9.900428251527500834, -1.599625672291262513 ) ) ;
#140661 = CARTESIAN_POINT ( 'NONE',  ( 0.6574224672675427206, -1.779203033188281990, -1.126420244723020270 ) ) ;
#140663 = CARTESIAN_POINT ( 'NONE',  ( 1.499999999999989120, 1.275000000000019229, 0.000000000000000000 ) ) ;
#140662 = CARTESIAN_POINT ( 'NONE',  ( 1.364683531249996529, 10.71354166700806942, 0.7879004041258405033 ) ) ;
#140664 = CARTESIAN_POINT ( 'NONE',  ( 1.328490337915340991, -1.252144239891037403, 1.520259730874585768 ) ) ;
#140665 = CARTESIAN_POINT ( 'NONE',  ( -3.851398154733808088, 6.650992392901508232, -1.199719254218450271 ) ) ;
#140666 = CARTESIAN_POINT ( 'NONE',  ( -0.4967775439449015895, 7.792564024146572343, -1.990974371293803280 ) ) ;
#140668 = VERTEX_POINT ( 'NONE', #173494 ) ;
#140667 = CARTESIAN_POINT ( 'NONE',  ( 5.238451434589118882, 1.072694688086765158, -1.459716015685054602 ) ) ;
#140669 = CARTESIAN_POINT ( 'NONE',  ( 6.426201623197458801, 9.480690412830290015, -1.082531754730537088 ) ) ;
#140670 = CARTESIAN_POINT ( 'NONE',  ( 8.048736748007069508, 12.54194330598362406, -0.7998128361456352531 ) ) ;
#140672 = CARTESIAN_POINT ( 'NONE',  ( 4.592568387165754551, -0.4099775813008778025, -1.825014511474598589 ) ) ;
#140671 = CIRCLE ( 'NONE', #182046, 11.09999999999999964 ) ;
#140673 = ORIENTED_EDGE ( 'NONE', *, *, #192933, .T. ) ;
#140674 = CARTESIAN_POINT ( 'NONE',  ( 4.768459183169745152, -0.8803848081004579385, -1.873848736155204087 ) ) ;
#140675 = CARTESIAN_POINT ( 'NONE',  ( 1.224999999999974332, 2.374999999999988454, -3.295974604355933479E-14 ) ) ;
#140676 = CARTESIAN_POINT ( 'NONE',  ( -5.424670858799220063, 9.342883411992149334, 0.000000000000000000 ) ) ;
#140677 = CARTESIAN_POINT ( 'NONE',  ( 0.8814639207992844838, -0.9023425969398091162, -3.213948531368630679 ) ) ;
#140678 = CARTESIAN_POINT ( 'NONE',  ( 7.391166297744269365, 11.77477778067701664, 1.040834085586084257E-14 ) ) ;
#140679 = CARTESIAN_POINT ( 'NONE',  ( -8.482597663644387609, 13.04811437422715414, -0.7998128361456281477 ) ) ;
#140680 = CARTESIAN_POINT ( 'NONE',  ( 6.912678218121202534, 9.158153569265168770, 1.599625672291268286 ) ) ;
#140681 = EDGE_CURVE ( 'NONE', #110280, #26662, #189858, .T. ) ;
#140682 = CARTESIAN_POINT ( 'NONE',  ( -4.911752498546917423, 4.707425932596563278, -0.3822207396134598145 ) ) ;
#140683 = CARTESIAN_POINT ( 'NONE',  ( -1.364683531250010295, 5.592708333674750953, 0.7879004041258379498 ) ) ;
#140684 = CARTESIAN_POINT ( 'NONE',  ( -1.500000000000013101, 0.4208333333333572068, 0.8660254037844403729 ) ) ;
#140685 = CARTESIAN_POINT ( 'NONE',  ( 4.510177812457000002, 1.961482754637720927, -0.04604004567236585910 ) ) ;
#140686 = CARTESIAN_POINT ( 'NONE',  ( 1.563827143785265328, 1.649830188709809686, -1.158509706484150970 ) ) ;
#140687 = CYLINDRICAL_SURFACE ( 'NONE', #100309, 1.500000000000000222 ) ;
#140688 = CARTESIAN_POINT ( 'NONE',  ( 7.680942717881078075, -5.294771359305314284, 7.874499448206171870 ) ) ;
#140689 = DIRECTION ( 'NONE',  ( 0.000000000000000000, 0.000000000000000000, 1.000000000000000000 ) ) ;
#140690 = CARTESIAN_POINT ( 'NONE',  ( 1.563515255687727645, 1.843751956470768283, -0.3144994141817195055 ) ) ;
#140691 = CARTESIAN_POINT ( 'NONE',  ( -0.6823417656250212460, 5.051041667008086655, 1.181850606188767472 ) ) ;
#140692 = CARTESIAN_POINT ( 'NONE',  ( 2.531496316177814787, -0.1932786158439051827, 2.003878288502713101 ) ) ;
#140694 = CARTESIAN_POINT ( 'NONE',  ( 3.568056664072499995, -1.041641863948725932, 1.843179926220348541 ) ) ;
#140693 = CARTESIAN_POINT ( 'NONE',  ( -6.453317930424837812, 7.591587675992828466, 1.082531754730549967 ) ) ;
#140696 = EDGE_CURVE ( 'NONE', #162407, #113693, #203214, .T. ) ;
#140695 = DIRECTION ( 'NONE',  ( 3.552713678800500929E-15, 0.000000000000000000, 1.000000000000000000 ) ) ;
#140697 = CARTESIAN_POINT ( 'NONE',  ( 5.055165704564410944, 1.723227314588217318, -1.147259442322377865 ) ) ;
#140698 = CARTESIAN_POINT ( 'NONE',  ( 7.015418140428412386, 7.149352350113456822, 0.7998128361456331437 ) ) ;
#140700 = CARTESIAN_POINT ( 'NONE',  ( 6.620655732516652847, 0.5779860733656561056, 2.127054332187257923 ) ) ;
#140699 = CARTESIAN_POINT ( 'NONE',  ( 0.5211768519108473940, -1.983982463993728906, 0.6597393503331959730 ) ) ;
#140702 = ORIENTED_EDGE ( 'NONE', *, *, #69404, .F. ) ;
#140701 = CARTESIAN_POINT ( 'NONE',  ( 4.893472065931465664, 1.353474861756031267, 1.225258530246610134 ) ) ;
#140703 = CARTESIAN_POINT ( 'NONE',  ( 6.903072767652295383, 11.20533532890304684, 1.040834085586084257E-14 ) ) ;
#140704 = CARTESIAN_POINT ( 'NONE',  ( -3.797692425159308716, 7.444741906078900406, 0.000000000000000000 ) ) ;
#140705 =( NAMED_UNIT ( * ) SI_UNIT ( $, .STERADIAN. ) SOLID_ANGLE_UNIT ( ) );
#140706 = CARTESIAN_POINT ( 'NONE',  ( -11.69053533621101160, 4.400474013969419396, 5.144636342886200531 ) ) ;
#140707 = CARTESIAN_POINT ( 'NONE',  ( 0.6823417656249934904, 11.50520833367473017, 1.181850606188764807 ) ) ;
#140708 = CARTESIAN_POINT ( 'NONE',  ( 5.742805640131908973, 1.844151595126357179, 0.5056804652876015771 ) ) ;
#140709 = CARTESIAN_POINT ( 'NONE',  ( -9.104463846776669200, 10.58062822844965645, -1.199719254218441611 ) ) ;
#140710 = CARTESIAN_POINT ( 'NONE',  ( 7.305145839664861640, 7.417091655897478653, 0.7998128361456341429 ) ) ;
#140711 = CARTESIAN_POINT ( 'NONE',  ( -4.356712336337761644E-14, 2.859375000341351392, -1.570758158831810247 ) ) ;
#140712 = CARTESIAN_POINT ( 'NONE',  ( 4.487385655998888723, 4.337630808194552934, 0.7216878364870317197 ) ) ;
#140713 = CARTESIAN_POINT ( 'NONE',  ( -1.000000000000017097, 5.868705557303652398, 4.125226524755080781 ) ) ;
#140714 = CARTESIAN_POINT ( 'NONE',  ( 5.495132332240461714, 5.305409230568988832, 0.7998128361456341429 ) ) ;
#140715 = ORIENTED_EDGE ( 'NONE', *, *, #130589, .T. ) ;
#140716 = CIRCLE ( 'NONE', #192466, 3.970406073902761790 ) ;
#140717 = CARTESIAN_POINT ( 'NONE',  ( -7.435720902452096936, 7.639705572474380091, 0.000000000000000000 ) ) ;
#140718 = CARTESIAN_POINT ( 'NONE',  ( 5.448842280278080707, -1.824126957265741256, -0.8596167168879662590 ) ) ;
#140719 = CARTESIAN_POINT ( 'NONE',  ( 0.000000000000000000, -1.500000000000001332, 0.000000000000000000 ) ) ;
#140720 = CARTESIAN_POINT ( 'NONE',  ( -0.3870405448657274761, 1.264806443676224079, 11.85654951141428981 ) ) ;
#140721 = CARTESIAN_POINT ( 'NONE',  ( 0.1394461523057084484, 7.629137130509043629, -2.319723760180956607 ) ) ;
#140722 = EDGE_CURVE ( 'NONE', #66223, #20303, #109386, .T. ) ;
#140723 = CARTESIAN_POINT ( 'NONE',  ( -4.433153041988574294, 8.115836282387899558, 1.040834085586084257E-14 ) ) ;
#140724 = CARTESIAN_POINT ( 'NONE',  ( 8.581948047770334043, 12.95609712246668899, 0.000000000000000000 ) ) ;
#140725 = CARTESIAN_POINT ( 'NONE',  ( 2.078894642590666031, 1.835759051837970945, 0.7136754054878727827 ) ) ;
#140726 = CARTESIAN_POINT ( 'NONE',  ( 3.831657784458125438, 0.6766976527424087839, -1.899625577706779422 ) ) ;
#140727 = CARTESIAN_POINT ( 'NONE',  ( -8.355902744723985975, 8.642974711799791265, 1.040834085586084257E-14 ) ) ;
#140728 = CARTESIAN_POINT ( 'NONE',  ( 6.727182134110237577, 2.938513203633616566, 2.740843696613648017 ) ) ;
#140729 = STYLED_ITEM ( 'NONE', ( #150639 ), #144182 ) ;
#140730 = CARTESIAN_POINT ( 'NONE',  ( 4.136819237485493517, -1.907179771870757268, 1.079280405373375773 ) ) ;
#140731 = DIRECTION ( 'NONE',  ( 0.000000000000000000, 1.000000000000000000, 0.000000000000000000 ) ) ;
#140732 = CARTESIAN_POINT ( 'NONE',  ( 2.309485145960771035, -0.4240201670873133266, 1.878992650109307716 ) ) ;
#140733 = CARTESIAN_POINT ( 'NONE',  ( -8.616370316684697883, 10.01118577667568132, -1.199719254218446718 ) ) ;
#140734 = CARTESIAN_POINT ( 'NONE',  ( 1.836970198721030181E-16, 13.49999999999999822, 1.500000000000000222 ) ) ;
#140735 = CARTESIAN_POINT ( 'NONE',  ( 0.2333540202161792088, 2.022347194651296753, -2.461825824937914575 ) ) ;
#140736 = CARTESIAN_POINT ( 'NONE',  ( 0.000000000000000000, 0.9330127018934565308, 0.000000000000000000 ) ) ;
#140737 = CARTESIAN_POINT ( 'NONE',  ( 8.284195553149872993, 9.623648552551724578, -1.199719254218445830 ) ) ;
#140738 = CARTESIAN_POINT ( 'NONE',  ( 4.476163270806094552, 8.373940915915776273, 0.7998128361456462443 ) ) ;
#140739 = DIRECTION ( 'NONE',  ( 0.000000000000000000, 0.000000000000000000, -1.000000000000000000 ) ) ;
#140740 = CARTESIAN_POINT ( 'NONE',  ( 4.746763178560250651, 7.591621904078704297, 1.082531754730549078 ) ) ;
#140741 = ORIENTED_EDGE ( 'NONE', *, *, #35015, .F. ) ;
#140743 = CARTESIAN_POINT ( 'NONE',  ( 2.367839801511921305, 0.5346396131555611886, -1.940748983941695371 ) ) ;
#140742 = CARTESIAN_POINT ( 'NONE',  ( 5.653808312887880660, 0.7519890275384639722, 1.680886247995525773 ) ) ;
#140744 = CARTESIAN_POINT ( 'NONE',  ( 5.888098204360154853, -0.06530352750959941832, 2.297622472229691404 ) ) ;
#140745 = CARTESIAN_POINT ( 'NONE',  ( 3.010441868158566958, 0.6223964701937385602, 1.753942229013090159 ) ) ;
#140746 = CARTESIAN_POINT ( 'NONE',  ( 1.642778471875001811, -1.042708332855375009, 2.845375778867859751 ) ) ;
#140747 = CARTESIAN_POINT ( 'NONE',  ( -15.75000000000000000, 11.29999999999999893, 0.6999999999999992895 ) ) ;
#140748 = SURFACE_STYLE_FILL_AREA ( #10685 ) ;
#140749 = CARTESIAN_POINT ( 'NONE',  ( -6.669721502918952716, 9.868759955792373972, 1.199719254218452047 ) ) ;
#140750 = CARTESIAN_POINT ( 'NONE',  ( -4.502716413514310290, 6.346531463890372926, -1.443375672974066548 ) ) ;
#140751 = CARTESIAN_POINT ( 'NONE',  ( 5.812080397998875547, 1.403551008015807788, -1.549792465900756477 ) ) ;
#140752 = CARTESIAN_POINT ( 'NONE',  ( 6.832946231607457399, 7.074118146404578589, -0.7216878364870257245 ) ) ;
#140753 = ORIENTED_EDGE ( 'NONE', *, *, #111106, .F. ) ;
#140754 = CARTESIAN_POINT ( 'NONE',  ( -1.500000000000079492, 7.438721522839117917, 4.195160983902621155 ) ) ;
#140755 = CARTESIAN_POINT ( 'NONE',  ( -11.04978080397792972, 12.49155475012286942, 1.057339094031728211 ) ) ;
#140756 = CARTESIAN_POINT ( 'NONE',  ( 5.777914075412113881, 1.032862044635925569, 1.381300780159310460 ) ) ;
#140757 = CARTESIAN_POINT ( 'NONE',  ( -4.238895582566952314, 8.097128612970093897, 1.040834085586084257E-14 ) ) ;
#140758 = CARTESIAN_POINT ( 'NONE',  ( 1.564674090997038025, -0.9275931817575002736, 1.464960531123546961 ) ) ;
#140759 = CARTESIAN_POINT ( 'NONE',  ( 6.844806938814767427, -6.074287852078585459, 7.461813752226492014 ) ) ;
#140760 = SURFACE_STYLE_USAGE ( .BOTH. , #74656 ) ;
#140761 = CARTESIAN_POINT ( 'NONE',  ( 6.315302488195832176, -1.857785929941946135, -1.123309179604212504 ) ) ;
#140762 = CARTESIAN_POINT ( 'NONE',  ( 4.670415550810885996, -1.190324863180821646, 1.384379922071424351 ) ) ;
#140763 = CARTESIAN_POINT ( 'NONE',  ( 1.727322521004183598, 0.1496332796787832875, -1.956138870750294023 ) ) ;
#140764 = DIRECTION ( 'NONE',  ( 0.000000000000000000, -1.000000000000000000, 0.000000000000000000 ) ) ;
#140765 = CARTESIAN_POINT ( 'NONE',  ( -8.967828540435322182, 12.54988483289483980, 1.199719254218462483 ) ) ;
#140766 = CARTESIAN_POINT ( 'NONE',  ( 7.938462636001388795, 9.220293482545153907, -1.199719254218441611 ) ) ;
#140767 = CARTESIAN_POINT ( 'NONE',  ( 3.703867829435038228, 1.536975034498413439, 1.461131120854219700 ) ) ;
#140768 = CARTESIAN_POINT ( 'NONE',  ( 11.94105721237523277, 12.69999999999999929, 1.187919463087244720 ) ) ;
#140769 = CARTESIAN_POINT ( 'NONE',  ( -5.181866634007240791, 6.340624232048664766, 1.284222742053082733 ) ) ;
#140770 = CARTESIAN_POINT ( 'NONE',  ( -4.610256348478378285, 6.944848931137240555, -1.199160056556654697 ) ) ;
#140771 = CARTESIAN_POINT ( 'NONE',  ( 1.973570569994816060, -0.2575147360633044391, 2.054139978358980656 ) ) ;
#140773 = CARTESIAN_POINT ( 'NONE',  ( -1.500000000000008216, 14.78125000068279604, 3.469446951953614189E-15 ) ) ;
#140772 = CARTESIAN_POINT ( 'NONE',  ( 0.000000000000000000, -0.6185895741317448682, 0.000000000000000000 ) ) ;
#140775 = EDGE_LOOP ( 'NONE', ( #212845, #84063, #31714, #191559 ) ) ;
#140774 = CARTESIAN_POINT ( 'NONE',  ( 3.879691667246706110, 0.2712996660018602846, -2.204593333604548455 ) ) ;
#140776 = CARTESIAN_POINT ( 'NONE',  ( 1.231506118810040018, 2.296321937838792238, 0.1066795702680169711 ) ) ;
#140778 = CARTESIAN_POINT ( 'NONE',  ( 6.174688434915334589, 1.389358497796209013, -1.524562697504736164 ) ) ;
#140777 = CARTESIAN_POINT ( 'NONE',  ( 8.432808358020015049, 11.82173160345663376, 1.082531754730546636 ) ) ;
#140780 = CARTESIAN_POINT ( 'NONE',  ( 3.285556943750000514, -3.463541666188707957, 1.896917185911906500 ) ) ;
#140779 = CARTESIAN_POINT ( 'NONE',  ( 3.528865121306874464, 7.339036084825155015, -0.7998128361456362523 ) ) ;
#140781 = CYLINDRICAL_SURFACE ( 'NONE', #203126, 1.500000000000000222 ) ;
#140782 = CARTESIAN_POINT ( 'NONE',  ( 6.339398910184078417, 0.6979989802004606947, -1.704029730133400866 ) ) ;
#140783 = SURFACE_STYLE_USAGE ( .BOTH. , #74681 ) ;
#140784 = CARTESIAN_POINT ( 'NONE',  ( -0.1104750535120251481, 6.947232870375212421, -2.698533382536407732 ) ) ;
#140785 = CARTESIAN_POINT ( 'NONE',  ( 3.504663807952506538, 1.359994529648723249, -1.060664293495124477 ) ) ;
#140786 = CARTESIAN_POINT ( 'NONE',  ( 1.780482797753998092, -0.5424726148271253878, -1.942096288550937411 ) ) ;
#140787 = CARTESIAN_POINT ( 'NONE',  ( 3.077065830326791929, -0.9295426453954873658, 2.102514275539566935 ) ) ;
#140788 = CARTESIAN_POINT ( 'NONE',  ( 3.585499571845919942, 2.047054288528706412, -0.9635960562263863327 ) ) ;
#140789 = CARTESIAN_POINT ( 'NONE',  ( 5.795568699328918605, 1.593732954614892616, 1.376895199011922477 ) ) ;
#140790 = CARTESIAN_POINT ( 'NONE',  ( -5.777182853198894463, 9.754147405458438058, 0.7216878364870267237 ) ) ;
#140791 = CARTESIAN_POINT ( 'NONE',  ( 3.374023350818358580, -1.056766630983814625, 1.419390967538982418 ) ) ;
#140792 = CIRCLE ( 'NONE', #47398, 0.8300000000000008482 ) ;
#140793 = B_SPLINE_CURVE_WITH_KNOTS ( 'NONE', 3,
 ( #140504, #174059, #155651, #204359, #22417, #88526, #25631, #72234 ),
 .UNSPECIFIED., .F., .F.,
 ( 4, 2, 2, 4 ),
 ( 0.000000000000000000, 0.0002567066673176306157, 0.0005134133346352612315, 0.001026826669270521596 ),
 .UNSPECIFIED. ) ;
#140795 = CARTESIAN_POINT ( 'NONE',  ( 0.1469514510107531868, -1.837142584329341410, 1.370738489780512825 ) ) ;
#140794 = CARTESIAN_POINT ( 'NONE',  ( 8.188198428010544205, 8.517596018959260107, 0.000000000000000000 ) ) ;
#140796 = B_SPLINE_CURVE_WITH_KNOTS ( 'NONE', 3,
 ( #79431, #32817, #98891, #13357, #149772, #66343 ),
 .UNSPECIFIED., .F., .F.,
 ( 4, 2, 4 ),
 ( 0.000000000000000000, 0.0003258677429877279035, 0.0006517354859754558071 ),
 .UNSPECIFIED. ) ;
#140797 = CARTESIAN_POINT ( 'NONE',  ( 5.595603887632320195, -1.841320590885606068, 0.004091980732826016286 ) ) ;
#140798 = CARTESIAN_POINT ( 'NONE',  ( -3.436101866059630527, 6.096203712789787232, 1.199719254218462483 ) ) ;
#140799 = CARTESIAN_POINT ( 'NONE',  ( 0.7499999999999902300, 3.483333333333352044, 1.299038105676669330 ) ) ;
#140800 = CARTESIAN_POINT ( 'NONE',  ( 5.367185978643659539, 2.112682091867735146, -0.5819856738719306755 ) ) ;
#140801 = CARTESIAN_POINT ( 'NONE',  ( -3.867100128395853709, 5.534702787927018974, -1.599625672291256295 ) ) ;
#140802 = CARTESIAN_POINT ( 'NONE',  ( -3.505341441177800554, 15.51968381638693195, 11.48538216724446670 ) ) ;
#140803 = CARTESIAN_POINT ( 'NONE',  ( 5.934052368846653991, 1.230181698326970885, 1.665117723180092213 ) ) ;
#140804 = CARTESIAN_POINT ( 'NONE',  ( -11.89835103415199313, 9.771069141675340575, -1.561208891256348652 ) ) ;
#140805 = CARTESIAN_POINT ( 'NONE',  ( -0.6823417656249969321, 5.217708333674756283, -1.181850606188749264 ) ) ;
#140806 = CARTESIAN_POINT ( 'NONE',  ( 4.670489471188726149, -1.257041717089462773, 1.459967279689990960 ) ) ;
#140807 = CARTESIAN_POINT ( 'NONE',  ( -0.6823417656250003738, 9.901041667008065872, 1.181850606188754593 ) ) ;
#140808 = CARTESIAN_POINT ( 'NONE',  ( -2.318081078256692518, 5.648252324700675508, 1.040834085586084257E-14 ) ) ;
#140809 = CARTESIAN_POINT ( 'NONE',  ( 6.451439665316073935, -1.893653415279672902, 0.9546920624979161607 ) ) ;
#140811 = ORIENTED_EDGE ( 'NONE', *, *, #165849, .T. ) ;
#140810 = CARTESIAN_POINT ( 'NONE',  ( 4.065465959251388206, 5.836405933916976707, -1.599625672291269396 ) ) ;
#140812 = CARTESIAN_POINT ( 'NONE',  ( -4.828112100242303306, 4.805421336470338645, -0.7216878364870338292 ) ) ;
#140813 = CARTESIAN_POINT ( 'NONE',  ( 3.029357257649615054, 5.621668336311468117, -1.199719254218446718 ) ) ;
#140814 = CARTESIAN_POINT ( 'NONE',  ( 5.194182247366869731, 7.153241603385088965, 1.443375672974064550 ) ) ;
#140815 = CARTESIAN_POINT ( 'NONE',  ( 4.702146809683721784, 5.356480858934594025, 2.500000000000011102 ) ) ;
#140816 = CARTESIAN_POINT ( 'NONE',  ( 9.767704153745652818, 11.88520199868856331, 6.893175014280387813 ) ) ;
#140817 = CARTESIAN_POINT ( 'NONE',  ( 0.000000000000000000, -6.836568542494925182, 0.000000000000000000 ) ) ;
#140818 = CARTESIAN_POINT ( 'NONE',  ( 1.539427311113782837, 1.813978416018032558, -0.7477436361984082236 ) ) ;
#140819 = CARTESIAN_POINT ( 'NONE',  ( 0.6823417656249899377, 1.905208333674752952, 1.181850606188755259 ) ) ;
#140820 = EDGE_CURVE ( 'NONE', #47677, #11835, #105047, .T. ) ;
#140821 = CARTESIAN_POINT ( 'NONE',  ( -11.89942855770814134, 13.79999999999999893, -0.7000000000000009548 ) ) ;
#140822 = CARTESIAN_POINT ( 'NONE',  ( 5.687936657224680559, -1.243353266631580523, -1.517579924814119074 ) ) ;
#140823 = CARTESIAN_POINT ( 'NONE',  ( -8.076906825439122528, 10.44614393447756129, -1.599625672291263179 ) ) ;
#140824 = CARTESIAN_POINT ( 'NONE',  ( -5.599154252319524794, 6.595063384869953360, 1.082531754730546636 ) ) ;
#140825 = AXIS2_PLACEMENT_3D ( 'NONE', #100489, #153523, #38703 ) ;
#140826 = CARTESIAN_POINT ( 'NONE',  ( 0.5853300251711880398, -0.2802842603415867107, -2.245014038439311577 ) ) ;
#140828 = VERTEX_POINT ( 'NONE', #205954 ) ;
#140827 = CARTESIAN_POINT ( 'NONE',  ( -0.2106725631050281045, 2.870437361830021405, -2.492085498774513574 ) ) ;
#140829 = CARTESIAN_POINT ( 'NONE',  ( 0.7499999999999867883, -1.152083332650516434, -1.299038105676652011 ) ) ;
#140830 = CARTESIAN_POINT ( 'NONE',  ( 0.4560483712790652233, 0.7097975879313439540, 1.730851494400275747 ) ) ;
#140831 = CARTESIAN_POINT ( 'NONE',  ( 5.817694146727262705, -1.364776552785733399, 1.069276891063369650 ) ) ;
#140833 = CARTESIAN_POINT ( 'NONE',  ( 3.175498511859841333, 1.392037702009111033, 1.692654053968026151 ) ) ;
#140832 = CARTESIAN_POINT ( 'NONE',  ( -0.6801582343750282034, 1.432291667008027458, 1.178068619123810334 ) ) ;
#140834 = CARTESIAN_POINT ( 'NONE',  ( 4.524672722398297431, 1.423327999681742062, -1.816260527432728811 ) ) ;
#140835 = CARTESIAN_POINT ( 'NONE',  ( 0.6376604129620618844, -1.456937097490097255, -1.457867103223365213 ) ) ;
#140836 = CARTESIAN_POINT ( 'NONE',  ( 2.097507970028670510, -1.941522886764552203, 0.04780177728339052301 ) ) ;
#140837 = CARTESIAN_POINT ( 'NONE',  ( -5.734735788456164940, 5.792872629394710593, 0.7216878364870317197 ) ) ;
#140838 = EDGE_CURVE ( 'NONE', #40383, #163622, #71250, .T. ) ;
#140839 = CARTESIAN_POINT ( 'NONE',  ( 1.133562540163749688, 13.34197803161386453, -0.8395043811131129852 ) ) ;
#140840 = CARTESIAN_POINT ( 'NONE',  ( 4.676102344489991403, 2.097148071331572439, -0.3138259731317455392 ) ) ;
#140841 = CARTESIAN_POINT ( 'NONE',  ( -0.6801582343750334214, 0.1822916670080609869, 1.178068619123799898 ) ) ;
#140842 = CARTESIAN_POINT ( 'NONE',  ( 3.393204081532863459, -0.8197727808607684352, -1.842447475547980495 ) ) ;
#140843 = CARTESIAN_POINT ( 'NONE',  ( -5.883875478206491927, 5.966868934103426447, 0.000000000000000000 ) ) ;
#140844 = CARTESIAN_POINT ( 'NONE',  ( -7.445362632559989535, 8.715286488521982733, 1.199719254218452047 ) ) ;
#140845 = CARTESIAN_POINT ( 'NONE',  ( 10.09812548408005384, 10.67556790771522124, -0.7998128361456281477 ) ) ;
#140846 = CARTESIAN_POINT ( 'NONE',  ( 0.9436603434208358232, 0.7422609627109194586, -1.668170528445270140 ) ) ;
#140847 = CARTESIAN_POINT ( 'NONE',  ( -6.557303570864871034, 7.679217583210999010, -1.199719254218452047 ) ) ;
#140848 = CARTESIAN_POINT ( 'NONE',  ( -1.907519672996887294, 3.236073672982363369, 0.4612874649729363785 ) ) ;
#140849 = CARTESIAN_POINT ( 'NONE',  ( 1.512220381301902616, 8.756542408759468543, -2.494878041824251547 ) ) ;
#140850 = VERTEX_POINT ( 'NONE', #207019 ) ;
#140851 = CARTESIAN_POINT ( 'NONE',  ( 5.752824481226431530, -1.626044790292068498, 1.266090340377580947 ) ) ;
#140852 = CARTESIAN_POINT ( 'NONE',  ( -6.495764994278840021, 8.671754808115688107, 1.443375672974064550 ) ) ;
#140853 = DIRECTION ( 'NONE',  ( 0.5996521035822445223, -0.8002608041566132702, 0.000000000000000000 ) ) ;
#140854 = CARTESIAN_POINT ( 'NONE',  ( -4.939248034080176097, 4.656877549381960080, 1.214306433183764966E-14 ) ) ;
#140855 = CARTESIAN_POINT ( 'NONE',  ( -3.156015896931072540, 6.904045323053366268, 0.000000000000000000 ) ) ;
#140856 = CARTESIAN_POINT ( 'NONE',  ( 4.635418745873795210, -0.09682320349532060055, 2.017468490573450346 ) ) ;
#140857 = CARTESIAN_POINT ( 'NONE',  ( 5.338630837375411886, 1.324400161455315805, -1.783172940106398485 ) ) ;
#140859 = CARTESIAN_POINT ( 'NONE',  ( 8.378575743565351175, 11.75846021992619406, -1.082531754730543083 ) ) ;
#140858 = CARTESIAN_POINT ( 'NONE',  ( -5.915100157312088491, 10.12297696016459092, -0.7998128361456362523 ) ) ;
#140860 = CARTESIAN_POINT ( 'NONE',  ( 6.844168616800228477, 6.879284895888727824, -0.7998128361456281477 ) ) ;
#140861 = CARTESIAN_POINT ( 'NONE',  ( 3.678635468349491511, -1.985665955521208614, -0.5514216839303841544 ) ) ;
#140862 = CARTESIAN_POINT ( 'NONE',  ( 4.113907844847329187, 0.1017495355152969322, 2.013985960686740295 ) ) ;
#140863 = EDGE_LOOP ( 'NONE', ( #128163, #206431, #166464, #42683 ) ) ;
#140864 = CARTESIAN_POINT ( 'NONE',  ( 1.911175648939841265, 3.243131119507678850, -0.4542559028653492814 ) ) ;
#140865 = CARTESIAN_POINT ( 'NONE',  ( 3.734381245560244089, 6.444196322207211836, 1.199719254218462483 ) ) ;
#140866 = AXIS2_PLACEMENT_3D ( 'NONE', #212443, #182071, #48906 ) ;
#140868 = ORIENTED_EDGE ( 'NONE', *, *, #18861, .T. ) ;
#140867 = CARTESIAN_POINT ( 'NONE',  ( -6.257970421159510188, 9.458660037064859694, 1.199719254218452047 ) ) ;
#140869 = CARTESIAN_POINT ( 'NONE',  ( 5.631620320865258655, 7.357208097040313532, -1.234165276361798735 ) ) ;
#140870 = CARTESIAN_POINT ( 'NONE',  ( 4.464220131058834085, 1.617570847575640736, 1.203168917025834839 ) ) ;
#140871 = CARTESIAN_POINT ( 'NONE',  ( 2.290725937607818175, 1.422998120520948984, 1.168276728405498455 ) ) ;
#140872 = EDGE_CURVE ( 'NONE', #72330, #71109, #126709, .T. ) ;
#140873 = CARTESIAN_POINT ( 'NONE',  ( 1.489377799468382113, -0.3424701664414407931, -2.282033458877083199 ) ) ;
#140874 = CARTESIAN_POINT ( 'NONE',  ( 6.535912570239620578, 9.782925877658371405, 1.199719254218452047 ) ) ;
#140875 = CARTESIAN_POINT ( 'NONE',  ( 3.321700061091820366, -2.084211496276411779, 0.5730272365244913901 ) ) ;
#140876 = CARTESIAN_POINT ( 'NONE',  ( -5.117312914154178216, 8.057616602233474978, -1.199719254218452047 ) ) ;
#140877 = VERTEX_POINT ( 'NONE', #58650 ) ;
#140878 = CARTESIAN_POINT ( 'NONE',  ( -0.005973655271646400276, -7.189371949516665694, -9.500370076773238637 ) ) ;
#140879 = CARTESIAN_POINT ( 'NONE',  ( 1.867826558377215118, 0.9591755677602131769, 1.605880698980370225 ) ) ;
#140880 = CARTESIAN_POINT ( 'NONE',  ( 5.911001178172424986, 1.738356976118849984, 0.9299647631116741975 ) ) ;
#140883 = EDGE_CURVE ( 'NONE', #100853, #123093, #190763, .T. ) ;
#140882 = CARTESIAN_POINT ( 'NONE',  ( 9.205623113554624481, 10.80261038964432707, 1.082531754730549967 ) ) ;
#140881 = CARTESIAN_POINT ( 'NONE',  ( -1.364683531250010295, 4.030208333674751842, 0.7879004041258379498 ) ) ;
#140885 = CARTESIAN_POINT ( 'NONE',  ( 0.3818278861203865393, 2.057605126571937060, -0.7983354260262252033 ) ) ;
#140884 = CARTESIAN_POINT ( 'NONE',  ( -6.749261541504576911, 6.768559974710451677, 1.040834085586084257E-14 ) ) ;
#140886 = CARTESIAN_POINT ( 'NONE',  ( 1.734723475976807094E-15, 14.53394254119687012, 11.91973154060107376 ) ) ;
#140887 = CARTESIAN_POINT ( 'NONE',  ( 3.981290663907289140, 7.796589541200495965, -0.7998128361456221525 ) ) ;
#140888 = CARTESIAN_POINT ( 'NONE',  ( -4.062639585589296942, 7.891496616496157301, 0.7998128361456341429 ) ) ;
#140889 = AXIS2_PLACEMENT_3D ( 'NONE', #134380, #1115, #69310 ) ;
#140890 = CARTESIAN_POINT ( 'NONE',  ( 0.3000000000000016542, 3.322650755865477645, 0.5865692111442620815 ) ) ;
#140891 = CARTESIAN_POINT ( 'NONE',  ( 6.121945800013044447, -1.094813031782817303, -1.639340605029938835 ) ) ;
#140892 = EDGE_CURVE ( 'NONE', #132514, #63111, #160767, .T. ) ;
#140893 = CARTESIAN_POINT ( 'NONE',  ( 5.848310222665911162, 2.304730150483401463, 0.1192407711079427196 ) ) ;
#140894 = CARTESIAN_POINT ( 'NONE',  ( 5.881279174647062291, -0.04503291608629880066, 1.860690090596372137 ) ) ;
#140895 = CARTESIAN_POINT ( 'NONE',  ( 3.239185349552040183, -0.1472093337855179818, -2.057344904835652688 ) ) ;
#140896 = CARTESIAN_POINT ( 'NONE',  ( 5.775410249741494972, 8.721433810464993996, -1.082531754730537088 ) ) ;
#140897 = CARTESIAN_POINT ( 'NONE',  ( 8.018721507839716267, 8.319872945426633137, -0.7998128361456341429 ) ) ;
#140898 = CARTESIAN_POINT ( 'NONE',  ( 7.415946836550722843, 8.714654733139752807, 1.082531754730558626 ) ) ;
#140899 = CARTESIAN_POINT ( 'NONE',  ( 0.6823417656249899377, 3.738541667008085767, -1.181850606188754593 ) ) ;
#140900 = CARTESIAN_POINT ( 'NONE',  ( -11.04986227068298277, 12.49060002155663973, -1.056429153205399984 ) ) ;
#140901 = CARTESIAN_POINT ( 'NONE',  ( 4.636525345749193505, 8.353103970108639587, 1.040834085586084257E-14 ) ) ;
#140902 = CARTESIAN_POINT ( 'NONE',  ( 5.055217142685058285, 1.807878865648751221, -1.202052933306910765 ) ) ;
#140904 = CARTESIAN_POINT ( 'NONE',  ( 4.001369526190221571, -1.836035423186295201, 0.1395379388276704880 ) ) ;
#140903 = CARTESIAN_POINT ( 'NONE',  ( -3.226477370372317743, 4.787309570232886280, 1.443375672974064550 ) ) ;
#140905 = B_SPLINE_CURVE_WITH_KNOTS ( 'NONE', 3,
 ( #102192, #168259, #152020, #202863, #53435, #119573, #185559, #103263, #37187, #115312, #20910, #87004, #181302, #165060, #32930, #142195 ),
 .UNSPECIFIED., .F., .F.,
 ( 4, 2, 2, 2, 2, 2, 2, 4 ),
 ( -5.999999999627471727E-08, 0.001048291479606053029, 0.001572467219409077197, 0.002096642959212101365, 0.002620818699015125749, 0.003144994438818149267, 0.003669170178621173652, 0.004193345918424198036 ),
 .UNSPECIFIED. ) ;
#140907 = CARTESIAN_POINT ( 'NONE',  ( 11.89321938400731149, 12.33744721639322783, 1.599605898944313154 ) ) ;
#140906 = CARTESIAN_POINT ( 'NONE',  ( -9.871989323747691003, 3.235871879154613051, -6.146221223954435153 ) ) ;
#140908 = CARTESIAN_POINT ( 'NONE',  ( -10.97030319645364749, 11.30000000000000071, -1.695206765504804869 ) ) ;
#140909 = CARTESIAN_POINT ( 'NONE',  ( 0.8258823708265795593, -2.148021843699068789, 0.7105549608077809109 ) ) ;
#140910 = CARTESIAN_POINT ( 'NONE',  ( -3.985474048508588663, 7.835680043367737824, -0.2278754907324483936 ) ) ;
#140911 = CARTESIAN_POINT ( 'NONE',  ( -9.561191386655703894, -9.006862915010128035, 0.6000160562358372029 ) ) ;
#140912 = CARTESIAN_POINT ( 'NONE',  ( 5.901825473515108555, 7.257632781371366804, 1.250113620240392631 ) ) ;
#140913 = CARTESIAN_POINT ( 'NONE',  ( -4.841670253411603397, 5.781608396135871075, 1.082531754730549078 ) ) ;
#140914 = CARTESIAN_POINT ( 'NONE',  ( 0.4340482808194640607, -1.023182136338888659, -1.615339470012015166 ) ) ;
#140915 = CARTESIAN_POINT ( 'NONE',  ( 1.199668116878411128, -1.770032029468296964, -0.005122706785119778526 ) ) ;
#140916 = CARTESIAN_POINT ( 'NONE',  ( 5.795569859559966730, 1.859138327062941132, -0.7725605513991992135 ) ) ;
#140917 = CARTESIAN_POINT ( 'NONE',  ( 6.169123589417988995, 7.156064594864501416, -1.199719254218445830 ) ) ;
#140918 = CARTESIAN_POINT ( 'NONE',  ( 3.698352234880129874, -2.103465879664846216, -0.1051872838587295522 ) ) ;
#140920 = CARTESIAN_POINT ( 'NONE',  ( 3.040549542926245241, -1.448533627684518654, 1.253585735969472648 ) ) ;
#140919 = CARTESIAN_POINT ( 'NONE',  ( -2.765500147063310266, 6.170241238308400433, 1.040834085586084257E-14 ) ) ;
#140921 = DIRECTION ( 'NONE',  ( -5.578564026256490882E-16, -1.000000000000000000, -9.066213480720158442E-32 ) ) ;
#140922 = CARTESIAN_POINT ( 'NONE',  ( 4.246515029176777034, -1.947796394531702280, -0.2911330189915450339 ) ) ;
#140923 = CARTESIAN_POINT ( 'NONE',  ( 4.974870412032891487, -1.460018184141493647, 1.395898791055903976 ) ) ;
#140924 = CARTESIAN_POINT ( 'NONE',  ( 2.342468781959532453, 0.4075140148256419792, 1.825566309089213579 ) ) ;
#140926 = EDGE_LOOP ( 'NONE', ( #159299, #183617, #147480 ) ) ;
#140925 = CARTESIAN_POINT ( 'NONE',  ( 5.391107817497476695, 1.518517088589757424, -0.8181074574388611520 ) ) ;
#140928 = CARTESIAN_POINT ( 'NONE',  ( 3.660338286009610975, 6.253849852777763729, -1.082531754730543083 ) ) ;
#140927 = CARTESIAN_POINT ( 'NONE',  ( 2.561379550486083012, -1.920685204893451292, -1.086737900330703166 ) ) ;
#140929 = CARTESIAN_POINT ( 'NONE',  ( -1.364683531250012516, 2.842708333674754506, 0.7879004041258379498 ) ) ;
#140930 = CARTESIAN_POINT ( 'NONE',  ( 6.303176765056641706, -1.658072099422291057, 1.048360225930293321 ) ) ;
#140931 = CARTESIAN_POINT ( 'NONE',  ( 6.577677080924314801, 10.82570702772039262, 1.040834085586084257E-14 ) ) ;
#140932 = CARTESIAN_POINT ( 'NONE',  ( -10.34217224912604571, 10.96028913360221502, 0.7998128361456462443 ) ) ;
#140933 = CARTESIAN_POINT ( 'NONE',  ( 10.62873463776380056, 13.79999999999998295, 3.199999999999997957 ) ) ;
#140934 = CARTESIAN_POINT ( 'NONE',  ( -5.608178827873947725, 5.599964016548462986, -0.4038203069821116320 ) ) ;
#140935 = DIRECTION ( 'NONE',  ( 0.000000000000000000, 1.000000000000000000, 0.000000000000000000 ) ) ;
#140936 =( BOUNDED_SURFACE ( )  B_SPLINE_SURFACE ( 3, 2, ( 
 ( #96651, #164818, #212485 ),
 ( #94515, #181064, #130270 ),
 ( #44694, #196259, #31633 ),
 ( #47906, #114016, #97710 ),
 ( #16409, #163768, #32682 ),
 ( #148576, #127078, #110802 ) ),
 .UNSPECIFIED., .F., .F., .T. ) 
 B_SPLINE_SURFACE_WITH_KNOTS ( ( 4, 2, 4 ),
 ( 3, 3 ),
 ( 8.104322365866072748E-05, 0.0002156911409644568555, 0.0003503390582702529564 ),
 ( 0.000000000000000000, 1.000000000000000000 ),
 .UNSPECIFIED. ) 
 GEOMETRIC_REPRESENTATION_ITEM ( )  RATIONAL_B_SPLINE_SURFACE ( (
 ( 1.000000000000000000, 0.8104931255419008940, 1.000000000000000000),
 ( 1.000000000000000000, 0.8505897838743379236, 1.000000000000000000),
 ( 1.000000000000000000, 0.8859283899327281553, 1.000000000000000000),
 ( 1.000000000000000000, 0.9158911669206120099, 1.000000000000000000),
 ( 1.000000000000000000, 0.9074584363674400578, 1.000000000000000000),
 ( 1.000000000000000000, 0.8789000212885805796, 1.000000000000000000) ) ) 
 REPRESENTATION_ITEM ( '' )  SURFACE ( )  );
#140937 = VERTEX_POINT ( 'NONE', #143651 ) ;
#140938 = CARTESIAN_POINT ( 'NONE',  ( 2.453653613718423276, 1.598880132357576755, 1.315258840600006085 ) ) ;
#140939 = CARTESIAN_POINT ( 'NONE',  ( -1.201851678989727383E-14, 2.712500000000023892, 1.732050807568877637 ) ) ;
#140940 = CARTESIAN_POINT ( 'NONE',  ( 5.126954644262057492, 9.133197518281081173, 0.7998128361456462443 ) ) ;
#140941 = CARTESIAN_POINT ( 'NONE',  ( 3.553118775233146120, 6.302999783484076524, -1.199719254218453823 ) ) ;
#140942 = CARTESIAN_POINT ( 'NONE',  ( -0.04036499569192492781, -1.562578347245877630, -1.279382211958324689 ) ) ;
#140943 = CARTESIAN_POINT ( 'NONE',  ( 0.4019237886466816012, 10.45758545099816672, -1.499999999999998668 ) ) ;
#140944 = CARTESIAN_POINT ( 'NONE',  ( 0.6823417656249899377, 3.926041667008085767, -1.181850606188754593 ) ) ;
#140945 = EDGE_LOOP ( 'NONE', ( #192856, #193033, #206940 ) ) ;
#140947 = CARTESIAN_POINT ( 'NONE',  ( 9.327646496521982300, 11.90534021740758064, -1.443375672974057666 ) ) ;
#140946 = CARTESIAN_POINT ( 'NONE',  ( -1.500000000000015099, 11.72916666666666430, -0.8660254037844309360 ) ) ;
#140948 = CARTESIAN_POINT ( 'NONE',  ( 5.132185397524263060, 0.2004025303571632666, -2.006139158026089220 ) ) ;
#140949 = CARTESIAN_POINT ( 'NONE',  ( 5.313669575012682778, -1.220653882476211427, -1.476441452469556159 ) ) ;
#140950 = CARTESIAN_POINT ( 'NONE',  ( 6.639320575229294086, 0.002105643433562148347, 2.003388605011639179 ) ) ;
#140951 = CARTESIAN_POINT ( 'NONE',  ( 2.279091853667324141, 2.002311374866962979, -0.8913168663882904408 ) ) ;
#140952 = CARTESIAN_POINT ( 'NONE',  ( -2.788906526875773208E-15, 10.46875000068279604, -1.499999999999998446 ) ) ;
#140953 =( BOUNDED_CURVE ( )  B_SPLINE_CURVE ( 2, ( #30031, #141688, #108147, #28963, #193586, #158965, #74513, #58260, #93987 ),
 .UNSPECIFIED., .F., .T. ) 
 B_SPLINE_CURVE_WITH_KNOTS ( ( 3, 2, 2, 2, 3 ),
 ( 0.7053571428571427937, 0.7083333333333333703, 0.7142857142857143016, 0.7202380952380952328, 0.7232142857142856984 ),
 .UNSPECIFIED. ) 
 CURVE ( )  GEOMETRIC_REPRESENTATION_ITEM ( )  RATIONAL_B_SPLINE_CURVE ( ( 0.9330127018922194093, 0.9330127018922180770, 1.000000000000000000, 0.8660254037844387076, 1.000000000000000000, 0.8660254037844387076, 1.000000000000000000, 0.9330127018922194093, 0.9330127018922194093 ) ) 
 REPRESENTATION_ITEM ( '' )  );
#140955 = AXIS2_PLACEMENT_3D ( 'NONE', #202542, #27822, #11565 ) ;
#140954 = CARTESIAN_POINT ( 'NONE',  ( -1.402160292154681736E-14, 2.368750000682818602, -1.732050807568863648 ) ) ;
#140956 = CARTESIAN_POINT ( 'NONE',  ( 2.197387184563174944, 1.746976956643018219, -0.7784620831182070821 ) ) ;
#140957 = CARTESIAN_POINT ( 'NONE',  ( -6.230135280679522936, 7.227244901336242755, 1.199719254218450271 ) ) ;
#140959 = CARTESIAN_POINT ( 'NONE',  ( 0.2281389574181335589, 2.011207032379238591, 0.1455110067964115739 ) ) ;
#140958 = CARTESIAN_POINT ( 'NONE',  ( -4.311129659465605002, 4.131998812239033647, 0.7216878364870317197 ) ) ;
#140961 = EDGE_CURVE ( 'NONE', #207870, #21223, #164129, .T. ) ;
#140960 = CARTESIAN_POINT ( 'NONE',  ( -1.364683531250010295, 9.942708333674728394, 0.7879004041258445001 ) ) ;
#140963 = CARTESIAN_POINT ( 'NONE',  ( -5.284646014276622950, 9.387447126623207794, -0.7998128361456362523 ) ) ;
#140962 = CARTESIAN_POINT ( 'NONE',  ( 2.929326106026585830, -1.406127681732218360, -1.547418247020322601 ) ) ;
#140965 = ORIENTED_EDGE ( 'NONE', *, *, #11740, .F. ) ;
#140964 = CARTESIAN_POINT ( 'NONE',  ( 2.414726000362901637, 1.539333419754819854, 0.7781589270328890251 ) ) ;
#140966 = CARTESIAN_POINT ( 'NONE',  ( 6.258074605086497932, 0.8102346573028992305, -1.959903593942226907 ) ) ;
#140967 = CARTESIAN_POINT ( 'NONE',  ( 5.769158057814842699, 6.689438141327490150, 1.199719254218462483 ) ) ;
#140968 = CARTESIAN_POINT ( 'NONE',  ( -0.7027773505823969868, 13.37576698399828246, -1.183650206560545426 ) ) ;
#140969 = CARTESIAN_POINT ( 'NONE',  ( 0.6429252097494702056, -0.2364460082661112295, -1.947484529462916836 ) ) ;
#140970 =( BOUNDED_SURFACE ( )  B_SPLINE_SURFACE ( 3, 2, ( 
 ( #36643, #52900, #167722 ),
 ( #115832, #200197, #119034 ),
 ( #51850, #168784, #181818 ),
 ( #20389, #86473, #152537 ),
 ( #136304, #186092, #103801 ),
 ( #169850, #21438, #137375 ),
 ( #75560, #171998, #22513 ),
 ( #7333, #125459, #90763 ) ),
 .UNSPECIFIED., .F., .F., .F. ) 
 B_SPLINE_SURFACE_WITH_KNOTS ( ( 4, 2, 2, 4 ),
 ( 3, 3 ),
 ( 5.421010862427522170E-20, 0.0005123566476021758223, 0.0007685349714032637877, 0.001024713295204351645 ),
 ( 0.000000000000000000, 1.000000000000000000 ),
 .UNSPECIFIED. ) 
 GEOMETRIC_REPRESENTATION_ITEM ( )  RATIONAL_B_SPLINE_SURFACE ( (
 ( 1.000000000000000000, 0.7100530722026819896, 1.000000000000000000),
 ( 1.000000000000000000, 0.7667719522827127765, 1.000000000000000000),
 ( 1.000000000000000000, 0.8160440554223272747, 1.000000000000000000),
 ( 1.000000000000000000, 0.8737249316769533092, 1.000000000000000000),
 ( 1.000000000000000000, 0.8903164784318444713, 1.000000000000000000),
 ( 1.000000000000000000, 0.9150853305242792057, 1.000000000000000000),
 ( 1.000000000000000000, 0.9227739504731496956, 1.000000000000000000),
 ( 1.000000000000000000, 0.9238795325112855172, 1.000000000000000000) ) ) 
 REPRESENTATION_ITEM ( '' )  SURFACE ( )  );
#140971 = CARTESIAN_POINT ( 'NONE',  ( 0.000000000000000000, -4.500000000000003553, 0.000000000000000000 ) ) ;
#140972 = CARTESIAN_POINT ( 'NONE',  ( 5.656776405399742025, 7.622658444431597680, -1.599625672291262513 ) ) ;
#140973 = ORIENTED_EDGE ( 'NONE', *, *, #210859, .F. ) ;
#140974 = CARTESIAN_POINT ( 'NONE',  ( -11.80235830595198010, 13.79999999999999893, -1.696088231482795416 ) ) ;
#140975 = EDGE_LOOP ( 'NONE', ( #132778, #19595, #155052, #123518 ) ) ;
#140976 = CARTESIAN_POINT ( 'NONE',  ( 2.613665174717228368, -0.5667244042059360609, 1.720617414772870335 ) ) ;
#140977 = ORIENTED_EDGE ( 'NONE', *, *, #126509, .F. ) ;
#140978 = CARTESIAN_POINT ( 'NONE',  ( 8.920375002787457319, 12.49452237230570084, 1.199719254218450271 ) ) ;
#140979 = CARTESIAN_POINT ( 'NONE',  ( 4.224247379109608680, 7.085983154673295203, -1.199719254218452047 ) ) ;
#140980 = CARTESIAN_POINT ( 'NONE',  ( 4.072783076529101542, -1.339505953097392066, 1.219664821550008549 ) ) ;
#140981 = CARTESIAN_POINT ( 'NONE',  ( -4.769568550827871789, 5.176413985123565986, -0.9566739868914522216 ) ) ;
#140982 = CARTESIAN_POINT ( 'NONE',  ( -10.99873804690111356, -8.265528217051425486, 0.1803058380984418063 ) ) ;
#140983 = CARTESIAN_POINT ( 'NONE',  ( 5.616475580598488726, 6.148514233939430973, 0.8375902553012237739 ) ) ;
#140985 = CARTESIAN_POINT ( 'NONE',  ( 1.364683531250000303, 15.00520833367472839, -0.7879004041258355073 ) ) ;
#140984 = CARTESIAN_POINT ( 'NONE',  ( 4.088223475482699598, 0.9968510564385362205, -1.571365414726686227 ) ) ;
#140986 = EDGE_CURVE ( 'NONE', #132154, #161726, #64487, .T. ) ;
#140987 = CARTESIAN_POINT ( 'NONE',  ( 1.229944743773615956, 1.913488753162166045, 0.09234796458578581335 ) ) ;
#140988 = CARTESIAN_POINT ( 'NONE',  ( 0.7623938366894518204, -1.325735992016435105, 1.255310662410371370 ) ) ;
#140989 = CARTESIAN_POINT ( 'NONE',  ( 4.708566766960948335, 8.234178693335817201, 0.6429565889536159595 ) ) ;
#140990 = DIRECTION ( 'NONE',  ( 1.000000000000000000, 0.000000000000000000, 0.000000000000000000 ) ) ;
#140991 = B_SPLINE_CURVE_WITH_KNOTS ( 'NONE', 3,
 ( #152856, #203708, #170161, #55355, #187479, #86787, #6578, #171230, #53221, #87858 ),
 .UNSPECIFIED., .F., .F.,
 ( 4, 2, 2, 2, 4 ),
 ( 0.001366907522411799037, 0.001656827650609844034, 0.001946747778807889247, 0.002236667907005934243, 0.002526588035203979239 ),
 .UNSPECIFIED. ) ;
#140992 = CARTESIAN_POINT ( 'NONE',  ( 5.220047253295719614, 7.706380104734268599, 1.202949228536150938 ) ) ;
#140993 = CARTESIAN_POINT ( 'NONE',  ( 9.663580702207960726, 13.51594383518721365, 8.187698013202092895 ) ) ;
#140994 = DIRECTION ( 'NONE',  ( 0.000000000000000000, -1.000000000000000000, 0.000000000000000000 ) ) ;
#140995 = CARTESIAN_POINT ( 'NONE',  ( -4.181699849152211712, 3.976283482609832109, 0.4846375484205614481 ) ) ;
#140996 = CARTESIAN_POINT ( 'NONE',  ( 6.141480397310468575, 10.10888486359680982, 1.040834085586084257E-14 ) ) ;
#140997 = CARTESIAN_POINT ( 'NONE',  ( 5.401205523299864808, -1.691175329543142647, 1.008977833701154125 ) ) ;
#140998 = CARTESIAN_POINT ( 'NONE',  ( -4.762992037102518950, 4.451245552908022596, -0.7998128361456221525 ) ) ;
#140999 = CARTESIAN_POINT ( 'NONE',  ( 0.1280963075596490419, -1.331634228802502928, -1.703589906866372017 ) ) ;
#141000 = CARTESIAN_POINT ( 'NONE',  ( 0.8672654471616656480, 2.014311826519481929, -0.5594637955527237416 ) ) ;
#141001 = CARTESIAN_POINT ( 'NONE',  ( 6.422877973628248860, 1.797746274024723201, 0.6925914001822802701 ) ) ;
#141002 = CARTESIAN_POINT ( 'NONE',  ( -5.530836599371015794, 8.540060901653093950, 1.199719254218452047 ) ) ;
#141003 = ADVANCED_FACE ( 'NONE', ( #13592 ), #61287, .T. ) ;
#141004 = CARTESIAN_POINT ( 'NONE',  ( 1.852308540880560850, 0.5694407911355814367, 1.734573797025913189 ) ) ;
#141005 = CARTESIAN_POINT ( 'NONE',  ( 3.194164748978207680, -0.8942147705085048415, 2.017778291555922809 ) ) ;
#141006 = CARTESIAN_POINT ( 'NONE',  ( 1.499999999999993117, 9.885416667349465669, 0.8660254037844408170 ) ) ;
#141007 = CARTESIAN_POINT ( 'NONE',  ( 1.107505169401588274, 1.450017293480215352, 1.247013401884336403 ) ) ;
#141008 = CARTESIAN_POINT ( 'NONE',  ( 1.996483073472170133, 1.947676829468534265, 0.2919340086137369727 ) ) ;
#141009 = CARTESIAN_POINT ( 'NONE',  ( 2.489705217443307195, -1.937006489018164190, -0.1406711297040150188 ) ) ;
#141010 = VERTEX_POINT ( 'NONE', #196621 ) ;
#141011 = DIRECTION ( 'NONE',  ( 0.6716942845482061220, 0.000000000000000000, 0.7408284471490504952 ) ) ;
#141013 = CARTESIAN_POINT ( 'NONE',  ( 6.631710597105570315, 1.780986809720253694, -0.5397248755362458184 ) ) ;
#141012 = CARTESIAN_POINT ( 'NONE',  ( -5.490125858891038213, 5.369844688319787451, -0.7998128361456362523 ) ) ;
#141014 = CARTESIAN_POINT ( 'NONE',  ( 5.910428620914669473, 5.860197910680708944, 0.000000000000000000 ) ) ;
#141015 = DIRECTION ( 'NONE',  ( 0.000000000000000000, 1.000000000000000000, 0.000000000000000000 ) ) ;
#141016 = CARTESIAN_POINT ( 'NONE',  ( 4.028709946750490545, 3.988235255965033588, -0.8025987720412866011 ) ) ;
#141017 = CARTESIAN_POINT ( 'NONE',  ( -4.938913097128142304, 8.984092056616635347, -0.7998128361456362523 ) ) ;
#141018 = CARTESIAN_POINT ( 'NONE',  ( 2.630644284709309666, 0.2711686948545319886, 2.174668582101045633 ) ) ;
#141019 = PRESENTATION_STYLE_ASSIGNMENT (( #207027 ) ) ;
#141020 = CARTESIAN_POINT ( 'NONE',  ( 7.526711554241970248, 8.810193563817646734, -1.199719254218452047 ) ) ;
#141021 = DIRECTION ( 'NONE',  ( 1.561251128379126077E-17, 1.301042606982605475E-17, 1.000000000000000000 ) ) ;
#141022 = CARTESIAN_POINT ( 'NONE',  ( 2.754317325142870754, 0.6151756178996542479, 1.719052816137212503 ) ) ;
#141023 = CARTESIAN_POINT ( 'NONE',  ( -1.500000000000015099, 13.01041666734946567, -0.8660254037844309360 ) ) ;
#141024 = CARTESIAN_POINT ( 'NONE',  ( -10.15469386695561482, 10.94949038764413096, 1.040834085586084257E-14 ) ) ;
#141025 = TOROIDAL_SURFACE ( 'NONE', #9549, 11.92000000000000171, 0.08000000000000000167 ) ;
#141026 =( BOUNDED_SURFACE ( )  B_SPLINE_SURFACE ( 3, 2, ( 
 ( #49091, #128297, #181201 ),
 ( #11230, #143423, #77310 ),
 ( #61064, #193192, #94656 ),
 ( #44840, #110946, #176953 ),
 ( #33885, #102091, #186533 ),
 ( #150860, #202763, #66358 ),
 ( #287, #132504, #1360 ),
 ( #84773, #38162, #151918 ),
 ( #164958, #201695, #54413 ),
 ( #67422, #120554, #51215 ) ),
 .UNSPECIFIED., .F., .F., .T. ) 
 B_SPLINE_SURFACE_WITH_KNOTS ( ( 4, 2, 2, 2, 4 ),
 ( 3, 3 ),
 ( 0.000000000000000000, 0.0004557608768731892805, 0.0009115217537463785611, 0.001367282630619567896, 0.001823043507492757122 ),
 ( 0.000000000000000000, 1.000000000000000000 ),
 .UNSPECIFIED. ) 
 GEOMETRIC_REPRESENTATION_ITEM ( )  RATIONAL_B_SPLINE_SURFACE ( (
 ( 1.000000000000000000, 0.5626093260850774103, 1.000000000000000000),
 ( 1.000000000000000000, 0.5538465755378986222, 1.000000000000000000),
 ( 1.000000000000000000, 0.5614387302410062119, 1.000000000000000000),
 ( 1.000000000000000000, 0.6035072769098912548, 1.000000000000000000),
 ( 1.000000000000000000, 0.6388423421880006225, 1.000000000000000000),
 ( 1.000000000000000000, 0.7131546070456026287, 1.000000000000000000),
 ( 1.000000000000000000, 0.7507011191611827616, 1.000000000000000000),
 ( 1.000000000000000000, 0.8047563548239682341, 1.000000000000000000),
 ( 1.000000000000000000, 0.8208891226306104238, 1.000000000000000000),
 ( 1.000000000000000000, 0.8267197332297674395, 1.000000000000000000) ) ) 
 REPRESENTATION_ITEM ( '' )  SURFACE ( )  );
#141027 = CARTESIAN_POINT ( 'NONE',  ( -5.345048817422858534, 7.707963373851138833, -1.327269471787644317 ) ) ;
#141028 = CARTESIAN_POINT ( 'NONE',  ( -0.02968770228140016343, 0.2527710104786498047, -1.861515397111657144 ) ) ;
#141029 = CARTESIAN_POINT ( 'NONE',  ( 9.589694723567584234, 10.08239868711733855, -0.7998128361456281477 ) ) ;
#141030 = CARTESIAN_POINT ( 'NONE',  ( 0.9789820196765993687, -0.04640813864221354085, -1.926104504880983725 ) ) ;
#141031 = CARTESIAN_POINT ( 'NONE',  ( 5.453941704850034711, -0.7095916301838971485, 1.829088932523432964 ) ) ;
#141032 = TOROIDAL_SURFACE ( 'NONE', #12946, 0.8300000000000010703, 0.08000000000000000167 ) ;
#141033 = CARTESIAN_POINT ( 'NONE',  ( -1.500000000000001110, 14.52083333333333215, 0.8660254037844419273 ) ) ;
#141034 = CARTESIAN_POINT ( 'NONE',  ( -6.906989191158078079, 10.14557225873805812, -1.199719254218440723 ) ) ;
#141035 = CARTESIAN_POINT ( 'NONE',  ( 3.635557746758808495, 7.393234471193928847, -0.7998128361456291469 ) ) ;
#141036 = ADVANCED_FACE ( 'NONE', ( #147881 ), #48260, .F. ) ;
#141037 = CARTESIAN_POINT ( 'NONE',  ( -4.109529958273628658, 7.808552361378938045, 0.7216878364870338292 ) ) ;
#141038 = FACE_OUTER_BOUND ( 'NONE', #35304, .T. ) ;
#141039 = CARTESIAN_POINT ( 'NONE',  ( 5.067269747081383890, 1.798595138155817841, 1.025117745595036878 ) ) ;
#141041 = CARTESIAN_POINT ( 'NONE',  ( -1.201851678989727383E-14, 2.884375000341418804, 1.575800808251672791 ) ) ;
#141040 = DIRECTION ( 'NONE',  ( 0.000000000000000000, 0.000000000000000000, -1.000000000000000000 ) ) ;
#141042 = CARTESIAN_POINT ( 'NONE',  ( 4.817139702178411476, 1.183121084409150425, -1.970709701559998805 ) ) ;
#141043 = CARTESIAN_POINT ( 'NONE',  ( 7.131225611108100715, 7.422110755822004968, 0.7216878364870317197 ) ) ;
#141045 = CARTESIAN_POINT ( 'NONE',  ( 0.000000000000000000, 13.88000000000000078, 0.000000000000000000 ) ) ;
#141044 = CARTESIAN_POINT ( 'NONE',  ( 4.570507181582611267, 8.346359121906111511, 0.000000000000000000 ) ) ;
#141046 = CARTESIAN_POINT ( 'NONE',  ( 0.8852319118969053102, 2.019148884293726631, -1.085135299617467020 ) ) ;
#141047 = CARTESIAN_POINT ( 'NONE',  ( 7.721398836998350390, -5.907420853759296264, -7.721398836998385917 ) ) ;
#141048 = CIRCLE ( 'NONE', #47639, 0.07999999999999984901 ) ;
#141049 = CARTESIAN_POINT ( 'NONE',  ( -7.584860592202423035, 7.813701877183096833, -0.7998128361456362523 ) ) ;
#141050 = CARTESIAN_POINT ( 'NONE',  ( 4.382716955277085269, 1.733964400234957459, -0.8745241987923138005 ) ) ;
#141051 = ORIENTED_EDGE ( 'NONE', *, *, #213886, .F. ) ;
#141052 = CARTESIAN_POINT ( 'NONE',  ( 10.03267048398825168, 10.80712977418221676, 0.000000000000000000 ) ) ;
#141053 = ORIENTED_EDGE ( 'NONE', *, *, #147718, .T. ) ;
#141054 = CARTESIAN_POINT ( 'NONE',  ( 6.381121926128928479, -1.751337275642101510, -0.7685668267764720341 ) ) ;
#141055 = CARTESIAN_POINT ( 'NONE',  ( 6.827182134110228340, 0.006757161851634120239, 1.710856279483467191 ) ) ;
#141056 = CARTESIAN_POINT ( 'NONE',  ( 5.278529876733943915, -0.4946281652532490969, -1.954780475499573900 ) ) ;
#141058 = CARTESIAN_POINT ( 'NONE',  ( -4.665414256878304577, 5.575976400180357118, -1.082531754730549967 ) ) ;
#141057 = CARTESIAN_POINT ( 'NONE',  ( -9.124801077197171040, 10.60435499727357289, -1.199719254218441611 ) ) ;
#141059 = CARTESIAN_POINT ( 'NONE',  ( -1.642778471874998480, -1.888541666188708890, 2.845375778867863303 ) ) ;
#141061 = CARTESIAN_POINT ( 'NONE',  ( 6.661408102931688724, 0.2994711133218473931, -1.744046391327475964 ) ) ;
#141060 = CARTESIAN_POINT ( 'NONE',  ( 1.148509085094330029, -1.646982989033857869, 1.287593708729701802 ) ) ;
#141062 = CARTESIAN_POINT ( 'NONE',  ( 5.766250055133458119, 1.862018000461727052, -0.7743128548072516493 ) ) ;
#141064 = CARTESIAN_POINT ( 'NONE',  ( 3.099882009726143917, -2.289598904869084350, 0.1129434519280565069 ) ) ;
#141063 = CARTESIAN_POINT ( 'NONE',  ( 3.386504508363381571, 7.172948703057747011, -0.7998128361456362523 ) ) ;
#141065 = CARTESIAN_POINT ( 'NONE',  ( 1.939017046771335240, 0.6676067653633214194, -1.607389671016548949 ) ) ;
#141066 = CARTESIAN_POINT ( 'NONE',  ( 4.996790860652426159E-15, 0.6250000006827882704, 1.224999999999976330 ) ) ;
#141067 = CARTESIAN_POINT ( 'NONE',  ( 1.950155486560195772, 1.191851295230661467, 1.259505011191792923 ) ) ;
#141068 = CARTESIAN_POINT ( 'NONE',  ( -0.6801582343750438575, 1.630208333674734611, -1.178068619123879834 ) ) ;
#141069 = CARTESIAN_POINT ( 'NONE',  ( 1.890827768869116632, 0.1781016032055370568, 1.852494144255438346 ) ) ;
#141070 = CARTESIAN_POINT ( 'NONE',  ( 2.137404458564879484, -0.1051889750803415707, -2.168730265314787076 ) ) ;
#141071 = CARTESIAN_POINT ( 'NONE',  ( 3.362517798112668821, -1.944730434982215650, -0.5331690889110105580 ) ) ;
#141072 = CARTESIAN_POINT ( 'NONE',  ( 4.000000000000002665, -2.278188019141646974E-13, -2.052068128417946280 ) ) ;
#141073 = CARTESIAN_POINT ( 'NONE',  ( -1.201851678989727383E-14, 2.493750000682819046, 1.732050807568877637 ) ) ;
#141074 = CARTESIAN_POINT ( 'NONE',  ( 0.7977241263109683400, -0.6962278615636787737, 1.796346399320443821 ) ) ;
#141075 = CARTESIAN_POINT ( 'NONE',  ( 1.364683531249997417, 14.23437500034140157, 2.602085213965210642E-15 ) ) ;
#141076 = CARTESIAN_POINT ( 'NONE',  ( 3.586370468055916305, 1.236567345028506182, 1.845233891176313756 ) ) ;
#141077 = ORIENTED_EDGE ( 'NONE', *, *, #61168, .T. ) ;
#141078 = CARTESIAN_POINT ( 'NONE',  ( -0.2108831679770926115, 5.723481173670196043, -2.491210874135452613 ) ) ;
#141079 = CARTESIAN_POINT ( 'NONE',  ( -0.7500000000000215383, 0.6916666666666876351, 1.299038105676659116 ) ) ;
#141080 = CARTESIAN_POINT ( 'NONE',  ( 7.450369105909416589, 8.650851030771185890, -1.199719254218441611 ) ) ;
#141081 = CARTESIAN_POINT ( 'NONE',  ( -1.364683531250014514, 0.2802083336747505649, 0.7879004041258379498 ) ) ;
#141082 = CARTESIAN_POINT ( 'NONE',  ( 6.275645185405086757, 0.3810096023663198661, -2.188332947720336819 ) ) ;
#141083 = CARTESIAN_POINT ( 'NONE',  ( 4.721123852359588646, -1.751549048416237486, -0.8839179009662299080 ) ) ;
#141085 = CARTESIAN_POINT ( 'NONE',  ( -5.260200412422196159, 9.080724881227137502, -0.7216878364870207285 ) ) ;
#141084 = CARTESIAN_POINT ( 'NONE',  ( 8.839552966430002101, 11.33589776563360019, -1.443375672974052559 ) ) ;
#141086 = CYLINDRICAL_SURFACE ( 'NONE', #211641, 0.3999999999999993006 ) ;
#141087 = CARTESIAN_POINT ( 'NONE',  ( 5.290393965937395748, -2.244422280358076005, -0.2844362755431028567 ) ) ;
#141088 = CARTESIAN_POINT ( 'NONE',  ( -5.139949633356594383, 9.010708648975750634, 0.000000000000000000 ) ) ;
#141089 = CARTESIAN_POINT ( 'NONE',  ( 2.611848684353266226, 0.5523815846302374544, -1.987258587729407999 ) ) ;
#141090 = CARTESIAN_POINT ( 'NONE',  ( -6.878064000834399394, 6.918829510595249310, -0.7998128361456291469 ) ) ;
#141091 = EDGE_LOOP ( 'NONE', ( #117974, #54522, #160529, #28871, #31426, #65660, #145345, #194195 ) ) ;
#141092 = CARTESIAN_POINT ( 'NONE',  ( 0.7499999999999902300, 2.764583334016148974, 1.299038105676669330 ) ) ;
#141093 = CARTESIAN_POINT ( 'NONE',  ( -1.201851678989727383E-14, 3.884375000341423689, 1.575800808251672791 ) ) ;
#141094 = CARTESIAN_POINT ( 'NONE',  ( 4.991395955090764502, 1.385047395102714685, 1.257364466828891914 ) ) ;
#141095 = CARTESIAN_POINT ( 'NONE',  ( 3.111645937125429029, 0.04567828748044086562, 1.733733899787115229 ) ) ;
#141096 = CARTESIAN_POINT ( 'NONE',  ( 2.454330514505886018, -1.515118085899306521, -0.8562798468515414596 ) ) ;
#141097 = CARTESIAN_POINT ( 'NONE',  ( 0.8203738007961014489, 1.359819376615223785, -1.845384199244608947 ) ) ;
#141098 = CARTESIAN_POINT ( 'NONE',  ( 0.6752036787147744912, -2.078553970830565145, -0.7415856106591719454 ) ) ;
#141099 = CARTESIAN_POINT ( 'NONE',  ( 4.862875367868015886, 0.2033134212856284595, -2.080814050062954390 ) ) ;
#141100 = CARTESIAN_POINT ( 'NONE',  ( 5.859312505936116189, 1.912822604199882148, -0.3342364482464658115 ) ) ;
#141101 = EDGE_CURVE ( 'NONE', #2638, #59934, #74845, .T. ) ;
#141103 = ORIENTED_EDGE ( 'NONE', *, *, #43875, .F. ) ;
#141102 = CARTESIAN_POINT ( 'NONE',  ( 7.895893545578077877, 15.33679876036382694, 9.037963944523932369 ) ) ;
#141104 = FILL_AREA_STYLE_COLOUR ( '', #10558 ) ;
#141105 = CARTESIAN_POINT ( 'NONE',  ( 0.6158615555539399544, 0.1511424999406512648, 2.010826230049263863 ) ) ;
#141106 = PLANE ( 'NONE',  #82833 ) ;
#141107 = CARTESIAN_POINT ( 'NONE',  ( 0.000000000000000000, 3.481548657788669843, 0.000000000000000000 ) ) ;
#141108 = CARTESIAN_POINT ( 'NONE',  ( 0.000000000000000000, 2.999999999999999112, 0.000000000000000000 ) ) ;
#141109 = CARTESIAN_POINT ( 'NONE',  ( -9.515124878692420296, 9.995400534762978850, 1.040834085586084257E-14 ) ) ;
#141110 = CARTESIAN_POINT ( 'NONE',  ( 6.283314124929436417, 9.417951348137970413, -1.199719254218440723 ) ) ;
#141111 = SURFACE_STYLE_USAGE ( .BOTH. , #90200 ) ;
#141112 = CARTESIAN_POINT ( 'NONE',  ( 3.984828715814022981, -0.1808549858164226476, -1.816707794649790708 ) ) ;
#141113 = CARTESIAN_POINT ( 'NONE',  ( 1.641937377912294771, -1.598774535768614280, -1.521335986861327427 ) ) ;
#141114 = ORIENTED_EDGE ( 'NONE', *, *, #136635, .T. ) ;
#141115 = CARTESIAN_POINT ( 'NONE',  ( -3.323157048681004699, 6.891117300187535655, -0.7216878364870458196 ) ) ;
#141116 = CARTESIAN_POINT ( 'NONE',  ( -1.642778471875000035, -2.705208332855375986, -2.845375778867859751 ) ) ;
#141117 = CARTESIAN_POINT ( 'NONE',  ( -7.483210719738908168, 10.81783070874899799, 1.199719254218453823 ) ) ;
#141118 = CARTESIAN_POINT ( 'NONE',  ( 0.7033857886646873725, 1.779361102145039286, -0.9557781530431900263 ) ) ;
#141119 = CARTESIAN_POINT ( 'NONE',  ( -9.898321827454534372, 14.00000000001253930, -7.924999999986504839 ) ) ;
#141120 = ORIENTED_EDGE ( 'NONE', *, *, #145267, .F. ) ;
#141121 = CARTESIAN_POINT ( 'NONE',  ( -4.472210567661380587, 6.310941310395290493, 1.599625672291270506 ) ) ;
#141122 = CARTESIAN_POINT ( 'NONE',  ( 2.483057756668010541, -0.005615179255674587061, 1.861131632832468963 ) ) ;
#141123 = CARTESIAN_POINT ( 'NONE',  ( 4.390142812726693045, 4.016254791136236513, 1.214306433183764966E-14 ) ) ;
#141124 = CARTESIAN_POINT ( 'NONE',  ( 1.464677571780234644E-15, 19.00000000000000000, -11.92000000000000171 ) ) ;
#141125 = ORIENTED_EDGE ( 'NONE', *, *, #50663, .F. ) ;
#141126 = ORIENTED_EDGE ( 'NONE', *, *, #49103, .T. ) ;
#141127 = CARTESIAN_POINT ( 'NONE',  ( -4.985647801523292344, 6.839675073242382553, -1.599625672291256295 ) ) ;
#141128 = CARTESIAN_POINT ( 'NONE',  ( -9.657485491635913633, 10.16148791653038330, 1.040834085586084257E-14 ) ) ;
#141129 = CARTESIAN_POINT ( 'NONE',  ( 3.545350327189537687, -1.383302465072188792, -1.191577590537174158 ) ) ;
#141130 = AXIS2_PLACEMENT_3D ( 'NONE', #145287, #28291, #130144 ) ;
#141133 = ORIENTED_EDGE ( 'NONE', *, *, #26463, .F. ) ;
#141132 = CARTESIAN_POINT ( 'NONE',  ( -5.732732414299474222, 6.256854150074313559, -1.080652830874342163 ) ) ;
#141131 = CARTESIAN_POINT ( 'NONE',  ( -3.817502770699643388, 6.611447778194983194, 1.199719254218452935 ) ) ;
#141134 = CARTESIAN_POINT ( 'NONE',  ( 6.580239226864286195, 6.782991656975736028, -0.2881480849740332140 ) ) ;
#141135 = CARTESIAN_POINT ( 'NONE',  ( 0.4558326304775248139, 1.278721518017480685, 1.171137906463788347 ) ) ;
#141136 = CARTESIAN_POINT ( 'NONE',  ( 5.384640740818634974, 1.621930891500168670, -0.8712783443201177480 ) ) ;
#141137 = CARTESIAN_POINT ( 'NONE',  ( 4.969473931871945638, 0.2302171888925855225, -2.296178194122914018 ) ) ;
#141138 = CARTESIAN_POINT ( 'NONE',  ( 5.876533236880477240, 5.820653295974182129, 0.7998128361456352531 ) ) ;
#141139 = CARTESIAN_POINT ( 'NONE',  ( 6.573507624224045109, 2.070638407997299257, -0.6205318887850322929 ) ) ;
#141140 = CARTESIAN_POINT ( 'NONE',  ( 5.849453209292126310, 8.911780279894442103, 1.199719254218462483 ) ) ;
#141141 = CARTESIAN_POINT ( 'NONE',  ( 5.325646502758397460, -1.669998024346308618, 1.579374382026963675 ) ) ;
#141142 = CARTESIAN_POINT ( 'NONE',  ( -7.425025402139490360, 8.691559719698066289, 1.199719254218452047 ) ) ;
#141143 = CARTESIAN_POINT ( 'NONE',  ( 5.682452175617663137, -1.825344843996518529, -0.4084625512627630406 ) ) ;
#141144 = ORIENTED_EDGE ( 'NONE', *, *, #5382, .T. ) ;
#141146 = CIRCLE ( 'NONE', #196446, 11.92000000000000171 ) ;
#141145 = CIRCLE ( 'NONE', #110087, 0.09999999999999986677 ) ;
#141149 = EDGE_CURVE ( 'NONE', #80197, #127597, #27528, .T. ) ;
#141148 = CARTESIAN_POINT ( 'NONE',  ( -4.339491684825780737, 7.220434844675483355, -1.199719254218455378 ) ) ;
#141147 = CARTESIAN_POINT ( 'NONE',  ( 2.302860652515530848, -0.3306829512400177862, -1.883434002855538081 ) ) ;
#141150 = CARTESIAN_POINT ( 'NONE',  ( 4.248781725523794073, 0.5872999373685274804, 2.127227798101683387 ) ) ;
#141151 = CARTESIAN_POINT ( 'NONE',  ( 4.628176351164477786, 2.111873176223429738, 0.1524955421974716341 ) ) ;
#141152 = CARTESIAN_POINT ( 'NONE',  ( 1.224999999999969225, 0.6875000006828015930, -3.642919299551294898E-14 ) ) ;
#141153 = CARTESIAN_POINT ( 'NONE',  ( 6.883263157960364254, 6.036844454314826081, 2.541088405340941492 ) ) ;
#141154 = CARTESIAN_POINT ( 'NONE',  ( -0.2110808730066960626, 4.094899759311981136, -2.352064028521171135 ) ) ;
#141155 = CARTESIAN_POINT ( 'NONE',  ( 5.844973620822844218, 6.952128991449046502, 1.082531754730549967 ) ) ;
#141156 = CARTESIAN_POINT ( 'NONE',  ( -5.600926855776894975, 6.667407765562058053, -1.082531754730549967 ) ) ;
#141157 = EDGE_CURVE ( 'NONE', #93347, #84679, #161818, .T. ) ;
#141158 = CARTESIAN_POINT ( 'NONE',  ( 2.538448204128932240, 1.088115672400795431, -2.034946615453626872 ) ) ;
#141159 = CARTESIAN_POINT ( 'NONE',  ( 3.121486724888074882, 0.2905151309811822569, -1.940125473959073421 ) ) ;
#141160 = CARTESIAN_POINT ( 'NONE',  ( 6.737180511075488987, -0.09540316190201691970, -2.060463472160603882 ) ) ;
#141161 = CARTESIAN_POINT ( 'NONE',  ( 3.226477370372302644, 5.747678784534228313, 1.082531754730546636 ) ) ;
#141162 = CARTESIAN_POINT ( 'NONE',  ( 4.903208829997618423, 5.749440385532527564, -1.199719254218450271 ) ) ;
#141163 = ORIENTED_EDGE ( 'NONE', *, *, #28627, .T. ) ;
#141164 = CARTESIAN_POINT ( 'NONE',  ( 4.874232570624013050, -2.001857581374043349, -0.2420344392276354561 ) ) ;
#141165 = CARTESIAN_POINT ( 'NONE',  ( -8.890396042259075315, 11.39521468743417998, -1.599625672291263179 ) ) ;
#141166 = CARTESIAN_POINT ( 'NONE',  ( -10.47476534206535170, 5.237283261923990629, -5.169982392003922733 ) ) ;
#141167 = CARTESIAN_POINT ( 'NONE',  ( 8.503988664269582998, 10.94440607977979063, 1.599625672291281386 ) ) ;
#141168 = CARTESIAN_POINT ( 'NONE',  ( 1.481551236908748237, -0.05589941666775917473, 2.170521761658677828 ) ) ;
#141169 = CARTESIAN_POINT ( 'NONE',  ( 3.284841267552055299, 6.405332120898776793, -0.9495590844852130896 ) ) ;
#141170 = CARTESIAN_POINT ( 'NONE',  ( -5.973438521925780620, 14.55272270109815835, -10.36619016570325869 ) ) ;
#141171 = CARTESIAN_POINT ( 'NONE',  ( 5.184698244283005408, 7.856242361780820360, 1.254847465626233616 ) ) ;
#141172 = CARTESIAN_POINT ( 'NONE',  ( 0.9661734561289528900, 1.013198095218909245, 1.794397040888571437 ) ) ;
#141174 = CARTESIAN_POINT ( 'NONE',  ( -2.788906526875773208E-15, 8.468750000682796042, -1.499999999999998446 ) ) ;
#141173 = DIRECTION ( 'NONE',  ( 1.000000000000000000, 0.000000000000000000, 0.000000000000000000 ) ) ;
#141175 = CARTESIAN_POINT ( 'NONE',  ( -1.402160292154681736E-14, 0.6968750003414164729, -1.575800808251659024 ) ) ;
#141176 = DIRECTION ( 'NONE',  ( -0.7592566023653016805, -0.6507913734559627184, 4.115938288792108699E-15 ) ) ;
#141177 = EDGE_LOOP ( 'NONE', ( #111331, #37560, #168276, #150800, #3351 ) ) ;
#141178 = CARTESIAN_POINT ( 'NONE',  ( 3.088426618631805010, -1.137173348016347063, 1.537276688398481861 ) ) ;
#141179 =( GEOMETRIC_REPRESENTATION_CONTEXT ( 3 ) GLOBAL_UNCERTAINTY_ASSIGNED_CONTEXT ( ( #189810 ) ) GLOBAL_UNIT_ASSIGNED_CONTEXT ( ( #31192, #44251, #207788 ) ) REPRESENTATION_CONTEXT ( 'NONE', 'WORKASPACE' ) );
#141180 = CARTESIAN_POINT ( 'NONE',  ( 4.821055670345097077, -0.08498437303107277130, 1.767940285534306488 ) ) ;
#141181 = CARTESIAN_POINT ( 'NONE',  ( 6.550524494058025837, 7.671308660269694712, -1.199719254218452047 ) ) ;
#141182 = CARTESIAN_POINT ( 'NONE',  ( -4.939248034080176097, 4.656877549381960080, 1.214306433183764966E-14 ) ) ;
#141184 = CARTESIAN_POINT ( 'NONE',  ( -0.08300117844089061059, -1.750507139949438296, 0.7787328797612643738 ) ) ;
#141183 = DIRECTION ( 'NONE',  ( 0.000000000000000000, -1.000000000000000000, 0.000000000000000000 ) ) ;
#141185 = CARTESIAN_POINT ( 'NONE',  ( -1.402160292154681736E-14, 0.3375000000000208389, -1.732050807568870754 ) ) ;
#141186 = CARTESIAN_POINT ( 'NONE',  ( 0.8364851226981102617, -1.151554295457988930, 1.720357586142134076 ) ) ;
#141187 = CARTESIAN_POINT ( 'NONE',  ( 1.364683531249984538, -1.032291666325247714, -0.7879004041258309554 ) ) ;
#141188 = CARTESIAN_POINT ( 'NONE',  ( 6.192256348250350761, -1.861847689568534081, -0.1814220289034565448 ) ) ;
#141189 = CARTESIAN_POINT ( 'NONE',  ( 1.980809073483770000, -0.08854697198140694392, -1.823669195971427071 ) ) ;
#141191 = CARTESIAN_POINT ( 'NONE',  ( 4.798147134389644464, 8.131168186839138556, 0.8272934513729796047 ) ) ;
#141190 = CARTESIAN_POINT ( 'NONE',  ( 5.408869034151480903, 1.673104959687292448, -1.439203791633147267 ) ) ;
#141192 = CARTESIAN_POINT ( 'NONE',  ( 0.6823417656249899377, 0.5927083336747518416, 1.181850606188755259 ) ) ;
#141193 = CARTESIAN_POINT ( 'NONE',  ( 3.191897189531978096, -1.383228714077057830, -1.530316362279722231 ) ) ;
#141194 = CARTESIAN_POINT ( 'NONE',  ( -7.497822643557261024, 8.706213491360317747, -1.199719254218446718 ) ) ;
#141195 = CARTESIAN_POINT ( 'NONE',  ( 7.391166297744269365, 11.77477778067701664, 1.040834085586084257E-14 ) ) ;
#141196 = CARTESIAN_POINT ( 'NONE',  ( 3.683011284406639163, 7.448596931783069586, 0.7998128361456321445 ) ) ;
#141197 = CARTESIAN_POINT ( 'NONE',  ( 0.1811626231076196580, -0.1537715369321658587, -2.127283700313627346 ) ) ;
#141198 = CARTESIAN_POINT ( 'NONE',  ( 5.332099551924443404, 9.442809587212341427, 0.000000000000000000 ) ) ;
#141199 = CARTESIAN_POINT ( 'NONE',  ( 5.318829906782316819, -1.502041817331278173, 1.425132596443792643 ) ) ;
#141200 = CARTESIAN_POINT ( 'NONE',  ( 1.364683531249988757, 0.1968750003414204697, 0.000000000000000000 ) ) ;
#141201 = CARTESIAN_POINT ( 'NONE',  ( 2.706508253401081809, -0.8245430293080566742, -1.998349536214229616 ) ) ;
#141202 = CARTESIAN_POINT ( 'NONE',  ( -4.929275754869433257, 8.007250896656138650, 0.9949873637682864480 ) ) ;
#141204 = CARTESIAN_POINT ( 'NONE',  ( 1.803102349535959714, -1.659081995624330563, 1.046767247423967095 ) ) ;
#141203 = CARTESIAN_POINT ( 'NONE',  ( 3.229170203573806130, 1.826861024573895653, 0.8614713780644381869 ) ) ;
#141205 = CARTESIAN_POINT ( 'NONE',  ( -1.580000000000022276, 8.674529973577531194, 2.500000000000011102 ) ) ;
#141208 = CARTESIAN_POINT ( 'NONE',  ( 5.802526556968819804, 9.713438716531550554, -0.7216878364870267237 ) ) ;
#141207 = CARTESIAN_POINT ( 'NONE',  ( 1.737500000000001155, -0.5833333333333314830, 3.009438278150922130 ) ) ;
#141206 = FILL_AREA_STYLE ('',( #114847 ) ) ;
#141209 = CARTESIAN_POINT ( 'NONE',  ( -5.257529707049291900, 9.355811434857983500, 0.7998128361456291469 ) ) ;
#141210 = CARTESIAN_POINT ( 'NONE',  ( 0.8312679839070147292, -1.592664559859976237, -1.236796411087807801 ) ) ;
#141212 = CARTESIAN_POINT ( 'NONE',  ( 6.585463931165095985, -0.9389328202267492873, 1.978239266594773671 ) ) ;
#141211 = CARTESIAN_POINT ( 'NONE',  ( -4.446184310277715213, 7.274633231044262516, -1.199719254218452047 ) ) ;
#141213 =( BOUNDED_CURVE ( )  B_SPLINE_CURVE ( 2, ( #206250, #190004, #104505, #137003, #57876, #8045, #22133, #88246, #41654 ),
 .UNSPECIFIED., .F., .T. ) 
 B_SPLINE_CURVE_WITH_KNOTS ( ( 3, 2, 2, 2, 3 ),
 ( 0.1718749999999998335, 0.1770833333333333426, 0.1875000000000000000, 0.1979166666666666574, 0.2031250000000001388 ),
 .UNSPECIFIED. ) 
 CURVE ( )  GEOMETRIC_REPRESENTATION_ITEM ( )  RATIONAL_B_SPLINE_CURVE ( ( 0.9330127018922194093, 0.9330127018922171889, 1.000000000000000000, 0.8660254037844387076, 1.000000000000000000, 0.8660254037844387076, 1.000000000000000000, 0.9330127018922176330, 0.9330127018922194093 ) ) 
 REPRESENTATION_ITEM ( '' )  );
#141214 = CARTESIAN_POINT ( 'NONE',  ( 1.224646799147353059E-15, 6.999999999999999112, 9.999999999999998224 ) ) ;
#141215 = CARTESIAN_POINT ( 'NONE',  ( 6.082274476537278041, 0.9889857280602430967, 1.636697341158253272 ) ) ;
#141216 = CARTESIAN_POINT ( 'NONE',  ( -3.735435015764967837, 4.316761258935923884, -1.199719254218452047 ) ) ;
#141217 = B_SPLINE_CURVE_WITH_KNOTS ( 'NONE', 3,
 ( #140769, #208903, #75729, #192656 ),
 .UNSPECIFIED., .F., .F.,
 ( 4, 4 ),
 ( 0.000000000000000000, 0.0002445738358484001417 ),
 .UNSPECIFIED. ) ;
#141219 = CARTESIAN_POINT ( 'NONE',  ( 2.829704019156009220, 0.7231233381281775285, -1.882481713119791067 ) ) ;
#141218 = CARTESIAN_POINT ( 'NONE',  ( -6.995644074527074707, 11.10540915368285475, 0.000000000000000000 ) ) ;
#141220 = CARTESIAN_POINT ( 'NONE',  ( 1.499999999999987121, 3.795833333333356929, -0.8660254037844262731 ) ) ;
#141221 = CARTESIAN_POINT ( 'NONE',  ( 1.364683531249996529, 14.02604166700806942, 0.7879004041258405033 ) ) ;
#141222 = AXIS2_PLACEMENT_3D ( 'NONE', #134335, #33596, #118116 ) ;
#141223 = CARTESIAN_POINT ( 'NONE',  ( 6.176716277887216222, -1.639393978788429740, -0.5360894954027517478 ) ) ;
#141224 = CARTESIAN_POINT ( 'NONE',  ( 6.282224075085741433, 8.422623735723785643, 1.599625672291268286 ) ) ;
#141225 = CARTESIAN_POINT ( 'NONE',  ( 8.514157279702022407, 10.95626946445095307, -1.443375672974063439 ) ) ;
#141226 = CARTESIAN_POINT ( 'NONE',  ( -0.4000000000000343836, 3.372708439410141867, 0.4999999999999770184 ) ) ;
#141227 = CARTESIAN_POINT ( 'NONE',  ( 4.657402308249613654, 0.4116239899518738810, -1.824517662812553009 ) ) ;
#141228 = CARTESIAN_POINT ( 'NONE',  ( -5.608757509019071108, 5.629766575892905855, -0.3787719694710602325 ) ) ;
#141229 = CARTESIAN_POINT ( 'NONE',  ( 1.428671948192638208, -1.316369429293560156, 1.597808059233512656 ) ) ;
#141230 = CARTESIAN_POINT ( 'NONE',  ( -6.902509602688818191, 9.146290184594002781, -1.443375672974066548 ) ) ;
#141231 = CARTESIAN_POINT ( 'NONE',  ( 4.390861645979372341, 6.216034235099629157, -1.599625672291269396 ) ) ;
#141232 = CARTESIAN_POINT ( 'NONE',  ( 11.07790593930098311, 9.799999999999998934, 0.6999999999999992895 ) ) ;
#141233 = CARTESIAN_POINT ( 'NONE',  ( 0.07017708175168728413, 0.6932349927748741036, 1.673895389460538397 ) ) ;
#141234 = CARTESIAN_POINT ( 'NONE',  ( 6.034787771414195312, 6.213209619504250547, -0.7216878364870458196 ) ) ;
#141235 = CIRCLE ( 'NONE', #61550, 0.7499999999999997780 ) ;
#141236 = DIRECTION ( 'NONE',  ( 1.000000000000000000, -0.000000000000000000, -0.000000000000000000 ) ) ;
#141237 = ORIENTED_EDGE ( 'NONE', *, *, #99278, .T. ) ;
#141238 = CARTESIAN_POINT ( 'NONE',  ( 7.388830529323379359, 11.56412668427855195, -0.7216878364870267237 ) ) ;
#141240 = CARTESIAN_POINT ( 'NONE',  ( 8.076906825439115423, 10.44614393447756129, -1.599625672291262513 ) ) ;
#141239 = CARTESIAN_POINT ( 'NONE',  ( 1.627322669196319849, 0.1476378700930695564, -1.956383933670035713 ) ) ;
#141241 = CARTESIAN_POINT ( 'NONE',  ( 4.886306726311728355, -0.6496138446146214607, -1.802220356481977204 ) ) ;
#141242 = CARTESIAN_POINT ( 'NONE',  ( -3.578989363883261277, 7.119311991265024453, 1.040834085586084257E-14 ) ) ;
#141243 = CARTESIAN_POINT ( 'NONE',  ( 8.550388431712704573, 13.12720360364021133, 0.000000000000000000 ) ) ;
#141244 = CARTESIAN_POINT ( 'NONE',  ( 2.324088772396477673E-16, 0.6875000000000069944, -1.225000000000008749 ) ) ;
#141246 = EDGE_LOOP ( 'NONE', ( #77103, #198337, #102589, #57827 ) ) ;
#141245 = CARTESIAN_POINT ( 'NONE',  ( 3.701012746850603996, 7.261672604726938651, 1.040834085586084257E-14 ) ) ;
#141247 = CARTESIAN_POINT ( 'NONE',  ( -7.199016379176422120, 11.34267684244042584, 0.000000000000000000 ) ) ;
#141248 = CARTESIAN_POINT ( 'NONE',  ( 3.397504326804317909, 1.702965868850464082, 1.331369057855802174 ) ) ;
#141249 = CARTESIAN_POINT ( 'NONE',  ( -4.228163802615396705, 6.026220084508304708, -1.599625672291271394 ) ) ;
#141250 = CARTESIAN_POINT ( 'NONE',  ( 3.444653546323793947, 6.176457016423196222, 1.199719254218451159 ) ) ;
#141251 = CARTESIAN_POINT ( 'NONE',  ( 0.1762450972803020210, 2.096614079038420897, -0.3174041833761130360 ) ) ;
#141252 = ADVANCED_FACE ( 'NONE', ( #93813 ), #41856, .T. ) ;
#141253 = CARTESIAN_POINT ( 'NONE',  ( 4.594645031659345236, -0.4005623417570289280, -1.780931357837008733 ) ) ;
#141254 = CARTESIAN_POINT ( 'NONE',  ( 9.244745934994428538, 11.58786253049815329, -7.169110776657137585 ) ) ;
#141255 = CARTESIAN_POINT ( 'NONE',  ( 1.089067603693228525, 1.740485041285372958, -0.9256802945506740210 ) ) ;
#141256 = CARTESIAN_POINT ( 'NONE',  ( 3.884940529579200774, -1.786240503712609895, -0.6835825222790415934 ) ) ;
#141257 = ORIENTED_EDGE ( 'NONE', *, *, #208162, .T. ) ;
#141258 = CARTESIAN_POINT ( 'NONE',  ( 0.3544712801348807729, 3.975028838742734383, 0.9637995819944042974 ) ) ;
#141259 = CARTESIAN_POINT ( 'NONE',  ( 4.773860271397749599, -1.931934984910467890, 0.3821518213343431669 ) ) ;
#141260 = ORIENTED_EDGE ( 'NONE', *, *, #174519, .T. ) ;
#141261 = CARTESIAN_POINT ( 'NONE',  ( 6.462452672982783142, -1.777441430900746688, -0.7828909329169189135 ) ) ;
#141262 = VERTEX_POINT ( 'NONE', #107199 ) ;
#141263 = CARTESIAN_POINT ( 'NONE',  ( -5.692444392891315097, 7.734547439830227411, -1.599625672291271394 ) ) ;
#141265 = CARTESIAN_POINT ( 'NONE',  ( 6.293239850429793947, -0.1054838202379469042, -2.118119863012501991 ) ) ;
#141264 = CARTESIAN_POINT ( 'NONE',  ( -6.120580001926503755, 6.105374521861167914, -0.7998128361456362523 ) ) ;
#141266 = CARTESIAN_POINT ( 'NONE',  ( 8.122743427918724279, 8.649157885426255632, 0.7216878364870267237 ) ) ;
#141268 = ORIENTED_EDGE ( 'NONE', *, *, #212491, .F. ) ;
#141267 = CARTESIAN_POINT ( 'NONE',  ( 3.809155001108742056, 1.613891119516493999, -1.025466636117925212 ) ) ;
#141269 = DIRECTION ( 'NONE',  ( 0.000000000000000000, 1.000000000000000000, 0.000000000000000000 ) ) ;
#141270 = CARTESIAN_POINT ( 'NONE',  ( 9.622977958535885890, 4.242291508015296309, -7.169920593678716259 ) ) ;
#141271 = CARTESIAN_POINT ( 'NONE',  ( 5.918613486546395741, -0.7266362437793117968, -1.877539736040201079 ) ) ;
#141272 = CARTESIAN_POINT ( 'NONE',  ( -0.006800380015319074101, 7.009756401597622144, 1.999988438674507485 ) ) ;
#141274 = CARTESIAN_POINT ( 'NONE',  ( 5.735564631760892595, 0.5807582108038509272, -1.931123567068816493 ) ) ;
#141273 = CARTESIAN_POINT ( 'NONE',  ( 6.252569598636129378, 0.5776572744066664766, 1.731972519516040032 ) ) ;
#141275 = CARTESIAN_POINT ( 'NONE',  ( -2.314109536355652530, 5.457892750589173225, -0.8025987720412944837 ) ) ;
#141276 = CARTESIAN_POINT ( 'NONE',  ( 1.750525128138082254, -2.060206210462053988, -0.2049951091474821463 ) ) ;
#141277 = CARTESIAN_POINT ( 'NONE',  ( -5.280010757518168063, 8.247430752824802980, -1.199719254218446718 ) ) ;
#141278 = AXIS2_PLACEMENT_3D ( 'NONE', #3217, #34673, #136466 ) ;
#141279 = CARTESIAN_POINT ( 'NONE',  ( -5.902949979233523159, 7.165898849449257924, -1.132310321155009847 ) ) ;
#141280 = CARTESIAN_POINT ( 'NONE',  ( 1.230728480726485330, 2.855010058876359835, -0.7749999999999926947 ) ) ;
#141281 = CARTESIAN_POINT ( 'NONE',  ( 1.001543065824772753E-15, -3.171874999522042771, 3.793834371823810780 ) ) ;
#141282 = CARTESIAN_POINT ( 'NONE',  ( 4.788000803920411386, 8.737751371215816576, 1.040834085586084257E-14 ) ) ;
#141283 = EDGE_CURVE ( 'NONE', #115079, #113953, #154146, .T. ) ;
#141284 = CARTESIAN_POINT ( 'NONE',  ( 5.234856708652235291, 5.279956712948652431, 0.7216878364870338292 ) ) ;
#141285 = PLANE ( 'NONE',  #213721 ) ;
#141286 = CARTESIAN_POINT ( 'NONE',  ( -0.6823417656250039265, 12.38020833367473017, -1.181850606188755259 ) ) ;
#141288 = CARTESIAN_POINT ( 'NONE',  ( -6.282224075085783177, 8.422623735723785643, 1.599625672291269396 ) ) ;
#141287 = CARTESIAN_POINT ( 'NONE',  ( 6.925078400183550364, 4.696033252921790968, 2.518291795588607052 ) ) ;
#141289 = EDGE_CURVE ( 'NONE', #195055, #137303, #143829, .T. ) ;
#141290 = CARTESIAN_POINT ( 'NONE',  ( 4.869590383887318019, -0.2189826452120811340, -1.720196969245034513 ) ) ;
#141291 = CARTESIAN_POINT ( 'NONE',  ( -5.576481253922474401, 5.400316305864651056, -0.7998128361456221525 ) ) ;
#141292 = CIRCLE ( 'NONE', #89307, 0.08000000000000040412 ) ;
#141293 = CARTESIAN_POINT ( 'NONE',  ( 2.219664259111033378, 0.3580842396277704176, -2.038906786875307020 ) ) ;
#141294 = CARTESIAN_POINT ( 'NONE',  ( 3.146228450019908252, 0.9544266383219732752, 1.889993806685738464 ) ) ;
#141295 = CARTESIAN_POINT ( 'NONE',  ( 5.940443861082012944, 10.08226827123770697, 0.7998128361456462443 ) ) ;
#141296 = CARTESIAN_POINT ( 'NONE',  ( 0.08058608058607655278, -9.902238891812018551, 10.99970480893082225 ) ) ;
#141297 = CARTESIAN_POINT ( 'NONE',  ( 1.797640638355556320, -1.422838571669628127, -1.361938172677351400 ) ) ;
#141298 = CARTESIAN_POINT ( 'NONE',  ( 6.112872195911107198, 6.017013290715023111, -0.08730524813132384265 ) ) ;
#141300 = CARTESIAN_POINT ( 'NONE',  ( 0.1582721923853447621, 1.907395734848855051, 0.1385995803297388196 ) ) ;
#141299 = CARTESIAN_POINT ( 'NONE',  ( 3.475000000000000533, -2.304166666666668473, 2.006292185433948827 ) ) ;
#141301 = CARTESIAN_POINT ( 'NONE',  ( 3.838036126445078633, 2.281091060459582209, 0.2259633074802695485 ) ) ;
#141302 = CARTESIAN_POINT ( 'NONE',  ( 1.664397423953474009, -1.292156093668932693, 1.290017532847971271 ) ) ;
#141303 = CARTESIAN_POINT ( 'NONE',  ( 4.844006021832467646, 8.873367135438366304, 0.000000000000000000 ) ) ;
#141304 = CARTESIAN_POINT ( 'NONE',  ( 7.253248993186735660, 7.564471368247083660, 0.7216878364870317197 ) ) ;
#141305 = CARTESIAN_POINT ( 'NONE',  ( -8.830438121202295321, 9.196599317691152464, -0.7998128361456291469 ) ) ;
#141306 = CARTESIAN_POINT ( 'NONE',  ( 2.513933912945048199, -0.6273889547634775576, 1.913045067402745936 ) ) ;
#141307 = CARTESIAN_POINT ( 'NONE',  ( 1.832786370036399326, -1.861117592713131819, -0.6203919267877275878 ) ) ;
#141308 = CARTESIAN_POINT ( 'NONE',  ( -6.970863535720637216, 11.28442455831609337, 0.7998128361456481317 ) ) ;
#141309 = CARTESIAN_POINT ( 'NONE',  ( -7.061099074618889304, 7.132370430010492868, -0.7998128361456291469 ) ) ;
#141310 = CARTESIAN_POINT ( 'NONE',  ( 0.07516593201275456604, 0.0004601587237917924593, -2.044269526395313452 ) ) ;
#141312 = CARTESIAN_POINT ( 'NONE',  ( 3.203702280051218931, -1.767899805609447261, 0.08541964596707474211 ) ) ;
#141311 = CARTESIAN_POINT ( 'NONE',  ( 4.892568727727841349, 1.738426232616798295, -1.160983500135639890 ) ) ;
#141313 = CARTESIAN_POINT ( 'NONE',  ( 1.050790385994998077, 14.00000000000000533, 12.64745918785790302 ) ) ;
#141314 = CARTESIAN_POINT ( 'NONE',  ( 0.3928598746986839974, 1.819701785225702473, -1.220828600141062203 ) ) ;
#141315 = CARTESIAN_POINT ( 'NONE',  ( 5.454937174282652457, 0.3337844340769695606, -1.707832357695503234 ) ) ;
#141316 = CARTESIAN_POINT ( 'NONE',  ( 7.065770611016287006, 11.39514947949436774, 1.040834085586084257E-14 ) ) ;
#141317 = EDGE_CURVE ( 'NONE', #46791, #5559, #88753, .T. ) ;
#141318 = CARTESIAN_POINT ( 'NONE',  ( 5.977181698541591537, -2.287177818765488091, -0.2295778655121790968 ) ) ;
#141319 = CARTESIAN_POINT ( 'NONE',  ( 2.970855920843799236, 6.567331372341457474, 0.4599263646697975272 ) ) ;
#141320 = CARTESIAN_POINT ( 'NONE',  ( 5.676976676600826721, -0.7816020568793962120, -1.547713907698013092 ) ) ;
#141321 = CARTESIAN_POINT ( 'NONE',  ( 6.021977204206338641, 2.140098014189107278, -0.3652067468529682226 ) ) ;
#141322 = CARTESIAN_POINT ( 'NONE',  ( 2.683624340501134853, 5.218313266304903664, -1.199719254218446718 ) ) ;
#141323 = CARTESIAN_POINT ( 'NONE',  ( 0.2338150414605598693, 0.6575980258751003005, -2.012739700429423628 ) ) ;
#141324 = CARTESIAN_POINT ( 'NONE',  ( 3.281250000000002665, 0.7852924748301588487, 1.895863743164012849 ) ) ;
#141325 = CARTESIAN_POINT ( 'NONE',  ( 6.827182134110231004, 7.052068023338082803, 2.687205202894725975 ) ) ;
#141326 = CARTESIAN_POINT ( 'NONE',  ( 4.137660063496669594, -1.327783069688622586, -1.395926297547624984 ) ) ;
#141327 = CARTESIAN_POINT ( 'NONE',  ( 0.7500000000000006661, 10.61458333401613174, 1.299038105676657340 ) ) ;
#141328 = CARTESIAN_POINT ( 'NONE',  ( 1.471644961476214597, -1.907451222982279093, -1.138109381883713578 ) ) ;
#141329 = ORIENTED_EDGE ( 'NONE', *, *, #166507, .T. ) ;
#141330 = CARTESIAN_POINT ( 'NONE',  ( -1.201851678989727383E-14, 4.087500000000022560, -1.732050807568863648 ) ) ;
#141331 = CARTESIAN_POINT ( 'NONE',  ( 5.497994985541524215, 6.373081223675282736, -1.199719254218445830 ) ) ;
#141332 = CARTESIAN_POINT ( 'NONE',  ( 7.145310649601935182, 8.294949498412453437, -1.199719254218446718 ) ) ;
#141333 = AXIS2_PLACEMENT_3D ( 'NONE', #117567, #154278, #83927 ) ;
#141334 = CARTESIAN_POINT ( 'NONE',  ( 2.631719755377628811, -0.2151721393647449687, 2.210840341435269973 ) ) ;
#141335 = FACE_BOUND ( 'NONE', #1779, .T. ) ;
#141336 = CARTESIAN_POINT ( 'NONE',  ( 6.805829924380114804, 8.002851668940699881, 1.082531754730558626 ) ) ;
#141337 = CARTESIAN_POINT ( 'NONE',  ( -10.10046125205659173, 10.88621900359527572, -0.7216878364870267237 ) ) ;
#141338 = CARTESIAN_POINT ( 'NONE',  ( 7.526184669361807522, 7.953172667109813077, 0.000000000000000000 ) ) ;
#141339 = CARTESIAN_POINT ( 'NONE',  ( 0.5982800022500452952, -0.2930678230431381648, 1.994870242743536304 ) ) ;
#141341 = CARTESIAN_POINT ( 'NONE',  ( 6.848098694195379643, -0.8844518680410964340, 1.861345814548149624 ) ) ;
#141340 = CARTESIAN_POINT ( 'NONE',  ( 9.413438726589914651, 9.876766690643398405, 0.000000000000000000 ) ) ;
#141342 = CARTESIAN_POINT ( 'NONE',  ( 6.658462837642791676, 8.861568958707010779, 1.443375672974063439 ) ) ;
#141343 = CARTESIAN_POINT ( 'NONE',  ( -2.450294804887450884, 1.972237431424518794, 11.52773071619796497 ) ) ;
#141344 = CARTESIAN_POINT ( 'NONE',  ( -1.364683531250012516, 0.7802083336747528408, 0.7879004041258379498 ) ) ;
#141345 = CARTESIAN_POINT ( 'NONE',  ( 1.264531387369687065, -1.596916444607907382, -0.7631234423778727738 ) ) ;
#141346 = CARTESIAN_POINT ( 'NONE',  ( 0.7037502660087076034, 1.864169469917423161, 0.7691187473759173443 ) ) ;
#141347 = CARTESIAN_POINT ( 'NONE',  ( 5.249435226766168583, 1.738107782858036687, -0.09287461536438243459 ) ) ;
#141348 = CARTESIAN_POINT ( 'NONE',  ( 3.685359659257981146, 1.661040094275951340, 1.580089079255690088 ) ) ;
#141349 = CARTESIAN_POINT ( 'NONE',  ( -0.6823417656250246877, -0.1989583329919109023, 1.181850606188755259 ) ) ;
#141350 = CARTESIAN_POINT ( 'NONE',  ( 1.816098422328410900, 1.717562825535594140, 0.6636192267199735317 ) ) ;
#141351 = ADVANCED_FACE ( 'NONE', ( #70338 ), #23738, .T. ) ;
#141352 = CARTESIAN_POINT ( 'NONE',  ( 9.049177462117294013, 12.64479190819049670, -1.199719254218446718 ) ) ;
#141353 = CARTESIAN_POINT ( 'NONE',  ( 8.662485680320882508, 14.42234338554197315, 8.322065852714080947 ) ) ;
#141354 = CARTESIAN_POINT ( 'NONE',  ( 3.241029684393876842, -1.610631872634618933, 0.8593927405577477252 ) ) ;
#141355 = CARTESIAN_POINT ( 'NONE',  ( 4.324842380567116784, 0.8596320953860696612, -1.824118450417112847 ) ) ;
#141356 = CARTESIAN_POINT ( 'NONE',  ( -10.15522075183580419, 11.80651128435196462, 1.199719254218462483 ) ) ;
#141358 = CARTESIAN_POINT ( 'NONE',  ( -9.586610838029429260, -7.161464053357574855, 0.003376046620574835178 ) ) ;
#141357 = CARTESIAN_POINT ( 'NONE',  ( 2.589068414660402606, -0.3862909535316555454, -2.229145898733439157 ) ) ;
#141359 = CARTESIAN_POINT ( 'NONE',  ( 5.403390757083595730, 1.719820611593615656, 1.215146281773227921 ) ) ;
#141360 = B_SPLINE_CURVE_WITH_KNOTS ( 'NONE', 3,
 ( #54302, #169106, #3384, #38051, #20703, #72665, #150750, #6586, #84661, #2311 ),
 .UNSPECIFIED., .F., .F.,
 ( 4, 1, 1, 1, 1, 1, 1, 4 ),
 ( 0.000000000000000000, 0.09489293188423997272, 0.1878783894049059211, 0.2584743716234961797, 0.3617987437640678983, 0.5212292184658617877, 0.7337638816394396191, 1.000000000000000000 ),
 .UNSPECIFIED. ) ;
#141361 = CARTESIAN_POINT ( 'NONE',  ( 9.672792005750940447, 13.47495944640959920, 8.176450814826708324 ) ) ;
#141362 = CARTESIAN_POINT ( 'NONE',  ( 2.383334800519558705, -0.002349189141126820958, 2.070544812199434315 ) ) ;
#141363 = CARTESIAN_POINT ( 'NONE',  ( 3.357615597678655917, 7.068968630600412695, 0.7998128361456321445 ) ) ;
#141364 = CARTESIAN_POINT ( 'NONE',  ( -7.511572993685796537E-15, 0.3593750003414036831, -1.570758158831792262 ) ) ;
#141365 = CARTESIAN_POINT ( 'NONE',  ( 5.162787349232583090, 0.6159572760087470567, 2.029033592890214788 ) ) ;
#141366 = CONTEXT_DEPENDENT_SHAPE_REPRESENTATION ( #10487, #12554 ) ;
#141367 = CARTESIAN_POINT ( 'NONE',  ( 1.488762753728092969, -0.2822029396061729867, -1.905608977972670370 ) ) ;
#141368 = CARTESIAN_POINT ( 'NONE',  ( -4.248501033035892327, 6.049946853332221153, -1.599625672291271394 ) ) ;
#141369 = CARTESIAN_POINT ( 'NONE',  ( 9.094822116668764167, 9.505047312402055582, 0.7998128361456462443 ) ) ;
#141370 = CARTESIAN_POINT ( 'NONE',  ( 4.204437033569277560, 7.919277282557212416, 0.000000000000000000 ) ) ;
#141371 = CARTESIAN_POINT ( 'NONE',  ( -1.737500000000000266, -0.3645833323774189116, -3.009438278150923907 ) ) ;
#141372 = CIRCLE ( 'NONE', #207028, 0.04999999999999883010 ) ;
#141373 = CARTESIAN_POINT ( 'NONE',  ( -5.590039407536138150, 5.416134151747256986, 0.000000000000000000 ) ) ;
#141374 = CARTESIAN_POINT ( 'NONE',  ( -0.1047794747230318818, -2.156939676625940994, -0.5310815526072456549 ) ) ;
#141375 = CARTESIAN_POINT ( 'NONE',  ( 2.239418434904976607, -1.881632620311970649, 0.9459126739295388164 ) ) ;
#141376 = CARTESIAN_POINT ( 'NONE',  ( -6.140917232347002042, 6.129101290685087911, -0.7998128361456362523 ) ) ;
#141377 = CARTESIAN_POINT ( 'NONE',  ( 7.130698725783555680, 10.40656671580112658, 1.199719254218460707 ) ) ;
#141378 = CARTESIAN_POINT ( 'NONE',  ( 6.789920448004552078, -1.215336557376142101, -1.409407482083424590 ) ) ;
#141379 = CARTESIAN_POINT ( 'NONE',  ( 8.450809820019639318, 8.753699632978056755, -0.7998128361456291469 ) ) ;
#141380 = EDGE_CURVE ( 'NONE', #156687, #48021, #63597, .T. ) ;
#141381 = CARTESIAN_POINT ( 'NONE',  ( 11.97185388258315086, 9.720000092796073687, 0.8311143155443657671 ) ) ;
#141382 = CARTESIAN_POINT ( 'NONE',  ( -5.496904935697871863, 5.377753611261092637, 0.7998128361456281477 ) ) ;
#141384 = VERTEX_POINT ( 'NONE', #188374 ) ;
#141383 = CARTESIAN_POINT ( 'NONE',  ( -9.829298180227631576, 10.56986208646148384, 1.040834085586084257E-14 ) ) ;
#141385 = CARTESIAN_POINT ( 'NONE',  ( 0.3695850531008069706, -1.794773754367712693, -1.129184308951653781 ) ) ;
#141386 = DIRECTION ( 'NONE',  ( 0.000000000000000000, 0.000000000000000000, -1.000000000000000000 ) ) ;
#141388 = CARTESIAN_POINT ( 'NONE',  ( 3.332423539472821439, -1.170687260143790320, 1.574129132985650825 ) ) ;
#141387 = CARTESIAN_POINT ( 'NONE',  ( 0.6124999999999862776, -0.6666666666666556385, 1.060881119635903147 ) ) ;
#141389 = CARTESIAN_POINT ( 'NONE',  ( 0.5499753625364013354, 0.6768306982547143136, -2.053065283773393368 ) ) ;
#141391 = CARTESIAN_POINT ( 'NONE',  ( -4.885033903151685841, 6.706220529795296592, -1.250124166851230845 ) ) ;
#141390 = CARTESIAN_POINT ( 'NONE',  ( -4.390861645979385663, 6.216034235099629157, -1.599625672291271394 ) ) ;
#141392 = CARTESIAN_POINT ( 'NONE',  ( 1.364683531249986537, 2.155208333674751398, -0.7879004041258239610 ) ) ;
#141393 = CARTESIAN_POINT ( 'NONE',  ( 2.483973769465233961, -0.2969572910719043279, -1.714626640263767543 ) ) ;
#141394 = CARTESIAN_POINT ( 'NONE',  ( 6.982085921357777281, 7.248114451113292667, 1.040834085586084257E-14 ) ) ;
#141395 = CARTESIAN_POINT ( 'NONE',  ( -12.65289843835643069, 8.694282390621570045, -1.237672713095353982 ) ) ;
#141396 = CARTESIAN_POINT ( 'NONE',  ( 1.862657450031137474, -0.6818942500997280387, 1.897406292459068222 ) ) ;
#141397 = CARTESIAN_POINT ( 'NONE',  ( 6.825078400183550720, 7.629137130509051623, 2.844348168701658075 ) ) ;
#141398 = CYLINDRICAL_SURFACE ( 'NONE', #52841, 0.1000000000000000472 ) ;
#141399 = CARTESIAN_POINT ( 'NONE',  ( 2.641432621735483544, -1.459803026827242611, -1.325177341282377741 ) ) ;
#141400 = B_SPLINE_CURVE_WITH_KNOTS ( 'NONE', 3,
 ( #67707, #81868, #101307, #147954 ),
 .UNSPECIFIED., .F., .F.,
 ( 4, 4 ),
 ( 0.000000000000000000, 7.308104204455707247E-05 ),
 .UNSPECIFIED. ) ;
#141403 = ADVANCED_FACE ( 'NONE', ( #155893 ), #108319, .F. ) ;
#141402 = CARTESIAN_POINT ( 'NONE',  ( -5.072158865288277418, 7.010880990960010273, 1.443375672974058777 ) ) ;
#141401 = CARTESIAN_POINT ( 'NONE',  ( 5.343983030329363615, -1.218012673290536974, -1.474316871017400166 ) ) ;
#141404 = CARTESIAN_POINT ( 'NONE',  ( -6.265276382846530545, 6.482112999508623297, 0.000000000000000000 ) ) ;
#141405 = CARTESIAN_POINT ( 'NONE',  ( 7.198453214212898743, 7.362893269528701268, 0.7998128361456291469 ) ) ;
#141406 = CARTESIAN_POINT ( 'NONE',  ( -4.959250327548641479, 9.007818825440551791, -0.7998128361456362523 ) ) ;
#141407 = CARTESIAN_POINT ( 'NONE',  ( 2.754561962923445684, 2.004688795240500365, 0.2448751400806712664 ) ) ;
#141408 = CARTESIAN_POINT ( 'NONE',  ( 2.687227643083427534E-13, -3.232243495192088201, 3.285556943749999625 ) ) ;
#141409 = EDGE_CURVE ( 'NONE', #36526, #57617, #116524, .T. ) ;
#141410 = CARTESIAN_POINT ( 'NONE',  ( 5.192513718098597408, -2.289403112372697890, -0.2887273360754892826 ) ) ;
#141411 = CARTESIAN_POINT ( 'NONE',  ( 6.602011099637477010, 0.7519813002578833450, -1.812223124677159181 ) ) ;
#141412 = CARTESIAN_POINT ( 'NONE',  ( 3.397265449134680981, -1.732261247800225279, 0.9206733083975682241 ) ) ;
#141413 = CARTESIAN_POINT ( 'NONE',  ( 7.574201371528760163, 11.98831870009225931, 1.040834085586084257E-14 ) ) ;
#141414 = CARTESIAN_POINT ( 'NONE',  ( 0.3697678102792775756, -0.2496098759999023087, -2.000856779379902139 ) ) ;
#141415 = ORIENTED_EDGE ( 'NONE', *, *, #392, .T. ) ;
#141416 = CARTESIAN_POINT ( 'NONE',  ( 2.905574018005254722, -2.039320757748352086, 0.5691538075108558692 ) ) ;
#141418 = CARTESIAN_POINT ( 'NONE',  ( -6.181627972826976958, 9.299317504018391745, 1.199719254218452047 ) ) ;
#141417 = CARTESIAN_POINT ( 'NONE',  ( -4.783329267523015460, 4.474972321731942593, -0.7998128361456221525 ) ) ;
#141419 = CARTESIAN_POINT ( 'NONE',  ( 1.939159035295745737, 0.7054217538491478479, -1.700835786604155242 ) ) ;
#141420 = ORIENTED_EDGE ( 'NONE', *, *, #133002, .F. ) ;
#141421 = CARTESIAN_POINT ( 'NONE',  ( 3.098842478760281516, 1.825076540557273974, 0.8578426345753201732 ) ) ;
#141422 = CARTESIAN_POINT ( 'NONE',  ( -8.286004436246233951, 12.81875560892930466, 1.040834085586084257E-14 ) ) ;
#141423 = CARTESIAN_POINT ( 'NONE',  ( 9.427850895902821549, 13.54474674066948126, 7.423989997610757285 ) ) ;
#141424 = CARTESIAN_POINT ( 'NONE',  ( 2.619513681940002670, 1.793805257907291395, 1.130712135851599465 ) ) ;
#141425 = CARTESIAN_POINT ( 'NONE',  ( -1.201851678989727383E-14, 4.118750000682818602, -1.732050807568863648 ) ) ;
#141426 = CARTESIAN_POINT ( 'NONE',  ( 7.670162217029129259, 9.971608557999250166, 1.599625672291281386 ) ) ;
#141427 = CARTESIAN_POINT ( 'NONE',  ( 7.309781096423290769, 8.557108029695882578, 1.199719254218452935 ) ) ;
#141428 = CARTESIAN_POINT ( 'NONE',  ( 4.446593522994434444, 0.5459629501111874506, 1.987092823586662504 ) ) ;
#141430 = CARTESIAN_POINT ( 'NONE',  ( 1.786409390178132162, 1.601450680722369846, -0.9084932335857234253 ) ) ;
#141429 = CARTESIAN_POINT ( 'NONE',  ( -8.365544474831901667, 9.718555627847388578, 1.199719254218462483 ) ) ;
#141431 = CARTESIAN_POINT ( 'NONE',  ( 1.364683531249990311, 4.384375000341417028, 1.214306433183764966E-14 ) ) ;
#141432 = CARTESIAN_POINT ( 'NONE',  ( -1.608462485350604876, 8.735270501766756013, -2.463594439587629914 ) ) ;
#141433 = CARTESIAN_POINT ( 'NONE',  ( -9.499766273075884726, -9.919999999999998153, 0.06663900456894793212 ) ) ;
#141434 = DIRECTION ( 'NONE',  ( 0.000000000000000000, 0.000000000000000000, 1.000000000000000000 ) ) ;
#141435 = AXIS2_PLACEMENT_3D ( 'NONE', #46182, #175116, #97071 ) ;
#141436 = CARTESIAN_POINT ( 'NONE',  ( 0.8036966383840878914, 1.806304194667744500, 1.267646993260997723 ) ) ;
#141437 = CARTESIAN_POINT ( 'NONE',  ( 3.181238891614282416, -0.1630793868099291999, -2.256562113509274159 ) ) ;
#141438 = CARTESIAN_POINT ( 'NONE',  ( -8.351459436338037889, 10.76645531385962862, -1.443375672974059665 ) ) ;
#141439 = CARTESIAN_POINT ( 'NONE',  ( 3.445387325821075652, -1.671857736322950094, 0.6981543005735133534 ) ) ;
#141440 = CARTESIAN_POINT ( 'NONE',  ( 3.292102688380782460, -0.7811219226253396375, -1.749442990535796438 ) ) ;
#141441 = CARTESIAN_POINT ( 'NONE',  ( 4.352052382902608763, -0.7952921280917917279, 1.911720769834825973 ) ) ;
#141442 = CARTESIAN_POINT ( 'NONE',  ( -1.201851678989727383E-14, 2.634375000341417916, 1.575800808251672791 ) ) ;
#141443 = CARTESIAN_POINT ( 'NONE',  ( 2.993000350225515138, 1.691612214138412007, -1.012252976823005968 ) ) ;
#141444 = CARTESIAN_POINT ( 'NONE',  ( 1.395397119253296569, 1.457039974399224391, 1.260252556074402897 ) ) ;
#141445 = CARTESIAN_POINT ( 'NONE',  ( 4.030043484472041193, 1.001115284758803625, -1.580040089582811280 ) ) ;
#141447 = CARTESIAN_POINT ( 'NONE',  ( 5.228576739797318851, 7.698598165248225378, -1.206158463488806953 ) ) ;
#141446 = CARTESIAN_POINT ( 'NONE',  ( 2.051827946393524726, -1.855052535695273841, -1.372493790568436012 ) ) ;
#141448 = CARTESIAN_POINT ( 'NONE',  ( 3.719077791506773423, -1.640430839875358204, -0.8789487387581331745 ) ) ;
#141449 = CARTESIAN_POINT ( 'NONE',  ( -1.364683531250010295, 4.280208333674753618, 0.7879004041258379498 ) ) ;
#141450 = VECTOR ( 'NONE', #69981, 1000.000000000000000 ) ;
#141451 = CARTESIAN_POINT ( 'NONE',  ( -3.653032323878261600, 6.349289246911547835, -1.199719254218452047 ) ) ;
#141452 = CARTESIAN_POINT ( 'NONE',  ( 0.000000000000000000, 8.920000000000001705, 0.000000000000000000 ) ) ;
#141453 = CARTESIAN_POINT ( 'NONE',  ( 0.8738170914556376845, 2.029154634757854847, -0.5636997952245518251 ) ) ;
#141455 = CARTESIAN_POINT ( 'NONE',  ( -2.788906526875773208E-15, 8.937500000000001776, -1.499999999999998446 ) ) ;
#141454 = CARTESIAN_POINT ( 'NONE',  ( -1.364683531249997417, 4.571875000341417028, 1.214306433183764966E-14 ) ) ;
#141456 = CARTESIAN_POINT ( 'NONE',  ( 6.766866382711775429, -1.973269837180600561, -0.8828958408187634888 ) ) ;
#141457 = CARTESIAN_POINT ( 'NONE',  ( 2.180079139336263516, 2.078761533942363737, -0.4183221158333137457 ) ) ;
#141458 = CARTESIAN_POINT ( 'NONE',  ( 6.375650237155517708, 0.3431015828706286408, -1.990142738341105000 ) ) ;
#141459 = CARTESIAN_POINT ( 'NONE',  ( -1.364683531250000748, -0.9906249996585805295, 0.000000000000000000 ) ) ;
#141460 = CARTESIAN_POINT ( 'NONE',  ( -4.948362879307902418, 4.875437568721725512, 1.214306433183764966E-14 ) ) ;
#141461 = CARTESIAN_POINT ( 'NONE',  ( 5.986088515633498197, 6.942523675449257858, -1.199719254218446718 ) ) ;
#141462 = CARTESIAN_POINT ( 'NONE',  ( 0.9487563388480976245, 0.6265645459165304354, 2.068816658077163861 ) ) ;
#141464 = CARTESIAN_POINT ( 'NONE',  ( 3.009546912553647147, 5.494593250412460606, -1.082531754730543083 ) ) ;
#141463 = CARTESIAN_POINT ( 'NONE',  ( 6.038177310039780643, 8.137902509836795417, -1.599625672291283607 ) ) ;
#141465 = CARTESIAN_POINT ( 'NONE',  ( -4.462568837553487100, 5.235360394347691404, -1.199719254218453823 ) ) ;
#141466 = CARTESIAN_POINT ( 'NONE',  ( 4.469935555517978720, -0.9463019959239076240, 1.780667052345537238 ) ) ;
#141468 = CARTESIAN_POINT ( 'NONE',  ( -5.411112705185557203, 9.327065566109540740, 0.7216878364870267237 ) ) ;
#141467 = CARTESIAN_POINT ( 'NONE',  ( -8.839552966430007430, 11.33589776563360019, -1.443375672974059665 ) ) ;
#141469 = SURFACE_SIDE_STYLE ('',( #75357 ) ) ;
#141471 = CARTESIAN_POINT ( 'NONE',  ( 0.6823417656249934904, 10.19270833367473550, 1.181850606188764807 ) ) ;
#141470 = CARTESIAN_POINT ( 'NONE',  ( 0.7610528644104715967, -1.636749228899089470, 1.562301092707372607 ) ) ;
#141472 = CARTESIAN_POINT ( 'NONE',  ( -10.45741655484220267, 11.09474082360439873, -0.7998128361456221525 ) ) ;
#141474 = CARTESIAN_POINT ( 'NONE',  ( 6.275017575846199236, 1.753023089329442064, -0.9963169848806670004 ) ) ;
#141473 = CARTESIAN_POINT ( 'NONE',  ( -4.514501963226242864, 7.250374142863800664, 1.082531754730560403 ) ) ;
#141475 = CARTESIAN_POINT ( 'NONE',  ( -0.6823417656250003738, 0.7802083336747520637, -1.181850606188749264 ) ) ;
#141476 = CARTESIAN_POINT ( 'NONE',  ( 0.000000000000000000, 1000.000000000000000, 0.000000000000000000 ) ) ;
#141477 = DIRECTION ( 'NONE',  ( -0.7592566023653004592, 0.6507913734559639396, 0.000000000000000000 ) ) ;
#141478 = CARTESIAN_POINT ( 'NONE',  ( 2.912419603134624779, 1.249142870932816507, -1.189721958963300130 ) ) ;
#141479 = CARTESIAN_POINT ( 'NONE',  ( 4.760848217054122422, 5.583353003765119560, -1.199719254218452047 ) ) ;
#141480 = CARTESIAN_POINT ( 'NONE',  ( 7.178115983792402233, 7.339166500704784823, 0.7998128361456281477 ) ) ;
#141481 = AXIS2_PLACEMENT_3D ( 'NONE', #58251, #42026, #6271 ) ;
#141482 = CARTESIAN_POINT ( 'NONE',  ( 0.8250501123308005003, -1.682963436248402056, 0.5476568922856797084 ) ) ;
#141483 = B_SPLINE_CURVE_WITH_KNOTS ( 'NONE', 3,
 ( #109850, #175864, #163613, #34651 ),
 .UNSPECIFIED., .F., .F.,
 ( 4, 4 ),
 ( 4.336808689941991736E-19, 6.033646489354566999E-05 ),
 .UNSPECIFIED. ) ;
#141484 = CARTESIAN_POINT ( 'NONE',  ( 2.315091943819780340, 1.615584347832084600, -1.200805960377361981 ) ) ;
#141485 = CARTESIAN_POINT ( 'NONE',  ( 8.830779531597181986, 3.974415841077565403, 7.430925027917878900 ) ) ;
#141486 = CARTESIAN_POINT ( 'NONE',  ( 4.173040645679537697, -2.057929556117383374, -0.7971749352265260491 ) ) ;
#141487 = ORIENTED_EDGE ( 'NONE', *, *, #69404, .T. ) ;
#141488 = CARTESIAN_POINT ( 'NONE',  ( 0.7499999999999885647, -0.5166666666666444030, 1.299038105676657340 ) ) ;
#141489 = CARTESIAN_POINT ( 'NONE',  ( 7.565086526301031178, 11.76975868075249387, 1.040834085586084257E-14 ) ) ;
#141491 = CARTESIAN_POINT ( 'NONE',  ( 2.495720449669074803, -1.994069261235394741, 0.2986488809556055446 ) ) ;
#141490 = CARTESIAN_POINT ( 'NONE',  ( 4.020270485675044192, -2.114722421624544157, 0.1573160286183969692 ) ) ;
#141493 = ORIENTED_EDGE ( 'NONE', *, *, #75480, .T. ) ;
#141492 = CARTESIAN_POINT ( 'NONE',  ( 3.128980605277735361, 1.639808012139221116, 0.7702280095687010775 ) ) ;
#141494 = CARTESIAN_POINT ( 'NONE',  ( 4.980641328173811999, 6.904110530993182948, 1.599625672291269396 ) ) ;
#141495 = EDGE_LOOP ( 'NONE', ( #124769, #36145, #71401, #94180, #125911, #52746 ) ) ;
#141496 = CARTESIAN_POINT ( 'NONE',  ( 0.4615142869485132637, 1.850934062480696252, -0.2700578556205368574 ) ) ;
#141497 = CARTESIAN_POINT ( 'NONE',  ( 5.203632029546647608, 4.965325544092860532, 1.040834085586084257E-14 ) ) ;
#141498 = AXIS2_PLACEMENT_3D ( 'NONE', #68402, #132406, #65207 ) ;
#141499 = CARTESIAN_POINT ( 'NONE',  ( 5.988856447087389512, -0.2726756491404982441, -1.805090154579996442 ) ) ;
#141501 = CARTESIAN_POINT ( 'NONE',  ( 2.659291035590090058, 1.817528298045675061, -0.6055613653334031010 ) ) ;
#141500 = CARTESIAN_POINT ( 'NONE',  ( -2.591579918506545344, 6.175260338232929413, 1.040834085586084257E-14 ) ) ;
#141502 = FACE_OUTER_BOUND ( 'NONE', #20927, .T. ) ;
#141503 = CARTESIAN_POINT ( 'NONE',  ( -0.4019237886466871523, 8.479914550367427140, -1.499999999999998668 ) ) ;
#141504 = CARTESIAN_POINT ( 'NONE',  ( -1.364683531250014514, 1.051041667008090208, -0.7879004041258289570 ) ) ;
#141505 = CARTESIAN_POINT ( 'NONE',  ( 7.404161286838808920, 8.771181268467660885, -1.082531754730548412 ) ) ;
#141506 = CARTESIAN_POINT ( 'NONE',  ( -4.177320726786328819, 5.966903162707725805, -1.443375672974066548 ) ) ;
#141507 = CARTESIAN_POINT ( 'NONE',  ( -7.259464905474441565, 7.434073576000447048, -0.7998128361456362523 ) ) ;
#141508 = CARTESIAN_POINT ( 'NONE',  ( 3.023802379225454473, -0.4096935937694180518, 2.080477853870852378 ) ) ;
#141509 = EDGE_CURVE ( 'NONE', #210733, #196836, #166544, .T. ) ;
#141511 = CARTESIAN_POINT ( 'NONE',  ( -10.37109829931902816, 6.927524423111719898, -5.134218648570218591 ) ) ;
#141510 = CARTESIAN_POINT ( 'NONE',  ( 11.04536101718726293, 10.90000000000000036, -1.100000000000002087 ) ) ;
#141512 = CARTESIAN_POINT ( 'NONE',  ( 4.569576162043214929, 1.912950159424832375, -0.4759120794774750474 ) ) ;
#141513 = CARTESIAN_POINT ( 'NONE',  ( -0.1579526903544171412, -1.242116785587377592, -1.585096312452577205 ) ) ;
#141514 = EDGE_LOOP ( 'NONE', ( #198758, #26358, #161854, #186471 ) ) ;
#141515 = CARTESIAN_POINT ( 'NONE',  ( 0.1756132116073009508, 1.572246328413629435, 1.418195661691145304 ) ) ;
#141516 = CARTESIAN_POINT ( 'NONE',  ( -1.499999999999997780, 5.650000000000023448, 1.214306433183764966E-14 ) ) ;
#141517 = CARTESIAN_POINT ( 'NONE',  ( 1.451716722110554025, 1.566445173006292935, 1.353826630019476562 ) ) ;
#141518 = CARTESIAN_POINT ( 'NONE',  ( 2.202979905913711178, -0.4252542987780962291, 1.894666818490578164 ) ) ;
#141519 = VERTEX_POINT ( 'NONE', #199011 ) ;
#141520 = CARTESIAN_POINT ( 'NONE',  ( 5.180097208873055692, 8.201141289397330780, -1.199719254218450271 ) ) ;
#141521 = CARTESIAN_POINT ( 'NONE',  ( 5.352436782344940802, 9.466536356036257871, 0.000000000000000000 ) ) ;
#141523 = CARTESIAN_POINT ( 'NONE',  ( 5.133733721068893807, 9.141106441222381918, 1.040834085586084257E-14 ) ) ;
#141522 = CARTESIAN_POINT ( 'NONE',  ( 3.275413508211636238, 1.326730841477074208, 1.615706224610208519 ) ) ;
#141524 = CARTESIAN_POINT ( 'NONE',  ( 5.058600711230250013, 5.074324715956299414, -0.7216878364870458196 ) ) ;
#141526 = VERTEX_POINT ( 'NONE', #31223 ) ;
#141525 = CARTESIAN_POINT ( 'NONE',  ( 0.7327119416217167114, 1.673282569690562882, 0.6944263290599298477 ) ) ;
#141527 = CARTESIAN_POINT ( 'NONE',  ( 5.408869034151480903, 1.673104959687292448, -1.439203791633147267 ) ) ;
#141528 = SURFACE_SIDE_STYLE ('',( #75415 ) ) ;
#141529 = CARTESIAN_POINT ( 'NONE',  ( 3.716033540554028125, -2.174548934981130444, 0.3748234698989146296 ) ) ;
#141530 = CARTESIAN_POINT ( 'NONE',  ( -8.012344526598182026E-15, 8.609375000341403350, -1.575800808251669460 ) ) ;
#141531 = CARTESIAN_POINT ( 'NONE',  ( 2.561071438676546741, -1.588783617390630898, 1.063917234122884858 ) ) ;
#141532 = CARTESIAN_POINT ( 'NONE',  ( 9.433775957010412938, 9.900493459467314850, 0.000000000000000000 ) ) ;
#141533 = CARTESIAN_POINT ( 'NONE',  ( 5.353992430378140099, -0.7485205528568984468, 1.930488744064068785 ) ) ;
#141535 = CARTESIAN_POINT ( 'NONE',  ( 3.309602206082487008, -0.4233974974612622066, 2.119663826602156131 ) ) ;
#141534 = CARTESIAN_POINT ( 'NONE',  ( 1.499999999922324134, 8.635424801869593381, -2.574739023100856006 ) ) ;
#141536 = CARTESIAN_POINT ( 'NONE',  ( 4.370767597569780172, -0.0006098066561242150270, -2.191739723162715592 ) ) ;
#141537 = AXIS2_PLACEMENT_3D ( 'NONE', #40268, #189700, #59702 ) ;
#141538 = EDGE_CURVE ( 'NONE', #199393, #133314, #133630, .T. ) ;
#141539 = CARTESIAN_POINT ( 'NONE',  ( 6.966220764712143243, 6.002124920821316323, -2.500000000000000444 ) ) ;
#141540 = CARTESIAN_POINT ( 'NONE',  ( 4.167152111353856547, 5.955039778036558040, 1.599625672291262513 ) ) ;
#141541 = CARTESIAN_POINT ( 'NONE',  ( 3.285556943750000514, -2.851041666188706358, 1.896917185911906722 ) ) ;
#141542 = CARTESIAN_POINT ( 'NONE',  ( -5.002032328799064231, 4.800402236545811441, -0.7998128361456362523 ) ) ;
#141543 = SHAPE_REPRESENTATION ( 'rubber 510 pin', ( #200407 ), #3714 ) ;
#141544 = CARTESIAN_POINT ( 'NONE',  ( -8.514157279702027736, 10.95626946445095307, -1.443375672974059665 ) ) ;
#141545 = CARTESIAN_POINT ( 'NONE',  ( 3.901714345682657292, 7.774026846596938434, 0.7998128361456271485 ) ) ;
#141546 = CARTESIAN_POINT ( 'NONE',  ( 6.051642586050198780, 1.563818258945088191, 1.356687170345116211 ) ) ;
#141547 = CARTESIAN_POINT ( 'NONE',  ( 4.020081831311307141, -0.9914672019816127557, -1.651657144357060014 ) ) ;
#141548 = CARTESIAN_POINT ( 'NONE',  ( 6.485961931490698440, -2.116758087377061504, 0.05204923864161013075 ) ) ;
#141549 = CARTESIAN_POINT ( 'NONE',  ( 6.831329296439236032, 9.063246493969506545, -1.599625672291267398 ) ) ;
#141550 = CARTESIAN_POINT ( 'NONE',  ( 3.834746474454188013E-15, 13.06250000000000178, 1.500000000000001554 ) ) ;
#141551 = CARTESIAN_POINT ( 'NONE',  ( 5.453942691717160507, -0.7125396638749655898, 1.836196350841996949 ) ) ;
#141552 = CARTESIAN_POINT ( 'NONE',  ( 6.667932745306283771, -1.416340830354723135, 1.803254352984103859 ) ) ;
#141553 = CARTESIAN_POINT ( 'NONE',  ( 4.740742070742828496, 0.3150700179065483719, 1.798135100120237473 ) ) ;
#141554 = CARTESIAN_POINT ( 'NONE',  ( 5.343321937561575474, 8.287607122913563273, -1.082531754730548412 ) ) ;
#141555 = CARTESIAN_POINT ( 'NONE',  ( 4.663641652976547647, 4.543262804668490418, 1.214306433183764966E-14 ) ) ;
#141556 = EDGE_CURVE ( 'NONE', #17304, #60595, #53230, .T. ) ;
#141557 = CARTESIAN_POINT ( 'NONE',  ( -5.601453741101424022, 6.564059448486966986, -1.199719254218453823 ) ) ;
#141558 = CARTESIAN_POINT ( 'NONE',  ( 3.878514461961128479, 6.682628084666728085, -1.199719254218448494 ) ) ;
#141559 = VERTEX_POINT ( 'NONE', #50656 ) ;
#141561 = CARTESIAN_POINT ( 'NONE',  ( 6.187749739576326569, 1.925281575520617849, -0.5883678985393098193 ) ) ;
#141560 = CARTESIAN_POINT ( 'NONE',  ( 2.524749765808989466, -1.717266272480859834, 0.6646640004178904215 ) ) ;
#141562 = CARTESIAN_POINT ( 'NONE',  ( 1.019433853822170777, 2.295598214472119203, -0.1149376033552674814 ) ) ;
#141563 = CARTESIAN_POINT ( 'NONE',  ( 6.491066726104213203, 0.1889763263339637456, 1.952597990788194959 ) ) ;
#141564 = CARTESIAN_POINT ( 'NONE',  ( -4.720210035852093533, 8.658662141802762946, -0.7998128361456281477 ) ) ;
#141565 = CARTESIAN_POINT ( 'NONE',  ( -5.980802423990385641, 6.150226714305422782, 9.481663569016276247E-06 ) ) ;
#141566 = CARTESIAN_POINT ( 'NONE',  ( -3.460355519985875983, 5.060167411448709629, 1.599625672291267398 ) ) ;
#141567 = CARTESIAN_POINT ( 'NONE',  ( 0.2915762745691782287, -1.893489616766583339, 0.8377075429084477332 ) ) ;
#141568 = CARTESIAN_POINT ( 'NONE',  ( -5.822300622425855110, 5.757381912443740646, 0.7998128361456281477 ) ) ;
#141570 = CARTESIAN_POINT ( 'NONE',  ( 1.727212824277712944, -1.762453432929488528, 0.6273722324065673650 ) ) ;
#141569 = CARTESIAN_POINT ( 'NONE',  ( 2.401997865216979111, -0.8028288615537516604, -1.930668023334235484 ) ) ;
#141571 = CARTESIAN_POINT ( 'NONE',  ( 1.827499746633702182, -1.427720486614523221, 1.423741782973136694 ) ) ;
#141572 = ORIENTED_EDGE ( 'NONE', *, *, #194669, .T. ) ;
#141573 = CARTESIAN_POINT ( 'NONE',  ( 0.6823417656249917140, 3.655208333674754506, 1.181850606188765695 ) ) ;
#141574 = CARTESIAN_POINT ( 'NONE',  ( 1.874151978141885833, -0.08570891532005876778, -1.738468184182701881 ) ) ;
#141575 = CARTESIAN_POINT ( 'NONE',  ( 5.311043488251262268, 7.219303374425030562, -1.599625672291256295 ) ) ;
#141577 = CARTESIAN_POINT ( 'NONE',  ( 1.499999999999990896, 8.640473353474858342, 2.571377442220807996 ) ) ;
#141576 = SURFACE_STYLE_FILL_AREA ( #59203 ) ;
#141578 = CARTESIAN_POINT ( 'NONE',  ( 2.525662786804376836, -0.9926222177696201188, -1.410421675411769993 ) ) ;
#141579 = CARTESIAN_POINT ( 'NONE',  ( 2.331793494658142230, 1.030094174309360344, -1.934364310732391345 ) ) ;
#141580 = CARTESIAN_POINT ( 'NONE',  ( 5.725267921653402148, -0.05769419298589681389, 2.206291853148376170 ) ) ;
#141581 = CARTESIAN_POINT ( 'NONE',  ( -9.645452764996941042, 5.068254855380425639, -6.574395040668256307 ) ) ;
#141582 = TOROIDAL_SURFACE ( 'NONE', #169207, 10.89999999999920455, 0.2000000000000000111 ) ;
#141583 = CARTESIAN_POINT ( 'NONE',  ( 2.483468006519026439, -0.003752633953101049049, 2.171239807183155790 ) ) ;
#141584 = CARTESIAN_POINT ( 'NONE',  ( 0.8733498553583609603, 1.760202786292342170, -0.4843115980177821744 ) ) ;
#141585 = CARTESIAN_POINT ( 'NONE',  ( 3.784452290478927505, -0.6679156082517538895, -2.009268603764336358 ) ) ;
#141586 = CARTESIAN_POINT ( 'NONE',  ( -15.75000000000000000, 11.29999999999999893, -3.200000000000001510 ) ) ;
#141587 = ORIENTED_EDGE ( 'NONE', *, *, #191657, .F. ) ;
#141589 = CARTESIAN_POINT ( 'NONE',  ( -0.6823417656250003738, 1.530208333674752730, -1.181850606188749264 ) ) ;
#141588 = CARTESIAN_POINT ( 'NONE',  ( 3.702894494004336678, 1.966553232070525237, 1.177740060511106135 ) ) ;
#141590 = DIRECTION ( 'NONE',  ( 0.9982742078614211811, 0.000000000000000000, -0.05872483221476467591 ) ) ;
#141591 = CARTESIAN_POINT ( 'NONE',  ( 5.352771719296971042, 5.139321848801576387, 0.7998128361456341429 ) ) ;
#141592 = CARTESIAN_POINT ( 'NONE',  ( 5.461676247742112800, -1.750072316323016963, -1.367929348606132800 ) ) ;
#141593 = CARTESIAN_POINT ( 'NONE',  ( -5.097502569058207200, 8.890910730635814829, -0.7216878364870207285 ) ) ;
#141594 = CARTESIAN_POINT ( 'NONE',  ( 4.528060117284240071, 5.345453560662148718, 1.082531754730560403 ) ) ;
#141595 = CARTESIAN_POINT ( 'NONE',  ( -5.544921637864820951, 9.412899644243539754, -0.7216878364870207285 ) ) ;
#141596 = CARTESIAN_POINT ( 'NONE',  ( 0.04699017840226540899, -9.984793624843945281, 10.91963405940079568 ) ) ;
#141597 = ORIENTED_EDGE ( 'NONE', *, *, #107203, .T. ) ;
#141598 = CARTESIAN_POINT ( 'NONE',  ( 4.061172775696818782, -1.158689426361030561, 1.650081270007992318 ) ) ;
#141600 = CARTESIAN_POINT ( 'NONE',  ( 2.782143433959896051, -1.183836405090990640, -1.688839807681275174 ) ) ;
#141599 = CARTESIAN_POINT ( 'NONE',  ( 6.962275575817444384, 8.081408578997208991, -1.199719254218446718 ) ) ;
#141601 = CARTESIAN_POINT ( 'NONE',  ( -3.830881975230008507, 4.022296396677373487, 0.8449283794988144969 ) ) ;
#141602 = CARTESIAN_POINT ( 'NONE',  ( 8.011942431032855083, 8.311964022485323511, 0.7998128361456291469 ) ) ;
#141603 = CARTESIAN_POINT ( 'NONE',  ( 0.000000000000000000, -2.646874999522040639, -3.793834371823813001 ) ) ;
#141604 = CARTESIAN_POINT ( 'NONE',  ( -1.364683531249997417, 5.009375000341425022, 1.214306433183764966E-14 ) ) ;
#141605 = CARTESIAN_POINT ( 'NONE',  ( 6.685463922536254877, -0.9407050535897142352, 1.977304495687677521 ) ) ;
#141606 = CARTESIAN_POINT ( 'NONE',  ( 3.182267690267494231, 1.591318367894577701, 1.238320962759748234 ) ) ;
#141607 = CARTESIAN_POINT ( 'NONE',  ( 2.243484787601189634, 1.840893492186860492, 0.04347913094143729396 ) ) ;
#141608 = ADVANCED_FACE ( 'NONE', ( #97297 ), #130274, .F. ) ;
#141609 = CARTESIAN_POINT ( 'NONE',  ( 7.657657833620182153, 7.828355648845348291, -0.7998128361456281477 ) ) ;
#141610 = CARTESIAN_POINT ( 'NONE',  ( 6.616225513087798049, -0.8637638766970030524, -1.608286988965562214 ) ) ;
#141611 = CARTESIAN_POINT ( 'NONE',  ( -7.888146445052511169, 8.097259028849730811, 1.040834085586084257E-14 ) ) ;
#141612 = CARTESIAN_POINT ( 'NONE',  ( 5.735331106285326719, -2.048134886816056266, 0.9616036564972543221 ) ) ;
#141613 = CARTESIAN_POINT ( 'NONE',  ( 2.209725257209711469, -0.4604840958662699268, 2.054942820982478935 ) ) ;
#141614 = CARTESIAN_POINT ( 'NONE',  ( -5.936491157937300756, 8.019268665717216749, 1.599625672291263179 ) ) ;
#141615 = CARTESIAN_POINT ( 'NONE',  ( 8.860417081730671995, 10.29590700256267155, 1.199719254218453823 ) ) ;
#141616 = CARTESIAN_POINT ( 'NONE',  ( 7.146556367734771875, 8.470642196179646533, 1.082531754730549967 ) ) ;
#141617 = FILL_AREA_STYLE ('',( #187109 ) ) ;
#141618 = CARTESIAN_POINT ( 'NONE',  ( -5.865874016206865882, 9.995270118883347266, 0.000000000000000000 ) ) ;
#141619 = CARTESIAN_POINT ( 'NONE',  ( -3.777115976154627131, 7.353790098116948393, -0.6809694117130314917 ) ) ;
#141620 = CARTESIAN_POINT ( 'NONE',  ( 6.277061933002769045, 10.26706332190449622, 0.7216878364870438212 ) ) ;
#141621 = CARTESIAN_POINT ( 'NONE',  ( 4.007874524826865681, 7.816931064126571016, 0.2151701594551927443 ) ) ;
#141622 = CARTESIAN_POINT ( 'NONE',  ( -4.076197739202962467, 7.907314462378773001, 1.040834085586084257E-14 ) ) ;
#141623 = CARTESIAN_POINT ( 'NONE',  ( 3.779691724966814270, 0.2693221142107836696, -2.204936161957889329 ) ) ;
#141624 = CARTESIAN_POINT ( 'NONE',  ( 0.1533209562146371774, -1.769702838771534559, 1.318327933512997152 ) ) ;
#141626 = AXIS2_PLACEMENT_3D ( 'NONE', #40436, #106537, #122838 ) ;
#141625 = CARTESIAN_POINT ( 'NONE',  ( -4.261005416444848315, 8.193199762486115034, 0.7998128361456352531 ) ) ;
#141627 = CARTESIAN_POINT ( 'NONE',  ( 4.961394147597008697, 7.875711374583454827, -1.199719254218452047 ) ) ;
#141628 = CARTESIAN_POINT ( 'NONE',  ( 4.791432466842788784, -1.794507165602466037, 0.7932701521168731285 ) ) ;
#141629 = CARTESIAN_POINT ( 'NONE',  ( 9.077347539549325717, 10.54899253668443393, -1.199719254218446718 ) ) ;
#141631 =( BOUNDED_SURFACE ( )  B_SPLINE_SURFACE ( 3, 3, ( 
 ( #198177, #49810, #115937, #2089, #135348, #185120, #134295, #68163, #83360, #166766, #50879 ),
 ( #133227, #3158, #199232, #168886, #117002, #20490, #119138, #18361, #200302, #51954, #184063 ),
 ( #201362, #167826, #19425, #85504, #151591, #69230, #36745, #8515, #104980, #74596, #155849 ),
 ( #25825, #188332, #123442, #189404, #124498, #71363, #39972, #169949, #157995, #89805, #122375 ),
 ( #107155, #171020, #22617, #137479, #88726, #103903, #187268, #38894, #203493, #106079, #121292 ),
 ( #154784, #75660, #6369, #9584, #72438, #141767, #55146, #41046, #138539, #140700, #190457 ),
 ( #204563, #56211, #172102, #23695, #7436, #173180, #73517, #24760, #139619, #205642, #186192 ) ),
 .UNSPECIFIED., .T., .F., .T. ) 
 B_SPLINE_SURFACE_WITH_KNOTS ( ( 4, 3, 4 ),
 ( 4, 1, 1, 1, 1, 1, 1, 1, 4 ),
 ( 0.000000000000000000, 0.5000000000000000000, 1.000000000000000000 ),
 ( 0.000000000000000000, 0.2257091236145174484, 0.3979912149639216468, 0.5260416812932605657, 0.6190739408849097458, 0.6862087210430605211, 0.7361363507675404705, 0.7768852254246026989, 0.9999999999999998890 ),
 .UNSPECIFIED. ) 
 GEOMETRIC_REPRESENTATION_ITEM ( )  RATIONAL_B_SPLINE_SURFACE ( (
 ( 1.000000000000000222, 1.000000000000000222, 1.000000000000000000, 1.000000000000000000, 1.000000000000000222, 1.000000000000000000, 1.000000000000000000, 1.000000000000000000, 1.000000000000000222, 1.000000000000000000, 1.000000000000000000),
 ( 0.3333333333333334259, 0.3333333333333334259, 0.3333333333333333148, 0.3333333333333333703, 0.3333333333333334259, 0.3333333333333333703, 0.3333333333333333703, 0.3333333333333334259, 0.3333333333333333703, 0.3333333333333333703, 0.3333333333333333703),
 ( 0.3333333333333334259, 0.3333333333333334259, 0.3333333333333333148, 0.3333333333333333703, 0.3333333333333334259, 0.3333333333333333703, 0.3333333333333333703, 0.3333333333333334259, 0.3333333333333333703, 0.3333333333333333703, 0.3333333333333333703),
 ( 1.000000000000000222, 1.000000000000000222, 1.000000000000000000, 1.000000000000000000, 1.000000000000000222, 1.000000000000000000, 1.000000000000000000, 1.000000000000000000, 1.000000000000000222, 1.000000000000000000, 1.000000000000000000),
 ( 0.3333333333333334259, 0.3333333333333334259, 0.3333333333333333148, 0.3333333333333333703, 0.3333333333333334259, 0.3333333333333333703, 0.3333333333333333703, 0.3333333333333334259, 0.3333333333333333703, 0.3333333333333333703, 0.3333333333333333703),
 ( 0.3333333333333334259, 0.3333333333333334259, 0.3333333333333333148, 0.3333333333333333703, 0.3333333333333334259, 0.3333333333333333703, 0.3333333333333333703, 0.3333333333333334259, 0.3333333333333333703, 0.3333333333333333703, 0.3333333333333333703),
 ( 1.000000000000000222, 1.000000000000000222, 1.000000000000000000, 1.000000000000000000, 1.000000000000000222, 1.000000000000000000, 1.000000000000000000, 1.000000000000000000, 1.000000000000000222, 1.000000000000000000, 1.000000000000000000) ) ) 
 REPRESENTATION_ITEM ( '' )  SURFACE ( )  );
#141630 = CARTESIAN_POINT ( 'NONE',  ( -4.980508561475621043, 6.629897003107849685, 1.243112925831350246 ) ) ;
#141632 = CARTESIAN_POINT ( 'NONE',  ( -1.404019654740992440, 1.209281689291645367, 1.481605035838516216 ) ) ;
#141633 = CARTESIAN_POINT ( 'NONE',  ( -0.6823417656250003738, -0.03229166632524871350, -1.181850606188749264 ) ) ;
#141634 = CARTESIAN_POINT ( 'NONE',  ( -3.363831509966363598, 5.978201624052440266, -1.082531754730548412 ) ) ;
#141635 = CARTESIAN_POINT ( 'NONE',  ( -4.758548728716557541, 8.495464583570553785, 1.040834085586084257E-14 ) ) ;
#141636 = CARTESIAN_POINT ( 'NONE',  ( 3.867525618572264623, -1.764951123045129577, -1.175235903013646332 ) ) ;
#141637 = CARTESIAN_POINT ( 'NONE',  ( -5.798046968499580345, 6.793418213784815585, 1.199719254218452935 ) ) ;
#141638 = CARTESIAN_POINT ( 'NONE',  ( 5.207972885698374022, -2.151664816535401314, 0.2080130470862306957 ) ) ;
#141639 = CARTESIAN_POINT ( 'NONE',  ( 3.720104550828434942, 1.749555917645674530, 0.5740644926693627692 ) ) ;
#141640 = CARTESIAN_POINT ( 'NONE',  ( 5.014861385384292269, 0.1531656238677771009, 2.010801456750747285 ) ) ;
#141641 = CARTESIAN_POINT ( 'NONE',  ( -5.626640144655740805, 6.175545741207232098, 0.8476793345565808435 ) ) ;
#141642 = CARTESIAN_POINT ( 'NONE',  ( 0.6823417656249882723, 0.9885416670080832136, -1.181850606188749264 ) ) ;
#141643 = CARTESIAN_POINT ( 'NONE',  ( 6.615217694991038400, -1.686041314625020160, 0.4309386324203681728 ) ) ;
#141644 = CARTESIAN_POINT ( 'NONE',  ( 6.827182134110200806, 7.053609659044731472, 2.309100207511079805 ) ) ;
#141645 = CARTESIAN_POINT ( 'NONE',  ( 2.250290310188348464, 5.569163095287620990, 0.7216878364870438212 ) ) ;
#141646 = DIRECTION ( 'NONE',  ( 0.5131086435338283458, 0.8583236685137343169, -5.551115123125796507E-16 ) ) ;
#141647 = CARTESIAN_POINT ( 'NONE',  ( 3.625982885822197410, -1.285997354380935098, -1.737435825693343094 ) ) ;
#141648 = CARTESIAN_POINT ( 'NONE',  ( 6.046249930811113060, 1.863882344683247094, -0.7690052245405626374 ) ) ;
#141649 = CARTESIAN_POINT ( 'NONE',  ( -7.768458830506062007, 11.04665715469030296, 1.082531754730549967 ) ) ;
#141650 = CARTESIAN_POINT ( 'NONE',  ( 3.204151765443470357, -2.159293047372488950, 0.1044485798024074874 ) ) ;
#141651 = CARTESIAN_POINT ( 'NONE',  ( 3.339098322719173062, -1.740117145613935268, 0.9263661929081908886 ) ) ;
#141652 = CARTESIAN_POINT ( 'NONE',  ( -0.4382560683119304801, -7.666862915010147717, 10.99126615174920119 ) ) ;
#141653 = CARTESIAN_POINT ( 'NONE',  ( 1.149971759812302263, -1.820915985741960785, -1.417348977311111202 ) ) ;
#141654 = CARTESIAN_POINT ( 'NONE',  ( 2.565760370094140264, 2.021647365152558606, -0.3987750144259157858 ) ) ;
#141655 = CARTESIAN_POINT ( 'NONE',  ( 5.126486101458046285, 0.1468865524030492364, 1.936578770319798748 ) ) ;
#141659 = EDGE_LOOP ( 'NONE', ( #149677, #63823, #153791, #95530 ) ) ;
#141658 = ADVANCED_FACE ( 'NONE', ( #67935 ), #163356, .F. ) ;
#141657 = CARTESIAN_POINT ( 'NONE',  ( -6.908358566921340760, -6.724344753046663570, 6.684387857553240941 ) ) ;
#141656 = CARTESIAN_POINT ( 'NONE',  ( -7.497295758232720431, 10.73030023703809555, -1.082531754730543083 ) ) ;
#141660 = CARTESIAN_POINT ( 'NONE',  ( -7.442499979258930587, 7.647614495415686164, -0.7998128361456362523 ) ) ;
#141661 = CARTESIAN_POINT ( 'NONE',  ( -4.260029445439585061, 7.236136616047151193, -2.500000000000000444 ) ) ;
#141663 = ORIENTED_EDGE ( 'NONE', *, *, #46527, .F. ) ;
#141662 = CARTESIAN_POINT ( 'NONE',  ( -4.630991987519598396, 7.560518531151607213, 1.199719254218452935 ) ) ;
#141664 = CARTESIAN_POINT ( 'NONE',  ( -7.090551149822745813, 9.295395646258437949, 1.443375672974078761 ) ) ;
#141665 = CARTESIAN_POINT ( 'NONE',  ( 2.591098708763440062, -0.3764507303484417311, -2.174265822884546395 ) ) ;
#141666 = CARTESIAN_POINT ( 'NONE',  ( 2.960184520039609524, -4.197067588314596698, -1.425549731837409961 ) ) ;
#141667 = CARTESIAN_POINT ( 'NONE',  ( 6.684431423333510480, 1.132142624513672091, -1.601896353945003071 ) ) ;
#141668 = CARTESIAN_POINT ( 'NONE',  ( -0.02900071798685524560, 0.6937575422599016051, -2.255700163050919471 ) ) ;
#141669 = CARTESIAN_POINT ( 'NONE',  ( 1.499999999999989120, 4.785416667349486453, 0.8660254037844524744 ) ) ;
#141670 = SURFACE_SIDE_STYLE ('',( #173075 ) ) ;
#141671 = CARTESIAN_POINT ( 'NONE',  ( 0.07479286986302942364, 7.629137130509078268, -2.455503679634089220 ) ) ;
#141672 = CARTESIAN_POINT ( 'NONE',  ( 5.683513393433289096, -0.8240744568873883402, 1.646495476055845231 ) ) ;
#141673 = VERTEX_POINT ( 'NONE', #65803 ) ;
#141674 = CARTESIAN_POINT ( 'NONE',  ( 2.307559741017367383, -0.4527674059561050401, 2.010364544233154138 ) ) ;
#141675 = CARTESIAN_POINT ( 'NONE',  ( -1.360316468749999119, 0.3906250003414130090, -8.673617379884035472E-15 ) ) ;
#141676 = ADVANCED_FACE ( 'NONE', ( #181704 ), #5738, .T. ) ;
#141677 = CARTESIAN_POINT ( 'NONE',  ( -8.016948904382338981, 8.247528564734524892, -0.7998128361456291469 ) ) ;
#141678 = CARTESIAN_POINT ( 'NONE',  ( 11.94650005372637835, 11.15102700337638097, 1.135399707157307203 ) ) ;
#141679 = CARTESIAN_POINT ( 'NONE',  ( 10.35986303813127307, 9.178481322669741260, 6.010608889982933078 ) ) ;
#141680 = CARTESIAN_POINT ( 'NONE',  ( 5.281064527722868718, 6.119995689553514140, 1.199719254218462483 ) ) ;
#141681 = CARTESIAN_POINT ( 'NONE',  ( 0.7958619820324459582, -0.7424864502722209325, 1.922671381412993652 ) ) ;
#141684 = CARTESIAN_POINT ( 'NONE',  ( 5.214338956685347526, 1.703448749313410282, 0.6994016148276983591 ) ) ;
#141683 = CARTESIAN_POINT ( 'NONE',  ( 1.679899622522099012, -1.030144609347281026, -1.549723197825584764 ) ) ;
#141682 = CARTESIAN_POINT ( 'NONE',  ( -9.579665964948882007, -7.473374494045003757, 5.204170427930421283E-15 ) ) ;
#141685 = CARTESIAN_POINT ( 'NONE',  ( 6.958359152311676787, 9.141171649162195934, -1.599625672291262513 ) ) ;
#141686 = CARTESIAN_POINT ( 'NONE',  ( -9.404393215816320151, 14.49025778602134551, -7.453732457429351754 ) ) ;
#141687 = CARTESIAN_POINT ( 'NONE',  ( -4.769436176957319695, 8.786368983084006601, 0.7998128361456281477 ) ) ;
#141689 = VERTEX_POINT ( 'NONE', #81620 ) ;
#141688 = CARTESIAN_POINT ( 'NONE',  ( -0.4019237886466933696, 10.55133545031537423, 1.500000000000005995 ) ) ;
#141690 = CARTESIAN_POINT ( 'NONE',  ( 5.022202109028018668, -1.178465353167540197, -1.865713892744431446 ) ) ;
#141691 = CARTESIAN_POINT ( 'NONE',  ( 0.4214394802095830506, -0.1064560406111268731, 2.159113264384164399 ) ) ;
#141692 = AXIS2_PLACEMENT_3D ( 'NONE', #77974, #162441, #191711 ) ;
#141693 = CARTESIAN_POINT ( 'NONE',  ( -4.419594888374909658, 8.100018436505289188, 0.7216878364870458196 ) ) ;
#141694 = CARTESIAN_POINT ( 'NONE',  ( -0.1933232215488022709, -0.4202133615931051835, -1.872389726556406897 ) ) ;
#141695 = CARTESIAN_POINT ( 'NONE',  ( -0.2058462039469660110, -0.8663896114125648751, -1.819200108291472606 ) ) ;
#141696 = CARTESIAN_POINT ( 'NONE',  ( -4.623281625960056651, 5.318713365471549714, 1.186903574614258439 ) ) ;
#141697 = VECTOR ( 'NONE', #212088, 1000.000000000000000 ) ;
#141698 = CARTESIAN_POINT ( 'NONE',  ( 8.029509147085835963, 15.33973900756292252, -8.919384641555231141 ) ) ;
#141699 = CARTESIAN_POINT ( 'NONE',  ( 5.830699381415811899, 1.280921311228696347, -1.420062396151056117 ) ) ;
#141700 = CARTESIAN_POINT ( 'NONE',  ( -15.75000000000000000, 13.40000000000000036, 1.099999999999996758 ) ) ;
#141701 = EDGE_CURVE ( 'NONE', #26543, #5628, #195896, .T. ) ;
#141702 = CARTESIAN_POINT ( 'NONE',  ( 0.7955152940811484052, -0.6771210053572243037, 1.743984199989514927 ) ) ;
#141703 = CARTESIAN_POINT ( 'NONE',  ( 2.167204200501818612, 1.841733140229084853, -0.8216742516050157263 ) ) ;
#141705 = CARTESIAN_POINT ( 'NONE',  ( 4.283879487498391647, 1.375451533845202245, 1.594966088981208729 ) ) ;
#141704 = CARTESIAN_POINT ( 'NONE',  ( -8.877891658850122880, 9.251961778280284321, 0.7998128361456462443 ) ) ;
#141706 = CARTESIAN_POINT ( 'NONE',  ( 7.476431642932036326, 10.80992178580769014, 1.199719254218460707 ) ) ;
#141708 = CARTESIAN_POINT ( 'NONE',  ( -9.338868881714763148, 9.789768538289042255, -0.7998128361456291469 ) ) ;
#141707 = CARTESIAN_POINT ( 'NONE',  ( 1.499999999999987566, -0.4749999999999823808, 0.000000000000000000 ) ) ;
#141709 =( NAMED_UNIT ( * ) PLANE_ANGLE_UNIT ( ) SI_UNIT ( $, .RADIAN. ) );
#141710 = CARTESIAN_POINT ( 'NONE',  ( 3.902606965841335818, -1.998407076283228223, -0.2920856897847978195 ) ) ;
#141711 = CARTESIAN_POINT ( 'NONE',  ( 1.364683531249988535, 4.155208333674753618, -0.7879004041258239610 ) ) ;
#141712 = CARTESIAN_POINT ( 'NONE',  ( 8.419250204406344196, 12.76628297187536809, 1.040834085586084257E-14 ) ) ;
#141713 = CARTESIAN_POINT ( 'NONE',  ( 4.077527805175058973, 2.036875575534887961, -0.7240464584713502960 ) ) ;
#141714 = CARTESIAN_POINT ( 'NONE',  ( 6.393551957296131683, 9.616838495890963401, 1.199719254218452047 ) ) ;
#141715 = CARTESIAN_POINT ( 'NONE',  ( -0.7499999999999972244, 5.608333333333353821, -1.299038105676652011 ) ) ;
#141717 = FACE_OUTER_BOUND ( 'NONE', #166573, .T. ) ;
#141716 = CARTESIAN_POINT ( 'NONE',  ( 4.908934136599710563, 7.884784371745123366, 1.199719254218451159 ) ) ;
#141718 = CARTESIAN_POINT ( 'NONE',  ( 7.361714222096048310, 10.57212177821199184, -1.082531754730537976 ) ) ;
#141720 = CARTESIAN_POINT ( 'NONE',  ( -1.823506805412349330, 2.449817705437798754, -2.460149088936845807 ) ) ;
#141719 = CARTESIAN_POINT ( 'NONE',  ( 1.785821596895339702, -2.044763721651895239, 0.7304308730638265912 ) ) ;
#141722 = CARTESIAN_POINT ( 'NONE',  ( 0.8020088176248600931, 1.394402496181508466, -1.202495849378336423 ) ) ;
#141721 = CARTESIAN_POINT ( 'NONE',  ( -6.480434237652138663, 8.583592582059388576, 1.443375672974078761 ) ) ;
#141723 = CARTESIAN_POINT ( 'NONE',  ( 1.364683531249986537, 2.155208333674751398, -0.7879004041258239610 ) ) ;
#141725 = CARTESIAN_POINT ( 'NONE',  ( 2.243918346939121733, 2.191141468336772036, 0.05030144379260945153 ) ) ;
#141724 = B_SPLINE_CURVE_WITH_KNOTS ( 'NONE', 3,
 ( #42105, #141757, #92986, #45291 ),
 .UNSPECIFIED., .F., .F.,
 ( 4, 4 ),
 ( 0.000000000000000000, 0.0002564548269640155843 ),
 .UNSPECIFIED. ) ;
#141726 = CARTESIAN_POINT ( 'NONE',  ( -9.529120656610874963E-19, -8.332912386296857932, 10.92578969873750161 ) ) ;
#141727 = CARTESIAN_POINT ( 'NONE',  ( 3.292113192954935208, -0.9186832275986864804, 2.067785417532372438 ) ) ;
#141728 = CARTESIAN_POINT ( 'NONE',  ( -6.723954117373590833, 9.932031339322813679, -1.199719254218440723 ) ) ;
#141729 = CARTESIAN_POINT ( 'NONE',  ( 0.6823417656249899377, 4.488541667008086655, -1.181850606188754593 ) ) ;
#141730 = CARTESIAN_POINT ( 'NONE',  ( 6.170003545802125622, 6.961323287618347955, -0.9016653442153206299 ) ) ;
#141731 = CARTESIAN_POINT ( 'NONE',  ( -1.500000000000001110, 12.27083333333333925, 0.8660254037844419273 ) ) ;
#141732 = CARTESIAN_POINT ( 'NONE',  ( 5.695833931516881776, 9.659240330162777610, -0.7216878364870458196 ) ) ;
#141733 = CARTESIAN_POINT ( 'NONE',  ( 4.868267778354250730, -1.156333057219432581, 1.339767963349105528 ) ) ;
#141734 =( GEOMETRIC_REPRESENTATION_CONTEXT ( 3 ) GLOBAL_UNCERTAINTY_ASSIGNED_CONTEXT ( ( #33171 ) ) GLOBAL_UNIT_ASSIGNED_CONTEXT ( ( #177270, #63515, #14741 ) ) REPRESENTATION_CONTEXT ( 'NONE', 'WORKASPACE' ) );
#141735 = CARTESIAN_POINT ( 'NONE',  ( 9.694243528971124846, 11.26870452434320491, 1.199719254218450271 ) ) ;
#141736 = CARTESIAN_POINT ( 'NONE',  ( 0.4113322892924773377, 1.832542443981843405, 1.037592781499405259 ) ) ;
#141738 = CARTESIAN_POINT ( 'NONE',  ( -1.201851678989727383E-14, 1.712500000000019229, 1.732050807568877637 ) ) ;
#141737 = CARTESIAN_POINT ( 'NONE',  ( -1.364683531250010295, 10.38020833367473195, 0.7879004041258445001 ) ) ;
#141739 = CARTESIAN_POINT ( 'NONE',  ( 0.6956774629466413451, -1.390297546174504850, -1.395334862655448260 ) ) ;
#141740 = CARTESIAN_POINT ( 'NONE',  ( -5.418418667316934112, 6.350518529071726981, -1.199719254218453823 ) ) ;
#141741 = CYLINDRICAL_SURFACE ( 'NONE', #18505, 4.000000000000000000 ) ;
#141742 = ORIENTED_EDGE ( 'NONE', *, *, #153335, .T. ) ;
#141743 = CARTESIAN_POINT ( 'NONE',  ( 6.480434237652121787, 9.543961796360731498, 1.082531754730558626 ) ) ;
#141744 = CARTESIAN_POINT ( 'NONE',  ( 4.487079325084206260, 1.670935625628103605, -0.8411387520786616223 ) ) ;
#141745 = CARTESIAN_POINT ( 'NONE',  ( 4.030184149050713316, 1.145922430192683805, 1.723988044715177859 ) ) ;
#141746 = CARTESIAN_POINT ( 'NONE',  ( 0.6124999999999914957, 2.083333333333339699, 1.060881119635884051 ) ) ;
#141747 = CARTESIAN_POINT ( 'NONE',  ( -5.546694241322218666, 8.524874810634301525, 1.082531754730550855 ) ) ;
#141748 = CARTESIAN_POINT ( 'NONE',  ( 3.338979018791977449, -0.9437212195340001220, 0.5034934222078586430 ) ) ;
#141749 = CARTESIAN_POINT ( 'NONE',  ( 9.088043039861931405, 9.497138389460751284, 1.040834085586084257E-14 ) ) ;
#141750 = CARTESIAN_POINT ( 'NONE',  ( -10.10098813738111545, 11.74323990082152491, -1.199719254218441611 ) ) ;
#141751 = CARTESIAN_POINT ( 'NONE',  ( 5.657495238652423097, 9.822437888394988548, 0.000000000000000000 ) ) ;
#141752 = CARTESIAN_POINT ( 'NONE',  ( 0.000000000000000000, -6.532648833121157850, 0.000000000000000000 ) ) ;
#141753 = CARTESIAN_POINT ( 'NONE',  ( 1.364683531249990311, 5.176041667008085767, 0.7879004041258500513 ) ) ;
#141754 = CARTESIAN_POINT ( 'NONE',  ( 4.070719198475009293, 1.388998261151509039, -1.385754695631277844 ) ) ;
#141755 = CARTESIAN_POINT ( 'NONE',  ( 1.757185253014027282, -2.006138798620077157, -0.2004061740628823030 ) ) ;
#141756 = CARTESIAN_POINT ( 'NONE',  ( -0.1104750535120025967, -0.004616138082884357029, -2.103378236956429337 ) ) ;
#141757 = CARTESIAN_POINT ( 'NONE',  ( 4.097995649369902793, 7.467253099217946222, -0.6374303210496650163 ) ) ;
#141758 = CARTESIAN_POINT ( 'NONE',  ( 0.7373108528737730705, -1.318359053027039263, -1.327247110734230962 ) ) ;
#141759 = CARTESIAN_POINT ( 'NONE',  ( 1.364683531249988535, 3.905208333674751842, -0.7879004041258239610 ) ) ;
#141760 = CARTESIAN_POINT ( 'NONE',  ( 3.498294685330126441, -0.9886941555459362041, 1.753605845479579095 ) ) ;
#141762 = CARTESIAN_POINT ( 'NONE',  ( 3.181382749799996468, 1.670748044588391990, 1.300414933884207480 ) ) ;
#141761 = CARTESIAN_POINT ( 'NONE',  ( -7.076992996653451939, 7.358839372291564374, 0.7216878364870317197 ) ) ;
#141763 = CARTESIAN_POINT ( 'NONE',  ( 6.825078400183572036, 7.051914997414900022, 2.742498282622223726 ) ) ;
#141764 = CARTESIAN_POINT ( 'NONE',  ( 4.352052382902608763, -0.7952921280917917279, 1.911720769834825973 ) ) ;
#141765 = CARTESIAN_POINT ( 'NONE',  ( 8.005163354226054295, 8.304055099544019214, 0.000000000000000000 ) ) ;
#141767 = CARTESIAN_POINT ( 'NONE',  ( 6.620655732516615544, 2.958939621373418483, 2.526443930770333246 ) ) ;
#141766 = CARTESIAN_POINT ( 'NONE',  ( 0.6266517258138035729, 0.1575598857218879489, 2.084883927750030175 ) ) ;
#141769 = ORIENTED_EDGE ( 'NONE', *, *, #20625, .F. ) ;
#141768 = CARTESIAN_POINT ( 'NONE',  ( 5.122008332510333162, -0.9777984688263160473, -1.541441239866998103 ) ) ;
#141770 = CARTESIAN_POINT ( 'NONE',  ( 8.320953590485093088, 10.73086516036454618, 1.599625672291281386 ) ) ;
#141771 = CARTESIAN_POINT ( 'NONE',  ( 3.332168893502668539, 7.719402352560120306, -2.450693629706207854 ) ) ;
#141772 = CARTESIAN_POINT ( 'NONE',  ( 9.687436728043250511, 13.40831512142563042, -8.157569025435085663 ) ) ;
#141773 = CIRCLE ( 'NONE', #197075, 0.08000000000000012657 ) ;
#141774 = CARTESIAN_POINT ( 'NONE',  ( -10.52476609942256758, 3.676887381874808902, 5.198941853688804571 ) ) ;
#141775 = CARTESIAN_POINT ( 'NONE',  ( 0.6823417656249969321, 12.33854166700806765, -1.181850606188757036 ) ) ;
#141776 = CARTESIAN_POINT ( 'NONE',  ( -0.09351100681491937572, -0.3904691765420374439, -1.774915231904458990 ) ) ;
#141777 = CARTESIAN_POINT ( 'NONE',  ( -8.646349277213090545, 11.11049346154719508, 1.599625672291269396 ) ) ;
#141778 = CARTESIAN_POINT ( 'NONE',  ( 4.984594031318565932, 8.967110136513669616, 0.7998128361456462443 ) ) ;
#141779 = CARTESIAN_POINT ( 'NONE',  ( 2.860407222358956503, 6.280966159486672140, 0.7216878364870338292 ) ) ;
#141780 = CARTESIAN_POINT ( 'NONE',  ( 9.492905263954437345, -8.233136995002492853, -0.3773006915670611416 ) ) ;
#141781 = CARTESIAN_POINT ( 'NONE',  ( 3.551346171775753735, 6.230655402791975384, 1.199719254218462483 ) ) ;
#141782 = ORIENTED_EDGE ( 'NONE', *, *, #187807, .F. ) ;
#141783 = ADVANCED_FACE ( 'NONE', ( #36854 ), #113130, .F. ) ;
#141784 = PRODUCT_DEFINITION ( 'UNKNOWN', '', #180335, #115456 ) ;
#141785 = CARTESIAN_POINT ( 'NONE',  ( -6.774234028683526532, 7.932303117332766718, 1.199719254218452047 ) ) ;
#141786 = AXIS2_PLACEMENT_3D ( 'NONE', #121279, #5274, #137467 ) ;
#141787 = CARTESIAN_POINT ( 'NONE',  ( 5.114861317887108072, 0.1511565883688982259, 2.010826320608386730 ) ) ;
#141789 = CARTESIAN_POINT ( 'NONE',  ( 6.017840079619279692, 8.114175741012878973, -1.599625672291281386 ) ) ;
#141788 = DIRECTION ( 'NONE',  ( 0.000000000000000000, 0.000000000000000000, 1.000000000000000000 ) ) ;
#141790 = SURFACE_SIDE_STYLE ('',( #193680 ) ) ;
#141791 = CARTESIAN_POINT ( 'NONE',  ( -0.1405533004718312329, 2.055874972810427526, -2.136773944524199109 ) ) ;
#141792 = CARTESIAN_POINT ( 'NONE',  ( -5.612712406377534435, 5.650512016969639895, 0.7216878364870317197 ) ) ;
#141793 = CARTESIAN_POINT ( 'NONE',  ( 3.602716132929354664, 5.226254793216122074, 1.599625672291267398 ) ) ;
#141794 = CARTESIAN_POINT ( 'NONE',  ( 2.553506168856953806, 1.519147476331883517, 1.253303911792477132 ) ) ;
#141795 = CARTESIAN_POINT ( 'NONE',  ( 3.093375225471244772, -0.3905761854139707667, 1.978056131710544063 ) ) ;
#141796 = CARTESIAN_POINT ( 'NONE',  ( -8.128276786592724790, 9.441743324901704426, -1.199719254218446718 ) ) ;
#141797 = CARTESIAN_POINT ( 'NONE',  ( 6.727182134110176293, 6.032839922080010631, 2.883943260000087605 ) ) ;
#141798 = CARTESIAN_POINT ( 'NONE',  ( 4.048915112334880106, -1.821525731582713359, -1.218098874207810933 ) ) ;
#141799 = CARTESIAN_POINT ( 'NONE',  ( 1.580854408705430370, 0.9623865910009720137, 1.305104700536227957 ) ) ;
#141800 = CARTESIAN_POINT ( 'NONE',  ( 2.414956338186133422, 1.719780681555121982, 0.8681123839546500687 ) ) ;
#141801 = CARTESIAN_POINT ( 'NONE',  ( -7.971304249830880373, 11.38727316052296601, 1.199719254218453823 ) ) ;
#141802 = FILL_AREA_STYLE ('',( #206746 ) ) ;
#141803 = CARTESIAN_POINT ( 'NONE',  ( 0.2333540202161610289, 7.629137130509112907, -2.645727818377396900 ) ) ;
#141804 = CARTESIAN_POINT ( 'NONE',  ( 0.000000000000000000, 0.000000000000000000, 0.000000000000000000 ) ) ;
#141805 = CARTESIAN_POINT ( 'NONE',  ( 6.747154001095143627, 11.02343010125301959, -0.7998128361456291469 ) ) ;
#141806 = EDGE_CURVE ( 'NONE', #5998, #7325, #162888, .T. ) ;
#141807 = CARTESIAN_POINT ( 'NONE',  ( 5.931855901178834323, 6.879252291918818152, 1.199719254218462483 ) ) ;
#141808 =( BOUNDED_CURVE ( )  B_SPLINE_CURVE ( 2, ( #166567, #51760, #67956, #149246, #148194, #34419, #35485, #66888, #819 ),
 .UNSPECIFIED., .F., .T. ) 
 B_SPLINE_CURVE_WITH_KNOTS ( ( 3, 2, 2, 2, 3 ),
 ( 0.4843749999999997780, 0.4895833333333333148, 0.5000000000000000000, 0.5104166666666666297, 0.5156250000000002220 ),
 .UNSPECIFIED. ) 
 CURVE ( )  GEOMETRIC_REPRESENTATION_ITEM ( )  RATIONAL_B_SPLINE_CURVE ( ( 0.9330127018922194093, 0.9330127018922165227, 1.000000000000000000, 0.8660254037844387076, 1.000000000000000000, 0.8660254037844387076, 1.000000000000000000, 0.9330127018922165227, 0.9330127018922194093 ) ) 
 REPRESENTATION_ITEM ( '' )  );
#141809 = CARTESIAN_POINT ( 'NONE',  ( -6.784764760059077915, -8.039737506397905520, 6.649736275991423362 ) ) ;
#141810 = CARTESIAN_POINT ( 'NONE',  ( 5.777182853198898904, 6.873039762554409293, -1.082531754730548412 ) ) ;
#141811 = ORIENTED_EDGE ( 'NONE', *, *, #51634, .T. ) ;
#141813 = CARTESIAN_POINT ( 'NONE',  ( 2.930340344496225935, -0.9942814366015439997, -1.750357268347104256 ) ) ;
#141812 = CARTESIAN_POINT ( 'NONE',  ( 5.548353751603532835, -1.447698842669535413, 1.137588655622793876 ) ) ;
#141814 = CARTESIAN_POINT ( 'NONE',  ( 4.499567255430725332, 2.252980053716880704, 0.4539551632626090405 ) ) ;
#141816 = CARTESIAN_POINT ( 'NONE',  ( 3.766312297878508630, -0.7504043340197141809, -1.703115836376113634 ) ) ;
#141815 = CARTESIAN_POINT ( 'NONE',  ( -0.02919842301646497981, 7.629137130509056952, -2.673797582091000269 ) ) ;
#141818 = DIRECTION ( 'NONE',  ( -1.000000000000000000, 5.421010862427522170E-16, 0.000000000000000000 ) ) ;
#141817 = APPLICATION_CONTEXT ( 'automotive_design' ) ;
#141819 = CARTESIAN_POINT ( 'NONE',  ( -1.387358672534890536, 7.315968950354793776, -4.254625267136668221 ) ) ;
#141820 = CARTESIAN_POINT ( 'NONE',  ( 4.207966135563082410, 7.175396087857922822, -1.043745235818753780 ) ) ;
#141821 = CARTESIAN_POINT ( 'NONE',  ( -7.670162217029145246, 9.971608557999250166, 1.599625672291295375 ) ) ;
#141822 = CARTESIAN_POINT ( 'NONE',  ( -6.156811154381562012, 6.355570232966157640, 0.7216878364870257245 ) ) ;
#141823 = CARTESIAN_POINT ( 'NONE',  ( 6.075741423153157683, -1.117747424998961403, 1.766673535877111290 ) ) ;
#141824 = CARTESIAN_POINT ( 'NONE',  ( 7.158341918335438869, 7.453746447587225710, -0.7216878364870257245 ) ) ;
#141825 = ORIENTED_EDGE ( 'NONE', *, *, #188097, .T. ) ;
#141826 = DIRECTION ( 'NONE',  ( 0.000000000000000000, 0.000000000000000000, -1.000000000000000000 ) ) ;
#141827 = CARTESIAN_POINT ( 'NONE',  ( 3.070819976954436203, 2.800000000000017586, -2.497101503361887076 ) ) ;
#141828 = CARTESIAN_POINT ( 'NONE',  ( 6.287718881003963034, 1.195215413365672275, 1.243919913892058693 ) ) ;
#141829 = CARTESIAN_POINT ( 'NONE',  ( -4.680589345215810049, 6.483773540883647435, -1.599625672291256295 ) ) ;
#141830 = CARTESIAN_POINT ( 'NONE',  ( 1.195528834012358210, 1.529115512818737699, 0.8178816217611245554 ) ) ;
#141831 = CARTESIAN_POINT ( 'NONE',  ( 1.579999999999991189, 8.674529973577531194, 2.500000000000000444 ) ) ;
#141832 = CARTESIAN_POINT ( 'NONE',  ( -5.840764256335890359, 6.042828518458865261, -0.4463971771759592810 ) ) ;
#141833 = CARTESIAN_POINT ( 'NONE',  ( 5.366168305121062687, -2.161276524852562275, 0.2057630808787509757 ) ) ;
#141834 = CARTESIAN_POINT ( 'NONE',  ( 4.072732355924274295, -1.704239406772959153, -0.6552279023967976235 ) ) ;
#141835 = CARTESIAN_POINT ( 'NONE',  ( 2.201936455694650796, 0.7555380192853027310, -1.810630540845730385 ) ) ;
#141836 = DIRECTION ( 'NONE',  ( 0.000000000000000000, -1.000000000000000000, 0.000000000000000000 ) ) ;
#141837 = CARTESIAN_POINT ( 'NONE',  ( -10.15522075183580419, 11.80651128435196462, 1.199719254218462483 ) ) ;
#141838 = CARTESIAN_POINT ( 'NONE',  ( 8.437251666405968464, 8.737881787095446384, 1.040834085586084257E-14 ) ) ;
#141839 = PRESENTATION_LAYER_ASSIGNMENT (  '', '', ( #134861 ) ) ;
#141840 = CARTESIAN_POINT ( 'NONE',  ( 2.209781436637091367, 1.640924847721588975, 1.343087772177023131 ) ) ;
#141841 = CARTESIAN_POINT ( 'NONE',  ( -0.05503291520805722592, -6.406027784105811307, 11.00000000000011902 ) ) ;
#141842 = LINE ( 'NONE', #160178, #101213 ) ;
#141843 = CARTESIAN_POINT ( 'NONE',  ( -5.013591113304329383, 6.604120902668014992, -1.237928687022475494 ) ) ;
#141844 = CARTESIAN_POINT ( 'NONE',  ( 1.164989683304976875, 1.570165760251106990, -1.349419213858449318 ) ) ;
#141846 = CARTESIAN_POINT ( 'NONE',  ( 0.7500000000000006661, 14.36458333401613530, 1.299038105676657340 ) ) ;
#141845 = DIRECTION ( 'NONE',  ( 0.000000000000000000, 0.000000000000000000, 1.000000000000000000 ) ) ;
#141848 = ORIENTED_EDGE ( 'NONE', *, *, #192668, .F. ) ;
#141847 = CARTESIAN_POINT ( 'NONE',  ( 3.791809789012908549, 2.091298394358314550, -0.7490737107957652352 ) ) ;
#141849 = CARTESIAN_POINT ( 'NONE',  ( 0.5285108043569552994, -1.967359331218739626, 1.188758619093014168 ) ) ;
#141851 = CARTESIAN_POINT ( 'NONE',  ( 0.3562053913853078790, -1.961198556353323186, -0.05404869553313899899 ) ) ;
#141850 = CARTESIAN_POINT ( 'NONE',  ( 2.510230996824538430, 6.080353262937265413, 0.000000000000000000 ) ) ;
#141853 = CARTESIAN_POINT ( 'NONE',  ( 1.001543065824772753E-15, -3.871874999522043836, 3.793834371823811669 ) ) ;
#141852 = CARTESIAN_POINT ( 'NONE',  ( 5.903649544107831382, 5.852288987739402870, -0.7998128361456481317 ) ) ;
#141854 = CARTESIAN_POINT ( 'NONE',  ( 6.480030769895370746, -1.807141314969593848, -0.3518929191878711338 ) ) ;
#141855 =( LENGTH_UNIT ( ) NAMED_UNIT ( * ) SI_UNIT ( .MILLI., .METRE. ) );
#141856 = CARTESIAN_POINT ( 'NONE',  ( -0.1102773484824119410, 2.860927498608015984, -2.691535809252169731 ) ) ;
#141857 = CARTESIAN_POINT ( 'NONE',  ( 2.731144534912807842, -1.610196803864067938, 0.6186328129335681991 ) ) ;
#141858 = CARTESIAN_POINT ( 'NONE',  ( 0.9191581010105540628, -1.820984308097562954, 0.8666112775468014506 ) ) ;
#141859 = CARTESIAN_POINT ( 'NONE',  ( 3.005426500355699915, 1.909594650917462388, 1.212984053805040041 ) ) ;
#141860 = CARTESIAN_POINT ( 'NONE',  ( 5.074884281356676574, -1.982714853632736807, -0.7105774565657559938 ) ) ;
#141861 = CARTESIAN_POINT ( 'NONE',  ( -5.641601317062239218, 8.635599732330991429, -1.082531754730549967 ) ) ;
#141862 = CARTESIAN_POINT ( 'NONE',  ( 3.409201082634921498, -0.3482811000503453491, 1.734931447941751692 ) ) ;
#141864 = CARTESIAN_POINT ( 'NONE',  ( 6.620655732516684822, -0.005281389526603020787, 2.273887028200880511 ) ) ;
#141863 = CARTESIAN_POINT ( 'NONE',  ( 4.760321331729593375, 5.686701320840210627, -1.082531754730548412 ) ) ;
#141865 = CARTESIAN_POINT ( 'NONE',  ( 5.138538782746885580, -1.577291412575715812, 0.9494700402261007088 ) ) ;
#141866 = CARTESIAN_POINT ( 'NONE',  ( -5.786632634934295361, 5.645492917045106473, 0.7998128361456341429 ) ) ;
#141867 = CARTESIAN_POINT ( 'NONE',  ( 4.975479186090847605, 7.788180902872553268, 1.082531754730558626 ) ) ;
#141868 = CARTESIAN_POINT ( 'NONE',  ( -1.201851678989727383E-14, 3.962500000000022116, 1.732050807568877637 ) ) ;
#141869 = CARTESIAN_POINT ( 'NONE',  ( 4.382901342696458258, 1.958101449220098988, -0.9841704303943515919 ) ) ;
#141870 = CARTESIAN_POINT ( 'NONE',  ( -4.946027110887008860, 4.664786472323266153, -0.7998128361456221525 ) ) ;
#141871 = CARTESIAN_POINT ( 'NONE',  ( 0.05548385694414996461, 15.44694884557249459, 11.95573287483746583 ) ) ;
#141872 = CARTESIAN_POINT ( 'NONE',  ( 6.320769956279724155, -1.466918727022302971, 1.461273828345016845 ) ) ;
#141873 = CARTESIAN_POINT ( 'NONE',  ( -11.92046840572485777, 9.947478752057296703, -1.382231356234943309 ) ) ;
#141874 = CARTESIAN_POINT ( 'NONE',  ( 1.364683531249988535, 4.905208333674756283, -0.7879004041258300672 ) ) ;
#141875 = CARTESIAN_POINT ( 'NONE',  ( 3.299358975845566810, 1.519210379524044585, 1.184558777233129412 ) ) ;
#141876 = CARTESIAN_POINT ( 'NONE',  ( 1.364683531249996529, 10.21354166700806587, 0.7879004041258405033 ) ) ;
#141877 = CARTESIAN_POINT ( 'NONE',  ( -4.446711195602264688, 4.290177271065136466, -0.7216878364870207285 ) ) ;
#141878 = CARTESIAN_POINT ( 'NONE',  ( 0.1236698368150884464, 1.936885272324913698, 1.087587522935773876 ) ) ;
#141879 = ORIENTED_EDGE ( 'NONE', *, *, #198557, .T. ) ;
#141881 =( NAMED_UNIT ( * ) PLANE_ANGLE_UNIT ( ) SI_UNIT ( $, .RADIAN. ) );
#141880 = CARTESIAN_POINT ( 'NONE',  ( -5.343321937561608337, 5.406499480009534508, 0.7216878364870257245 ) ) ;
#141882 = CARTESIAN_POINT ( 'NONE',  ( 3.181359600701000989, 6.863336634126477875, 0.000000000000000000 ) ) ;
#141883 = DIRECTION ( 'NONE',  ( 0.000000000000000000, -0.000000000000000000, 1.000000000000000000 ) ) ;
#141884 = CARTESIAN_POINT ( 'NONE',  ( 11.92046840572485777, 11.15252124794270649, -1.382231356234943753 ) ) ;
#141885 = CARTESIAN_POINT ( 'NONE',  ( 11.90252275860789588, 7.647352740710921637, -1.095560775704444323 ) ) ;
#141886 = CARTESIAN_POINT ( 'NONE',  ( 8.202319746143333035, 12.51319743723517952, -0.7216878364870328300 ) ) ;
#141887 = CARTESIAN_POINT ( 'NONE',  ( 0.7835587076311965049, -1.864072139945194717, 0.6119401183290390511 ) ) ;
#141888 = CARTESIAN_POINT ( 'NONE',  ( 1.364683531249988757, 1.446875000341421469, 0.000000000000000000 ) ) ;
#141889 = LINE ( 'NONE', #207898, #81869 ) ;
#141890 = CARTESIAN_POINT ( 'NONE',  ( 5.512146440779991607, 1.959692598237902761, -0.09458084330612320789 ) ) ;
#141891 = CARTESIAN_POINT ( 'NONE',  ( -9.332089804907933939, 9.781859615347734405, 1.040834085586084257E-14 ) ) ;
#141892 = CARTESIAN_POINT ( 'NONE',  ( -5.544921637864833386, 7.492161215640853023, -1.443375672974051449 ) ) ;
#141893 = CARTESIAN_POINT ( 'NONE',  ( 6.649309733611729278, -1.732918351142084035, -1.292073167451508686 ) ) ;
#141895 = ORIENTED_EDGE ( 'NONE', *, *, #15710, .T. ) ;
#141894 = CARTESIAN_POINT ( 'NONE',  ( -1.782949938078044694, -3.499999999999999556, 2.093702347113241657 ) ) ;
#141896 = CARTESIAN_POINT ( 'NONE',  ( 0.7499999999999885647, -0.7354166659838470288, 1.299038105676657340 ) ) ;
#141897 = EDGE_CURVE ( 'NONE', #144032, #201878, #49285, .T. ) ;
#141898 = CARTESIAN_POINT ( 'NONE',  ( 6.872342997630815020, -1.214913955043941174, 1.553259342649115249 ) ) ;
#141899 = CARTESIAN_POINT ( 'NONE',  ( 6.222016520869273926, -1.489155408782488088, -0.8877787665630013647 ) ) ;
#141901 = CARTESIAN_POINT ( 'NONE',  ( 3.456733517523991051, -1.933646301634945885, -1.031433503814835007 ) ) ;
#141900 = CARTESIAN_POINT ( 'NONE',  ( 1.360316468749985575, 0.2864583336747233422, -0.7853790794158961308 ) ) ;
#141902 = CARTESIAN_POINT ( 'NONE',  ( 4.260959797893453249, -1.712736962785869288, 1.546631824827559454 ) ) ;
#141903 = CARTESIAN_POINT ( 'NONE',  ( 5.817669245088300300, -2.011504375995844196, 0.4472435552253516411 ) ) ;
#141904 = CARTESIAN_POINT ( 'NONE',  ( 2.255715180780485607, 0.8305992003537970847, 1.755491392210324353 ) ) ;
#141905 = CARTESIAN_POINT ( 'NONE',  ( -4.067082893975237035, 7.688754443039000464, 1.040834085586084257E-14 ) ) ;
#141906 = CARTESIAN_POINT ( 'NONE',  ( 5.519825572852568030, -0.5132647233585425628, 2.057443900658859182 ) ) ;
#141907 =( NAMED_UNIT ( * ) SI_UNIT ( $, .STERADIAN. ) SOLID_ANGLE_UNIT ( ) );
#141908 = CARTESIAN_POINT ( 'NONE',  ( 3.024064729735044921, -1.777011313454954999, 0.9530116517338580451 ) ) ;
#141909 = CARTESIAN_POINT ( 'NONE',  ( -4.568734577680880093, 7.313645526394248364, -1.082531754730548412 ) ) ;
#141910 = CARTESIAN_POINT ( 'NONE',  ( -6.312203035614172286, 9.521931420595302953, -1.199719254218452047 ) ) ;
#141911 = CARTESIAN_POINT ( 'NONE',  ( 8.224992744984721327, 12.74757530245756243, 1.040834085586084257E-14 ) ) ;
#141912 = CARTESIAN_POINT ( 'NONE',  ( 0.000000000000000000, -1.000000000000000888, 0.000000000000000000 ) ) ;
#141913 = CARTESIAN_POINT ( 'NONE',  ( -6.180537922983287302, 8.303989891604203422, -1.599625672291271394 ) ) ;
#141914 = CARTESIAN_POINT ( 'NONE',  ( -0.01291931824900539524, 15.45162602843430300, 11.96434918058137242 ) ) ;
#141915 = CARTESIAN_POINT ( 'NONE',  ( 1.491528662501849123, 8.751894132169937279, -2.513572095680560281 ) ) ;
#141916 = EDGE_LOOP ( 'NONE', ( #143809, #34880, #202971, #111254, #162784 ) ) ;
#141917 = CARTESIAN_POINT ( 'NONE',  ( 5.946181061342999286, 2.058424064105804696, 0.1035008386942332104 ) ) ;
#141918 = CARTESIAN_POINT ( 'NONE',  ( -7.282137903871469753, 8.628820655005750240, 1.082531754730549078 ) ) ;
#141919 = EDGE_CURVE ( 'NONE', #176022, #23505, #49140, .T. ) ;
#141920 = CARTESIAN_POINT ( 'NONE',  ( 6.471393748265543699, 5.229711127717882491, 2.420000000000010587 ) ) ;
#141921 = CARTESIAN_POINT ( 'NONE',  ( -5.440899717785814715, 5.242137847038546461, 0.7998128361456341429 ) ) ;
#141922 = CARTESIAN_POINT ( 'NONE',  ( 4.899084735882781594, -0.2492385452713632155, -2.004177415419911679 ) ) ;
#141924 = ORIENTED_EDGE ( 'NONE', *, *, #142048, .T. ) ;
#141923 = CARTESIAN_POINT ( 'NONE',  ( -1.500000000000001332, 0.9000000000000187850, 0.000000000000000000 ) ) ;
#141926 = CARTESIAN_POINT ( 'NONE',  ( 8.080296364064698977, 12.37083682481011060, -0.7216878364870328300 ) ) ;
#141925 = CARTESIAN_POINT ( 'NONE',  ( -4.142898457427624415, 6.991076079377632091, 1.199719254218452935 ) ) ;
#141927 = CARTESIAN_POINT ( 'NONE',  ( 5.524057522564145728, 8.532151978711786100, 1.199719254218462483 ) ) ;
#141928 = CARTESIAN_POINT ( 'NONE',  ( 3.854412985283267368, 0.7401793164230722200, 1.923571582979522798 ) ) ;
#141929 = CARTESIAN_POINT ( 'NONE',  ( 3.006482587178582300, -1.942541511447487990, 0.5404910644229294903 ) ) ;
#141930 = ORIENTED_EDGE ( 'NONE', *, *, #150147, .T. ) ;
#141931 = CARTESIAN_POINT ( 'NONE',  ( 1.907519672996875082, 3.236073672982398008, -0.4612874649729831744 ) ) ;
#141932 = CARTESIAN_POINT ( 'NONE',  ( 4.517891501851804215, 6.293959390292322986, -1.599625672291255185 ) ) ;
#141934 = VERTEX_POINT ( 'NONE', #114203 ) ;
#141933 = CARTESIAN_POINT ( 'NONE',  ( -11.41381675112453387, 10.19999999999998153, 3.704697986577180746 ) ) ;
#141935 = CARTESIAN_POINT ( 'NONE',  ( 5.788239156490550208, 7.236076679697275083, -1.185412701995581797 ) ) ;
#141936 = CARTESIAN_POINT ( 'NONE',  ( 2.688827190807027367, -1.158510681541668141, -1.649829502315000251 ) ) ;
#141937 = CARTESIAN_POINT ( 'NONE',  ( 2.571990918753517708, -1.761868631437716548, -0.5344257538507578564 ) ) ;
#141938 = CARTESIAN_POINT ( 'NONE',  ( 1.383892495861089644, 2.130622466349596511, -0.8869745915042435147 ) ) ;
#141939 = CARTESIAN_POINT ( 'NONE',  ( 5.747730777550676073, 5.670383760089384495, 0.000000000000000000 ) ) ;
#141940 = CARTESIAN_POINT ( 'NONE',  ( 3.409602121571019051, -0.4253414365745535886, 2.119164713334599881 ) ) ;
#141941 = CARTESIAN_POINT ( 'NONE',  ( 9.582915646760733708, 10.07448976417602893, 0.7998128361456462443 ) ) ;
#141942 = CARTESIAN_POINT ( 'NONE',  ( -6.250472511100020334, 7.250971670160158311, 1.199719254218450271 ) ) ;
#141943 = ORIENTED_EDGE ( 'NONE', *, *, #213278, .F. ) ;
#141944 = CARTESIAN_POINT ( 'NONE',  ( 1.744777856283234785, -1.581906188472384400, 0.9981555316627908070 ) ) ;
#141945 = EDGE_CURVE ( 'NONE', #170139, #181670, #64475, .T. ) ;
#141946 = CARTESIAN_POINT ( 'NONE',  ( 5.928588038458690868, 1.899881307248694418, 0.5261610973047344819 ) ) ;
#141948 = CARTESIAN_POINT ( 'NONE',  ( 9.042925270190632858, 10.61279623905300085, 1.082531754730549967 ) ) ;
#141947 = CARTESIAN_POINT ( 'NONE',  ( 0.6823417656249899377, 4.676041667008086655, -1.181850606188754593 ) ) ;
#141950 = CARTESIAN_POINT ( 'NONE',  ( 1.049787907720298286, -1.741764784136769162, -1.355102641770723704 ) ) ;
#141949 = CARTESIAN_POINT ( 'NONE',  ( -5.063080299699540987, 7.994345218703034384, 1.199719254218464037 ) ) ;
#141951 = CARTESIAN_POINT ( 'NONE',  ( 2.993041990875914493, 6.420974562437304911, 0.3677586026352899218 ) ) ;
#141952 = CARTESIAN_POINT ( 'NONE',  ( 5.843727902690005749, 6.776436293681846301, -1.199719254218445830 ) ) ;
#141953 = CARTESIAN_POINT ( 'NONE',  ( -4.574986769607567894, 7.424902766929059261, 1.199719254218464037 ) ) ;
#141954 = CARTESIAN_POINT ( 'NONE',  ( 6.639320575229257670, 2.427506520031021520, 2.484945200759064665 ) ) ;
#141955 = CARTESIAN_POINT ( 'NONE',  ( 4.557473252141114983, 0.4328338235230348996, -1.923210603423119780 ) ) ;
#141956 = CARTESIAN_POINT ( 'NONE',  ( 5.145303760848274344, -1.981494167013456709, 1.182657305203537401 ) ) ;
#141957 = CARTESIAN_POINT ( 'NONE',  ( 5.494539847903294749, 1.833519193728103014, 0.3179774322314922741 ) ) ;
#141958 = CARTESIAN_POINT ( 'NONE',  ( 3.414939784243501641, -1.565044402038212379, 1.343584798420148774 ) ) ;
#141959 = CARTESIAN_POINT ( 'NONE',  ( 5.450014563013511726, 8.341805509282339770, -1.082531754730543083 ) ) ;
#141960 = CARTESIAN_POINT ( 'NONE',  ( 6.052789233858158369, 6.026285292448116948, 0.000000000000000000 ) ) ;
#141961 = CARTESIAN_POINT ( 'NONE',  ( 5.671053392266061977, 9.838255734277600695, 0.7998128361456331437 ) ) ;
#141962 = CARTESIAN_POINT ( 'NONE',  ( 1.364683531249988757, 1.446875000341421469, 0.000000000000000000 ) ) ;
#141963 = CARTESIAN_POINT ( 'NONE',  ( -4.304844010029503565, 14.48099179547451953, 11.21040724251216325 ) ) ;
#141964 = CARTESIAN_POINT ( 'NONE',  ( 5.083944415000174466, 7.914723669933440675, -1.082531754730549078 ) ) ;
#141965 = CARTESIAN_POINT ( 'NONE',  ( 4.861888260954045471, -0.5834894554452072502, 2.091229948656031734 ) ) ;
#141966 = CARTESIAN_POINT ( 'NONE',  ( 4.586165880992498778, 5.350526861157986147, -2.420000000000000373 ) ) ;
#141968 = CARTESIAN_POINT ( 'NONE',  ( 4.352959896991869471, 0.3989296284454147412, -1.797357466088687961 ) ) ;
#141967 = CARTESIAN_POINT ( 'NONE',  ( -4.799223189557577207, 4.701441264013013210, 0.7216878364870317197 ) ) ;
#141970 = CARTESIAN_POINT ( 'NONE',  ( 6.720655732516649827, 2.453385726714229609, 2.309856631140958960 ) ) ;
#141969 = CARTESIAN_POINT ( 'NONE',  ( -11.80251051724219202, 11.29999999999998117, 1.695257889419070851 ) ) ;
#141971 = CARTESIAN_POINT ( 'NONE',  ( 6.585463931165095985, -0.9389328202267492873, 1.978239266594773671 ) ) ;
#141972 = DIRECTION ( 'NONE',  ( 1.000000000000000000, -7.771561172376097755E-16, -4.440892098500627148E-16 ) ) ;
#141973 = CARTESIAN_POINT ( 'NONE',  ( 0.1755611466353265426, -0.002217706044388422469, -2.244164702216360219 ) ) ;
#141974 = CARTESIAN_POINT ( 'NONE',  ( -4.044288467547167976, 7.756266588949179308, -0.5710662792986564984 ) ) ;
#141975 = FILL_AREA_STYLE ('',( #41260 ) ) ;
#141976 = CARTESIAN_POINT ( 'NONE',  ( 6.580239226864286195, 6.782991656975736028, -0.2881480849740332140 ) ) ;
#141977 = CARTESIAN_POINT ( 'NONE',  ( -3.973948422136970748, 6.690004688251493192, -1.082531754730546636 ) ) ;
#141978 = CARTESIAN_POINT ( 'NONE',  ( -7.721398836998398352, -5.907420853759296264, -7.721398836998357496 ) ) ;
#141979 = CARTESIAN_POINT ( 'NONE',  ( 0.7601953647339227960, -1.285989511019115517, 1.216233164963770763 ) ) ;
#141980 = CARTESIAN_POINT ( 'NONE',  ( 5.496744759480266751, -1.964553546248495541, -0.4387526145827134183 ) ) ;
#141981 = CARTESIAN_POINT ( 'NONE',  ( 6.440286661691305703, 7.472421512516709718, 1.199719254218462483 ) ) ;
#141982 = CARTESIAN_POINT ( 'NONE',  ( 4.629967194361879201, -1.293677666091449296, -1.661686202823991820 ) ) ;
#141983 = CARTESIAN_POINT ( 'NONE',  ( 2.776846452629442297, 1.641606522343663555, -0.9870246354491112317 ) ) ;
#141984 = CARTESIAN_POINT ( 'NONE',  ( -0.02244404828160086532, 2.859736408857795009, -2.677210243787793598 ) ) ;
#141985 = CARTESIAN_POINT ( 'NONE',  ( 4.756286019550246102, -1.969087757444639042, -0.05037552155932183140 ) ) ;
#141986 = CARTESIAN_POINT ( 'NONE',  ( 5.713150811708690213, 1.648777711927760015, -1.166343465331370455 ) ) ;
#141987 = CARTESIAN_POINT ( 'NONE',  ( 2.219420098953532428, -1.815089452277141691, 0.4520615115926190919 ) ) ;
#141990 = EDGE_LOOP ( 'NONE', ( #68405, #131390, #69494, #176639 ) ) ;
#141989 = CARTESIAN_POINT ( 'NONE',  ( 0.7383556378116812313, 1.137082172773289379, -1.537495029474859276 ) ) ;
#141988 = CARTESIAN_POINT ( 'NONE',  ( 5.250533987919646428, 0.5060912822462645400, 1.648968847961843620 ) ) ;
#141992 = CARTESIAN_POINT ( 'NONE',  ( 3.199361063144961825, 6.676412307070352270, -0.7216878364870267237 ) ) ;
#141991 = CARTESIAN_POINT ( 'NONE',  ( 2.543839704335303153, -1.636039663378138886, -1.481301067789652537 ) ) ;
#141993 =( GEOMETRIC_REPRESENTATION_CONTEXT ( 3 ) GLOBAL_UNCERTAINTY_ASSIGNED_CONTEXT ( ( #117978 ) ) GLOBAL_UNIT_ASSIGNED_CONTEXT ( ( #194247, #42698, #110933 ) ) REPRESENTATION_CONTEXT ( 'NONE', 'WORKASPACE' ) );
#141994 = CARTESIAN_POINT ( 'NONE',  ( -1.364683531250000748, 1.821875000341421913, 0.000000000000000000 ) ) ;
#141995 = CARTESIAN_POINT ( 'NONE',  ( 6.355910407107248083, -0.6622273607519140182, 1.846833223631501264 ) ) ;
#141996 = CARTESIAN_POINT ( 'NONE',  ( 8.911787042884274257, 9.291506392986812912, 0.7998128361456462443 ) ) ;
#141997 = CARTESIAN_POINT ( 'NONE',  ( -7.987977580929896071, -5.530730635397370420, 7.987977580929924493 ) ) ;
#141998 = DIRECTION ( 'NONE',  ( 0.000000000000000000, 0.000000000000000000, 1.000000000000000000 ) ) ;
#141999 = CARTESIAN_POINT ( 'NONE',  ( -5.607584625718504689, 5.587669329723240708, -0.3781269150280338609 ) ) ;
#142000 = CARTESIAN_POINT ( 'NONE',  ( 1.961466609329724164, 1.720096886549182136, 1.151944459977225055 ) ) ;
#142001 = CARTESIAN_POINT ( 'NONE',  ( 0.7499999999999902300, 2.733333333333351600, 1.299038105676669330 ) ) ;
#142002 = CARTESIAN_POINT ( 'NONE',  ( 5.392392409933256303, 7.314210449720692786, 1.599625672291267398 ) ) ;
#142003 = CARTESIAN_POINT ( 'NONE',  ( -8.064402442030170093, 8.302891025323665630, 0.7998128361456602331 ) ) ;
#142004 = CARTESIAN_POINT ( 'NONE',  ( 3.932747076415766596, 6.745899468197171345, 1.199719254218451159 ) ) ;
#142005 = CARTESIAN_POINT ( 'NONE',  ( 6.235037545507011281, 1.978399733989940401, 0.7636319146847592165 ) ) ;
#142006 = DIRECTION ( 'NONE',  ( 0.9989735196462989908, 1.504112749676232550E-16, -0.04529798058948674572 ) ) ;
#142007 = CARTESIAN_POINT ( 'NONE',  ( 0.6823417656249882723, 2.176041667008084435, -1.181850606188749264 ) ) ;
#142009 = CARTESIAN_POINT ( 'NONE',  ( 4.518945272056516416, 4.166524327021037699, 0.7998128361456341429 ) ) ;
#142008 = CARTESIAN_POINT ( 'NONE',  ( -11.43209210103587914, 11.15596075983916080, -3.649125173352125273 ) ) ;
#142010 = CARTESIAN_POINT ( 'NONE',  ( 5.044295983762377311, 1.882185518538554314, -0.7230303062365079914 ) ) ;
#142011 = CARTESIAN_POINT ( 'NONE',  ( 5.173012249488437853, 1.686445640873093899, -0.9088423865804375890 ) ) ;
#142012 = CARTESIAN_POINT ( 'NONE',  ( 2.964592600559622593, -2.025863808726846127, -0.8364240203130177687 ) ) ;
#142013 = DIRECTION ( 'NONE',  ( 0.000000000000000000, 0.000000000000000000, -1.000000000000000000 ) ) ;
#142014 = CARTESIAN_POINT ( 'NONE',  ( 1.499999999999987121, 0.3270833340161527492, -0.8660254037844323793 ) ) ;
#142015 = CARTESIAN_POINT ( 'NONE',  ( 5.379157392057874354, -1.821786014368693252, -0.8570216514257876783 ) ) ;
#142016 = CARTESIAN_POINT ( 'NONE',  ( 1.529408426332915960, -0.2309274165002393187, 1.898302859121250519 ) ) ;
#142017 = CARTESIAN_POINT ( 'NONE',  ( -7.040761844198392794, 7.108643661186573759, -0.7998128361456291469 ) ) ;
#142019 = CARTESIAN_POINT ( 'NONE',  ( 0.1226730236999207246, 0.3474926252081366185, 1.986097365194151809 ) ) ;
#142018 = FACE_OUTER_BOUND ( 'NONE', #35417, .T. ) ;
#142020 = CARTESIAN_POINT ( 'NONE',  ( -1.364683531250000748, 9.671875000341396245, 0.000000000000000000 ) ) ;
#142022 = CARTESIAN_POINT ( 'NONE',  ( -4.620296487206990932, 8.612372678375294299, 0.000000000000000000 ) ) ;
#142021 = CARTESIAN_POINT ( 'NONE',  ( 3.790639713653580767, 1.765158817303988048, -1.120165474576743536 ) ) ;
#142024 = EDGE_LOOP ( 'NONE', ( #120772, #29716, #134697, #138816 ) ) ;
#142023 = CARTESIAN_POINT ( 'NONE',  ( 1.729112849636908367, -1.625594568690587050, 0.5768372424696955880 ) ) ;
#142025 =( NAMED_UNIT ( * ) SI_UNIT ( $, .STERADIAN. ) SOLID_ANGLE_UNIT ( ) );
#142026 = CARTESIAN_POINT ( 'NONE',  ( 5.717788096661236885, 7.693838750903348789, 1.599625672291267398 ) ) ;
#142027 = CARTESIAN_POINT ( 'NONE',  ( -0.8478968130440378559, 13.27085527049493230, 1.205503722529886135 ) ) ;
#142028 = DIRECTION ( 'NONE',  ( -3.330669073875479482E-16, 3.330669073875479482E-16, 1.000000000000000000 ) ) ;
#142029 = DIRECTION ( 'NONE',  ( 0.000000000000000000, 1.000000000000000000, 0.000000000000000000 ) ) ;
#142030 = CARTESIAN_POINT ( 'NONE',  ( 5.626797444871351139, 6.523350759560078593, 1.199719254218462483 ) ) ;
#142031 = EDGE_LOOP ( 'NONE', ( #88692, #65591, #131391, #54429 ) ) ;
#142032 = DIRECTION ( 'NONE',  ( 0.000000000000000000, 0.000000000000000000, 1.000000000000000000 ) ) ;
#142033 = CARTESIAN_POINT ( 'NONE',  ( 2.666445455534327102, 0.6121260541337695260, 1.705033028387469285 ) ) ;
#142034 = CARTESIAN_POINT ( 'NONE',  ( 4.403700966340357681, 4.032072637018845107, -0.7998128361456211532 ) ) ;
#142035 = CARTESIAN_POINT ( 'NONE',  ( 5.910428620914669473, 5.860197910680708944, 0.000000000000000000 ) ) ;
#142036 = CARTESIAN_POINT ( 'NONE',  ( 3.439928307436474597, -1.081519596823855345, -1.453003583242311381 ) ) ;
#142037 = CARTESIAN_POINT ( 'NONE',  ( 0.6499431002536731894, 3.350073969687604958, 0.06915891592279559130 ) ) ;
#142038 = CARTESIAN_POINT ( 'NONE',  ( -10.96075698767256767, -7.841077028191815401, 0.3746540212968124117 ) ) ;
#142039 = CARTESIAN_POINT ( 'NONE',  ( 5.378845419373885051, 6.306261619127770501, 1.070519943709395960 ) ) ;
#142040 = ADVANCED_FACE ( 'NONE', ( #22724, #37939 ), #153827, .F. ) ;
#142041 = CARTESIAN_POINT ( 'NONE',  ( 4.492532346964829060, 1.824898331334467549, 0.3640980636450250052 ) ) ;
#142042 = CARTESIAN_POINT ( 'NONE',  ( 1.845192132668025176, 0.3254238344292461060, -1.887580106770263999 ) ) ;
#142043 = CARTESIAN_POINT ( 'NONE',  ( 0.8326870614539466642, 0.1294382003846420159, 1.821050407652326619 ) ) ;
#142044 = DIRECTION ( 'NONE',  ( 0.3502638921866464417, -1.953969548649013438E-16, 0.9366510587354618389 ) ) ;
#142045 = CARTESIAN_POINT ( 'NONE',  ( -5.600926855776894975, 6.667407765562058053, -1.082531754730549967 ) ) ;
#142046 = CARTESIAN_POINT ( 'NONE',  ( 6.124909263556299166, 6.992440323537196356, 0.9511531368890328020 ) ) ;
#142047 = CARTESIAN_POINT ( 'NONE',  ( -11.41381675112453387, 10.19999999999998153, 3.704697986577180302 ) ) ;
#142048 = EDGE_CURVE ( 'NONE', #157004, #24729, #130478, .T. ) ;
#142049 = CARTESIAN_POINT ( 'NONE',  ( -3.765305043611756552, 7.354576300424668922, -0.6638232778202641793 ) ) ;
#142050 = FACE_OUTER_BOUND ( 'NONE', #40053, .T. ) ;
#142051 = CARTESIAN_POINT ( 'NONE',  ( 7.456621297836072415, 9.722477485607340597, 1.443375672974076540 ) ) ;
#142052 = CARTESIAN_POINT ( 'NONE',  ( 6.280130250669472503, -1.091077088088190372, -1.639371140202023014 ) ) ;
#142053 = CARTESIAN_POINT ( 'NONE',  ( -4.822949958159302497, 6.649860922651058992, -1.599625672291256295 ) ) ;
#142055 = CARTESIAN_POINT ( 'NONE',  ( -0.1099460098627005888, 6.494484681433106310, 3.110387376256865011 ) ) ;
#142054 = B_SPLINE_CURVE_WITH_KNOTS ( 'NONE', 3,
 ( #135949, #3763, #66631, #117624, #18968, #20036, #37366, #103441, #17894, #201964, #52553 ),
 .UNSPECIFIED., .F., .F.,
 ( 4, 1, 1, 1, 1, 1, 1, 1, 4 ),
 ( 0.000000000000000000, 0.2257091236145174484, 0.3979912149639216468, 0.5260416812932605657, 0.6190739408849097458, 0.6862087210430605211, 0.7361363507675404705, 0.7768852254246026989, 0.9999999999999998890 ),
 .UNSPECIFIED. ) ;
#142056 = CARTESIAN_POINT ( 'NONE',  ( 0.1465796939425691170, -1.677718324701961361, 1.247191284554289625 ) ) ;
#142057 = CARTESIAN_POINT ( 'NONE',  ( 7.690499447449630210, 9.995335326823163058, 1.599625672291281386 ) ) ;
#142058 = CARTESIAN_POINT ( 'NONE',  ( 5.104483318454627216, -0.6487533354903095573, -1.814000550502705922 ) ) ;
#142059 = CARTESIAN_POINT ( 'NONE',  ( -5.096975683733680818, 8.033889833409558534, -1.199719254218452047 ) ) ;
#142060 = CARTESIAN_POINT ( 'NONE',  ( 1.535882326342351334, 0.9031702520058831896, -1.586444745400449108 ) ) ;
#142061 = CARTESIAN_POINT ( 'NONE',  ( 2.578998426009218470, -2.112161100990978202, -0.6396139477699358533 ) ) ;
#142062 = CARTESIAN_POINT ( 'NONE',  ( 11.97929049433705728, 12.22000000000000064, 0.7046979865771804130 ) ) ;
#142063 = CARTESIAN_POINT ( 'NONE',  ( 0.7910927259777954523, -0.04954035392716604758, -1.911929172785244102 ) ) ;
#142064 = VERTEX_POINT ( 'NONE', #58456 ) ;
#142065 = CARTESIAN_POINT ( 'NONE',  ( 6.895365913452266682, -1.760736289220961481, 0.8823945077177670626 ) ) ;
#142066 = CARTESIAN_POINT ( 'NONE',  ( 2.120557540808472918, 0.002150750411172245441, 1.942234967187633110 ) ) ;
#142067 = ORIENTED_EDGE ( 'NONE', *, *, #111491, .T. ) ;
#142068 = CARTESIAN_POINT ( 'NONE',  ( 0.8782795706883707032, -0.2985837142155840507, 1.993765709762222782 ) ) ;
#142070 = CARTESIAN_POINT ( 'NONE',  ( 6.139480533765972581, 1.719935631569947221, -0.7110793932548589158 ) ) ;
#142069 = CARTESIAN_POINT ( 'NONE',  ( -4.281342646865346602, 8.216926531310035031, 0.7998128361456352531 ) ) ;
#142071 = CARTESIAN_POINT ( 'NONE',  ( 3.413620815590684199, 7.204584394822967752, 0.7998128361456281477 ) ) ;
#142072 = CARTESIAN_POINT ( 'NONE',  ( -11.48243876534946040, 13.79999999999999893, -3.200000000000001510 ) ) ;
#142073 = CARTESIAN_POINT ( 'NONE',  ( 8.940712233207955606, 12.51824914112961729, 1.199719254218450271 ) ) ;
#142074 = CARTESIAN_POINT ( 'NONE',  ( -4.660252114795309097, 6.460046772059735432, -1.599625672291256295 ) ) ;
#142075 = CARTESIAN_POINT ( 'NONE',  ( -6.635789839245807897, 6.706452665400368218, 0.7998128361456341429 ) ) ;
#142076 = CARTESIAN_POINT ( 'NONE',  ( 2.243918346939121733, 2.191141468336772036, 0.05030144379260945153 ) ) ;
#142077 = CARTESIAN_POINT ( 'NONE',  ( 5.043269954603547767, 4.986162489899998995, -0.7216878364870197293 ) ) ;
#142078 = CARTESIAN_POINT ( 'NONE',  ( 1.499999999999990896, 4.525000000000021672, 1.214306433183764966E-14 ) ) ;
#142079 = CARTESIAN_POINT ( 'NONE',  ( 6.966220764712143243, 6.002124920821316323, -2.500000000000000444 ) ) ;
#142080 = CARTESIAN_POINT ( 'NONE',  ( 2.719161800852238464, -0.1789327596440904167, 1.816892639718168390 ) ) ;
#142081 = CARTESIAN_POINT ( 'NONE',  ( 1.734723475976807094E-15, -3.469446951953614189E-15, 0.9487424039605132364 ) ) ;
#142082 = CARTESIAN_POINT ( 'NONE',  ( -3.415764635639130020, 6.072476943965863683, 1.199719254218462483 ) ) ;
#142083 = CARTESIAN_POINT ( 'NONE',  ( -4.712608863230891565, 8.343829661033030476, -0.7091526064728018719 ) ) ;
#142084 = DIRECTION ( 'NONE',  ( -0.000000000000000000, 1.000000000000000000, -0.000000000000000000 ) ) ;
#142085 = CARTESIAN_POINT ( 'NONE',  ( 7.564559641420864899, 10.91273778404466199, -1.199719254218446718 ) ) ;
#142087 = EDGE_CURVE ( 'NONE', #110148, #19108, #137373, .T. ) ;
#142086 = CARTESIAN_POINT ( 'NONE',  ( 0.5570954828270138215, -1.626785562868319435, -1.031698974670463009 ) ) ;
#142088 = CARTESIAN_POINT ( 'NONE',  ( 5.963715375765574755, -0.4800653121489819042, 1.901962685674676523 ) ) ;
#142089 = CARTESIAN_POINT ( 'NONE',  ( -1.402160292154681736E-14, 15.31250000000000000, 1.732050807568881190 ) ) ;
#142090 = CARTESIAN_POINT ( 'NONE',  ( -8.037286134802835491, 8.271255333558444889, -0.7998128361456291469 ) ) ;
#142091 = CARTESIAN_POINT ( 'NONE',  ( 4.904298879841284098, 6.744767997946721216, 1.599625672291267398 ) ) ;
#142092 = CARTESIAN_POINT ( 'NONE',  ( 5.232042516939362287, 2.159042084939459816, 0.3751777721049884273 ) ) ;
#142093 = AXIS2_PLACEMENT_3D ( 'NONE', #100784, #2189, #132265 ) ;
#142094 = DIRECTION ( 'NONE',  ( 0.3321398189114310173, 0.9432301631592798774, 3.697785493223492838E-32 ) ) ;
#142095 = EDGE_CURVE ( 'NONE', #164595, #213437, #87750, .T. ) ;
#142096 = CARTESIAN_POINT ( 'NONE',  ( 4.065334711822697678, 1.773058433220272789, 1.068561072119569522 ) ) ;
#142098 = CARTESIAN_POINT ( 'NONE',  ( -0.6823417656249969321, 3.280208333674754062, -1.181850606188749264 ) ) ;
#142097 = SURFACE_STYLE_FILL_AREA ( #109640 ) ;
#142099 = ORIENTED_EDGE ( 'NONE', *, *, #174390, .F. ) ;
#142100 = CARTESIAN_POINT ( 'NONE',  ( 4.623847096394516853, 0.3921523929481546267, 2.264879156731691712 ) ) ;
#142101 = CARTESIAN_POINT ( 'NONE',  ( 5.802526556968819804, 9.713438716531550554, -0.7216878364870267237 ) ) ;
#142103 = CARTESIAN_POINT ( 'NONE',  ( 1.499999999999972911, 4.577083334016149863, -0.8660254037844417052 ) ) ;
#142102 = CARTESIAN_POINT ( 'NONE',  ( 5.899206235721897507, 6.055031161196562373, 0.000000000000000000 ) ) ;
#142104 = CARTESIAN_POINT ( 'NONE',  ( 0.4106429779945898195, 1.576260533944493503, -1.664518642746879662 ) ) ;
#142105 = CARTESIAN_POINT ( 'NONE',  ( 6.620655732516647518, 0.5865983125455545011, 1.978983952526007339 ) ) ;
#142106 = CARTESIAN_POINT ( 'NONE',  ( -5.589704470584107909, 9.743348658981940247, -0.7998128361456362523 ) ) ;
#142107 = CARTESIAN_POINT ( 'NONE',  ( 5.296799794911354553, 1.588725326081788847, 1.116492485978479499 ) ) ;
#142108 = CARTESIAN_POINT ( 'NONE',  ( 10.04622863760192963, 10.82294762006482713, -0.7216878364870257245 ) ) ;
#142109 = ORIENTED_EDGE ( 'NONE', *, *, #158235, .T. ) ;
#142110 = CARTESIAN_POINT ( 'NONE',  ( 5.677967274442059953, 1.882970570262190835, -0.3333453579756898155 ) ) ;
#142111 = CARTESIAN_POINT ( 'NONE',  ( 6.071300242175304618, 0.1216566699881876934, -1.720563304769450630 ) ) ;
#142112 = CARTESIAN_POINT ( 'NONE',  ( 5.717982508692024624, 0.9896897593998502662, -1.756851901128737348 ) ) ;
#142114 = CARTESIAN_POINT ( 'NONE',  ( 0.000000000000000000, -5.166862915010145052, 0.000000000000000000 ) ) ;
#142113 = CARTESIAN_POINT ( 'NONE',  ( -7.967387826325084355, 12.44703623068796361, 0.7998128361456481317 ) ) ;
#142115 = CARTESIAN_POINT ( 'NONE',  ( -1.642778471874998480, -1.538541666188709245, 2.845375778867863303 ) ) ;
#142117 = CARTESIAN_POINT ( 'NONE',  ( 0.5316681593682397455, 0.9152217321290991858, -1.514687162473850490 ) ) ;
#142116 = CARTESIAN_POINT ( 'NONE',  ( 1.412182186510477777, 1.403042805649477920, -1.550086674462275216 ) ) ;
#142118 = CARTESIAN_POINT ( 'NONE',  ( 5.537732479266092689, -1.587839044716709669, 1.242724925242834066 ) ) ;
#142120 = CARTESIAN_POINT ( 'NONE',  ( 2.818655624875044285, 2.158736131429010996, 0.7712820022114060814 ) ) ;
#142119 = CARTESIAN_POINT ( 'NONE',  ( 5.910428620914669473, 5.860197910680708944, 0.000000000000000000 ) ) ;
#142121 = CARTESIAN_POINT ( 'NONE',  ( 1.763200577577472172, 0.8928190760214287369, 1.493706742695336764 ) ) ;
#142122 =( GEOMETRIC_REPRESENTATION_CONTEXT ( 3 ) GLOBAL_UNCERTAINTY_ASSIGNED_CONTEXT ( ( #174161 ) ) GLOBAL_UNIT_ASSIGNED_CONTEXT ( ( #185150, #207546, #69258 ) ) REPRESENTATION_CONTEXT ( 'NONE', 'WORKASPACE' ) );
#142123 = CARTESIAN_POINT ( 'NONE',  ( 11.89321938400742340, 11.26255278360675227, -1.599605898944273852 ) ) ;
#142124 = CARTESIAN_POINT ( 'NONE',  ( 2.002904151241869712, 1.714182390810105927, 0.2594085799107764823 ) ) ;
#142125 = CARTESIAN_POINT ( 'NONE',  ( -3.755786496842897795E-14, 2.609375000341406459, -1.570758158831778273 ) ) ;
#142126 = CARTESIAN_POINT ( 'NONE',  ( 1.521681963465530529, 1.834278628056866367, -0.3135228456460791846 ) ) ;
#142127 = CARTESIAN_POINT ( 'NONE',  ( 2.840461511066312728, -1.118188532415839598, 1.860977255340636516 ) ) ;
#142128 = CARTESIAN_POINT ( 'NONE',  ( 3.098842478760281516, 1.825076540557273974, 0.8578426345753201732 ) ) ;
#142129 = CARTESIAN_POINT ( 'NONE',  ( 3.500000000000003109, -2.127848526677250785E-13, -2.052068128417947612 ) ) ;
#142130 = CARTESIAN_POINT ( 'NONE',  ( 1.499999999999987121, 1.577083334016150751, -0.8660254037844253849 ) ) ;
#142131 = CARTESIAN_POINT ( 'NONE',  ( 6.709608095207008738, -0.4227469423600908605, 1.886647698053174116 ) ) ;
#142132 = CARTESIAN_POINT ( 'NONE',  ( -8.012344526598182026E-15, 14.79687500034140157, -1.575800808251669460 ) ) ;
#142133 = CARTESIAN_POINT ( 'NONE',  ( 3.393049125975013069, -2.141818966976690497, -0.5891788363768469816 ) ) ;
#142134 = ORIENTED_EDGE ( 'NONE', *, *, #78480, .F. ) ;
#142135 = CARTESIAN_POINT ( 'NONE',  ( -0.2108831679770924727, 4.091978752061476321, -2.452067053820900622 ) ) ;
#142136 = CARTESIAN_POINT ( 'NONE',  ( 1.499999999999987121, 0.004166666666691258049, 0.8660254037844524744 ) ) ;
#142137 = CARTESIAN_POINT ( 'NONE',  ( 7.751511138711133064, 10.06651563329490529, -1.599625672291262513 ) ) ;
#142138 = CARTESIAN_POINT ( 'NONE',  ( 0.6823417656249882723, -0.07395833299191079124, -1.181850606188749264 ) ) ;
#142139 = CARTESIAN_POINT ( 'NONE',  ( 6.293255338728928727, -0.1078348580665164369, -2.218937141123643375 ) ) ;
#142141 = CARTESIAN_POINT ( 'NONE',  ( 4.316819842036943911, -1.455217238560998272, 1.315978175897666080 ) ) ;
#142140 = COLOUR_RGB ( '', 0.09019608, 0.27058824, 0.51372549) ;
#142143 = CARTESIAN_POINT ( 'NONE',  ( -4.744990575102892905, 8.479646737687938085, 0.7216878364870458196 ) ) ;
#142142 = CARTESIAN_POINT ( 'NONE',  ( 4.033714395265605823, 4.664753868353354704, -1.199719254218446718 ) ) ;
#142144 = DIRECTION ( 'NONE',  ( 0.000000000000000000, 1.000000000000000000, 0.000000000000000000 ) ) ;
#142145 = CARTESIAN_POINT ( 'NONE',  ( 6.081380179524085605, 2.093784091706856199, -0.8575614380509981594 ) ) ;
#142146 = CARTESIAN_POINT ( 'NONE',  ( 2.172402883950707686, -0.9704110660942105726, -1.820128386451558500 ) ) ;
#142147 = CARTESIAN_POINT ( 'NONE',  ( -5.693534442735004752, 8.729875052244421951, 1.199719254218452047 ) ) ;
#142148 = ORIENTED_EDGE ( 'NONE', *, *, #168717, .F. ) ;
#142149 = CARTESIAN_POINT ( 'NONE',  ( -0.7500000000000215383, 2.972916667349487341, 1.299038105676671107 ) ) ;
#142150 = CARTESIAN_POINT ( 'NONE',  ( 3.620239363633662499, 1.188986022374241225, -1.444006105232335191 ) ) ;
#142151 = CARTESIAN_POINT ( 'NONE',  ( 2.355775467714062543, 0.08314403793566874090, -1.732266345623443948 ) ) ;
#142152 = CARTESIAN_POINT ( 'NONE',  ( 6.058177568126345669, -1.550975213528119623, 1.548612826651605712 ) ) ;
#142153 = CARTESIAN_POINT ( 'NONE',  ( 1.149787729276055437, -1.740433383357189223, -1.356609624190791008 ) ) ;
#142154 = CARTESIAN_POINT ( 'NONE',  ( 5.876890087061106271, 1.793433424740819904, -0.7452851482259108540 ) ) ;
#142155 = CARTESIAN_POINT ( 'NONE',  ( 8.022420187971052385, 15.29110919921158285, 8.925725321005275603 ) ) ;
#142156 = CARTESIAN_POINT ( 'NONE',  ( -0.03452862918938356951, -1.956592590566148093, -0.4871966601913205186 ) ) ;
#142157 = CARTESIAN_POINT ( 'NONE',  ( -0.08743476694611679312, -2.120266877281291595, -0.04547849331201780226 ) ) ;
#142158 = CARTESIAN_POINT ( 'NONE',  ( -15.75000000000000000, 9.799999999999998934, -1.800000000000001155 ) ) ;
#142159 = CARTESIAN_POINT ( 'NONE',  ( 6.434220164165640021, -1.621181005584397372, -1.198863592720422977 ) ) ;
#142160 = CARTESIAN_POINT ( 'NONE',  ( -8.910733272679575379, 11.41894145625809820, -1.599625672291263179 ) ) ;
#142161 = CARTESIAN_POINT ( 'NONE',  ( 7.253775878511261155, 8.421492265473332850, 1.199719254218462483 ) ) ;
#142162 = CARTESIAN_POINT ( 'NONE',  ( 5.063044020060520900, 4.871582543017558109, 0.7998128361456352531 ) ) ;
#142163 = CARTESIAN_POINT ( 'NONE',  ( 4.371595934376539816, 1.770262903079304451, -0.4459408992859363319 ) ) ;
#142164 = CARTESIAN_POINT ( 'NONE',  ( 2.397764582540245382, 1.705505620506567510, 1.400368488499253994 ) ) ;
#142165 = ORIENTED_EDGE ( 'NONE', *, *, #19530, .F. ) ;
#142166 = CARTESIAN_POINT ( 'NONE',  ( -4.055297343818976330, 5.824542549245813383, 1.443375672974065660 ) ) ;
#142167 = ADVANCED_FACE ( 'NONE', ( #72555 ), #157037, .F. ) ;
#142168 = CARTESIAN_POINT ( 'NONE',  ( 0.000000000000000000, -1.684374999522041172, -3.793834371823813001 ) ) ;
#142169 = CARTESIAN_POINT ( 'NONE',  ( -6.509886312855995172, 10.74661779830734254, -0.7998128361456291469 ) ) ;
#142170 = CARTESIAN_POINT ( 'NONE',  ( 1.301042304527067817, -0.3004618026806615272, -1.997203725593140078 ) ) ;
#142171 = CARTESIAN_POINT ( 'NONE',  ( -2.081668171172168513E-14, 5.868705557303649734, 4.125226524755077229 ) ) ;
#142172 = VERTEX_POINT ( 'NONE', #106191 ) ;
#142173 = CARTESIAN_POINT ( 'NONE',  ( -5.255720823952942489, 6.160704378480398979, -1.199719254218453823 ) ) ;
#142174 = CARTESIAN_POINT ( 'NONE',  ( 2.447915292705178825, -0.8007319036262178225, 1.680036726287994719 ) ) ;
#142175 = CARTESIAN_POINT ( 'NONE',  ( 4.715538499454675403, 4.395883092318884522, 1.214306433183764966E-14 ) ) ;
#142176 = FACE_OUTER_BOUND ( 'NONE', #128112, .T. ) ;
#142177 = ORIENTED_EDGE ( 'NONE', *, *, #183780, .F. ) ;
#142178 = PRODUCT_DEFINITION_FORMATION_WITH_SPECIFIED_SOURCE ( 'ANY', '', #31690, .NOT_KNOWN. ) ;
#142179 = CARTESIAN_POINT ( 'NONE',  ( -9.155833807930273238, 9.576227618873799585, -0.7998128361456291469 ) ) ;
#142180 = CARTESIAN_POINT ( 'NONE',  ( 3.932112477472641920, 0.9751300899686901058, -1.543267412809447681 ) ) ;
#142181 = VECTOR ( 'NONE', #107321, 1000.000000000000000 ) ;
#142183 = CARTESIAN_POINT ( 'NONE',  ( -5.030466903028923298, 6.770262730772157234, -1.447917484242104758 ) ) ;
#142182 = CARTESIAN_POINT ( 'NONE',  ( -4.817943484809863008, 6.714296380401858499, 1.599625672291263179 ) ) ;
#142184 = CARTESIAN_POINT ( 'NONE',  ( 6.395636025722083673, 6.905704815116233242, -0.7835738547974178125 ) ) ;
#142185 = CARTESIAN_POINT ( 'NONE',  ( 6.327499943094792023, -1.427716970705223520, 1.423745300580002482 ) ) ;
#142186 = CARTESIAN_POINT ( 'NONE',  ( 5.736236344406846932, 0.3633543575551900773, 1.804753862313414281 ) ) ;
#142187 = AXIS2_PLACEMENT_3D ( 'NONE', #7908, #141176, #159511 ) ;
#142188 = CARTESIAN_POINT ( 'NONE',  ( 4.653107873243750525, -1.855428480829583338, 1.371977642438865885 ) ) ;
#142189 = CARTESIAN_POINT ( 'NONE',  ( 4.716257332707354699, 6.595662536282280719, -1.599625672291269396 ) ) ;
#142190 = CARTESIAN_POINT ( 'NONE',  ( 6.837200347746461127, -1.934230338078479772, 0.9651617863762137484 ) ) ;
#142191 = CARTESIAN_POINT ( 'NONE',  ( 7.630541526392844887, 7.796719957080126662, 0.7998128361456341429 ) ) ;
#142192 = CARTESIAN_POINT ( 'NONE',  ( 1.979929434068830929, -1.904991468646766606, -0.3768183752349169580 ) ) ;
#142193 = EDGE_CURVE ( 'NONE', #51705, #36647, #26427, .T. ) ;
#142194 = CARTESIAN_POINT ( 'NONE',  ( 5.290469632519504195, -2.184888740097378879, 0.7135917202819259675 ) ) ;
#142195 = CARTESIAN_POINT ( 'NONE',  ( 9.348761378620915607, 13.52553930298125096, -7.449808453853658641 ) ) ;
#142196 = CARTESIAN_POINT ( 'NONE',  ( -5.738844160334429567, 9.917344963690652548, 0.000000000000000000 ) ) ;
#142197 = CARTESIAN_POINT ( 'NONE',  ( 4.873830839387755631, 1.077430855447782942, 1.529020332772989210 ) ) ;
#142198 = ORIENTED_EDGE ( 'NONE', *, *, #90702, .T. ) ;
#142200 = CARTESIAN_POINT ( 'NONE',  ( -3.800028193580205382, 7.655393002477360653, -0.7998128361456481317 ) ) ;
#142199 = CARTESIAN_POINT ( 'NONE',  ( 2.584119536544440265, 1.026460374567798484, 1.613398670029235538 ) ) ;
#142201 = CARTESIAN_POINT ( 'NONE',  ( 4.459734715955371520, 0.4851516707722826061, -2.152740496749529608 ) ) ;
#142202 = CARTESIAN_POINT ( 'NONE',  ( 0.6124999999999707345, 0.7291666673494984208, -1.060881119635972647 ) ) ;
#142203 = CARTESIAN_POINT ( 'NONE',  ( 6.883263157960402445, -0.003972766660574957552, 2.046037087719229319 ) ) ;
#142204 = CARTESIAN_POINT ( 'NONE',  ( 6.007671464186834065, 7.141943142040370063, 1.082531754730549967 ) ) ;
#142205 = CARTESIAN_POINT ( 'NONE',  ( -6.333067150914850174, 8.481940657524365434, 1.443375672974064550 ) ) ;
#142206 = CARTESIAN_POINT ( 'NONE',  ( 1.124223373062693820, 1.177560201100100734, -1.580856549663816280 ) ) ;
#142207 = ADVANCED_FACE ( 'NONE', ( #40079 ), #115275, .T. ) ;
#142208 = CARTESIAN_POINT ( 'NONE',  ( 2.714277975868684578, -2.282582259777651501, 0.3379699517906120110 ) ) ;
#142209 = CARTESIAN_POINT ( 'NONE',  ( 1.978885927095444863, 1.829411362569667743, 0.7090815385668995940 ) ) ;
#142210 = DIRECTION ( 'NONE',  ( 1.000000000000000000, 0.000000000000000000, 0.000000000000000000 ) ) ;
#142211 = CARTESIAN_POINT ( 'NONE',  ( 6.262562444065095768, -0.7369429887811511648, -1.926613908347002413 ) ) ;
#142212 = CARTESIAN_POINT ( 'NONE',  ( 4.541618270897912701, 4.400902192243413502, 1.214306433183764966E-14 ) ) ;
#142213 = CARTESIAN_POINT ( 'NONE',  ( 4.135954056172497673, 2.015980767636461835, -0.05432360925018697717 ) ) ;
#142214 = CARTESIAN_POINT ( 'NONE',  ( 3.984117037569365305, 5.741498858621315371, 1.599625672291261402 ) ) ;
#142215 = ORIENTED_EDGE ( 'NONE', *, *, #207501, .T. ) ;
#142216 = CARTESIAN_POINT ( 'NONE',  ( 4.839077477813122918, -1.706110771555340744, -1.074664961451990308 ) ) ;
#142217 = CARTESIAN_POINT ( 'NONE',  ( -9.622536337397040285, 12.24937836509514710, 1.599625672291281386 ) ) ;
#142218 =( BOUNDED_CURVE ( )  B_SPLINE_CURVE ( 2, ( #124005, #108801, #128282, #192091, #27474, #93572, #159617, #156425, #11214 ),
 .UNSPECIFIED., .F., .T. ) 
 B_SPLINE_CURVE_WITH_KNOTS ( ( 3, 2, 2, 2, 3 ),
 ( 0.2656250000000002220, 0.2708333333333333148, 0.2812500000000000000, 0.2916666666666666852, 0.2968749999999998335 ),
 .UNSPECIFIED. ) 
 CURVE ( )  GEOMETRIC_REPRESENTATION_ITEM ( )  RATIONAL_B_SPLINE_CURVE ( ( 0.9330127018922194093, 0.9330127018922221849, 1.000000000000000000, 0.8660254037844387076, 1.000000000000000000, 0.8660254037844387076, 1.000000000000000000, 0.9330127018922215187, 0.9330127018922194093 ) ) 
 REPRESENTATION_ITEM ( '' )  );
#142219 = DIRECTION ( 'NONE',  ( -0.000000000000000000, 0.000000000000000000, -1.000000000000000000 ) ) ;
#142220 = CARTESIAN_POINT ( 'NONE',  ( -0.2409995289980038091, -0.004801160710915519658, -2.000252362011435636 ) ) ;
#142221 = CARTESIAN_POINT ( 'NONE',  ( 8.940712233207955606, 12.51824914112961729, 1.199719254218450271 ) ) ;
#142222 = CARTESIAN_POINT ( 'NONE',  ( 2.360437767749205218, -2.170642449777848260, 0.04973808404824981572 ) ) ;
#142223 = CARTESIAN_POINT ( 'NONE',  ( -0.4019237886466871523, 12.19866454968463110, -1.499999999999998668 ) ) ;
#142224 = CARTESIAN_POINT ( 'NONE',  ( -11.86145016429273191, 10.09412123665269334, -1.100000000000000089 ) ) ;
#142225 = CARTESIAN_POINT ( 'NONE',  ( 2.389737607000471442, -0.8038258883538219601, 1.689183408448757362 ) ) ;
#142226 = CARTESIAN_POINT ( 'NONE',  ( 6.696550776676711614, -0.5693818166121329405, -2.085215994158528208 ) ) ;
#142228 = FILL_AREA_STYLE ('',( #210378 ) ) ;
#142227 = DIRECTION ( 'NONE',  ( 0.000000000000000000, -1.000000000000000000, 0.000000000000000000 ) ) ;
#142229 = CARTESIAN_POINT ( 'NONE',  ( -1.364683531250012516, 1.030208333674754062, 0.7879004041258379498 ) ) ;
#142230 = CARTESIAN_POINT ( 'NONE',  ( 0.000000000000000000, 3.079999999999999183, 0.000000000000000000 ) ) ;
#142231 =( BOUNDED_CURVE ( )  B_SPLINE_CURVE ( 2, ( #131136, #98573, #49815, #16219, #214397, #66026, #115941, #90866, #70300 ),
 .UNSPECIFIED., .F., .T. ) 
 B_SPLINE_CURVE_WITH_KNOTS ( ( 3, 2, 2, 2, 3 ),
 ( 0.4553571428571427937, 0.4583333333333333148, 0.4642857142857143016, 0.4702380952380952328, 0.4732142857142856984 ),
 .UNSPECIFIED. ) 
 CURVE ( )  GEOMETRIC_REPRESENTATION_ITEM ( )  RATIONAL_B_SPLINE_CURVE ( ( 0.9330127018922194093, 0.9330127018922180770, 1.000000000000000000, 0.8660254037844387076, 1.000000000000000000, 0.8660254037844387076, 1.000000000000000000, 0.9330127018922194093, 0.9330127018922194093 ) ) 
 REPRESENTATION_ITEM ( '' )  );
#142232 = CARTESIAN_POINT ( 'NONE',  ( 3.773993364719562482, 1.897484654492180178, -0.2369724479281897223 ) ) ;
#142233 = CARTESIAN_POINT ( 'NONE',  ( 4.153014383403249354, -1.471681513620528348, -0.9827620175600642050 ) ) ;
#142234 = CARTESIAN_POINT ( 'NONE',  ( 1.365713085969634477, 0.5541664655046051324, -1.830235057661818487 ) ) ;
#142235 = CARTESIAN_POINT ( 'NONE',  ( -5.091250377131585125, 5.898545847196970726, 1.199719254218450271 ) ) ;
#142237 = CARTESIAN_POINT ( 'NONE',  ( -0.2060670157024322158, -0.8220983527124374746, -1.729069022899624164 ) ) ;
#142236 = PRESENTATION_STYLE_ASSIGNMENT (( #94545 ) ) ;
#142238 = CARTESIAN_POINT ( 'NONE',  ( -0.7500000000000006661, -0.3916666666666443475, -1.299038105676652011 ) ) ;
#142239 = CARTESIAN_POINT ( 'NONE',  ( 1.223191768902037957, -1.870915810643185795, -0.8869332102946840823 ) ) ;
#142240 = CARTESIAN_POINT ( 'NONE',  ( 1.364683531249988757, -0.8031249996585804185, 0.000000000000000000 ) ) ;
#142241 = CARTESIAN_POINT ( 'NONE',  ( 5.946149726614579301, 1.868617323842229894, 0.09011704611043556967 ) ) ;
#142242 = CARTESIAN_POINT ( 'NONE',  ( 1.295219883412350503, 1.381147610352757127, 1.194082977437810333 ) ) ;
#142244 = CARTESIAN_POINT ( 'NONE',  ( 4.599920620972065777, 8.367456947080912144, 0.1478172174028801744 ) ) ;
#142243 = CARTESIAN_POINT ( 'NONE',  ( 5.602238545945851023, -2.207063162045197924, -0.003355105161521875021 ) ) ;
#142245 = CARTESIAN_POINT ( 'NONE',  ( 1.364683531249988535, 5.717708333674752730, -0.7879004041258300672 ) ) ;
#142246 = CARTESIAN_POINT ( 'NONE',  ( 2.963389562657412046, 1.741120879107743935, 1.105697716663532892 ) ) ;
#142247 = CARTESIAN_POINT ( 'NONE',  ( -7.874588291438845644, 8.081441182967111558, -0.7998128361456291469 ) ) ;
#142248 = CARTESIAN_POINT ( 'NONE',  ( 7.781490099239519509, 11.16582331816642260, 1.199719254218460707 ) ) ;
#142249 = DIRECTION ( 'NONE',  ( -0.000000000000000000, -1.000000000000000000, -0.000000000000000000 ) ) ;
#142250 = AXIS2_PLACEMENT_3D ( 'NONE', #212499, #28435, #64140 ) ;
#142251 = CARTESIAN_POINT ( 'NONE',  ( -0.02890330888918044711, -9.971207602185762298, -10.91966316483285304 ) ) ;
#142252 = CARTESIAN_POINT ( 'NONE',  ( 7.530627977747744062, 7.750430493652658015, -0.7998128361456341429 ) ) ;
#142253 = VERTEX_POINT ( 'NONE', #208877 ) ;
#142254 = CARTESIAN_POINT ( 'NONE',  ( 4.879381568908511824, -0.1049739508458477355, 2.067839077007492143 ) ) ;
#142255 = CARTESIAN_POINT ( 'NONE',  ( -1.364683531250014514, 0.5510416670080878765, -0.7879004041258289570 ) ) ;
#142256 = CARTESIAN_POINT ( 'NONE',  ( 2.407699484934812784, -0.4761397456576694776, 2.108333575599189214 ) ) ;
#142257 = CARTESIAN_POINT ( 'NONE',  ( -4.604461168338175980, 8.383524640989071131, 0.06638267717353450725 ) ) ;
#142258 = CARTESIAN_POINT ( 'NONE',  ( 3.246744516521868018, 1.970913372098213712, 0.4403762775553735631 ) ) ;
#142259 = CARTESIAN_POINT ( 'NONE',  ( 6.620655732516618208, 1.260995252412312251, 2.189931766300906801 ) ) ;
#142260 = PRODUCT_DEFINITION_SHAPE ( 'NONE', 'NONE',  #52109 ) ;
#142261 = ORIENTED_EDGE ( 'NONE', *, *, #112034, .T. ) ;
#142263 = CARTESIAN_POINT ( 'NONE',  ( 6.860062538834778678, 8.066123052471139587, -1.082531754730543083 ) ) ;
#142262 = CARTESIAN_POINT ( 'NONE',  ( 3.475000000000000533, -1.545833333333334503, -2.006292185433951047 ) ) ;
#142264 = CARTESIAN_POINT ( 'NONE',  ( -5.908321080505254841, 10.11506803722328129, 0.7998128361456291469 ) ) ;
#142265 = CARTESIAN_POINT ( 'NONE',  ( 1.217982839071569012, 0.9896824804975331569, -1.756856037137774162 ) ) ;
#142267 = CARTESIAN_POINT ( 'NONE',  ( 5.952700804540856261, -1.878875186057769264, -1.127905468421293689 ) ) ;
#142266 = CARTESIAN_POINT ( 'NONE',  ( -5.752737250900127997, 5.605948302338584099, 0.000000000000000000 ) ) ;
#142268 = CARTESIAN_POINT ( 'NONE',  ( -3.716631501448782515, 7.355961102242025262, 0.5892660917431468137 ) ) ;
#142269 = CARTESIAN_POINT ( 'NONE',  ( 4.623256175466384121, 1.666654777633369555, 0.9376445158523970536 ) ) ;
#142270 = CARTESIAN_POINT ( 'NONE',  ( -4.451154503988200339, 4.087435097607984957, 1.214306433183764966E-14 ) ) ;
#142271 = CARTESIAN_POINT ( 'NONE',  ( 5.707619481228810798, 7.681975366232176583, -1.443375672974057666 ) ) ;
#142273 = CARTESIAN_POINT ( 'NONE',  ( 3.655875201264874974, 1.122517324909186653, 1.674876314423722423 ) ) ;
#142272 = CARTESIAN_POINT ( 'NONE',  ( -8.310784975052669665, 12.63974020429606249, -0.7216878364870267237 ) ) ;
#142274 = CARTESIAN_POINT ( 'NONE',  ( -8.012344526598182026E-15, 13.60937500034139447, -1.575800808251669460 ) ) ;
#142275 = CARTESIAN_POINT ( 'NONE',  ( 5.666962058884261744, -1.561145826413099291, -0.7335915956277230254 ) ) ;
#142276 = CARTESIAN_POINT ( 'NONE',  ( 7.388267364804250725, 7.584343111885245570, -0.7998128361456341429 ) ) ;
#142277 = CARTESIAN_POINT ( 'NONE',  ( 8.920901888111986366, 12.39117405523060889, 1.082531754730546636 ) ) ;
#142278 = COLOUR_RGB ( '', 0.66274510, 0.83137255, 0.94901961) ;
#142279 = CARTESIAN_POINT ( 'NONE',  ( -11.44786932348563901, 11.29999999999999893, -3.303370173849772051 ) ) ;
#142280 = CARTESIAN_POINT ( 'NONE',  ( 4.182764291190976813, -0.1809548918480126112, -1.861743760598027597 ) ) ;
#142281 = CARTESIAN_POINT ( 'NONE',  ( 1.500000000000053291, 7.750000000000000000, 15.74999999999999289 ) ) ;
#142283 =( BOUNDED_CURVE ( )  B_SPLINE_CURVE ( 2, ( #60314, #193524, #192438, #110213, #12624 ),
 .UNSPECIFIED., .F., .T. ) 
 B_SPLINE_CURVE_WITH_KNOTS ( ( 3, 2, 3 ),
 ( 0.1347995350948868465, 0.1375000000000000111, 0.1409922313975706942 ),
 .UNSPECIFIED. ) 
 CURVE ( )  GEOMETRIC_REPRESENTATION_ITEM ( )  RATIONAL_B_SPLINE_CURVE ( ( 0.9388907138593196589, 0.9131695131383610331, 1.000000000000000000, 0.8877111300685985862, 0.9636488443798396641 ) ) 
 REPRESENTATION_ITEM ( '' )  );
#142282 = CARTESIAN_POINT ( 'NONE',  ( 1.077107760077404830, 1.911388382048292645, 0.7958064784282169457 ) ) ;
#142284 = CARTESIAN_POINT ( 'NONE',  ( 0.3387883092347047653, -5.166862915010296042, 10.99523224158955870 ) ) ;
#142285 = ORIENTED_EDGE ( 'NONE', *, *, #46711, .F. ) ;
#142286 = CARTESIAN_POINT ( 'NONE',  ( 6.393201686769759640, -0.09647555762395694512, -1.809044896826275783 ) ) ;
#142287 = CARTESIAN_POINT ( 'NONE',  ( 5.252858170651868441, 5.093032385374103299, -0.7998128361456481317 ) ) ;
#142288 = CARTESIAN_POINT ( 'NONE',  ( -0.03552856956758054796, -1.956598898622825766, -0.4871759670460884539 ) ) ;
#142289 = CARTESIAN_POINT ( 'NONE',  ( -0.07045567476893913050, -1.776642250867260575, 0.3530574836328649324 ) ) ;
#142290 = ADVANCED_FACE ( 'NONE', ( #205687 ), #209790, .T. ) ;
#142291 = CARTESIAN_POINT ( 'NONE',  ( 4.868786560638885597, 7.733982516503781213, 1.082531754730548412 ) ) ;
#142292 = CARTESIAN_POINT ( 'NONE',  ( 10.72462670916096172, 9.912391986280232103, -5.392981251122232145 ) ) ;
#142293 = ORIENTED_EDGE ( 'NONE', *, *, #44659, .T. ) ;
#142294 = CARTESIAN_POINT ( 'NONE',  ( 9.368320956918616105, 10.03205532593431037, 0.7216878364870458196 ) ) ;
#142295 = ADVANCED_FACE ( 'NONE', ( #59448 ), #152535, .T. ) ;
#142297 = CARTESIAN_POINT ( 'NONE',  ( 8.437251666405968464, 8.737881787095446384, 1.040834085586084257E-14 ) ) ;
#142296 = CARTESIAN_POINT ( 'NONE',  ( 0.2386218892466463737, -1.902018210125755004, -0.4804332253167050149 ) ) ;
#142298 = CARTESIAN_POINT ( 'NONE',  ( 4.552287420941045326, -1.248256511182913364, 1.453175340101879875 ) ) ;
#142299 = CARTESIAN_POINT ( 'NONE',  ( -11.41126283316785361, 13.75874606908456954, 3.405403429622881006 ) ) ;
#142300 = CARTESIAN_POINT ( 'NONE',  ( -5.584154938098890852, 7.410262610144577877, 1.243513269814926492 ) ) ;
#142301 = SURFACE_SIDE_STYLE ('',( #76192 ) ) ;
#142303 = ORIENTED_EDGE ( 'NONE', *, *, #157010, .T. ) ;
#142302 = CARTESIAN_POINT ( 'NONE',  ( 5.694061328059515148, 5.745419092265303007, -0.7216878364870207285 ) ) ;
#142304 = CARTESIAN_POINT ( 'NONE',  ( -9.002250809794006159, 10.56534270192358704, -1.082531754730543971 ) ) ;
#142305 = CARTESIAN_POINT ( 'NONE',  ( 1.516726440323381331, 1.451591637995581996, -1.601975981646540426 ) ) ;
#142306 = CARTESIAN_POINT ( 'NONE',  ( -3.688700311369816909, 6.461178242310183784, -1.199719254218450271 ) ) ;
#142307 = ADVANCED_FACE ( 'NONE', ( #97854 ), #133570, .T. ) ;
#142308 = CARTESIAN_POINT ( 'NONE',  ( 6.021229618244865023, 10.03886863134542828, -0.7216878364870458196 ) ) ;
#142309 = CARTESIAN_POINT ( 'NONE',  ( -2.656508033273816238, 5.186677574539687363, -1.199719254218446718 ) ) ;
#142310 = CARTESIAN_POINT ( 'NONE',  ( 4.313378725478684395, -0.3118687524542098632, 1.798583714455632476 ) ) ;
#142311 = CARTESIAN_POINT ( 'NONE',  ( 10.23763000547997493, 9.286261708574206963, 5.789277571301806979 ) ) ;
#142312 = CARTESIAN_POINT ( 'NONE',  ( 1.370321444179344983, -1.253680685346630019, 1.521333489566406127 ) ) ;
#142313 = CARTESIAN_POINT ( 'NONE',  ( 3.427896188528327226, -1.883279545317056547, 0.3315703044584616399 ) ) ;
#142314 = ORIENTED_EDGE ( 'NONE', *, *, #74394, .F. ) ;
#142315 = CARTESIAN_POINT ( 'NONE',  ( 0.3645075752534430724, 4.000000000000008882, 0.9782388703846671696 ) ) ;
#142316 = CARTESIAN_POINT ( 'NONE',  ( 3.402753045726066183, 0.4761229057644749130, 1.911014528907057697 ) ) ;
#142317 = EDGE_LOOP ( 'NONE', ( #43890, #117276, #202539, #24660 ) ) ;
#142318 = CARTESIAN_POINT ( 'NONE',  ( 5.601106521291020712, -0.4677194688633263264, 1.884795189151499795 ) ) ;
#142319 = ORIENTED_EDGE ( 'NONE', *, *, #137537, .F. ) ;
#142320 = CARTESIAN_POINT ( 'NONE',  ( -5.074494633264801990, 9.142270515442742607, 0.7998128361456291469 ) ) ;
#142322 = CARTESIAN_POINT ( 'NONE',  ( 6.901817412891589676, -6.554751173179806045, -6.500815856195342413 ) ) ;
#142321 = CARTESIAN_POINT ( 'NONE',  ( -3.962726036944197894, 7.845207153068690431, -0.7998128361456481317 ) ) ;
#142323 = CARTESIAN_POINT ( 'NONE',  ( 7.634649897826745857, 8.079715433652276957, 0.7216878364870267237 ) ) ;
#142324 = CARTESIAN_POINT ( 'NONE',  ( 4.020093958671668410, -1.906945023982812515, 0.1437811316862200317 ) ) ;
#142325 = CARTESIAN_POINT ( 'NONE',  ( 6.983263157960370116, 1.266851337794393961, 2.060309365732877485 ) ) ;
#142326 = CARTESIAN_POINT ( 'NONE',  ( -2.788906526875773208E-15, 12.68749999999999822, -1.499999999999998446 ) ) ;
#142327 = CARTESIAN_POINT ( 'NONE',  ( 7.499070966595098753, -5.223177556212323935, 8.016215341155817242 ) ) ;
#142328 = CARTESIAN_POINT ( 'NONE',  ( 5.233069312805943341, 1.860886824452904653, 0.7683393057746935595 ) ) ;
#142329 = FACE_OUTER_BOUND ( 'NONE', #131923, .T. ) ;
#142330 = CARTESIAN_POINT ( 'NONE',  ( 5.707590141996651489, -0.4392596013848491521, 1.771934311310577659 ) ) ;
#142331 = CARTESIAN_POINT ( 'NONE',  ( 6.727182134110205602, 7.053355583909074689, 2.409100679957976165 ) ) ;
#142332 = CARTESIAN_POINT ( 'NONE',  ( 2.400909748719297188, 0.4512941399696759337, 2.020426262116347349 ) ) ;
#142333 = CARTESIAN_POINT ( 'NONE',  ( -6.738566041191992539, 7.820414121934134322, 1.199719254218450271 ) ) ;
#142334 = STYLED_ITEM ( 'NONE', ( #196189 ), #60737 ) ;
#142335 = CARTESIAN_POINT ( 'NONE',  ( -5.043389779576542331, 7.890798448915884222, -1.099773784605091009 ) ) ;
#142336 = DIRECTION ( 'NONE',  ( 1.276756478318932585E-15, -1.000000000000000000, 1.665334536937738262E-16 ) ) ;
#142337 = CARTESIAN_POINT ( 'NONE',  ( 1.642778471875001811, -3.142708332855375986, 2.845375778867859751 ) ) ;
#142338 = CARTESIAN_POINT ( 'NONE',  ( 7.135668919494039031, 7.219368582364847242, 1.040834085586084257E-14 ) ) ;
#142339 = VECTOR ( 'NONE', #198702, 1000.000000000000114 ) ;
#142340 = CARTESIAN_POINT ( 'NONE',  ( -5.135841261478327979, 4.886236314679810455, 0.7998128361456341429 ) ) ;
#142341 = CARTESIAN_POINT ( 'NONE',  ( 5.722950238744211937, 5.849399164722627553, 0.7216878364870328300 ) ) ;
#142342 = CARTESIAN_POINT ( 'NONE',  ( 0.2331713839410576306, 0.005725554726919174046, -1.953566683266183102 ) ) ;
#142343 = CARTESIAN_POINT ( 'NONE',  ( 1.364683531249996529, 11.77604166700806410, 0.7879004041258405033 ) ) ;
#142344 = CARTESIAN_POINT ( 'NONE',  ( -3.764360206088648297, 7.543504007078730922, -0.7998128361456281477 ) ) ;
#142346 = CARTESIAN_POINT ( 'NONE',  ( -7.618755976236585958, 7.853246491889623648, 0.000000000000000000 ) ) ;
#142345 = DIRECTION ( 'NONE',  ( -1.000000000000000000, 7.387867266669436732E-31, 0.000000000000000000 ) ) ;
#142347 = CARTESIAN_POINT ( 'NONE',  ( 4.781731028689206298, 1.437863813525115830, -0.9690746147167289548 ) ) ;
#142348 = CARTESIAN_POINT ( 'NONE',  ( -3.903858165731105778, 6.641919395739846799, 1.199719254218464037 ) ) ;
#142349 = CARTESIAN_POINT ( 'NONE',  ( 2.852461952307944415, -2.064405766265942521, -0.1567919417525542591 ) ) ;
#142350 = CARTESIAN_POINT ( 'NONE',  ( 3.919616530476960126, -1.461442364795034976, -1.532149496301576486 ) ) ;
#142351 = CARTESIAN_POINT ( 'NONE',  ( 6.889514614038635187, 11.18951748302043114, -0.7998128361456291469 ) ) ;
#142352 = EDGE_CURVE ( 'NONE', #37959, #66325, #31246, .T. ) ;
#142353 = CARTESIAN_POINT ( 'NONE',  ( 1.393335261261628988, -1.782783755681414117, 0.8371470673369950655 ) ) ;
#142354 = CARTESIAN_POINT ( 'NONE',  ( 6.017762162252820346, 6.076696597586958681, 0.5614182107811436229 ) ) ;
#142355 = CARTESIAN_POINT ( 'NONE',  ( 4.880572111239557920, 4.796348339308675435, -0.7216878364870197293 ) ) ;
#142357 = FACE_OUTER_BOUND ( 'NONE', #170186, .T. ) ;
#142356 = CARTESIAN_POINT ( 'NONE',  ( -3.475000000000000533, -1.750000000000001554, 0.000000000000000000 ) ) ;
#142358 = CARTESIAN_POINT ( 'NONE',  ( 4.084120828622629595, -2.267077656855093881, -0.3380819097023191055 ) ) ;
#142359 = CARTESIAN_POINT ( 'NONE',  ( 0.3108172448005979138, 1.586703044182024458, 0.9029097728878652251 ) ) ;
#142360 = EDGE_CURVE ( 'NONE', #158767, #23152, #178560, .T. ) ;
#142361 = CARTESIAN_POINT ( 'NONE',  ( 6.717138760927786834, 6.801359740696030443, -0.7998128361456481317 ) ) ;
#142362 = CARTESIAN_POINT ( 'NONE',  ( 6.060131475184119765, 9.053608573481392696, -1.082531754730537976 ) ) ;
#142363 = CARTESIAN_POINT ( 'NONE',  ( -7.648771216403934758, 12.07531685244661723, -0.7998128361456291469 ) ) ;
#142364 = CARTESIAN_POINT ( 'NONE',  ( 1.195565668251681535, 1.858513546554524609, -0.7743570246632487386 ) ) ;
#142365 = CARTESIAN_POINT ( 'NONE',  ( 2.571086506140254357, 1.750134206675527437, 0.8865088104979682582 ) ) ;
#142366 = CARTESIAN_POINT ( 'NONE',  ( -9.182950115157607840, 9.607863310639020327, 0.7998128361456462443 ) ) ;
#142367 = CARTESIAN_POINT ( 'NONE',  ( -6.847031270101295419, 7.946956888995021728, -1.199719254218446718 ) ) ;
#142368 = CARTESIAN_POINT ( 'NONE',  ( 4.318600669050608687, 4.999583595936801572, -2.420000000000000373 ) ) ;
#142370 = CARTESIAN_POINT ( 'NONE',  ( 3.959615635602866668, 1.756445048235187212, -0.2166398133998989062 ) ) ;
#142369 = CARTESIAN_POINT ( 'NONE',  ( 4.962875334715753262, 0.2052988877573138915, -2.080521221900538009 ) ) ;
#142371 = CARTESIAN_POINT ( 'NONE',  ( -8.065673738749977062, 13.99999998464209305, 8.613976760017859391 ) ) ;
#142372 = CARTESIAN_POINT ( 'NONE',  ( 6.316396932256916230, 2.136508426756661638, 0.8310160958180726753 ) ) ;
#142373 = CARTESIAN_POINT ( 'NONE',  ( 5.261534320672216936, 0.8623632012556389226, 1.511560460804670880 ) ) ;
#142374 = CARTESIAN_POINT ( 'NONE',  ( 6.428537391173986038, 10.65171072301167854, 0.7998128361456462443 ) ) ;
#142375 = CARTESIAN_POINT ( 'NONE',  ( 5.942043047034061942, -1.969448396301001436, -1.185220976332189924 ) ) ;
#142376 = CARTESIAN_POINT ( 'NONE',  ( 2.971951545985364262, 6.549969527005830905, 0.4930404537322597980 ) ) ;
#142377 = CARTESIAN_POINT ( 'NONE',  ( 5.536419981033642301, 1.670246277208887742, -0.4650152690930853816 ) ) ;
#142378 = CARTESIAN_POINT ( 'NONE',  ( 5.758309058547314230, -2.171350062218261989, -0.005773456755737981470 ) ) ;
#142379 = CARTESIAN_POINT ( 'NONE',  ( -0.7500000000000006661, 11.20833333333333393, -1.299038105676657340 ) ) ;
#142380 = CARTESIAN_POINT ( 'NONE',  ( 6.491432910188612126, -0.4373703761123280964, 1.975813455233149218 ) ) ;
#142381 = CARTESIAN_POINT ( 'NONE',  ( 4.562500000000002665, -1.451031289061298857, -1.451031289060931595 ) ) ;
#142382 = CARTESIAN_POINT ( 'NONE',  ( -1.499999999999997780, 5.431250000682820378, 1.214306433183764966E-14 ) ) ;
#142383 = CARTESIAN_POINT ( 'NONE',  ( 4.120081753510516975, -0.9896868749219210892, -1.652585292789155558 ) ) ;
#142384 = CARTESIAN_POINT ( 'NONE',  ( -1.402160292154681736E-14, 11.59375000068279427, 1.732050807568881190 ) ) ;
#142385 = CARTESIAN_POINT ( 'NONE',  ( 0.01275469579824477576, -2.220946917248843189, -0.04775700320917666830 ) ) ;
#142386 = VERTEX_POINT ( 'NONE', #99967 ) ;
#142387 = CARTESIAN_POINT ( 'NONE',  ( 1.499999999999990896, 4.525000000000021672, 1.214306433183764966E-14 ) ) ;
#142388 = CARTESIAN_POINT ( 'NONE',  ( 4.847203612085560387, 5.613824621309978724, -1.199719254218452047 ) ) ;
#142389 = CARTESIAN_POINT ( 'NONE',  ( 7.253775878511261155, 8.421492265473332850, 1.199719254218462483 ) ) ;
#142390 = CARTESIAN_POINT ( 'NONE',  ( 2.385647502782287432, 0.1060323020976374625, -2.218877139873560278 ) ) ;
#142391 = CARTESIAN_POINT ( 'NONE',  ( 0.000000000000000000, 0.000000000000000000, 0.000000000000000000 ) ) ;
#142392 = CARTESIAN_POINT ( 'NONE',  ( 7.293923454472087897, 8.572294120714675003, 1.082531754730558626 ) ) ;
#142393 = CARTESIAN_POINT ( 'NONE',  ( -9.124274191872636663, 11.66807252865000244, -1.443375672974058777 ) ) ;
#142394 = AXIS2_PLACEMENT_3D ( 'NONE', #118052, #36719, #84414 ) ;
#142395 = CARTESIAN_POINT ( 'NONE',  ( 7.349928672384120176, 7.747540670635879145, 0.7216878364870267237 ) ) ;
#142396 = CARTESIAN_POINT ( 'NONE',  ( 0.8795299900376440938, -0.4926441280813895762, -1.955172062459666904 ) ) ;
#142398 = CARTESIAN_POINT ( 'NONE',  ( 4.967260703730732807, 1.792967015482237469, 1.019669102033170516 ) ) ;
#142397 = CARTESIAN_POINT ( 'NONE',  ( 8.751951852821344247, 10.16936423550178503, -1.199719254218446718 ) ) ;
#142399 = CARTESIAN_POINT ( 'NONE',  ( -1.201851678989727383E-14, 5.337500000000019895, -1.732050807568863648 ) ) ;
#142400 = FACE_OUTER_BOUND ( 'NONE', #29212, .T. ) ;
#142401 = CARTESIAN_POINT ( 'NONE',  ( -2.069187086148977173, 1.970899860167975914, 11.59589854942345077 ) ) ;
#142402 = CARTESIAN_POINT ( 'NONE',  ( -1.402160292154681736E-14, 0.4468750003414233563, -1.575800808251665908 ) ) ;
#142403 = CARTESIAN_POINT ( 'NONE',  ( 0.6843625024184678551, -0.2082719882288592839, -1.757362784332392458 ) ) ;
#142404 = CARTESIAN_POINT ( 'NONE',  ( 6.047464834240314779, -1.219521636822028077, 1.233209766127696616 ) ) ;
#142405 = CARTESIAN_POINT ( 'NONE',  ( 5.829613671240826633, 0.8500414093583901209, -1.518663286469445151 ) ) ;
#142406 = CARTESIAN_POINT ( 'NONE',  ( 2.701037021348651646, 1.938191879511786730, 1.223809664465740354 ) ) ;
#142407 = CARTESIAN_POINT ( 'NONE',  ( 0.6823417656249882723, -0.1572916663252488245, 1.181850606188755259 ) ) ;
#142408 = CARTESIAN_POINT ( 'NONE',  ( 1.833694255977034615, 1.820935426717207317, 0.2711280389895084353 ) ) ;
#142409 = CARTESIAN_POINT ( 'NONE',  ( 10.01963921569910632, 11.64833282552586091, 1.199719254218450271 ) ) ;
#142410 =( LENGTH_UNIT ( ) NAMED_UNIT ( * ) SI_UNIT ( .MILLI., .METRE. ) );
#142411 = CARTESIAN_POINT ( 'NONE',  ( 3.082817581614716307, -0.1327354176642106531, -1.820802398864965088 ) ) ;
#142412 = CARTESIAN_POINT ( 'NONE',  ( 3.375625116643202972, -0.3961014713874110305, -1.976955985980306307 ) ) ;
#142413 = CARTESIAN_POINT ( 'NONE',  ( -8.618179199781044630, 13.20629283305325963, 0.7998128361456341429 ) ) ;
#142414 = CARTESIAN_POINT ( 'NONE',  ( -11.41381675112453387, 12.69999999999999929, -3.704697986577184299 ) ) ;
#142415 = CARTESIAN_POINT ( 'NONE',  ( 5.368238606676455582, 1.035150450411811640, 1.833903993397972387 ) ) ;
#142416 = CARTESIAN_POINT ( 'NONE',  ( 9.271941217832353033, 15.45702117623653749, 8.565526717805919787 ) ) ;
#142417 = CARTESIAN_POINT ( 'NONE',  ( 2.154816067267216084, -0.5500195584662926906, -1.995915215819036748 ) ) ;
#142418 = CARTESIAN_POINT ( 'NONE',  ( 2.679707916995359263, 6.278076336469897711, -0.7998128361456291469 ) ) ;
#142419 = CARTESIAN_POINT ( 'NONE',  ( -1.360316468750056851, 0.6510416670080609869, -0.7853790794158981292 ) ) ;
#142420 = CARTESIAN_POINT ( 'NONE',  ( 4.582752651445391123, -1.384437811569695587, 1.606279107262520434 ) ) ;
#142421 = CARTESIAN_POINT ( 'NONE',  ( 1.154767827468632824, -1.519305277103833118, 1.184426060187010465 ) ) ;
#142422 = ORIENTED_EDGE ( 'NONE', *, *, #64571, .F. ) ;
#142423 = CARTESIAN_POINT ( 'NONE',  ( -4.899292406491858820, 6.809203455697518947, -1.599625672291271394 ) ) ;
#142424 = CARTESIAN_POINT ( 'NONE',  ( 8.072990401933337168, 11.50590700464255356, -1.199719254218446718 ) ) ;
#142425 = CARTESIAN_POINT ( 'NONE',  ( 5.438229012412886476, 7.437962829272074750, -1.443375672974078761 ) ) ;
#142426 = CARTESIAN_POINT ( 'NONE',  ( 3.475000000000000533, -1.210416665710750683, 2.006292185433948827 ) ) ;
#142427 = CARTESIAN_POINT ( 'NONE',  ( -4.381256195510448315, 8.263215994737505454, 1.040834085586084257E-14 ) ) ;
#142428 = CARTESIAN_POINT ( 'NONE',  ( 6.064709079624690524, 0.6667526090060638122, 2.013086243192941716 ) ) ;
#142429 = CARTESIAN_POINT ( 'NONE',  ( 2.098786246049421766, -0.5609894644466472124, -2.029802036486601846 ) ) ;
#142431 = CARTESIAN_POINT ( 'NONE',  ( -5.438755897737433287, 6.374245297895642537, -1.199719254218453823 ) ) ;
#142430 = PRESENTATION_LAYER_ASSIGNMENT (  '', '', ( #21291 ) ) ;
#142432 = CARTESIAN_POINT ( 'NONE',  ( 8.776205506747620788, 9.133327934160710981, -0.7998128361456221525 ) ) ;
#142433 = CARTESIAN_POINT ( 'NONE',  ( 6.350447304104193336, -1.851927549110881976, -0.1832485138882292142 ) ) ;
#142434 = CARTESIAN_POINT ( 'NONE',  ( 6.805303039055573322, 10.02693841461847057, 1.199719254218460707 ) ) ;
#142435 = DIRECTION ( 'NONE',  ( -3.491481338843133355E-15, 0.000000000000000000, -1.000000000000000000 ) ) ;
#142436 = CARTESIAN_POINT ( 'NONE',  ( -5.659602779061863487, 5.567567761852417085, 0.7998128361456281477 ) ) ;
#142438 = ORIENTED_EDGE ( 'NONE', *, *, #186296, .T. ) ;
#142437 = CARTESIAN_POINT ( 'NONE',  ( -10.48008955368359629, 11.32911868882677986, 1.040834085586084257E-14 ) ) ;
#142439 = CARTESIAN_POINT ( 'NONE',  ( 0.2289750728588327566, 1.457791096766167360, -1.540313549178488284 ) ) ;
#142440 =( LENGTH_UNIT ( ) NAMED_UNIT ( * ) SI_UNIT ( .MILLI., .METRE. ) );
#142442 = CARTESIAN_POINT ( 'NONE',  ( 2.682025323810240280, -1.127217178123595565, -1.605522638798158264 ) ) ;
#142441 = CARTESIAN_POINT ( 'NONE',  ( -1.225000000000042277, -0.9791666666666447583, 0.7072540797572656190 ) ) ;
#142443 = CARTESIAN_POINT ( 'NONE',  ( 1.499129196564863209, 1.767075381950654611, -1.244890797856931686 ) ) ;
#142445 = CARTESIAN_POINT ( 'NONE',  ( -6.133411998150831046, 5.998805638374869353, -0.1291943307598683033 ) ) ;
#142444 = CARTESIAN_POINT ( 'NONE',  ( -5.808742468812186033, 5.741564066561132940, 0.000000000000000000 ) ) ;
#142446 = CARTESIAN_POINT ( 'NONE',  ( -1.201851678989727383E-14, 1.821875000341421691, 1.575800808251672791 ) ) ;
#142447 = CARTESIAN_POINT ( 'NONE',  ( 2.431276410161122392, 0.8208083392724160321, -1.534589408508793440 ) ) ;
#142448 = CARTESIAN_POINT ( 'NONE',  ( 6.317736394288135493, 8.393778431468064127, 1.443375672974076540 ) ) ;
#142449 = CARTESIAN_POINT ( 'NONE',  ( -10.88575987782614796, 5.812703298851592315, -6.395352192321499984 ) ) ;
#142450 = CIRCLE ( 'NONE', #17754, 0.5000000000000004441 ) ;
#142451 = CARTESIAN_POINT ( 'NONE',  ( 2.337267334706777611, -1.242538083881424837, 1.587593183769491878 ) ) ;
#142452 = CARTESIAN_POINT ( 'NONE',  ( -0.08500055850267987378, -9.912493587006867557, -10.99967158169069847 ) ) ;
#142453 = CARTESIAN_POINT ( 'NONE',  ( -5.483346782084204563, 5.361935765378481378, 0.000000000000000000 ) ) ;
#142454 = CARTESIAN_POINT ( 'NONE',  ( 2.764479830724082543, -1.360639549628063882, 1.426867346614549836 ) ) ;
#142456 = CARTESIAN_POINT ( 'NONE',  ( -6.292392690518214593, 7.474117906093608710, -1.082531754730549967 ) ) ;
#142455 = CARTESIAN_POINT ( 'NONE',  ( 5.783449990912790106, 0.1341079605299954347, -1.907733270042926810 ) ) ;
#142457 = CARTESIAN_POINT ( 'NONE',  ( -6.753369912938502750, 7.051555451282599307, 0.000000000000000000 ) ) ;
#142458 = CARTESIAN_POINT ( 'NONE',  ( 5.254667053748194760, 8.288139441751686931, 1.199719254218452047 ) ) ;
#142459 = CARTESIAN_POINT ( 'NONE',  ( -5.582925393777276035, 9.735439736040634173, 0.7998128361456291469 ) ) ;
#142460 = CARTESIAN_POINT ( 'NONE',  ( 1.172527652694483669, 0.8205418800426617087, 1.845675728695548745 ) ) ;
#142461 = CARTESIAN_POINT ( 'NONE',  ( 3.782361668088245921, 6.396210465202840645, -1.082531754730548412 ) ) ;
#142462 = CARTESIAN_POINT ( 'NONE',  ( 6.176872536373793743, -2.188556106905717780, -0.7317919303653409591 ) ) ;
#142463 = CARTESIAN_POINT ( 'NONE',  ( 5.828557447170540584, -1.245780601409246957, 1.515539014345569147 ) ) ;
#142464 = CARTESIAN_POINT ( 'NONE',  ( 3.221486639279776298, 0.2924833653642990861, -1.939731193138781951 ) ) ;
#142465 = CARTESIAN_POINT ( 'NONE',  ( 7.964525173024008531, 11.37936423758166526, 1.199719254218460707 ) ) ;
#142466 = CARTESIAN_POINT ( 'NONE',  ( 1.143204175302305670, 0.8197749522141674072, 1.842446510343001442 ) ) ;
#142467 = ORIENTED_EDGE ( 'NONE', *, *, #31970, .F. ) ;
#142468 = CARTESIAN_POINT ( 'NONE',  ( 0.7084050413898737020, 1.255986415914780885, -1.704487872487458144 ) ) ;
#142470 = CARTESIAN_POINT ( 'NONE',  ( -5.371001409308059138, 9.417918744168066070, -0.7998128361456231517 ) ) ;
#142469 = CARTESIAN_POINT ( 'NONE',  ( -3.541704441667874903, 5.155074486744371853, -1.599625672291256295 ) ) ;
#142471 = CARTESIAN_POINT ( 'NONE',  ( 1.868857239601273923, 1.762127240619456803, -0.5335365013287920455 ) ) ;
#142472 = ORIENTED_EDGE ( 'NONE', *, *, #208381, .T. ) ;
#142473 = CARTESIAN_POINT ( 'NONE',  ( 11.62584726340593377, 8.214503055780935981, 3.002169211754254885 ) ) ;
#142474 = CARTESIAN_POINT ( 'NONE',  ( 2.830460552442021438, -1.048868820301660953, -1.842999677239331113 ) ) ;
#142475 = CARTESIAN_POINT ( 'NONE',  ( -1.499999999999997780, 4.431250000682819490, 1.214306433183764966E-14 ) ) ;
#142476 = CARTESIAN_POINT ( 'NONE',  ( 7.182068686937156166, 9.402166106225269715, 1.599625672291281386 ) ) ;
#142477 = CARTESIAN_POINT ( 'NONE',  ( 7.201315867513990554, 8.430565262634994284, -1.199719254218452047 ) ) ;
#142478 = CARTESIAN_POINT ( 'NONE',  ( 2.706383518077785322, -0.7856088873096721548, -1.905365358233277240 ) ) ;
#142480 = CARTESIAN_POINT ( 'NONE',  ( 1.346931166825489967, 0.5339940059071214273, -1.762130705996706181 ) ) ;
#142479 = CARTESIAN_POINT ( 'NONE',  ( -7.771848369131641121, 10.09024240211882351, -1.599625672291263179 ) ) ;
#142481 = CARTESIAN_POINT ( 'NONE',  ( -1.364683531250010295, 4.780208333674755394, 0.7879004041258379498 ) ) ;
#142482 = CARTESIAN_POINT ( 'NONE',  ( -1.737500000000000266, -2.858333333333334281, -3.009438278150923907 ) ) ;
#142483 = CARTESIAN_POINT ( 'NONE',  ( 1.352862181796068208, 4.252167665669599472, -0.3040832447043536058 ) ) ;
#142484 = CARTESIAN_POINT ( 'NONE',  ( 2.881411693390222961, 6.438990010880548454, -0.3632046419933783743 ) ) ;
#142485 = AXIS2_PLACEMENT_3D ( 'NONE', #47831, #61923, #95519 ) ;
#142486 = CARTESIAN_POINT ( 'NONE',  ( 1.313402753022639091, 1.947697196196996217, 1.037691534346518729 ) ) ;
#142487 = CARTESIAN_POINT ( 'NONE',  ( 3.163607282743227334, 0.3354078767881124024, -2.237311900363625483 ) ) ;
#142488 = VECTOR ( 'NONE', #70608, 1000.000000000000000 ) ;
#142489 = CARTESIAN_POINT ( 'NONE',  ( -7.971831135155409420, 11.28392484344787405, 1.082531754730549967 ) ) ;
#142490 = CARTESIAN_POINT ( 'NONE',  ( 2.953145165254339233, -1.595657772652997464, 0.8577772064107972438 ) ) ;
#142491 = CARTESIAN_POINT ( 'NONE',  ( 3.309697661505988986, -1.145383095959727315, -1.535415057543190409 ) ) ;
#142492 = CARTESIAN_POINT ( 'NONE',  ( 4.756339170418532269, -2.069830778647030023, -0.05414847147890837487 ) ) ;
#142493 = CARTESIAN_POINT ( 'NONE',  ( -0.6823417656250003738, 2.780208333674753618, -1.181850606188749264 ) ) ;
#142494 = CARTESIAN_POINT ( 'NONE',  ( 2.623849442957484346, -1.133682707547468471, -1.612724008377570017 ) ) ;
#142495 = CARTESIAN_POINT ( 'NONE',  ( 0.08292192553204823235, -0.1316706149618769306, -1.895886810074402185 ) ) ;
#142496 = CARTESIAN_POINT ( 'NONE',  ( 3.010468980803046257, 1.356049738124785353, -1.288842618233053683 ) ) ;
#142497 = ADVANCED_FACE ( 'NONE', ( #166032 ), #166448, .T. ) ;
#142499 = CARTESIAN_POINT ( 'NONE',  ( 4.602896574056089207, 8.480248385054199645, 0.1803159889683242367 ) ) ;
#142498 = CARTESIAN_POINT ( 'NONE',  ( 2.333053021162025953, 2.238922732217122125, 0.5587339331782120722 ) ) ;
#142500 = CARTESIAN_POINT ( 'NONE',  ( 3.771788145607783527, -1.833817148065859604, 0.3161742572238452897 ) ) ;
#142501 = CARTESIAN_POINT ( 'NONE',  ( -1.201851678989727383E-14, 3.696875000341422801, -1.575800808251660134 ) ) ;
#142502 = CARTESIAN_POINT ( 'NONE',  ( -3.113568832632681360, 6.784247404713427798, -0.7998128361456281477 ) ) ;
#142503 = CARTESIAN_POINT ( 'NONE',  ( 7.461064606222022277, 7.598996883547496139, 1.040834085586084257E-14 ) ) ;
#142504 = CARTESIAN_POINT ( 'NONE',  ( -1.362971619486218700, 3.697045066695971105, 0.6272962186313906230 ) ) ;
#142505 = CARTESIAN_POINT ( 'NONE',  ( 0.8562495616285453748, 2.103569811481691865, -0.1051806538951201714 ) ) ;
#142506 = CARTESIAN_POINT ( 'NONE',  ( 1.364683531249990311, 4.676041667008083103, 0.7879004041258500513 ) ) ;
#142507 = CARTESIAN_POINT ( 'NONE',  ( 5.993488848236776967, 1.632462841753023808, 1.416962642945495565 ) ) ;
#142508 = CARTESIAN_POINT ( 'NONE',  ( 6.481118763745143063, -1.847444428138062422, -0.8165197575118980922 ) ) ;
#142509 = CARTESIAN_POINT ( 'NONE',  ( -0.6823417656250003738, -0.7822916663252423852, -1.181850606188749264 ) ) ;
#142510 = CARTESIAN_POINT ( 'NONE',  ( -3.768803514918943609, 7.340761834139994058, 0.7216878364870317197 ) ) ;
#142513 = CARTESIAN_POINT ( 'NONE',  ( 3.551873057100287223, 5.166937871415542283, 1.443375672974062551 ) ) ;
#142512 = CARTESIAN_POINT ( 'NONE',  ( 6.925078400183574345, 6.038986730273901316, 2.350556043039519150 ) ) ;
#142511 = CARTESIAN_POINT ( 'NONE',  ( 4.701645408888975197, 8.707279753670952971, 0.000000000000000000 ) ) ;
#142514 = CARTESIAN_POINT ( 'NONE',  ( -0.2104748580754183529, 0.2283854016844401591, -2.137091067173245929 ) ) ;
#142515 = CARTESIAN_POINT ( 'NONE',  ( 4.487517715496184501, -0.5331711073110931842, 1.944729879240604253 ) ) ;
#142517 = CARTESIAN_POINT ( 'NONE',  ( -5.248414861821563804, 9.137251415518218067, 0.7216878364870267237 ) ) ;
#142516 = CARTESIAN_POINT ( 'NONE',  ( -10.15469386695561482, 10.94949038764413096, 1.040834085586084257E-14 ) ) ;
#142518 =( NAMED_UNIT ( * ) PLANE_ANGLE_UNIT ( ) SI_UNIT ( $, .RADIAN. ) );
#142520 = CARTESIAN_POINT ( 'NONE',  ( -1.364683531250010740, 10.13020833367472839, 0.7879004041258445001 ) ) ;
#142519 = CARTESIAN_POINT ( 'NONE',  ( 5.858325616802108726, 0.8718737102157668728, 1.978260574764856283 ) ) ;
#142521 = CARTESIAN_POINT ( 'NONE',  ( -11.12441040585762408, 5.813956397379768326, 4.514688396320016395 ) ) ;
#142523 = CARTESIAN_POINT ( 'NONE',  ( 6.134388704033759687, 0.6352148712998658686, 1.913799669303432927 ) ) ;
#142522 = CARTESIAN_POINT ( 'NONE',  ( -7.199016378732087773, 7.501199984716642177, 0.7216878364870317197 ) ) ;
#142524 = CARTESIAN_POINT ( 'NONE',  ( 0.6823417656249899377, 0.6552083336747518416, 1.181850606188755259 ) ) ;
#142525 = EDGE_CURVE ( 'NONE', #114168, #173093, #85724, .T. ) ;
#142526 = FACE_OUTER_BOUND ( 'NONE', #182541, .T. ) ;
#142527 = CARTESIAN_POINT ( 'NONE',  ( -0.7500000000000006661, 8.708333333333332149, -1.299038105676657340 ) ) ;
#142528 = CARTESIAN_POINT ( 'NONE',  ( 1.506044924156377807, -0.6181864485952697219, -1.610478869194363227 ) ) ;
#142529 = CARTESIAN_POINT ( 'NONE',  ( 6.373214726875630731, 9.593111727067046957, 1.199719254218452047 ) ) ;
#142530 = AXIS2_PLACEMENT_3D ( 'NONE', #211779, #115425, #98070 ) ;
#142531 = CARTESIAN_POINT ( 'NONE',  ( 6.690022453700429139, 6.769724048930809701, 0.7998128361456331437 ) ) ;
#142532 = CARTESIAN_POINT ( 'NONE',  ( 1.364683531249986537, -0.7822916663252464931, -0.7879004041258309554 ) ) ;
#142533 = CARTESIAN_POINT ( 'NONE',  ( 0.5964902553294594290, 1.476022596236561846, -0.9760666246667221158 ) ) ;
#142534 = CARTESIAN_POINT ( 'NONE',  ( 1.752591402120354358, 1.991486659738419984, 0.2933061901304565011 ) ) ;
#142535 =( NAMED_UNIT ( * ) PLANE_ANGLE_UNIT ( ) SI_UNIT ( $, .RADIAN. ) );
#142536 = CARTESIAN_POINT ( 'NONE',  ( 2.860407222358963608, 5.320596945185329218, 1.082531754730548412 ) ) ;
#142537 = CARTESIAN_POINT ( 'NONE',  ( 3.944505925199864649, 2.195883038551619038, 0.2190369969904403802 ) ) ;
#142538 = CARTESIAN_POINT ( 'NONE',  ( 5.207971749312423348, 0.6875717650507988665, -2.059362367386765591 ) ) ;
#142539 = EDGE_LOOP ( 'NONE', ( #171808, #54270, #46379, #5620 ) ) ;
#142540 = CARTESIAN_POINT ( 'NONE',  ( 5.096939404094710468, 4.911127157724081371, 0.000000000000000000 ) ) ;
#142541 = CARTESIAN_POINT ( 'NONE',  ( 6.751597309481075726, 10.82068792779586985, 1.040834085586084257E-14 ) ) ;
#142543 = CARTESIAN_POINT ( 'NONE',  ( 3.286732619643798703, 1.587825416925658262, -1.242744175535138940 ) ) ;
#142542 = CARTESIAN_POINT ( 'NONE',  ( 3.106218681870171139, -0.8574772492565514437, 1.939554460742904274 ) ) ;
#142545 = ORIENTED_EDGE ( 'NONE', *, *, #125104, .F. ) ;
#142544 = CARTESIAN_POINT ( 'NONE',  ( 3.867288652163490159, -1.509380944159900428, -1.001465339209107075 ) ) ;
#142546 = CARTESIAN_POINT ( 'NONE',  ( 5.956828388357757298, 8.042995434541133193, 1.599625672291269396 ) ) ;
#142547 = ORIENTED_EDGE ( 'NONE', *, *, #50310, .T. ) ;
#142548 = CARTESIAN_POINT ( 'NONE',  ( 0.7427767429722329506, -1.606530860214189893, 0.9580933318182258684 ) ) ;
#142549 = VECTOR ( 'NONE', #59035, 1000.000000000000000 ) ;
#142550 = CARTESIAN_POINT ( 'NONE',  ( 5.654876981934024549, -1.436564326775534806, 1.126588154728463742 ) ) ;
#142552 = CARTESIAN_POINT ( 'NONE',  ( 1.077184250232362306, 1.452872634298128629, 1.248800971253192005 ) ) ;
#142551 = CARTESIAN_POINT ( 'NONE',  ( -1.499999999999993339, 10.64264068711930733, 1.232676135170975238E-14 ) ) ;
#142553 = CARTESIAN_POINT ( 'NONE',  ( -9.470156251935129887, 4.005132839944305800, -6.837168546664702085 ) ) ;
#142554 = CARTESIAN_POINT ( 'NONE',  ( -0.6823417656250212460, 2.113541667008083991, 1.181850606188767472 ) ) ;
#142555 = DIRECTION ( 'NONE',  ( 0.9366510587354612838, 0.000000000000000000, 0.3502638921866474409 ) ) ;
#142556 = CARTESIAN_POINT ( 'NONE',  ( 5.313408243115378404, -0.3210861823062812759, 2.137610926513198617 ) ) ;
#142557 = CARTESIAN_POINT ( 'NONE',  ( -5.668717624289589807, 5.786127781192186958, 0.7216878364870257245 ) ) ;
#142558 = EDGE_CURVE ( 'NONE', #160336, #4753, #40876, .T. ) ;
#142559 = CARTESIAN_POINT ( 'NONE',  ( -5.589704470584107909, 9.743348658981940247, -0.7998128361456362523 ) ) ;
#142560 = CARTESIAN_POINT ( 'NONE',  ( 2.971057270251746374, -1.603071526910588629, 1.388259434452358665 ) ) ;
#142562 = CARTESIAN_POINT ( 'NONE',  ( -11.68287950975655676, 8.167437761341201252, 4.460353674290588266 ) ) ;
#142561 = CARTESIAN_POINT ( 'NONE',  ( -0.1296875068448125057, 0.2507808023153486054, -1.861542470327881560 ) ) ;
#142563 = CARTESIAN_POINT ( 'NONE',  ( 4.745367521161733215, -1.522072814771213922, -1.252777155790285590 ) ) ;
#142564 = CARTESIAN_POINT ( 'NONE',  ( 6.205323455156911194, 1.660478276859885582, -0.9486371710855368011 ) ) ;
#142565 = ORIENTED_EDGE ( 'NONE', *, *, #85154, .T. ) ;
#142566 = CARTESIAN_POINT ( 'NONE',  ( 0.05257324754554763141, -1.379058229334565455, 1.606613856852637356 ) ) ;
#142567 = CARTESIAN_POINT ( 'NONE',  ( 7.694789056592527210, 14.38989046813754946, 9.211249139029591859 ) ) ;
#142568 = CARTESIAN_POINT ( 'NONE',  ( 1.135311898753359472, -0.04898221611688948623, -2.069941200615910581 ) ) ;
#142569 = CARTESIAN_POINT ( 'NONE',  ( 2.484236259141327618, -0.3323325037456366093, -1.913154051555246316 ) ) ;
#142570 = VERTEX_POINT ( 'NONE', #106981 ) ;
#142571 = CARTESIAN_POINT ( 'NONE',  ( 4.518610335104485287, 8.493738834255713854, 0.000000000000000000 ) ) ;
#142572 = CARTESIAN_POINT ( 'NONE',  ( 5.956828388357757298, 8.042995434541133193, 1.599625672291269396 ) ) ;
#142574 = CARTESIAN_POINT ( 'NONE',  ( 7.006866460164219212, 7.069099046480051385, -0.7998128361456281477 ) ) ;
#142573 = CARTESIAN_POINT ( 'NONE',  ( 3.837900784552390476, 2.080585211200749018, 0.2046572434392830431 ) ) ;
#142575 = CARTESIAN_POINT ( 'NONE',  ( 3.675669042636310557, 6.342012078834061484, -1.082531754730549967 ) ) ;
#142577 = VERTEX_POINT ( 'NONE', #139439 ) ;
#142576 = CARTESIAN_POINT ( 'NONE',  ( 0.7503001202024300875, 1.784421795204504946, 0.3107989935832651818 ) ) ;
#142578 = CARTESIAN_POINT ( 'NONE',  ( 5.496761087669068679, -0.5331231007881258588, -2.141394884921154151 ) ) ;
#142579 = CARTESIAN_POINT ( 'NONE',  ( -9.003941998343226207E-15, -6.291672674598899562, -10.90688615205694845 ) ) ;
#142580 = AXIS2_PLACEMENT_3D ( 'NONE', #134246, #86526, #168840 ) ;
#142581 = CARTESIAN_POINT ( 'NONE',  ( 2.766872162265196611, -1.522532973755141850, 1.597636210702752635 ) ) ;
#142582 = LINE ( 'NONE', #208589, #203413 ) ;
#142583 = EDGE_CURVE ( 'NONE', #79391, #213798, #67833, .T. ) ;
#142584 = CARTESIAN_POINT ( 'NONE',  ( 1.453610327690219473, -1.385809040371610346, -1.317956379189986871 ) ) ;
#142585 = CARTESIAN_POINT ( 'NONE',  ( 7.560643217915098191, 11.97250085420964716, -0.7998128361456291469 ) ) ;
#142586 = CARTESIAN_POINT ( 'NONE',  ( 5.441872305809390298, 1.387781221417656141, 1.536568222347669987 ) ) ;
#142588 = CARTESIAN_POINT ( 'NONE',  ( 2.360439101503517101, 0.9236781337260314695, 1.954550705658316456 ) ) ;
#142587 = CARTESIAN_POINT ( 'NONE',  ( 1.579999999999991189, 8.674529973577531194, -2.499999999999989342 ) ) ;
#142589 = CARTESIAN_POINT ( 'NONE',  ( 5.372676843235411503, -0.05303982195071360595, -2.191091664329389399 ) ) ;
#142590 = ORIENTED_EDGE ( 'NONE', *, *, #25220, .F. ) ;
#142591 = DIRECTION ( 'NONE',  ( 0.7592566023653005702, -0.6507913734559639396, 0.000000000000000000 ) ) ;
#142592 = LINE ( 'NONE', #157756, #62926 ) ;
#142593 = CARTESIAN_POINT ( 'NONE',  ( -0.3006164276377518707, 8.220220202721305824, 1.980250916746241652 ) ) ;
#142594 = CARTESIAN_POINT ( 'NONE',  ( 3.627688620108284745, 6.389997935838436227, 1.199719254218452047 ) ) ;
#142595 = CARTESIAN_POINT ( 'NONE',  ( -1.364683531250000748, 15.42187500034139447, 0.000000000000000000 ) ) ;
#142596 = CARTESIAN_POINT ( 'NONE',  ( -8.188761592974040937, 11.53701037756964887, -1.082531754730543971 ) ) ;
#142597 = CARTESIAN_POINT ( 'NONE',  ( 4.525389411911321602, 8.501647757197021704, -0.7998128361456381397 ) ) ;
#142598 = CARTESIAN_POINT ( 'NONE',  ( 6.069205674026176389, 1.823072449729469247, 0.9810699074010442722 ) ) ;
#142599 = CARTESIAN_POINT ( 'NONE',  ( 3.897031312914517098, 1.626875583419360005, -1.031562066982329329 ) ) ;
#142600 = CARTESIAN_POINT ( 'NONE',  ( 0.3160300859305562593, 1.034144755472726995, -1.730879882831819705 ) ) ;
#142601 = CARTESIAN_POINT ( 'NONE',  ( 0.000000000000000000, -6.134628647623513231, 10.91970695577495931 ) ) ;
#142602 = CARTESIAN_POINT ( 'NONE',  ( 5.335297142177534369, 6.183267073083954735, -1.199719254218452047 ) ) ;
#142604 = EDGE_CURVE ( 'NONE', #145077, #91753, #95592, .T. ) ;
#142603 = CARTESIAN_POINT ( 'NONE',  ( 0.4019237886466816012, 13.17633545031536890, -1.499999999999998668 ) ) ;
#142605 = CARTESIAN_POINT ( 'NONE',  ( 4.979337304519595442, -0.1005905848140927622, 1.967025916208066327 ) ) ;
#142606 = CARTESIAN_POINT ( 'NONE',  ( 6.527265088719197195, -1.491963682546100900, -1.740339723829595453 ) ) ;
#142607 = CARTESIAN_POINT ( 'NONE',  ( 5.215394836314163562, -0.2642288504575221464, 1.806346989861665087 ) ) ;
#142608 = EDGE_CURVE ( 'NONE', #41918, #11599, #171924, .T. ) ;
#142609 = CARTESIAN_POINT ( 'NONE',  ( 7.865138509703455405, 8.348618814175074121, -0.7216878364870317197 ) ) ;
#142610 = CARTESIAN_POINT ( 'NONE',  ( 3.429849674132933846, 5.024577257953626308, -1.443375672974058777 ) ) ;
#142611 = CARTESIAN_POINT ( 'NONE',  ( -6.629010762438975135, 6.698543742459062145, -0.7998128361456362523 ) ) ;
#142612 = CARTESIAN_POINT ( 'NONE',  ( 5.041653019435334393, 6.975290837464928728, -1.599625672291269396 ) ) ;
#142613 = ORIENTED_EDGE ( 'NONE', *, *, #158235, .F. ) ;
#142615 = CARTESIAN_POINT ( 'NONE',  ( 5.783453021694040963, 0.1439598661895292731, -2.008088619348106896 ) ) ;
#142614 = CARTESIAN_POINT ( 'NONE',  ( 3.227900028218867234, 1.797025815167479390, 0.4004103908350764573 ) ) ;
#142616 = CARTESIAN_POINT ( 'NONE',  ( 1.124856824619735463, 0.4467566299657543816, -2.254411929275771609 ) ) ;
#142617 = CARTESIAN_POINT ( 'NONE',  ( 5.348475771816908697, -1.946495798708135938, -0.2439133590248846462 ) ) ;
#142618 = CARTESIAN_POINT ( 'NONE',  ( -5.042743069279040036, 7.970618449879118828, 1.199719254218464037 ) ) ;
#142619 = CARTESIAN_POINT ( 'NONE',  ( -5.343912927829680193, 6.631183989036703252, -1.180091537758539921 ) ) ;
#142620 = CARTESIAN_POINT ( 'NONE',  ( -2.286521462199063492, 5.819358805874190743, 1.040834085586084257E-14 ) ) ;
#142621 = CARTESIAN_POINT ( 'NONE',  ( 0.5024991115675537801, 2.064720838319131779, 0.1538615064654233477 ) ) ;
#142622 = CARTESIAN_POINT ( 'NONE',  ( -4.984557751679625781, 5.844347460828191565, 1.199719254218452935 ) ) ;
#142624 = CARTESIAN_POINT ( 'NONE',  ( 6.719637426148988624, -1.715392417075599196, 0.4352852820774539833 ) ) ;
#142623 = CARTESIAN_POINT ( 'NONE',  ( 1.857086946601906652, 0.3542020299988774545, -2.060351931225719468 ) ) ;
#142625 = CARTESIAN_POINT ( 'NONE',  ( -8.917737905728749581, 3.447199233515649386, -8.029567276306266876 ) ) ;
#142626 = ORIENTED_EDGE ( 'NONE', *, *, #64812, .T. ) ;
#142627 = CARTESIAN_POINT ( 'NONE',  ( -0.2102771530458458771, 0.2260464284578807270, -2.237246294970319127 ) ) ;
#142628 = CARTESIAN_POINT ( 'NONE',  ( 2.383973883943972805, -0.2989522671389834851, -1.714397271258593092 ) ) ;
#142629 = CARTESIAN_POINT ( 'NONE',  ( 6.634017235788401301, 6.634108284708264414, 0.7998128361456341429 ) ) ;
#142631 = CARTESIAN_POINT ( 'NONE',  ( 1.567523721964578121, 8.684745761082966808, 2.500978756717656015 ) ) ;
#142630 = PLANE ( 'NONE',  #158706 ) ;
#142632 = CARTESIAN_POINT ( 'NONE',  ( 2.261930500750704454, 0.7363377991795038158, 1.559957641100855330 ) ) ;
#142633 = CARTESIAN_POINT ( 'NONE',  ( 2.314256413632868714, 1.428969747754246233, -1.661726224907192684 ) ) ;
#142634 = CARTESIAN_POINT ( 'NONE',  ( 0.1231123065759693186, 0.2931380485183229800, 1.709000606096510166 ) ) ;
#142635 = CARTESIAN_POINT ( 'NONE',  ( 4.846401659255799466, 2.200796399388889935, 0.1645688927329121420 ) ) ;
#142636 = CARTESIAN_POINT ( 'NONE',  ( -10.82855876678636520, 5.585670971531701667, -6.509986581443756748 ) ) ;
#142637 = CIRCLE ( 'NONE', #49230, 0.07999999999999951594 ) ;
#142638 = CARTESIAN_POINT ( 'NONE',  ( 2.958077724197702096, -0.6850214551260015439, 2.060201288156039645 ) ) ;
#142639 = CARTESIAN_POINT ( 'NONE',  ( 0.9260630535584664091, 1.089557764695957554, -1.464779044915397455 ) ) ;
#142640 = CARTESIAN_POINT ( 'NONE',  ( 3.837202554855035697, -1.762604653963547818, -1.172905022591600233 ) ) ;
#142641 = AXIS2_PLACEMENT_3D ( 'NONE', #5760, #89205, #208248 ) ;
#142642 = CARTESIAN_POINT ( 'NONE',  ( 6.539320575229216281, 4.696526872534390940, 2.559412612844500057 ) ) ;
#142643 = VERTEX_POINT ( 'NONE', #170851 ) ;
#142645 = CARTESIAN_POINT ( 'NONE',  ( -1.402160292154681736E-14, 1.259375000341419248, -1.575800808251659024 ) ) ;
#142644 = CARTESIAN_POINT ( 'NONE',  ( 4.177453601039508690, 1.497175104222212783, 1.735980874517801587 ) ) ;
#142646 = CARTESIAN_POINT ( 'NONE',  ( 4.325214697959421706, 5.004837554829479451, 1.199719254218462483 ) ) ;
#142647 = CARTESIAN_POINT ( 'NONE',  ( 6.516288422252827672, -2.220882151245454850, 0.05110445944340144542 ) ) ;
#142648 = CARTESIAN_POINT ( 'NONE',  ( -6.155038550924159857, 8.203964280876741455, 1.443375672974078761 ) ) ;
#142649 = CARTESIAN_POINT ( 'NONE',  ( 2.901081683644312736, 6.328419697652925002, 0.7216878364870338292 ) ) ;
#142650 = CARTESIAN_POINT ( 'NONE',  ( -5.029711800545518585, 8.811821500704338561, 0.7216878364870458196 ) ) ;
#142651 = CARTESIAN_POINT ( 'NONE',  ( 2.943528747942701695, 6.448217615992859919, 0.000000000000000000 ) ) ;
#142652 = ORIENTED_EDGE ( 'NONE', *, *, #164009, .F. ) ;
#142653 = CARTESIAN_POINT ( 'NONE',  ( 4.535779832184696936, -1.617819081767550182, 1.203352566194588746 ) ) ;
#142655 = CARTESIAN_POINT ( 'NONE',  ( 1.692308231870808921, 1.020316376917740575, -1.792489025137546044 ) ) ;
#142654 = CARTESIAN_POINT ( 'NONE',  ( 7.474622759835693131, 7.614814729430110951, -0.7998128361456281477 ) ) ;
#142656 = DIRECTION ( 'NONE',  ( 0.000000000000000000, 0.000000000000000000, 1.000000000000000000 ) ) ;
#142657 = CARTESIAN_POINT ( 'NONE',  ( 3.065552130021340194, 6.590578228417936835, 0.000000000000000000 ) ) ;
#142658 = CARTESIAN_POINT ( 'NONE',  ( 3.285556943750000070, -3.084374999522042415, 0.000000000000000000 ) ) ;
#142659 = CARTESIAN_POINT ( 'NONE',  ( -1.001543065824772872E-14, 4.821875000341419693, 1.575800808251672791 ) ) ;
#142660 = CARTESIAN_POINT ( 'NONE',  ( 5.050807487124363782, -1.850163549229045579, -1.174163402404400092 ) ) ;
#142661 = CARTESIAN_POINT ( 'NONE',  ( 4.008435526009396455, -1.928752077057366732, 0.5880193435906443389 ) ) ;
#142662 = CARTESIAN_POINT ( 'NONE',  ( 1.979791773625012352, -1.805961398883266344, -0.3578489297004632808 ) ) ;
#142663 = CARTESIAN_POINT ( 'NONE',  ( 6.928380191783277908, 8.041863964290678624, 1.199719254218462483 ) ) ;
#142664 =( NAMED_UNIT ( * ) SI_UNIT ( $, .STERADIAN. ) SOLID_ANGLE_UNIT ( ) );
#142665 = CARTESIAN_POINT ( 'NONE',  ( 5.860330175037709921, 0.7421476303169188826, 1.668095884353037128 ) ) ;
#142666 = CARTESIAN_POINT ( 'NONE',  ( -6.877010230629689858, 9.046264573866535486, 1.599625672291283607 ) ) ;
#142668 = CARTESIAN_POINT ( 'NONE',  ( -4.281342646865346602, 8.216926531310035031, 0.7998128361456352531 ) ) ;
#142667 = CARTESIAN_POINT ( 'NONE',  ( 5.770491790047429959, -1.440319307945096217, 1.744843718407377731 ) ) ;
#142669 = CARTESIAN_POINT ( 'NONE',  ( 1.489043601129129701, -0.3103829872296200443, -2.082944856911663312 ) ) ;
#142670 = CARTESIAN_POINT ( 'NONE',  ( -7.110325215724114578, 7.260077271291732082, 0.000000000000000000 ) ) ;
#142671 = CARTESIAN_POINT ( 'NONE',  ( 8.749089199520284410, 9.101692242395490240, 0.7998128361456481317 ) ) ;
#142672 = CARTESIAN_POINT ( 'NONE',  ( 5.519577934094840543, 9.453608333170423705, 0.7216878364870317197 ) ) ;
#142673 = DIRECTION ( 'NONE',  ( -1.000000000000000000, 0.000000000000000000, 2.220446049250313081E-16 ) ) ;
#142674 = CARTESIAN_POINT ( 'NONE',  ( -6.015013705957189316, 10.16926642359206134, 0.7998128361456481317 ) ) ;
#142675 = UNCERTAINTY_MEASURE_WITH_UNIT (LENGTH_MEASURE( 1.000000000000000082E-05 ), #178473, 'distance_accuracy_value', 'NONE');
#142676 = CARTESIAN_POINT ( 'NONE',  ( 6.956180625287912811, -6.372104534815299814, 6.956180625285773189 ) ) ;
#142677 = CARTESIAN_POINT ( 'NONE',  ( 6.602457619730749627, 10.64669162308715222, 0.7216878364870438212 ) ) ;
#142678 = CARTESIAN_POINT ( 'NONE',  ( 4.167679133687917314, 7.375052378509237450, -0.7893339205088979460 ) ) ;
#142679 = CARTESIAN_POINT ( 'NONE',  ( -8.459924665247381625, 11.85336729522185806, 1.082531754730560403 ) ) ;
#142681 = CARTESIAN_POINT ( 'NONE',  ( 2.812952309885875746, -0.6487812942810657901, -2.124531788647378239 ) ) ;
#142680 = CARTESIAN_POINT ( 'NONE',  ( 1.441811196653530747, -1.994930912159533332, 0.7194735443712959588 ) ) ;
#142682 =( GEOMETRIC_REPRESENTATION_CONTEXT ( 3 ) GLOBAL_UNCERTAINTY_ASSIGNED_CONTEXT ( ( #213995 ) ) GLOBAL_UNIT_ASSIGNED_CONTEXT ( ( #101529, #72206, #2931 ) ) REPRESENTATION_CONTEXT ( 'NONE', 'WORKASPACE' ) );
#142683 = CARTESIAN_POINT ( 'NONE',  ( 0.3466626200071438180, 2.201290530325435757, 0.1579762268871589825 ) ) ;
#142684 = CARTESIAN_POINT ( 'NONE',  ( -6.445975688654487001, 6.485002823043819475, -0.7998128361456362523 ) ) ;
#142685 = CARTESIAN_POINT ( 'NONE',  ( 5.229694566569264680, 7.124396299129368337, 1.599625672291267398 ) ) ;
#142686 = CARTESIAN_POINT ( 'NONE',  ( 4.457442142980160504, 1.574409630067734156, 1.170308293268598421 ) ) ;
#142687 = CARTESIAN_POINT ( 'NONE',  ( 7.540305987494599016, 11.94877408538573427, -0.7998128361456291469 ) ) ;
#142688 = CARTESIAN_POINT ( 'NONE',  ( -5.266216980226317013, 6.417262052691032004, 1.151019644853501944 ) ) ;
#142689 = CARTESIAN_POINT ( 'NONE',  ( -1.607015867998815128, 0.9165151389911810886, 1.199999999999999734 ) ) ;
#142690 = CARTESIAN_POINT ( 'NONE',  ( -1.364683531250012516, 1.030208333674754062, 0.7879004041258379498 ) ) ;
#142691 = CARTESIAN_POINT ( 'NONE',  ( -4.163762573172648196, 7.871823745427799501, 0.000000000000000000 ) ) ;
#142693 = EDGE_LOOP ( 'NONE', ( #67795, #62503, #212497, #158810 ) ) ;
#142692 = CARTESIAN_POINT ( 'NONE',  ( -5.829642864196175722, 7.824335979694092558, 1.443375672974064550 ) ) ;
#142694 = CARTESIAN_POINT ( 'NONE',  ( 3.287459871768631636, 0.04819156399121089784, -2.120204644799832394 ) ) ;
#142695 = CARTESIAN_POINT ( 'NONE',  ( -4.288121723672178476, 8.224835454251337552, -0.7998128361456362523 ) ) ;
#142696 = CARTESIAN_POINT ( 'NONE',  ( 4.592742373648754040, -0.4705147408641910944, -2.109722102427157964 ) ) ;
#142697 = CARTESIAN_POINT ( 'NONE',  ( 3.544333174469185721, -1.503253232081468216, 1.062929765333266108 ) ) ;
#142698 = B_SPLINE_CURVE_WITH_KNOTS ( 'NONE', 3,
 ( #74523, #123363, #22538, #75588, #142757, #44168, #126554, #192515, #89725, #24682, #58270, #141698, #205564, #90787, #88646, #154705 ),
 .UNSPECIFIED., .F., .F.,
 ( 4, 2, 2, 2, 2, 2, 2, 4 ),
 ( 0.000000000000000000, 0.0005319996970288863375, 0.001063999394057772675, 0.001595999091086659121, 0.002127998788115545350, 0.002659998485144431796, 0.003191998182173318242, 0.004255997576231089832 ),
 .UNSPECIFIED. ) ;
#142699 = CARTESIAN_POINT ( 'NONE',  ( -5.155981903556834389, 6.496760599866445496, 1.199444197134313272 ) ) ;
#142700 = CARTESIAN_POINT ( 'NONE',  ( -1.364683531250014514, 0.3010416670080866552, -0.7879004041258359514 ) ) ;
#142701 = CARTESIAN_POINT ( 'NONE',  ( 6.263578219495629540, 0.9010232283708031753, 1.488777805958479528 ) ) ;
#142702 = CARTESIAN_POINT ( 'NONE',  ( 6.727182134110209155, 1.290711256955964448, 1.927001067762003972 ) ) ;
#142703 = CARTESIAN_POINT ( 'NONE',  ( 2.738383840280320669, 6.138605547061593448, 0.7216878364870338292 ) ) ;
#142704 = CARTESIAN_POINT ( 'NONE',  ( -6.050251585826448952, 7.027409288634817841, -1.057721621305447890 ) ) ;
#142705 = CARTESIAN_POINT ( 'NONE',  ( 3.116266767097406909, -1.064116542966097922, -1.881565754655416756 ) ) ;
#142706 = TOROIDAL_SURFACE ( 'NONE', #194459, 9.559451093910105612, 0.08000000000000000167 ) ;
#142707 = CARTESIAN_POINT ( 'NONE',  ( 5.536482449520531368, 1.943773098233076757, -0.5350085594507182352 ) ) ;
#142708 = CARTESIAN_POINT ( 'NONE',  ( -7.443063143778079649, 10.66702885350765584, 1.082531754730549967 ) ) ;
#142710 = CARTESIAN_POINT ( 'NONE',  ( 1.833122199354455972, 0.2117775504973731793, 2.151289291301178075 ) ) ;
#142709 = AXIS2_PLACEMENT_3D ( 'NONE', #23999, #205958, #58654 ) ;
#142711 = CARTESIAN_POINT ( 'NONE',  ( 3.198462767114045313, -0.5687421903855809369, -1.887558129442780341 ) ) ;
#142712 = CARTESIAN_POINT ( 'NONE',  ( 0.01162390915069450026, -2.148011843722149372, 0.4338911918742721641 ) ) ;
#142713 = CARTESIAN_POINT ( 'NONE',  ( 1.202667248822903989, -2.307758714249080079, 0.002725711325006137473 ) ) ;
#142714 = CARTESIAN_POINT ( 'NONE',  ( 4.634287131779754709, 0.3355949523314147309, 1.912704035658734592 ) ) ;
#142717 = VERTEX_POINT ( 'NONE', #205474 ) ;
#142716 = CARTESIAN_POINT ( 'NONE',  ( 1.387778780781445676E-16, 4.000000000000003553, -2.500000000000007994 ) ) ;
#142715 = CARTESIAN_POINT ( 'NONE',  ( -9.015808962963337336, 10.58116054728778366, 1.082531754730558626 ) ) ;
#142718 = CARTESIAN_POINT ( 'NONE',  ( -6.981522756394290319, 7.109807735406931783, 0.7998128361456341429 ) ) ;
#142719 = CARTESIAN_POINT ( 'NONE',  ( 0.000000000000000000, -4.500000000000003553, 0.000000000000000000 ) ) ;
#142721 = VERTEX_POINT ( 'NONE', #10471 ) ;
#142720 = CARTESIAN_POINT ( 'NONE',  ( -3.644109427023046521, 7.473487774827342278, 0.000000000000000000 ) ) ;
#142722 = CARTESIAN_POINT ( 'NONE',  ( -7.931156673870055407, 11.23647130528163096, 1.082531754730549967 ) ) ;
#142723 = CARTESIAN_POINT ( 'NONE',  ( 2.063769564651289912, 0.3772465526380370804, -2.174136642525636098 ) ) ;
#142724 = CARTESIAN_POINT ( 'NONE',  ( 1.642778471875001811, -0.6927083328553753638, 2.845375778867859751 ) ) ;
#142725 = CARTESIAN_POINT ( 'NONE',  ( 5.998874280538830206, 0.3792253423284037139, 1.924579554046601970 ) ) ;
#142726 = CARTESIAN_POINT ( 'NONE',  ( -1.201851678989727383E-14, 4.759375000341419693, -1.575800808251660134 ) ) ;
#142727 = CARTESIAN_POINT ( 'NONE',  ( -0.7499999999999972244, 3.889583334016149863, -1.299038105676652011 ) ) ;
#142728 = CARTESIAN_POINT ( 'NONE',  ( 4.834557559160812978, 6.939504195329335268, -1.414529171088283688 ) ) ;
#142730 = DIRECTION ( 'NONE',  ( 0.000000000000000000, -1.000000000000000000, 0.000000000000000000 ) ) ;
#142729 = CARTESIAN_POINT ( 'NONE',  ( 0.1747926744264659826, 0.006858446013176252437, -1.855468577918440332 ) ) ;
#142731 = CARTESIAN_POINT ( 'NONE',  ( 5.138538782746885580, -1.577291412575715812, 0.9494700402261007088 ) ) ;
#142732 = VERTEX_POINT ( 'NONE', #90694 ) ;
#142733 = CARTESIAN_POINT ( 'NONE',  ( 0.6801582343749674742, -0.4427083329919187515, -1.178068619123886718 ) ) ;
#142734 = CARTESIAN_POINT ( 'NONE',  ( -8.694856585065634746, 9.038420858865048757, 0.7998128361456462443 ) ) ;
#142735 = LINE ( 'NONE', #90771, #113830 ) ;
#142736 = CARTESIAN_POINT ( 'NONE',  ( 6.521762860236213655, -0.4636855090699961712, 2.076960040381255812 ) ) ;
#142737 = CARTESIAN_POINT ( 'NONE',  ( -2.324999999999999289, -0.05106627235655240848, -0.5000000000000004441 ) ) ;
#142738 = CARTESIAN_POINT ( 'NONE',  ( 4.039439701867726384, 6.800097854565950506, 1.199719254218462483 ) ) ;
#142740 = EDGE_CURVE ( 'NONE', #64117, #152385, #33924, .T. ) ;
#142739 =( GEOMETRIC_REPRESENTATION_CONTEXT ( 3 ) GLOBAL_UNCERTAINTY_ASSIGNED_CONTEXT ( ( #33203 ) ) GLOBAL_UNIT_ASSIGNED_CONTEXT ( ( #161297, #127823, #75775 ) ) REPRESENTATION_CONTEXT ( 'NONE', 'WORKASPACE' ) );
#142741 = CARTESIAN_POINT ( 'NONE',  ( 0.3036813079041804087, -0.5503025168475895734, 1.985974332091578809 ) ) ;
#142744 = CARTESIAN_POINT ( 'NONE',  ( 4.880324068823122197, -0.2306306682541107433, -1.826696389425507938 ) ) ;
#142743 = CARTESIAN_POINT ( 'NONE',  ( 2.066652149400012295, 1.381653119961171239, -1.247030302550973468 ) ) ;
#142742 = DIRECTION ( 'NONE',  ( 1.000000000000000000, -7.771561172376097755E-16, -4.440892098500627148E-16 ) ) ;
#142745 = CARTESIAN_POINT ( 'NONE',  ( 5.635385404774530649, 9.726366738878972740, 0.7998128361456462443 ) ) ;
#142746 = CARTESIAN_POINT ( 'NONE',  ( -9.383881589528572320, 14.59418599432876640, -7.387911200823596758 ) ) ;
#142747 = CARTESIAN_POINT ( 'NONE',  ( -5.498713818794216834, 8.572860667638675380, -1.199719254218452047 ) ) ;
#142749 = ORIENTED_EDGE ( 'NONE', *, *, #58125, .F. ) ;
#142748 = CARTESIAN_POINT ( 'NONE',  ( 0.000000000000000000, -1.600000000000000755, 0.000000000000000000 ) ) ;
#142750 = CARTESIAN_POINT ( 'NONE',  ( 4.459734715955371520, 0.4851516707722826061, -2.152740496749529608 ) ) ;
#142751 = CARTESIAN_POINT ( 'NONE',  ( 6.485631321617453260, 1.553040037441177690, 1.645414220380213788 ) ) ;
#142752 = CARTESIAN_POINT ( 'NONE',  ( -5.368665641331555882, 8.246898433986675769, 1.082531754730548412 ) ) ;
#142753 = CARTESIAN_POINT ( 'NONE',  ( 5.713115418873079498, 1.475880075617709730, -1.050242514106846992 ) ) ;
#142754 = CARTESIAN_POINT ( 'NONE',  ( 0.2160302486270138655, 1.032475520995678853, -1.731998313101141163 ) ) ;
#142755 = EDGE_CURVE ( 'NONE', #192824, #196589, #26256, .T. ) ;
#142756 = CARTESIAN_POINT ( 'NONE',  ( -4.636780943466218829, 5.307142521894840037, 1.176014350056652225 ) ) ;
#142757 = CARTESIAN_POINT ( 'NONE',  ( 9.175343923411263702, 14.33640814621786674, -7.734832872067204157 ) ) ;
#142758 = EDGE_CURVE ( 'NONE', #160077, #16835, #23008, .T. ) ;
#142759 = CARTESIAN_POINT ( 'NONE',  ( 5.268181577278353345, 1.909906527651853425, -0.09793718704654422180 ) ) ;
#142760 = SURFACE_STYLE_FILL_AREA ( #76644 ) ;
#142761 = CARTESIAN_POINT ( 'NONE',  ( 0.3560485870845608858, 0.7116971694140910021, 1.730184004908103867 ) ) ;
#142762 = CARTESIAN_POINT ( 'NONE',  ( 1.885954221117658092, -2.015980662343511032, 0.05432778586660082232 ) ) ;
#142764 = CARTESIAN_POINT ( 'NONE',  ( 4.301466803424673913, 1.691180239654224815, 1.254954771472403641 ) ) ;
#142763 = CARTESIAN_POINT ( 'NONE',  ( -8.666686507633592385, 11.13422023037111330, 1.599625672291269396 ) ) ;
#142765 = CARTESIAN_POINT ( 'NONE',  ( 8.178592977541601527, 10.56477777859713463, 1.599625672291281386 ) ) ;
#142767 = CARTESIAN_POINT ( 'NONE',  ( -8.850775351622791831, 9.220326086515070685, -0.7998128361456291469 ) ) ;
#142766 = CARTESIAN_POINT ( 'NONE',  ( -1.402160292154681736E-14, -0.6624999999999758860, -1.732050807568870754 ) ) ;
#142768 = CARTESIAN_POINT ( 'NONE',  ( 0.000000000000000000, 2.000000000000001776, 0.000000000000000000 ) ) ;
#142769 = CARTESIAN_POINT ( 'NONE',  ( 3.252217677095782911, 0.9042450522839510230, -1.806111763424333105 ) ) ;
#142770 = CARTESIAN_POINT ( 'NONE',  ( -1.364683531249997417, 3.509375000341423245, 1.214306433183764966E-14 ) ) ;
#142771 = CARTESIAN_POINT ( 'NONE',  ( 9.083599731475976213, 12.58098820582193689, 1.082531754730546636 ) ) ;
#142772 = CARTESIAN_POINT ( 'NONE',  ( 3.936934155531632396, 0.3128429973590241553, 2.138701728237289768 ) ) ;
#142773 = CARTESIAN_POINT ( 'NONE',  ( 6.933015448541703485, 9.181880338089085214, 1.599625672291268286 ) ) ;
#142774 = CARTESIAN_POINT ( 'NONE',  ( 1.499999999999990896, 5.025000000000022560, 1.214306433183764966E-14 ) ) ;
#142776 =( NAMED_UNIT ( * ) PLANE_ANGLE_UNIT ( ) SI_UNIT ( $, .RADIAN. ) );
#142775 = CARTESIAN_POINT ( 'NONE',  ( 5.833751235630055376, 10.02806988486892514, 0.7998128361456331437 ) ) ;
#142777 = CARTESIAN_POINT ( 'NONE',  ( 7.904040366642689719, 10.24446639921506552, 1.443375672974076540 ) ) ;
#142779 = CARTESIAN_POINT ( 'NONE',  ( 9.327139308102928794, 13.85903420602375036, -7.550757598840666773 ) ) ;
#142778 = CARTESIAN_POINT ( 'NONE',  ( 1.645237833728605548, -0.3177867502775574837, -2.147667186158049191 ) ) ;
#142781 = CARTESIAN_POINT ( 'NONE',  ( 0.4679805871025365382, -1.733519288248483559, -0.6209854868195128219 ) ) ;
#142780 = CARTESIAN_POINT ( 'NONE',  ( -7.402388683381436074, 7.738467673474211495, 0.7216878364870317197 ) ) ;
#142782 = B_SPLINE_CURVE_WITH_KNOTS ( 'NONE', 3,
 ( #185385, #40224, #107415, #203753 ),
 .UNSPECIFIED., .F., .F.,
 ( 4, 4 ),
 ( 0.000000000000000000, 0.0003389024754017963548 ),
 .UNSPECIFIED. ) ;
#142783 = CARTESIAN_POINT ( 'NONE',  ( 1.364683531249988535, 2.613541667008089764, 0.7879004041258500513 ) ) ;
#142784 = CARTESIAN_POINT ( 'NONE',  ( 2.191216702865448784, 1.696344223602393786, 1.387594652289561248 ) ) ;
#142785 = DIRECTION ( 'NONE',  ( 0.000000000000000000, 8.546850786086437571E-32, 1.000000000000000000 ) ) ;
#142786 = CARTESIAN_POINT ( 'NONE',  ( 2.413256113406063275, 2.020865564879420262, 1.017551375885389131 ) ) ;
#142787 = CARTESIAN_POINT ( 'NONE',  ( -7.043624497499477499, 8.176315654292865887, 1.199719254218450271 ) ) ;
#142788 = CARTESIAN_POINT ( 'NONE',  ( -1.201851678989727383E-14, 4.259375000341417028, -1.575800808251660134 ) ) ;
#142789 = CARTESIAN_POINT ( 'NONE',  ( 5.582388601459258304, 7.396495182493852738, 1.242574333668546638 ) ) ;
#142790 = CARTESIAN_POINT ( 'NONE',  ( 0.7500000000000006661, 12.83333333333333570, 1.299038105676657340 ) ) ;
#142791 = CARTESIAN_POINT ( 'NONE',  ( 5.994113311017540191, 9.046863725278862844, -1.082531754730548412 ) ) ;
#142792 = CARTESIAN_POINT ( 'NONE',  ( 4.129968326689526847, 0.9481555284369269643, -1.494110371635357648 ) ) ;
#142793 = AXIS2_PLACEMENT_3D ( 'NONE', #3245, #68250, #202515 ) ;
#142794 = CARTESIAN_POINT ( 'NONE',  ( 8.289920859751990889, 11.75899253876431416, 1.199719254218450271 ) ) ;
#142795 = CARTESIAN_POINT ( 'NONE',  ( 1.079290920250153496, -0.05147710300976635067, -2.105495365820194920 ) ) ;
#142796 = PRESENTATION_LAYER_ASSIGNMENT (  '', '', ( #87406 ) ) ;
#142798 = CARTESIAN_POINT ( 'NONE',  ( -1.402160292154681736E-14, 0.8375000000000232259, -1.732050807568863648 ) ) ;
#142797 = CARTESIAN_POINT ( 'NONE',  ( 0.6823417656249934904, 10.94270833367473550, 1.181850606188764807 ) ) ;
#142799 = CARTESIAN_POINT ( 'NONE',  ( -4.447956913735107598, 7.346977611736363656, 1.199719254218452935 ) ) ;
#142800 = CARTESIAN_POINT ( 'NONE',  ( 6.609000000000038177, 0.002801690667396730672, 2.000160786441218530 ) ) ;
#142802 = ORIENTED_EDGE ( 'NONE', *, *, #140986, .T. ) ;
#142801 = CARTESIAN_POINT ( 'NONE',  ( 5.097853226644959435, 1.222535334948423813, 1.337041937662573288 ) ) ;
#142803 = CARTESIAN_POINT ( 'NONE',  ( 3.379631771358857950, 1.185797501207178861, 1.446808710765794315 ) ) ;
#142804 = CARTESIAN_POINT ( 'NONE',  ( 3.924723049676182018, -1.394041313093749457, 1.530695986988836799 ) ) ;
#142805 = SHAPE_REPRESENTATION ( 'isolation 510', ( #200407 ), #13801 ) ;
#142806 = CARTESIAN_POINT ( 'NONE',  ( -5.275531169048901958, 8.208517892982092334, -1.082531754730549967 ) ) ;
#142807 = CARTESIAN_POINT ( 'NONE',  ( -1.115562610750309283E-14, 10.84375000068279604, 1.500000000000001554 ) ) ;
#142808 = CARTESIAN_POINT ( 'NONE',  ( -1.500511526392867001, 8.643217832945683909, 2.569261818345993653 ) ) ;
#142809 = CARTESIAN_POINT ( 'NONE',  ( 6.994027139803230320, 9.253060644560830994, -1.599625672291267398 ) ) ;
#142810 = FACE_BOUND ( 'NONE', #48835, .T. ) ;
#142811 = CARTESIAN_POINT ( 'NONE',  ( 0.6823417656249899377, 5.238541667008086655, -1.181850606188754593 ) ) ;
#142812 = CARTESIAN_POINT ( 'NONE',  ( 3.736726379466179804, -1.890069333072645241, -0.5255722985574098338 ) ) ;
#142813 = CARTESIAN_POINT ( 'NONE',  ( 1.282577132041575529, -1.967586879516727061, 0.4389604359977539172 ) ) ;
#142814 = ADVANCED_FACE ( 'NONE', ( #193505 ), #77615, .T. ) ;
#142815 = CARTESIAN_POINT ( 'NONE',  ( -5.320648938720212051, 5.172121614787156929, 0.000000000000000000 ) ) ;
#142816 = CARTESIAN_POINT ( 'NONE',  ( 6.639320575229252341, 0.005161017367553630275, 1.896863882003448021 ) ) ;
#142817 = CARTESIAN_POINT ( 'NONE',  ( 1.334983872447586872, -1.693447605269988276, 0.7947349781701130711 ) ) ;
#142818 = CARTESIAN_POINT ( 'NONE',  ( 1.364683531249990311, 4.384375000341417028, 1.214306433183764966E-14 ) ) ;
#142819 = CARTESIAN_POINT ( 'NONE',  ( 3.076434440837049866, 0.9091080936043660632, 1.796352098325330715 ) ) ;
#142821 = CARTESIAN_POINT ( 'NONE',  ( 2.917688350237046979, -1.423917071783699972, -1.567024636986138253 ) ) ;
#142820 = CARTESIAN_POINT ( 'NONE',  ( -4.907688418466881863, 8.669460888279271416, 0.7216878364870458196 ) ) ;
#142822 = CARTESIAN_POINT ( 'NONE',  ( 3.562760505341037831, 7.378580699531681830, -1.734723475976807094E-15 ) ) ;
#142823 = CARTESIAN_POINT ( 'NONE',  ( 5.301260566756325510, -1.777534899005998481, 1.061244097098137606 ) ) ;
#142824 = CARTESIAN_POINT ( 'NONE',  ( 7.289443866002793371, 8.533381260871966134, 1.199719254218452047 ) ) ;
#142826 = CARTESIAN_POINT ( 'NONE',  ( 4.390142812726693045, 4.016254791136236513, 1.214306433183764966E-14 ) ) ;
#142825 = CARTESIAN_POINT ( 'NONE',  ( -0.02372336622697389028, -2.029015295047017720, -0.5039539365503820090 ) ) ;
#142828 = ORIENTED_EDGE ( 'NONE', *, *, #53727, .T. ) ;
#142827 = CARTESIAN_POINT ( 'NONE',  ( 4.981388616008130654, 1.702979688329594676, -0.6582044668519275721 ) ) ;
#142829 = CARTESIAN_POINT ( 'NONE',  ( 9.101601193475611140, 9.512956235343358102, -0.7998128361456221525 ) ) ;
#142830 = CARTESIAN_POINT ( 'NONE',  ( 3.325722479477188021, 7.699077257575913436, -2.500000000000104361 ) ) ;
#142832 = CIRCLE ( 'NONE', #28699, 11.92000000000000171 ) ;
#142831 = CARTESIAN_POINT ( 'NONE',  ( 11.25027063990047616, 9.330753595378251219, 3.765175919509110791 ) ) ;
#142833 = CARTESIAN_POINT ( 'NONE',  ( -10.39320420135713263, 4.932286138528427344, 5.331284845095887626 ) ) ;
#142834 = CARTESIAN_POINT ( 'NONE',  ( 1.364683531249997417, 11.54687500034139802, 2.602085213965210642E-15 ) ) ;
#142835 = CARTESIAN_POINT ( 'NONE',  ( 5.233030847706650057, 1.768443763404730307, 0.7281017474275592871 ) ) ;
#142836 = CARTESIAN_POINT ( 'NONE',  ( -7.458957065812611198, 11.85386701009007204, 0.7998128361456481317 ) ) ;
#142837 = CARTESIAN_POINT ( 'NONE',  ( 6.602984505055297326, 7.662235663108029726, 1.199719254218462483 ) ) ;
#142838 = CARTESIAN_POINT ( 'NONE',  ( -1.360316468750006669, 2.442708333674733723, 0.7853790794158861388 ) ) ;
#142839 = CARTESIAN_POINT ( 'NONE',  ( 9.499668754586233277, -7.643695121331843367, 0.07933191752450531598 ) ) ;
#142840 = CARTESIAN_POINT ( 'NONE',  ( 5.118366684358879759, 5.930181538962194132, 1.199719254218462483 ) ) ;
#142841 = ORIENTED_EDGE ( 'NONE', *, *, #177464, .T. ) ;
#142842 = CARTESIAN_POINT ( 'NONE',  ( -7.611976899429754084, 7.845337568948314022, 0.7998128361456341429 ) ) ;
#142843 = CARTESIAN_POINT ( 'NONE',  ( 10.99934730582667797, -5.294005300192715424, -0.1376907581457621488 ) ) ;
#142845 = CARTESIAN_POINT ( 'NONE',  ( 6.343235766347262938, 8.493804042195527870, -1.599625672291281386 ) ) ;
#142844 = DIRECTION ( 'NONE',  ( 0.7071067811865489050, 0.000000000000000000, 0.7071067811865462405 ) ) ;
#142846 = B_SPLINE_CURVE_WITH_KNOTS ( 'NONE', 3,
 ( #122361, #6355, #72425, #23682, #155838, #107144 ),
 .UNSPECIFIED., .F., .F.,
 ( 4, 2, 4 ),
 ( 0.000000000000000000, 0.0003845013059668469482, 0.0007690026119336938965 ),
 .UNSPECIFIED. ) ;
#142847 = AXIS2_PLACEMENT_3D ( 'NONE', #124569, #10712, #110432 ) ;
#142848 = CARTESIAN_POINT ( 'NONE',  ( -6.489499031467138579, 6.765560312407735033, -0.1891594744549245088 ) ) ;
#142849 = CARTESIAN_POINT ( 'NONE',  ( -6.561783159334141580, 7.718130443053708767, -1.082531754730544860 ) ) ;
#142850 = CARTESIAN_POINT ( 'NONE',  ( 2.849184837166184536, 6.475799410002530898, 0.7998128361456362523 ) ) ;
#142851 = CARTESIAN_POINT ( 'NONE',  ( 1.867950311876313219, -1.955179860842346296, 0.2357939167430597172 ) ) ;
#142852 = CARTESIAN_POINT ( 'NONE',  ( 3.497672881252233967, -1.986097994744703721, 0.3474890017408845955 ) ) ;
#142853 = CARTESIAN_POINT ( 'NONE',  ( -6.509886312855995172, 10.74661779830734254, -0.7998128361456291469 ) ) ;
#142854 = CARTESIAN_POINT ( 'NONE',  ( 4.518610335104485287, 8.493738834255713854, 0.000000000000000000 ) ) ;
#142856 = ADVANCED_FACE ( 'NONE', ( #159940, #12603 ), #31021, .T. ) ;
#142855 = CARTESIAN_POINT ( 'NONE',  ( 6.827182134110231004, 7.052068023338082803, 2.687205202894725975 ) ) ;
#142857 = CARTESIAN_POINT ( 'NONE',  ( 3.714928722721734911, -0.1615716889580356697, 2.185543052782303874 ) ) ;
#142858 = CARTESIAN_POINT ( 'NONE',  ( 9.333039360705550180, 4.446953957879813402, -7.472411811099956225 ) ) ;
#142859 = CARTESIAN_POINT ( 'NONE',  ( 2.573164103464478991, 0.09656903795818297387, -1.924097065980167942 ) ) ;
#142860 = CARTESIAN_POINT ( 'NONE',  ( -7.160677686311960777, 11.50587440067263678, -0.7998128361456291469 ) ) ;
#142861 = CARTESIAN_POINT ( 'NONE',  ( 1.230761180058548954, 3.060133534840178360, 0.7750000000000100142 ) ) ;
#142862 = CARTESIAN_POINT ( 'NONE',  ( 0.2333540202161610289, 4.089650199633740435, -2.600675808310505044 ) ) ;
#142863 = EDGE_CURVE ( 'NONE', #25107, #2091, #147521, .T. ) ;
#142864 = CARTESIAN_POINT ( 'NONE',  ( 4.177320726786311056, 5.966903162707725805, -1.443375672974068769 ) ) ;
#142865 = CARTESIAN_POINT ( 'NONE',  ( 7.690499447449630210, 9.995335326823163058, 1.599625672291281386 ) ) ;
#142866 = AXIS2_PLACEMENT_3D ( 'NONE', #209183, #60823, #37920 ) ;
#142867 = CARTESIAN_POINT ( 'NONE',  ( 5.660692828905515839, 6.562895374266609849, -1.199719254218445830 ) ) ;
#142868 = CARTESIAN_POINT ( 'NONE',  ( 6.563555762791525972, 6.830105609444471426, -0.7216878364870458196 ) ) ;
#142869 = ORIENTED_EDGE ( 'NONE', *, *, #41407, .T. ) ;
#142871 = CARTESIAN_POINT ( 'NONE',  ( 3.229155175764964802, 1.820814436659716096, 0.8588418517583608081 ) ) ;
#142870 = CARTESIAN_POINT ( 'NONE',  ( 5.812015183962491172, 1.231757822100377320, -1.368757117762291253 ) ) ;
#142872 = CARTESIAN_POINT ( 'NONE',  ( 4.763194794223141848, -2.297684049645591919, -0.06285783202429616467 ) ) ;
#142874 = CARTESIAN_POINT ( 'NONE',  ( 1.885388715806934679, -1.754394424870173719, 0.6211283009984622794 ) ) ;
#142873 = CARTESIAN_POINT ( 'NONE',  ( -0.02900071798683095947, 5.719935618195115978, -2.767867108847458901 ) ) ;
#142875 = CARTESIAN_POINT ( 'NONE',  ( -1.642778471874998480, -1.101041666188708801, 2.845375778867863303 ) ) ;
#142876 = CARTESIAN_POINT ( 'NONE',  ( 0.000000000000000000, 0.000000000000000000, 0.000000000000000000 ) ) ;
#142877 = CARTESIAN_POINT ( 'NONE',  ( 10.23541933785883806, 1.000000000000000888, 6.134053304049035482 ) ) ;
#142878 = CARTESIAN_POINT ( 'NONE',  ( -6.496328159242330536, 10.73079995242472862, 0.000000000000000000 ) ) ;
#142879 = CARTESIAN_POINT ( 'NONE',  ( -4.800995793014949165, 8.615262501910491366, 0.7216878364870267237 ) ) ;
#142881 = CARTESIAN_POINT ( 'NONE',  ( 3.783945140921864070, -0.9226758061156097313, 1.627204332209288395 ) ) ;
#142880 = CARTESIAN_POINT ( 'NONE',  ( 5.179275120254928311, 1.405169897584326089, 1.548284651509527210 ) ) ;
#142882 = CARTESIAN_POINT ( 'NONE',  ( 5.504247177468168495, 9.365446107114122398, 0.7216878364870438212 ) ) ;
#142883 = ORIENTED_EDGE ( 'NONE', *, *, #164010, .F. ) ;
#142884 = VECTOR ( 'NONE', #83222, 1000.000000000000000 ) ;
#142885 = DIRECTION ( 'NONE',  ( 0.000000000000000000, 0.000000000000000000, 1.000000000000000000 ) ) ;
#142886 = CARTESIAN_POINT ( 'NONE',  ( 0.3610206255357477079, -7.699789852011537761, -10.99434576733086111 ) ) ;
#142887 = CARTESIAN_POINT ( 'NONE',  ( 6.498688201949993193, -0.4681372660274349951, -1.660085793416385513 ) ) ;
#142888 = CARTESIAN_POINT ( 'NONE',  ( -6.358937740009323214, 7.377514437221045718, -1.199719254218446718 ) ) ;
#142889 =( BOUNDED_CURVE ( )  B_SPLINE_CURVE ( 3, ( #57838, #73003, #74097, #156419 ),
 .UNSPECIFIED., .F., .T. ) 
 B_SPLINE_CURVE_WITH_KNOTS ( ( 4, 4 ),
 ( 1.570796326794897002, 2.200856270465477937 ),
 .UNSPECIFIED. ) 
 CURVE ( )  GEOMETRIC_REPRESENTATION_ITEM ( )  RATIONAL_B_SPLINE_CURVE ( ( 1.000000000000000000, 0.9671913951458355196, 0.9671913951458355196, 1.000000000000000000 ) ) 
 REPRESENTATION_ITEM ( '' )  );
#142890 = CARTESIAN_POINT ( 'NONE',  ( 1.758077109659747395, 1.659224110165247179, -0.5040892880595440051 ) ) ;
#142891 = FACE_OUTER_BOUND ( 'NONE', #165031, .T. ) ;
#142892 = DIRECTION ( 'NONE',  ( -8.638326563840814399E-31, 0.000000000000000000, -1.000000000000000000 ) ) ;
#142893 = CARTESIAN_POINT ( 'NONE',  ( 0.3999999999999758193, 2.999999999999999112, 2.420000000000000373 ) ) ;
#142894 = CARTESIAN_POINT ( 'NONE',  ( 5.875877563635198975, -2.119900239643329964, 0.4680052475878637708 ) ) ;
#142895 = CARTESIAN_POINT ( 'NONE',  ( 4.477060521952030747, -0.002618581577289170060, -1.825872481161804561 ) ) ;
#142896 = CARTESIAN_POINT ( 'NONE',  ( 2.641395077882052966, 1.795597516233004232, -0.7905247784146393064 ) ) ;
#142897 = CARTESIAN_POINT ( 'NONE',  ( 6.368375629516933145, -2.076896536817146810, -0.4110353314962181259 ) ) ;
#142898 = CARTESIAN_POINT ( 'NONE',  ( -9.480175724453545172, 12.08329098332774265, 1.599625672291281386 ) ) ;
#142899 = CARTESIAN_POINT ( 'NONE',  ( 7.076466111328892694, 10.34329533227067799, -1.199719254218441611 ) ) ;
#142900 = CARTESIAN_POINT ( 'NONE',  ( 2.965608807194367813, -1.734805745614193873, -1.219131234129526398 ) ) ;
#142901 = CARTESIAN_POINT ( 'NONE',  ( -2.765500147507697459, 5.209872024525476597, 1.082531754730560403 ) ) ;
#142902 = CARTESIAN_POINT ( 'NONE',  ( 0.000000000000000000, 15.00000000000000000, 0.000000000000000000 ) ) ;
#142903 = EDGE_CURVE ( 'NONE', #43199, #40760, #206238, .T. ) ;
#142904 = CARTESIAN_POINT ( 'NONE',  ( -5.565591498217608013, 6.214750235347503704, -0.9194985501971261188 ) ) ;
#142905 = CARTESIAN_POINT ( 'NONE',  ( 0.2861044793709514589, -1.271156181823060560, -1.634742764404630844 ) ) ;
#142907 = CARTESIAN_POINT ( 'NONE',  ( -1.500000000000001110, 14.30208333401613530, 0.8660254037844419273 ) ) ;
#142906 = CARTESIAN_POINT ( 'NONE',  ( -10.72721294398669123, 4.499566226064992236, 5.280202143233098333 ) ) ;
#142909 = VERTEX_POINT ( 'NONE', #192418 ) ;
#142908 = CARTESIAN_POINT ( 'NONE',  ( 3.844553043330910747, 1.187701353711614338, -1.876932147738763268 ) ) ;
#142910 = CARTESIAN_POINT ( 'NONE',  ( 1.090962482291182312, -0.5517420707249369727, 2.231415953587682299 ) ) ;
#142912 = CARTESIAN_POINT ( 'NONE',  ( 0.2507196182260813533, -0.4238382354822354259, -1.922440920834954436 ) ) ;
#142911 = CARTESIAN_POINT ( 'NONE',  ( 4.546061579283848353, 4.198160018786257552, -0.7998128361456211532 ) ) ;
#142914 = CARTESIAN_POINT ( 'NONE',  ( -1.737500000000000266, -2.858333333333334281, -3.009438278150923907 ) ) ;
#142913 = CARTESIAN_POINT ( 'NONE',  ( 4.228163802615382494, 6.026220084508304708, -1.599625672291269396 ) ) ;
#142915 = CARTESIAN_POINT ( 'NONE',  ( 0.1333542156527295908, 7.629137130509112907, -2.645925523406994717 ) ) ;
#142916 = CARTESIAN_POINT ( 'NONE',  ( 6.022987620897008121, -1.731432113864934674, 0.6267441317700100933 ) ) ;
#142917 = CARTESIAN_POINT ( 'NONE',  ( -5.669981010301158086, 6.148093781360158161, -0.7892279793065083426 ) ) ;
#142918 = CARTESIAN_POINT ( 'NONE',  ( -0.2104748580754166321, -0.006608320950486632102, -2.103482951484026309 ) ) ;
#142919 = CARTESIAN_POINT ( 'NONE',  ( 2.889346415704593607, 1.218289440699829473, 1.221169829160633435 ) ) ;
#142920 = CARTESIAN_POINT ( 'NONE',  ( 1.235564962061060035, 0.5807501988173838781, -1.931125984888550695 ) ) ;
#142921 = CARTESIAN_POINT ( 'NONE',  ( 3.147439182535469726, 1.035885224147353512, 2.052142740569740109 ) ) ;
#142922 = CARTESIAN_POINT ( 'NONE',  ( 2.566018446761752170, 2.219231934913689308, -0.4390887803658559130 ) ) ;
#142923 = CARTESIAN_POINT ( 'NONE',  ( 5.777981411418616098, 1.253425007971820326, 1.692306578934036798 ) ) ;
#142924 = CARTESIAN_POINT ( 'NONE',  ( -7.105881907338178038, 7.462819444748888920, -0.7216878364870338292 ) ) ;
#142925 = CARTESIAN_POINT ( 'NONE',  ( 3.198275679207917666, -0.5104862868050319413, -1.694526722652128781 ) ) ;
#142927 = CARTESIAN_POINT ( 'NONE',  ( 6.093372230586791893, -0.7761969640797984349, 2.157113249652943932 ) ) ;
#142926 = CARTESIAN_POINT ( 'NONE',  ( 3.051993976407674225, 6.574760382535328240, -0.7216878364870338292 ) ) ;
#142928 = CARTESIAN_POINT ( 'NONE',  ( 4.400242069895500485, 1.421654421768648868, -1.169904355399861595 ) ) ;
#142929 = CARTESIAN_POINT ( 'NONE',  ( -3.927058049452637700, 7.733318157670055371, -0.7998128361456281477 ) ) ;
#142930 = CARTESIAN_POINT ( 'NONE',  ( 6.290620086616457662, 6.441404310581745563, 1.040834085586084257E-14 ) ) ;
#142931 = CARTESIAN_POINT ( 'NONE',  ( -0.7499999999999972244, 4.108333333333360038, -1.299038105676652011 ) ) ;
#142932 = CARTESIAN_POINT ( 'NONE',  ( 4.277398745584213735, 1.430588233724191083, 1.660156109410643177 ) ) ;
#142933 = CARTESIAN_POINT ( 'NONE',  ( -3.924195396151603177, 6.665646164563756138, 1.199719254218464037 ) ) ;
#142934 = CARTESIAN_POINT ( 'NONE',  ( 0.4491468415840123019, 7.944909564338990648, -1.993991491228294777 ) ) ;
#142935 = CARTESIAN_POINT ( 'NONE',  ( 5.283670394142272464, -1.967056725255760474, 0.6460906113585006549 ) ) ;
#142936 = CARTESIAN_POINT ( 'NONE',  ( 0.2160302486270138655, 1.032475520995678853, -1.731998313101141163 ) ) ;
#142937 = VECTOR ( 'NONE', #166629, 1000.000000000000000 ) ;
#142938 = CARTESIAN_POINT ( 'NONE',  ( -1.364683531250012516, 4.738541667008091096, -0.7879004041258300672 ) ) ;
#142939 = CARTESIAN_POINT ( 'NONE',  ( 3.387250987759330645, 1.741285041988534621, -0.8245012487104221854 ) ) ;
#142940 = CARTESIAN_POINT ( 'NONE',  ( -1.364683531250010295, 9.380208333674735499, 0.7879004041258445001 ) ) ;
#142941 = DIRECTION ( 'NONE',  ( -0.000000000000000000, -1.000000000000000000, -0.000000000000000000 ) ) ;
#142942 = CARTESIAN_POINT ( 'NONE',  ( 0.5279477311770188752, -0.3182371573221299266, 2.198381937975202760 ) ) ;
#142943 = ORIENTED_EDGE ( 'NONE', *, *, #91910, .T. ) ;
#142946 = VECTOR ( 'NONE', #114890, 1000.000000000000000 ) ;
#142945 = CARTESIAN_POINT ( 'NONE',  ( -0.4294077647110545737, -6.532648833121157850, -9.469892045836658667 ) ) ;
#142944 = CARTESIAN_POINT ( 'NONE',  ( -4.014622883422336308, 5.777089012116397804, -1.443375672974066548 ) ) ;
#142947 = CARTESIAN_POINT ( 'NONE',  ( 3.408985558832261731, 6.064568021024562938, 1.199719254218462483 ) ) ;
#142948 = SURFACE_STYLE_FILL_AREA ( #24875 ) ;
#142949 = DIRECTION ( 'NONE',  ( 1.953992523340275511E-14, 0.000000000000000000, -1.000000000000000000 ) ) ;
#142950 = CARTESIAN_POINT ( 'NONE',  ( 4.894543267554960053, 4.887125941896303338, -0.6895117023006970269 ) ) ;
#142951 = CARTESIAN_POINT ( 'NONE',  ( 4.207107738942202246, 3.802713871720993399, 1.214306433183764966E-14 ) ) ;
#142952 = CARTESIAN_POINT ( 'NONE',  ( 1.152704166800899932, -0.4732522875653189520, -1.903817266927515961 ) ) ;
#142953 = CARTESIAN_POINT ( 'NONE',  ( -1.364683531250012516, 0.8427083336747532849, 0.7879004041258379498 ) ) ;
#142954 = DIRECTION ( 'NONE',  ( 6.314299915563594049E-62, 8.546850786086437571E-32, 1.000000000000000000 ) ) ;
#142955 = CARTESIAN_POINT ( 'NONE',  ( 5.775826483351648832, -1.914393393812302113, 0.4282712878391075062 ) ) ;
#142956 = CARTESIAN_POINT ( 'NONE',  ( -10.48453286206953727, 11.12637651536962125, 0.7998128361456462443 ) ) ;
#142957 = CARTESIAN_POINT ( 'NONE',  ( -6.195713011320804320, 7.291048603704809672, -1.082531754730543083 ) ) ;
#142958 = CARTESIAN_POINT ( 'NONE',  ( 6.139563164240942506, -1.562336469324271837, -1.494251390645913613 ) ) ;
#142960 = EDGE_LOOP ( 'NONE', ( #150233, #57029, #133431, #157777 ) ) ;
#142959 = CARTESIAN_POINT ( 'NONE',  ( -8.902524791715885399, 3.162178953954597471, -7.495381307383191860 ) ) ;
#142961 = CARTESIAN_POINT ( 'NONE',  ( -1.364683531250010295, 4.530208333674754506, 0.7879004041258379498 ) ) ;
#142962 = CARTESIAN_POINT ( 'NONE',  ( 0.1747926744264660381, 0.006858446013176254172, -1.855468577918440776 ) ) ;
#142963 = CARTESIAN_POINT ( 'NONE',  ( 6.292339289836506033, -1.631180892843343999, 0.5882027141154468897 ) ) ;
#142965 = CARTESIAN_POINT ( 'NONE',  ( 2.665787806004877414, 1.174844384069907655, 1.849873475113596566 ) ) ;
#142964 = CARTESIAN_POINT ( 'NONE',  ( 1.360316468750000896, 0.7656250003413994643, 0.000000000000000000 ) ) ;
#142966 = CARTESIAN_POINT ( 'NONE',  ( 4.700386263483860461, -2.306923794945021200, -0.06181454844297362694 ) ) ;
#142967 = CARTESIAN_POINT ( 'NONE',  ( 5.448532837019475217, 0.5942636223626071024, 1.973259177745954718 ) ) ;
#142968 = CARTESIAN_POINT ( 'NONE',  ( 1.095531938664672911, -1.942124713061957220, -0.0005026242578913541230 ) ) ;
#142969 = CARTESIAN_POINT ( 'NONE',  ( -4.867013957181525186, 8.622007350113015889, 0.7216878364870458196 ) ) ;
#142970 = CARTESIAN_POINT ( 'NONE',  ( 11.84668730067608244, 11.00636224908217287, 1.399999999999998357 ) ) ;
#142971 = CARTESIAN_POINT ( 'NONE',  ( 4.711248855110969913, 1.761570823303935551, -1.180294879073326308 ) ) ;
#142972 = FILL_AREA_STYLE_COLOUR ( '', #32781 ) ;
#142973 = CARTESIAN_POINT ( 'NONE',  ( 2.549454116737331244, -1.388485404012842261, 1.462446031800922253 ) ) ;
#142974 = CARTESIAN_POINT ( 'NONE',  ( -5.572037945092175981, 5.603058478803387032, 0.7216878364870317197 ) ) ;
#142975 = CARTESIAN_POINT ( 'NONE',  ( 5.544034191846948900, 0.8990280053539388971, -2.015528879820461583 ) ) ;
#142976 = CARTESIAN_POINT ( 'NONE',  ( -6.420668264523499147, 9.648474187656182366, 1.199719254218452935 ) ) ;
#142977 = CARTESIAN_POINT ( 'NONE',  ( -9.568546172724161636, -8.233137084989836652, 0.4683205530892458057 ) ) ;
#142978 = CARTESIAN_POINT ( 'NONE',  ( 0.2053145577999641036, -0.4904175937916722128, 1.758528939493007481 ) ) ;
#142979 = CARTESIAN_POINT ( 'NONE',  ( -6.343235766347277149, 8.493804042195527870, -1.599625672291271394 ) ) ;
#142981 = CARTESIAN_POINT ( 'NONE',  ( 6.639320575229282539, 7.629137130509070275, 2.703262396134015866 ) ) ;
#142980 = CARTESIAN_POINT ( 'NONE',  ( -4.758546912290684716, 8.291040531757728260, 0.8107885835855069834 ) ) ;
#142982 = CARTESIAN_POINT ( 'NONE',  ( 1.467638673046481657, 8.739153922842808342, -2.544768421592523033 ) ) ;
#142983 = ORIENTED_EDGE ( 'NONE', *, *, #140681, .T. ) ;
#142984 = CARTESIAN_POINT ( 'NONE',  ( 5.243067039532245843, -1.768777590322716309, 1.057421601032474623 ) ) ;
#142985 = CARTESIAN_POINT ( 'NONE',  ( 1.360316468749997565, 2.744791667008062763, 0.7853790794158921340 ) ) ;
#142986 = CARTESIAN_POINT ( 'NONE',  ( 0.000000000000000000, 0.9000000000000014655, 0.000000000000000000 ) ) ;
#142987 = CARTESIAN_POINT ( 'NONE',  ( -3.684065054611367351, 5.321161868511784299, -1.599625672291256295 ) ) ;
#142988 = CARTESIAN_POINT ( 'NONE',  ( -5.029148636026397945, 4.832037928311032182, 0.7998128361456281477 ) ) ;
#142989 = CARTESIAN_POINT ( 'NONE',  ( 4.740881522827352867, 1.933304458870839238, 0.5843455605825734755 ) ) ;
#142991 = ORIENTED_EDGE ( 'NONE', *, *, #26695, .F. ) ;
#142990 = CARTESIAN_POINT ( 'NONE',  ( -1.402160292154681736E-14, 0.2125000000000202283, 1.732050807568877637 ) ) ;
#142993 = CARTESIAN_POINT ( 'NONE',  ( 8.595506201384008449, 11.05117653974661529, 1.443375672974076540 ) ) ;
#142992 = CARTESIAN_POINT ( 'NONE',  ( -5.330290668828105538, 6.247702530834755130, 1.199719254218452935 ) ) ;
#142994 = CIRCLE ( 'NONE', #94585, 2.011244508837062295 ) ;
#142995 = CARTESIAN_POINT ( 'NONE',  ( 7.481401836642521452, 7.622723652371411696, 1.040834085586084257E-14 ) ) ;
#142996 = CARTESIAN_POINT ( 'NONE',  ( 4.241127833599818153, -1.794087422336073878, 1.013995622381487216 ) ) ;
#142997 = CARTESIAN_POINT ( 'NONE',  ( 2.408827471728996361, -1.163269702728772392, -1.646838680093346996 ) ) ;
#142998 = VERTEX_POINT ( 'NONE', #210808 ) ;
#142999 = DIRECTION ( 'NONE',  ( 1.000000000000000000, -5.578564026256504688E-16, 0.000000000000000000 ) ) ;
#143000 = CARTESIAN_POINT ( 'NONE',  ( 5.217190183160311356, 4.981143389975473568, -0.7998128361456211532 ) ) ;
#143002 = ORIENTED_EDGE ( 'NONE', *, *, #88639, .T. ) ;
#143001 = CARTESIAN_POINT ( 'NONE',  ( -3.096514578442687515, 6.188910745953249304, -0.7944190528704382359 ) ) ;
#143003 = CARTESIAN_POINT ( 'NONE',  ( 3.356795910091507906, -0.8196482158769199389, 1.842165019812888271 ) ) ;
#143004 = CARTESIAN_POINT ( 'NONE',  ( 2.431387202150552707, 0.8680758514147070004, -1.623638265414374171 ) ) ;
#143005 = CARTESIAN_POINT ( 'NONE',  ( 1.278406981455294744, 1.378070038918308038, 1.850917983980376658 ) ) ;
#143006 = CARTESIAN_POINT ( 'NONE',  ( 5.411639590510088027, 6.342609606130419131, -1.199719254218452047 ) ) ;
#143007 = CARTESIAN_POINT ( 'NONE',  ( 2.073706595668877384, 2.069181010895416950, -0.6253580070983978390 ) ) ;
#143008 = CARTESIAN_POINT ( 'NONE',  ( -6.684333426737305572, 7.757142738403693727, -1.199719254218446718 ) ) ;
#143009 = EDGE_CURVE ( 'NONE', #96770, #22085, #54112, .T. ) ;
#143010 = CARTESIAN_POINT ( 'NONE',  ( 2.864987100074483539, -0.7226686165877260759, 2.181857903572166801 ) ) ;
#143011 = ORIENTED_EDGE ( 'NONE', *, *, #99066, .T. ) ;
#143012 = CARTESIAN_POINT ( 'NONE',  ( -10.62873463776380056, 12.30000000000000071, -3.200000000000001510 ) ) ;
#143013 = AXIS2_PLACEMENT_3D ( 'NONE', #203956, #207180, #175772 ) ;
#143014 = CARTESIAN_POINT ( 'NONE',  ( 1.692057038649401601, -1.861345348035767344, -0.1864469194169729449 ) ) ;
#143015 = STYLED_ITEM ( 'NONE', ( #23309 ), #113029 ) ;
#143016 = CARTESIAN_POINT ( 'NONE',  ( 5.436387729582301098, 1.942169232299725046, 0.3377773032272758380 ) ) ;
#143018 = CARTESIAN_POINT ( 'NONE',  ( 9.395437264145964917, 10.06369101769952934, -0.7216878364870257245 ) ) ;
#143017 = CARTESIAN_POINT ( 'NONE',  ( -1.201851678989727383E-14, 3.196875000341420137, -1.575800808251660134 ) ) ;
#143020 = CARTESIAN_POINT ( 'NONE',  ( 0.4697016844467936103, 0.2121168557088908557, -2.196667960996725011 ) ) ;
#143019 = CARTESIAN_POINT ( 'NONE',  ( -5.526920175865215334, 9.599823971818089774, 0.7998128361456481317 ) ) ;
#143021 = CARTESIAN_POINT ( 'NONE',  ( 6.197728532230423859, -1.496850047335227085, -1.430563974149069661 ) ) ;
#143022 = CARTESIAN_POINT ( 'NONE',  ( 4.168242161197552420, 6.950367390450747251, -1.199719254218452047 ) ) ;
#143023 = CARTESIAN_POINT ( 'NONE',  ( -4.412288926243578935, 7.235088616337731260, 1.199719254218464037 ) ) ;
#143024 = CARTESIAN_POINT ( 'NONE',  ( 6.639320575229232801, 7.629137130509035636, 2.803262396134009737 ) ) ;
#143025 = CARTESIAN_POINT ( 'NONE',  ( 4.627780688875618331, -1.211982541104269062, -1.554853849032981072 ) ) ;
#143026 = CARTESIAN_POINT ( 'NONE',  ( 6.135022435551370279, 1.886083186425246971, 0.7231739236989165320 ) ) ;
#143027 = CARTESIAN_POINT ( 'NONE',  ( 4.723409996707597536, -0.1167165639803491167, 2.304856601038312913 ) ) ;
#143028 = CARTESIAN_POINT ( 'NONE',  ( 3.467685518289661317, -0.4070155273973393717, 2.021854410566482407 ) ) ;
#143029 = CARTESIAN_POINT ( 'NONE',  ( 6.534666852106798096, 7.686494751288491578, -1.082531754730543083 ) ) ;
#143030 = EDGE_CURVE ( 'NONE', #41517, #182554, #126875, .T. ) ;
#143032 = CARTESIAN_POINT ( 'NONE',  ( 6.378184920586140727, 6.405913593630768510, 0.000000000000000000 ) ) ;
#143031 = AXIS2_PLACEMENT_3D ( 'NONE', #123407, #137443, #136375 ) ;
#143033 = CARTESIAN_POINT ( 'NONE',  ( 4.899292406491845497, 6.809203455697518947, -1.599625672291273171 ) ) ;
#143034 = CARTESIAN_POINT ( 'NONE',  ( 0.6823417656249899377, 1.655208333674752730, 1.181850606188755259 ) ) ;
#143035 = CARTESIAN_POINT ( 'NONE',  ( 4.523580528814945545, 5.306540700819438960, 1.199719254218452047 ) ) ;
#143036 = CARTESIAN_POINT ( 'NONE',  ( 5.463572716182819811, 8.357623354646536384, 1.082531754730558626 ) ) ;
#143037 = CARTESIAN_POINT ( 'NONE',  ( 5.512245374570181156, 2.168932156859445737, -0.1011643165890318136 ) ) ;
#143039 = CARTESIAN_POINT ( 'NONE',  ( 3.983814121021773680, -1.821778379405362136, -0.2661574599523569007 ) ) ;
#143038 = CARTESIAN_POINT ( 'NONE',  ( -4.175548123328963079, 4.934189567714277302, 1.082531754730560403 ) ) ;
#143041 = CARTESIAN_POINT ( 'NONE',  ( 1.530808498934191324E-16, -1.500000000000001332, -1.249999999999999778 ) ) ;
#143040 = CARTESIAN_POINT ( 'NONE',  ( -10.10176665042269839, 1.000000000000000888, -6.279211784079198999 ) ) ;
#143042 = CARTESIAN_POINT ( 'NONE',  ( 5.882419586753742102, -0.3201050945752722532, -2.167950725039065052 ) ) ;
#143043 = CARTESIAN_POINT ( 'NONE',  ( 1.224999999999979217, 0.2083333340161329650, -0.7072540797572937077 ) ) ;
#143044 = CARTESIAN_POINT ( 'NONE',  ( 0.2985908658455891929, -2.261944659375872302, -0.05357643010404227607 ) ) ;
#143045 = CARTESIAN_POINT ( 'NONE',  ( -4.027792083363366693, 7.778134382787397882, 0.5015608049221946807 ) ) ;
#143046 = SURFACE_STYLE_FILL_AREA ( #141975 ) ;
#143047 = CARTESIAN_POINT ( 'NONE',  ( 4.831949485534527966, 8.212610664285437068, 0.9193987405316924599 ) ) ;
#143048 = CARTESIAN_POINT ( 'NONE',  ( -5.004368096775595021, 5.971422546727199077, 1.082531754730549078 ) ) ;
#143049 = CARTESIAN_POINT ( 'NONE',  ( -6.773846765317340868, -7.246166700180801001, -6.773846765317301788 ) ) ;
#143050 = CARTESIAN_POINT ( 'NONE',  ( 1.076598688339102772, -0.03801472141184288056, -1.769612961288852926 ) ) ;
#143051 = CARTESIAN_POINT ( 'NONE',  ( 5.162748661275342599, 0.5863960615675645194, 1.925778112416365317 ) ) ;
#143052 = CARTESIAN_POINT ( 'NONE',  ( 6.144869935491714230, 8.192100896205568361, -1.599625672291262513 ) ) ;
#143053 = CARTESIAN_POINT ( 'NONE',  ( 4.665121749186112332, -1.880042215448823661, -0.9491155671061396459 ) ) ;
#143054 = CARTESIAN_POINT ( 'NONE',  ( 3.515159831171112970, -1.768693170575957874, 0.7362056930131228860 ) ) ;
#143055 = CARTESIAN_POINT ( 'NONE',  ( 4.369805582306193870, 3.992528022312320957, 1.214306433183764966E-14 ) ) ;
#143056 = CARTESIAN_POINT ( 'NONE',  ( 4.580490420436008847, 1.213483934061266201, -1.551205257841874241 ) ) ;
#143057 = CARTESIAN_POINT ( 'NONE',  ( 5.431901110126942989, -1.969610648168946376, 0.4466083225366457854 ) ) ;
#143058 = CARTESIAN_POINT ( 'NONE',  ( 1.428351348257720588, 1.801920623737063520, 0.5021531274154652502 ) ) ;
#143061 = EDGE_LOOP ( 'NONE', ( #48010, #37690, #129046, #21288 ) ) ;
#143060 = CARTESIAN_POINT ( 'NONE',  ( 1.142663480069527671, 1.843847066288730074, 0.5072560978593986247 ) ) ;
#143059 = CARTESIAN_POINT ( 'NONE',  ( 5.373588365490253871, 1.660756567380991866, -0.4657003604296525157 ) ) ;
#143063 = CARTESIAN_POINT ( 'NONE',  ( 4.284013352238246419, 6.021101549076499637, -1.443375672974051449 ) ) ;
#143062 = CARTESIAN_POINT ( 'NONE',  ( 1.032169062358662348, -1.402649970393770484, -1.703791656331831605 ) ) ;
#143064 = CARTESIAN_POINT ( 'NONE',  ( 1.364683531249988535, 1.676041667008085101, 0.7879004041258500513 ) ) ;
#143065 = CARTESIAN_POINT ( 'NONE',  ( 6.672321430365630412, -0.9237476215336395402, -1.730755693189582667 ) ) ;
#143066 = CARTESIAN_POINT ( 'NONE',  ( 7.426115451983150706, 9.686887332112256388, -1.599625672291262513 ) ) ;
#143067 = CARTESIAN_POINT ( 'NONE',  ( 1.772826578343088544, 3.950000000000001954, -0.4500000000000284883 ) ) ;
#143068 = CARTESIAN_POINT ( 'NONE',  ( -8.762124912781128927, 3.934209603697779389, -7.549522310265974312 ) ) ;
#143069 = CARTESIAN_POINT ( 'NONE',  ( -3.716906668440817185, 7.488141546489591072, 0.7998128361456341429 ) ) ;
#143070 = ORIENTED_EDGE ( 'NONE', *, *, #142558, .F. ) ;
#143071 = CARTESIAN_POINT ( 'NONE',  ( 7.548736465707318821, -7.034525073441744603, 7.548736465708006271 ) ) ;
#143072 = ORIENTED_EDGE ( 'NONE', *, *, #60607, .F. ) ;
#143073 = CARTESIAN_POINT ( 'NONE',  ( 1.662640112210824306, -0.7432673875312334477, -1.932532381715674097 ) ) ;
#143074 = CARTESIAN_POINT ( 'NONE',  ( 1.499999999999987121, 2.545833333333351156, -0.8660254037844262731 ) ) ;
#143075 = CARTESIAN_POINT ( 'NONE',  ( 4.801558957534076022, 8.753569217098425170, 0.7998128361456462443 ) ) ;
#143076 = CARTESIAN_POINT ( 'NONE',  ( -6.191269702934848240, 10.37489842006599616, 0.000000000000000000 ) ) ;
#143077 = CARTESIAN_POINT ( 'NONE',  ( 3.984117037569365305, 5.741498858621315371, 1.599625672291261402 ) ) ;
#143078 = CARTESIAN_POINT ( 'NONE',  ( 6.199870563505585963, 1.461971410283597894, 1.536153618249151309 ) ) ;
#143079 = CARTESIAN_POINT ( 'NONE',  ( -10.91962425643199808, -9.999999999999994671, 0.09058751758333691284 ) ) ;
#143080 = CARTESIAN_POINT ( 'NONE',  ( 0.6823417656249899377, 3.092708333674754062, 1.181850606188765695 ) ) ;
#143082 = CARTESIAN_POINT ( 'NONE',  ( 9.083599731475976213, 12.58098820582193689, 1.082531754730546636 ) ) ;
#143081 = CARTESIAN_POINT ( 'NONE',  ( 11.01135777277262306, 0.000000000000000000, 1.399999999999998579 ) ) ;
#143083 = CARTESIAN_POINT ( 'NONE',  ( 5.237657596305253627, -1.897407540178517094, -0.6818907625677357309 ) ) ;
#143084 = EDGE_CURVE ( 'NONE', #156205, #163314, #27803, .T. ) ;
#143085 = CARTESIAN_POINT ( 'NONE',  ( 4.962082351039136086, -1.058791762104252632, 1.596325305674146433 ) ) ;
#143086 = SURFACE_STYLE_USAGE ( .BOTH. , #44496 ) ;
#143087 = CARTESIAN_POINT ( 'NONE',  ( 2.771223791512751333, 2.080116120148074010, -0.6901165687889163625 ) ) ;
#143088 =( BOUNDED_CURVE ( )  B_SPLINE_CURVE ( 2, ( #73236, #5018, #55943, #75397, #39689 ),
 .UNSPECIFIED., .F., .T. ) 
 B_SPLINE_CURVE_WITH_KNOTS ( ( 3, 2, 3 ),
 ( 0.2694919930870862679, 0.2750000000000000222, 0.2821090017918219117 ),
 .UNSPECIFIED. ) 
 CURVE ( )  GEOMETRIC_REPRESENTATION_ITEM ( )  RATIONAL_B_SPLINE_CURVE ( ( 0.9399548337079939309, 0.9114480397467834560, 1.000000000000000000, 0.8857089226533948478, 0.9664167589818952742 ) ) 
 REPRESENTATION_ITEM ( '' )  );
#143089 = CARTESIAN_POINT ( 'NONE',  ( 0.000000000000000000, -2.000000000000001776, 0.000000000000000000 ) ) ;
#143090 = CARTESIAN_POINT ( 'NONE',  ( -1.201851678989727383E-14, 1.243750000682821044, 1.732050807568877637 ) ) ;
#143091 = CARTESIAN_POINT ( 'NONE',  ( 5.326436552476821795, -0.9091558477445594866, -1.796327993944699219 ) ) ;
#143092 = CARTESIAN_POINT ( 'NONE',  ( 1.670022949053862948, 1.907054940702715085, -0.1439945843566131367 ) ) ;
#143093 = CARTESIAN_POINT ( 'NONE',  ( -6.880926654135487652, 7.986501503701545879, 1.199719254218450271 ) ) ;
#143095 = CARTESIAN_POINT ( 'NONE',  ( -0.08826282632121498772, -1.242921985031696153, -1.588411632956095110 ) ) ;
#143094 = CARTESIAN_POINT ( 'NONE',  ( -4.609409038966253647, 4.479991421656468908, -0.7216878364870207285 ) ) ;
#143096 = CARTESIAN_POINT ( 'NONE',  ( 1.364683531249996529, 10.02604166700806587, 0.7879004041258405033 ) ) ;
#143098 = CARTESIAN_POINT ( 'NONE',  ( -7.944151662964566540, 8.232874793072271657, 0.000000000000000000 ) ) ;
#143097 = CARTESIAN_POINT ( 'NONE',  ( 3.948837864290375421, -1.739349124335771712, -1.159800787976144720 ) ) ;
#143100 = ORIENTED_EDGE ( 'NONE', *, *, #17125, .T. ) ;
#143099 = CARTESIAN_POINT ( 'NONE',  ( 1.553258647468837461, 0.5056154618373939202, -1.648988316134043286 ) ) ;
#143101 = CARTESIAN_POINT ( 'NONE',  ( 6.345950370838201238, -1.386202306585911925, -1.604841549997563455 ) ) ;
#143102 = CARTESIAN_POINT ( 'NONE',  ( 5.823390672269506574, 6.752709524857930745, -1.199719254218446718 ) ) ;
#143103 = CARTESIAN_POINT ( 'NONE',  ( -0.7511099776682679252, 13.27260870304410822, 1.266036383821782296 ) ) ;
#143104 = CARTESIAN_POINT ( 'NONE',  ( 0.02191154088442351378, -9.962467531990274239, 9.579628365760351372 ) ) ;
#143105 = CARTESIAN_POINT ( 'NONE',  ( 11.48243876534946217, 9.799999999999998934, -3.200000000000001510 ) ) ;
#143106 = CARTESIAN_POINT ( 'NONE',  ( 4.794779880727245036, 8.745660294157122649, -0.7998128361456281477 ) ) ;
#143108 = AXIS2_PLACEMENT_3D ( 'NONE', #68788, #36300, #119763 ) ;
#143107 = CARTESIAN_POINT ( 'NONE',  ( 3.070819976953864661, 2.800000000000017586, 2.497101503370694253 ) ) ;
#143109 = CARTESIAN_POINT ( 'NONE',  ( 2.297251093426439628, 1.655750149966995544, -0.7352264245090130990 ) ) ;
#143110 = CARTESIAN_POINT ( 'NONE',  ( -7.040761844198392794, 7.108643661186573759, -0.7998128361456291469 ) ) ;
#143111 = VERTEX_POINT ( 'NONE', #45146 ) ;
#143112 = CARTESIAN_POINT ( 'NONE',  ( 3.354752944377597856, 6.001296637494123232, -1.199719254218446718 ) ) ;
#143113 = CIRCLE ( 'NONE', #191442, 0.05000000000000059258 ) ;
#143114 = ORIENTED_EDGE ( 'NONE', *, *, #182300, .T. ) ;
#143115 = CARTESIAN_POINT ( 'NONE',  ( 5.143339171537801846, 7.093924681584509173, 1.599625672291269396 ) ) ;
#143116 = CARTESIAN_POINT ( 'NONE',  ( 4.125510307337266980, -0.3055505145112321075, 1.785335377935037826 ) ) ;
#143117 = CARTESIAN_POINT ( 'NONE',  ( 0.6384131795730921821, 3.364835436752191988, 0.1378994657016461289 ) ) ;
#143118 = CARTESIAN_POINT ( 'NONE',  ( -7.334597915313094241, 9.580116872663850813, 1.040834085586084257E-14 ) ) ;
#143119 = CARTESIAN_POINT ( 'NONE',  ( 4.163006777067105091, 7.380761635867615134, 0.7803290320304544503 ) ) ;
#143120 = CARTESIAN_POINT ( 'NONE',  ( 3.701460696238024539, -1.407827198975480032, -1.217257945129922803 ) ) ;
#143121 = CARTESIAN_POINT ( 'NONE',  ( 2.091283074759576532, -0.4175699524238601357, 1.869371669076219211 ) ) ;
#143122 = CARTESIAN_POINT ( 'NONE',  ( 0.8151338971811080691, -0.2727355552937099636, 1.804975678908596226 ) ) ;
#143123 = CARTESIAN_POINT ( 'NONE',  ( 4.860027775985512832, 8.063079866353717762, 0.9206262284592428013 ) ) ;
#143124 = FACE_OUTER_BOUND ( 'NONE', #79520, .T. ) ;
#143125 = CARTESIAN_POINT ( 'NONE',  ( 5.638349000628050334, 7.351887578364292075, 1.232751772250343381 ) ) ;
#143126 = CARTESIAN_POINT ( 'NONE',  ( -10.99945475518247484, -9.908704762181759662, 0.1095286008944308248 ) ) ;
#143127 = CARTESIAN_POINT ( 'NONE',  ( -4.012850279964973232, 4.744375417122949301, 1.082531754730560403 ) ) ;
#143128 = CARTESIAN_POINT ( 'NONE',  ( 8.107412671292042461, 9.521364873671299023, 1.082531754730558626 ) ) ;
#143129 = CARTESIAN_POINT ( 'NONE',  ( 5.823099318722479545, -1.778931037738925802, -0.8454068362369684397 ) ) ;
#143130 = CARTESIAN_POINT ( 'NONE',  ( -3.405069135326500351, 7.124331091189553433, 1.040834085586084257E-14 ) ) ;
#143131 = CARTESIAN_POINT ( 'NONE',  ( -4.009193028827814587, 7.297902834095492786, -0.7581239365674132813 ) ) ;
#143132 = EDGE_CURVE ( 'NONE', #97798, #401, #33383, .T. ) ;
#143133 = CARTESIAN_POINT ( 'NONE',  ( 0.4278232814946582585, 1.072867435734598196, -1.794206126505201837 ) ) ;
#143134 = CARTESIAN_POINT ( 'NONE',  ( 7.934546212495622086, 10.28005655271014795, -1.599625672291262513 ) ) ;
#143135 = CARTESIAN_POINT ( 'NONE',  ( 5.086904980214876915, -0.2357887182157791250, -1.911833357141810241 ) ) ;
#143136 = CARTESIAN_POINT ( 'NONE',  ( -5.259673527097670664, 8.223703984000886535, -1.199719254218446718 ) ) ;
#143137 = CARTESIAN_POINT ( 'NONE',  ( 1.764397251013736234, -1.293498944356825664, 1.288518760371157201 ) ) ;
#143138 = CARTESIAN_POINT ( 'NONE',  ( 1.612255294781844706, -2.189918024983358080, 0.2725913246661854084 ) ) ;
#143139 = CARTESIAN_POINT ( 'NONE',  ( -1.115562610750309283E-14, 10.31250000000000000, 1.500000000000001554 ) ) ;
#143140 = CARTESIAN_POINT ( 'NONE',  ( 0.8614045922798494459, -1.509235727096858826, -1.174430983434850972 ) ) ;
#143141 = ADVANCED_FACE ( 'NONE', ( #111258, #15792, #176202, #29947, #161008, #78675, #178338 ), #144801, .T. ) ;
#143142 = ORIENTED_EDGE ( 'NONE', *, *, #23723, .T. ) ;
#143143 = CARTESIAN_POINT ( 'NONE',  ( 0.5198876536083548716, 1.948639688611382148, -0.2852860490613322031 ) ) ;
#143144 = CARTESIAN_POINT ( 'NONE',  ( 2.964326597902953608, -1.795398894311397209, -0.7408281928331180710 ) ) ;
#143145 = CARTESIAN_POINT ( 'NONE',  ( 1.036482258494644038, 1.943774389176852857, -0.5350038931242264706 ) ) ;
#143147 = CARTESIAN_POINT ( 'NONE',  ( 5.559367761144698328, 1.520187721101939671, 1.073055572604255214 ) ) ;
#143146 = CARTESIAN_POINT ( 'NONE',  ( -5.336015975430226099, 8.383046517047350932, -1.199719254218453823 ) ) ;
#143148 = CARTESIAN_POINT ( 'NONE',  ( 3.400062661977048428, 7.188766548940353829, -1.734723475976807094E-15 ) ) ;
#143150 = EDGE_CURVE ( 'NONE', #184212, #138616, #128596, .T. ) ;
#143149 = FACE_OUTER_BOUND ( 'NONE', #183558, .T. ) ;
#143151 = CARTESIAN_POINT ( 'NONE',  ( 9.856941372335116469, 11.45851867493453291, 1.199719254218450271 ) ) ;
#143152 = CARTESIAN_POINT ( 'NONE',  ( -5.091250377131585125, 5.898545847196970726, 1.199719254218450271 ) ) ;
#143153 = CARTESIAN_POINT ( 'NONE',  ( -5.576146316970437944, 9.727530813099326323, 0.000000000000000000 ) ) ;
#143154 = CARTESIAN_POINT ( 'NONE',  ( 2.507599501126521524, -2.167277876680247850, 0.3246147914140809498 ) ) ;
#143155 = CARTESIAN_POINT ( 'NONE',  ( 3.551873057100287223, 5.166937871415542283, 1.443375672974062551 ) ) ;
#143156 = CARTESIAN_POINT ( 'NONE',  ( 6.003228155800906407, 10.22579295840155744, 0.000000000000000000 ) ) ;
#143157 = LINE ( 'NONE', #10954, #179121 ) ;
#143158 = CARTESIAN_POINT ( 'NONE',  ( 3.176193443437186126, -1.086901434622984830, 1.466744820640853098 ) ) ;
#143159 = CARTESIAN_POINT ( 'NONE',  ( -4.243865776277440993, 4.909930479533815451, -1.199719254218446718 ) ) ;
#143160 = CARTESIAN_POINT ( 'NONE',  ( -3.521367211247373508, 5.131347717920458962, -1.599625672291256295 ) ) ;
#143161 = CARTESIAN_POINT ( 'NONE',  ( -5.188065202531182862, 7.850521293832936287, -1.269213148129512136 ) ) ;
#143162 = DIRECTION ( 'NONE',  ( 0.000000000000000000, -1.000000000000000000, 0.000000000000000000 ) ) ;
#143163 = CARTESIAN_POINT ( 'NONE',  ( 8.516493047678546091, 13.08765898893368629, -0.7998128361456352531 ) ) ;
#143164 = CARTESIAN_POINT ( 'NONE',  ( 1.066875820281657949, -1.741210523058086324, -0.8246449397346886645 ) ) ;
#143165 = CARTESIAN_POINT ( 'NONE',  ( 5.225427317040848507, 0.1961275920050585819, -1.951957996302315257 ) ) ;
#143166 = CARTESIAN_POINT ( 'NONE',  ( 1.499999999999993117, 15.10416666666666430, 0.8660254037844409281 ) ) ;
#143167 = CARTESIAN_POINT ( 'NONE',  ( -6.795661308947694934, 8.951357498570873261, -1.599625672291263179 ) ) ;
#143168 = CARTESIAN_POINT ( 'NONE',  ( 4.364835388595708743, 7.179726155748598515, 1.199719254218462483 ) ) ;
#143169 = CARTESIAN_POINT ( 'NONE',  ( 5.442994344319362021, -1.727133847215430729, -1.348975639928217118 ) ) ;
#143170 = CIRCLE ( 'NONE', #67013, 0.08000000000000020983 ) ;
#143171 = ADVANCED_FACE ( 'NONE', ( #14732 ), #26635, .T. ) ;
#143172 = CARTESIAN_POINT ( 'NONE',  ( 0.1265484174145335983, 2.536982183874235908, -2.076146791065092145 ) ) ;
#143173 = CARTESIAN_POINT ( 'NONE',  ( 4.487213805514509879, 0.09639557921744396074, 2.068113308821089902 ) ) ;
#143175 = CARTESIAN_POINT ( 'NONE',  ( 0.6823417656249882723, 1.488541667008083547, -1.181850606188749264 ) ) ;
#143174 = DIRECTION ( 'NONE',  ( -0.7613463080411786432, 0.000000000000000000, -0.6483454320283800199 ) ) ;
#143177 = ORIENTED_EDGE ( 'NONE', *, *, #83202, .F. ) ;
#143176 = VECTOR ( 'NONE', #145173, 1000.000000000000000 ) ;
#143178 = CARTESIAN_POINT ( 'NONE',  ( 3.692236332591435577, 1.971970683719068695, 1.181021729054130054 ) ) ;
#143180 = ORIENTED_EDGE ( 'NONE', *, *, #206662, .T. ) ;
#143179 = CARTESIAN_POINT ( 'NONE',  ( 7.456621297836072415, 9.722477485607340597, 1.443375672974076540 ) ) ;
#143182 = DIRECTION ( 'NONE',  ( 0.000000000000000000, 1.000000000000000000, 0.000000000000000000 ) ) ;
#143181 = CARTESIAN_POINT ( 'NONE',  ( 5.478903473698239601, 7.485416367438324059, -1.443375672974078761 ) ) ;
#143183 = CARTESIAN_POINT ( 'NONE',  ( -7.721398836998399240, -5.907420853759296264, -7.721398836998356607 ) ) ;
#143184 = CARTESIAN_POINT ( 'NONE',  ( -8.072954122294394352, 8.383144328957069291, -0.7998128361456362523 ) ) ;
#143185 = CARTESIAN_POINT ( 'NONE',  ( 3.855361883123554989, 1.927135149742021047, -0.2389370807101970084 ) ) ;
#143186 = EDGE_LOOP ( 'NONE', ( #148170, #171854, #171646, #207060 ) ) ;
#143187 = CARTESIAN_POINT ( 'NONE',  ( 8.012505595552012139, 11.33137838057728786, -1.082531754730543083 ) ) ;
#143188 = ORIENTED_EDGE ( 'NONE', *, *, #147466, .F. ) ;
#143189 = CARTESIAN_POINT ( 'NONE',  ( 5.343983030329363615, -1.218012673290536974, -1.474316871017400166 ) ) ;
#143190 = CARTESIAN_POINT ( 'NONE',  ( 5.913083851878619512, 1.523424462977729599, 0.8087443918367646090 ) ) ;
#143191 = CARTESIAN_POINT ( 'NONE',  ( 4.856657812281613751, -1.900414607462055816, -0.6748505307947461063 ) ) ;
#143192 = CARTESIAN_POINT ( 'NONE',  ( 2.970157261343746136, 6.585292010301047938, 0.4235207732182846851 ) ) ;
#143193 = CARTESIAN_POINT ( 'NONE',  ( 1.946200625105892312, 0.8427435547867198062, -2.039832142532324255 ) ) ;
#143195 = CARTESIAN_POINT ( 'NONE',  ( -3.038435823238377687, 6.558942537171132514, -0.7216878364870458196 ) ) ;
#143194 = CARTESIAN_POINT ( 'NONE',  ( 5.843201017809841247, 5.919415396974013532, 1.040834085586084257E-14 ) ) ;
#143198 = B_SPLINE_CURVE_WITH_KNOTS ( 'NONE', 3,
 ( #84787, #66371, #50163, #98920, #33899, #52293 ),
 .UNSPECIFIED., .F., .F.,
 ( 4, 2, 4 ),
 ( 1.039251754646360662E-16, 0.002037829324722970417, 0.004075658649445835884 ),
 .UNSPECIFIED. ) ;
#143197 = CARTESIAN_POINT ( 'NONE',  ( 6.696582006438861256, -0.4751199114862921791, -1.704715723353955381 ) ) ;
#143196 = CARTESIAN_POINT ( 'NONE',  ( 1.851626064562774010, 2.084957031469181654, -0.1549042654368226746 ) ) ;
#143199 = CARTESIAN_POINT ( 'NONE',  ( 5.818982467333652764, 0.9914020171761170896, -1.755767668913270407 ) ) ;
#143201 = CARTESIAN_POINT ( 'NONE',  ( 3.363489724395284597, 2.236470799849974878, -0.5019982374358539223 ) ) ;
#143200 = CARTESIAN_POINT ( 'NONE',  ( 6.073126464278658432, 6.050012061272033392, 0.000000000000000000 ) ) ;
#143202 = CARTESIAN_POINT ( 'NONE',  ( 1.517106797927396444, -0.9646358079543941866, -1.448293472534349702 ) ) ;
#143203 = CARTESIAN_POINT ( 'NONE',  ( 2.689816194747224110, 2.012238202079220439, -0.6693303307304664385 ) ) ;
#143204 = PLANE ( 'NONE',  #187030 ) ;
#143205 = CARTESIAN_POINT ( 'NONE',  ( 0.7722569432341424012, -1.726285329646786382, 0.1615719764154876226 ) ) ;
#143206 = CARTESIAN_POINT ( 'NONE',  ( -0.6801582343750420812, 1.880208333674727950, -1.178068619123883165 ) ) ;
#143207 = CARTESIAN_POINT ( 'NONE',  ( 1.187708300173949461, -1.176858333569561932, -1.441725857702576219 ) ) ;
#143208 = CARTESIAN_POINT ( 'NONE',  ( 1.240952474410524031, -2.118199589774888647, -0.4760015480929754017 ) ) ;
#143209 = CARTESIAN_POINT ( 'NONE',  ( 2.958220528980558761, -1.197304571117228100, 1.622486353517027968 ) ) ;
#143210 = CARTESIAN_POINT ( 'NONE',  ( 4.843750000000003553, 1.895863743164186710, 0.7852924748297296365 ) ) ;
#143211 = CARTESIAN_POINT ( 'NONE',  ( -1.402160292154681736E-14, 1.368750000682821710, -1.732050807568863648 ) ) ;
#143212 = CARTESIAN_POINT ( 'NONE',  ( 0.2352082051719720512, -1.762675558584745783, 0.7775455664775063891 ) ) ;
#143213 = CARTESIAN_POINT ( 'NONE',  ( 1.364683531250000303, 12.75520833367473550, -0.7879004041258355073 ) ) ;
#143214 = CARTESIAN_POINT ( 'NONE',  ( 3.516091144284401171, -0.6417545297995127518, 2.126723297420398673 ) ) ;
#143215 = EDGE_LOOP ( 'NONE', ( #72978, #63502, #200571, #97167 ) ) ;
#143216 = CARTESIAN_POINT ( 'NONE',  ( -5.810221930991193690E-16, 2.500000000682804036, -1.225000000000023626 ) ) ;
#143217 = CARTESIAN_POINT ( 'NONE',  ( 1.499999999999985123, -0.4541666666666469010, -0.8660254037844323793 ) ) ;
#143218 = CARTESIAN_POINT ( 'NONE',  ( 7.293396569147545527, 10.59638086639245280, 1.199719254218460707 ) ) ;
#143219 = CARTESIAN_POINT ( 'NONE',  ( -1.364683531250014514, 0.2385416670080863499, -0.7879004041258359514 ) ) ;
#143220 = CARTESIAN_POINT ( 'NONE',  ( 4.703538834289092030, -1.515240342570793430, -1.246145567450624991 ) ) ;
#143222 = CARTESIAN_POINT ( 'NONE',  ( -5.856759171423528088, 8.816340885760650892, 1.082531754730548412 ) ) ;
#143221 = CARTESIAN_POINT ( 'NONE',  ( 3.765413976293345844, 5.416068943807445635, 1.599625672291267398 ) ) ;
#143223 = CARTESIAN_POINT ( 'NONE',  ( 0.000000000000000000, -6.134628647623513231, 10.91970695577495931 ) ) ;
#143224 = CARTESIAN_POINT ( 'NONE',  ( 5.378307924748570557, -1.263187946576078247, 1.876752126472463367 ) ) ;
#143225 = CARTESIAN_POINT ( 'NONE',  ( 2.189955769151647580, -1.345473201219016701, -1.563545076720110227 ) ) ;
#143226 = CARTESIAN_POINT ( 'NONE',  ( -8.044065211609668253, 8.279164256499745633, 0.7998128361456602331 ) ) ;
#143227 = ORIENTED_EDGE ( 'NONE', *, *, #136379, .T. ) ;
#143228 = CARTESIAN_POINT ( 'NONE',  ( 1.499999999999987121, 1.327083334016149641, -0.8660254037844253849 ) ) ;
#143229 = CARTESIAN_POINT ( 'NONE',  ( 3.637841704585748293, 0.8437669887123750989, -1.669527271503386201 ) ) ;
#143230 = CARTESIAN_POINT ( 'NONE',  ( 2.127222352579770881, 0.3811697317757706815, 1.691523546451817683 ) ) ;
#143231 = CARTESIAN_POINT ( 'NONE',  ( 0.1348729467166914497, 0.4002676433968958558, 2.257031873882467732 ) ) ;
#143232 = CARTESIAN_POINT ( 'NONE',  ( 0.8509352111321017986, 0.6423128672003556305, 2.111239891224323983 ) ) ;
#143233 = CARTESIAN_POINT ( 'NONE',  ( 4.100566281481184738, -0.6756360485904688851, -2.053482476349233643 ) ) ;
#143234 = CARTESIAN_POINT ( 'NONE',  ( 5.472584303614713264, -0.04973451981254246174, -1.941474127069875433 ) ) ;
#143235 = CARTESIAN_POINT ( 'NONE',  ( 8.680911210833158975, 14.87390181681097090, 8.226265084022907459 ) ) ;
#143236 = CARTESIAN_POINT ( 'NONE',  ( 0.2187500114561492792, -0.7852927567033060052, 1.895863743164095894 ) ) ;
#143237 = CARTESIAN_POINT ( 'NONE',  ( 9.578206935409037115, -9.746166700193986898, -0.1671882239534273895 ) ) ;
#143238 = CARTESIAN_POINT ( 'NONE',  ( -0.2046613956954954905, -0.1581703332043625232, -2.086340352340488646 ) ) ;
#143239 = CARTESIAN_POINT ( 'NONE',  ( -1.360316468750010666, 2.869791667008063207, -0.7853790794158961308 ) ) ;
#143240 = CARTESIAN_POINT ( 'NONE',  ( 5.731092321990707283, 2.014232586630093191, 0.09613807139101374077 ) ) ;
#143241 = CARTESIAN_POINT ( 'NONE',  ( -9.691380875670077444, 10.20103253123691189, 0.7998128361456462443 ) ) ;
#143242 = CARTESIAN_POINT ( 'NONE',  ( 6.958359152311676787, 9.141171649162195934, -1.599625672291262513 ) ) ;
#143243 = CARTESIAN_POINT ( 'NONE',  ( 4.415115299905642665, 5.179997933758551554, -1.199719254218450271 ) ) ;
#143244 = CARTESIAN_POINT ( 'NONE',  ( 3.422296110638740174, 1.157362003623555236, -1.411967061744797691 ) ) ;
#143245 = CARTESIAN_POINT ( 'NONE',  ( 2.239569982544288518, -1.971322999760493300, 0.9919465654871155724 ) ) ;
#143246 = ORIENTED_EDGE ( 'NONE', *, *, #204596, .F. ) ;
#143247 = CARTESIAN_POINT ( 'NONE',  ( -5.275531169048911728, 6.287779464379406491, -1.082531754730549967 ) ) ;
#143248 = CARTESIAN_POINT ( 'NONE',  ( -3.285556943750000070, -1.596874999522043037, 0.000000000000000000 ) ) ;
#143249 = CARTESIAN_POINT ( 'NONE',  ( -8.518600588087975822, 8.832788862391110385, 1.040834085586084257E-14 ) ) ;
#143250 = CARTESIAN_POINT ( 'NONE',  ( 1.072527844217635584, 0.8224262283116140493, 1.844967818783457725 ) ) ;
#143251 = CARTESIAN_POINT ( 'NONE',  ( 1.506653248757179320, -2.110590818861147078, -0.2044851626497797559 ) ) ;
#143252 = CARTESIAN_POINT ( 'NONE',  ( -1.264911064067348656, 3.850000000000018296, 0.5000000000000064393 ) ) ;
#143253 = ORIENTED_EDGE ( 'NONE', *, *, #204318, .T. ) ;
#143254 = CARTESIAN_POINT ( 'NONE',  ( -6.069210040772897052, 7.109775131437022999, -1.199719254218453823 ) ) ;
#143255 = CARTESIAN_POINT ( 'NONE',  ( 2.395144146474707636, -1.664902989962243174, 0.8314883405181148213 ) ) ;
#143256 = CARTESIAN_POINT ( 'NONE',  ( 3.018661757337009810, 6.673522483535157868, 0.000000000000000000 ) ) ;
#143257 = CARTESIAN_POINT ( 'NONE',  ( 0.3741789627117291239, 1.245922373857488274, 1.766349570875298758 ) ) ;
#143258 = CARTESIAN_POINT ( 'NONE',  ( 6.276017556857773627, 1.753032240926259311, -0.9962986157117934560 ) ) ;
#143259 = ORIENTED_EDGE ( 'NONE', *, *, #150826, .F. ) ;
#143260 = ORIENTED_EDGE ( 'NONE', *, *, #195779, .F. ) ;
#143261 = CARTESIAN_POINT ( 'NONE',  ( -10.63367255181986160, 11.30037282007833532, 1.040834085586084257E-14 ) ) ;
#143262 = CARTESIAN_POINT ( 'NONE',  ( 4.406759617291758246, 1.409692282476209924, -1.160130723419292353 ) ) ;
#143264 = CARTESIAN_POINT ( 'NONE',  ( -5.140457058134151325, 6.683247392444177315, -1.432107399977754270 ) ) ;
#143263 = CARTESIAN_POINT ( 'NONE',  ( -4.793689830883590020, 7.750332681742931662, 1.199719254218452935 ) ) ;
#143265 = CARTESIAN_POINT ( 'NONE',  ( 6.533654944624902150, 6.813559398729744032, -0.4760831665120857648 ) ) ;
#143266 = CARTESIAN_POINT ( 'NONE',  ( 6.169296033003512925, -0.7230314695168098549, -1.882185070641306801 ) ) ;
#143267 = CARTESIAN_POINT ( 'NONE',  ( 6.281194495005370193, 1.273289214079580622, 1.330099835651930684 ) ) ;
#143268 = CARTESIAN_POINT ( 'NONE',  ( -0.02299388927986567924, 0.7252709198883336983, -1.993311845943528837 ) ) ;
#143269 = CARTESIAN_POINT ( 'NONE',  ( 4.881611394917170443, 2.154576904714616603, -0.8270325966449257882 ) ) ;
#143270 = CARTESIAN_POINT ( 'NONE',  ( 5.987861119090863049, 7.014868056141362551, 1.199719254218452047 ) ) ;
#143271 = CARTESIAN_POINT ( 'NONE',  ( 0.2806372051839324810, -1.998264896860867834, -0.5032370445638265632 ) ) ;
#143272 = CARTESIAN_POINT ( 'NONE',  ( 2.208448867685277150, 1.735655609654564113, 0.8713670519163093653 ) ) ;
#143273 = EDGE_CURVE ( 'NONE', #114068, #204013, #130423, .T. ) ;
#143274 = CARTESIAN_POINT ( 'NONE',  ( 5.220190998831037987, -1.937735447606624639, -1.235822935930783517 ) ) ;
#143275 = DIRECTION ( 'NONE',  ( -1.000000000000000000, 0.000000000000000000, 0.000000000000000000 ) ) ;
#143276 = CARTESIAN_POINT ( 'NONE',  ( -7.747558435566414659, 8.003516027774422170, -0.7998128361456362523 ) ) ;
#143277 = CARTESIAN_POINT ( 'NONE',  ( 4.926551758443064699, 1.790249073151507497, 0.5424879929923772659 ) ) ;
#143278 = EDGE_LOOP ( 'NONE', ( #110254, #140246, #110588, #155744 ) ) ;
#143281 = CARTESIAN_POINT ( 'NONE',  ( -4.610654757099099221, 7.536791762327691657, 1.199719254218452935 ) ) ;
#143280 = CARTESIAN_POINT ( 'NONE',  ( -1.500000000000013101, -0.04791666598384902026, 0.8660254037844403729 ) ) ;
#143279 = CARTESIAN_POINT ( 'NONE',  ( 2.900541297466651347, -1.884798985816903860, -0.3226963764228693576 ) ) ;
#143282 = CARTESIAN_POINT ( 'NONE',  ( 4.231241840954825584, 0.1069408422738199749, 2.204416794138922331 ) ) ;
#143283 = CARTESIAN_POINT ( 'NONE',  ( 6.983263157960370116, 2.036707217602062414, 2.350489458799970066 ) ) ;
#143284 = CARTESIAN_POINT ( 'NONE',  ( 4.489158259456265121, 7.291082831790689056, -1.082531754730548412 ) ) ;
#143285 = CARTESIAN_POINT ( 'NONE',  ( -6.753369912938502750, 7.051555451282599307, 0.000000000000000000 ) ) ;
#143286 = CARTESIAN_POINT ( 'NONE',  ( 2.214082964306641532, -0.9260232682030484774, -1.740301080291997149 ) ) ;
#143287 = CARTESIAN_POINT ( 'NONE',  ( 1.360874125193665130, 0.9374058560891560532, 2.108772699047257948 ) ) ;
#143288 = CARTESIAN_POINT ( 'NONE',  ( 2.963279974173158138, 1.655882904019840840, 1.051842618152734499 ) ) ;
#143289 = CARTESIAN_POINT ( 'NONE',  ( 11.55950211276791428, 11.37999999999998302, 3.221476510067112109 ) ) ;
#143290 = CARTESIAN_POINT ( 'NONE',  ( 6.086800983681886379, 1.986285820840045124, 0.5554444937589071429 ) ) ;
#143291 = CARTESIAN_POINT ( 'NONE',  ( 4.419594888374914099, 5.218910793601261311, -1.082531754730548412 ) ) ;
#143292 = CARTESIAN_POINT ( 'NONE',  ( 3.784388871581423786, -0.6371526190629381858, -1.913262240507591416 ) ) ;
#143293 = CARTESIAN_POINT ( 'NONE',  ( 4.030516805012513082, 7.924296382481737844, 0.000000000000000000 ) ) ;
#143294 = VERTEX_POINT ( 'NONE', #168453 ) ;
#143295 = CARTESIAN_POINT ( 'NONE',  ( -10.13488352141530768, 11.78278451552804817, 1.199719254218462483 ) ) ;
#143296 = CARTESIAN_POINT ( 'NONE',  ( 2.972033609136344623, 6.549060441754430251, -0.4946758370507741698 ) ) ;
#143297 = CARTESIAN_POINT ( 'NONE',  ( 8.374132434735052755, 12.92157160716627295, -0.7998128361456352531 ) ) ;
#143298 = CARTESIAN_POINT ( 'NONE',  ( 2.026474435558190734, 1.113403481674969608, 1.863675736879222278 ) ) ;
#143299 = SURFACE_STYLE_FILL_AREA ( #190919 ) ;
#143300 = CARTESIAN_POINT ( 'NONE',  ( -0.8991744117087477894, 14.53091782053303049, -11.99999999953292296 ) ) ;
#143301 = CARTESIAN_POINT ( 'NONE',  ( -2.976926559254097437, 6.503136272932390050, -0.2410342056339362937 ) ) ;
#143302 = CARTESIAN_POINT ( 'NONE',  ( 2.020564968092851021, 1.743606242109306148, 0.6777753874912320065 ) ) ;
#143303 = CARTESIAN_POINT ( 'NONE',  ( 0.2806372051839324810, -1.998264896860867834, -0.5032370445638265632 ) ) ;
#143305 = CARTESIAN_POINT ( 'NONE',  ( 6.827182134110178602, 3.710826266403470797, 2.225597045202745594 ) ) ;
#143304 = CARTESIAN_POINT ( 'NONE',  ( 0.07755575628183573877, 1.325091491099144259, -2.441202027401535357 ) ) ;
#143306 = CARTESIAN_POINT ( 'NONE',  ( -1.364683531250000748, -1.240624999658580752, 0.000000000000000000 ) ) ;
#143307 = CARTESIAN_POINT ( 'NONE',  ( -1.456203110946918233, 3.350064908098031147, 0.3915051095678106496 ) ) ;
#143308 = CARTESIAN_POINT ( 'NONE',  ( 1.752457306817490457, 1.891635876823925200, 0.2793096714826873161 ) ) ;
#143309 = CARTESIAN_POINT ( 'NONE',  ( 3.854177328971124084, 0.6370089842938561064, 1.651420920916975232 ) ) ;
#143310 = CARTESIAN_POINT ( 'NONE',  ( 1.348149404638066873, 0.9416913409402676294, -1.664245089135652389 ) ) ;
#143311 = CARTESIAN_POINT ( 'NONE',  ( -4.232116505760120440, 8.089219690028791376, -0.7998128361456281477 ) ) ;
#143312 = CARTESIAN_POINT ( 'NONE',  ( 6.398046686924231174, -0.9077857338794625974, -1.686868998638735073 ) ) ;
#143313 = CARTESIAN_POINT ( 'NONE',  ( 0.7499999999999885647, -0.01666666666664401442, 1.299038105676657340 ) ) ;
#143314 = CARTESIAN_POINT ( 'NONE',  ( 1.240778115703184303, -2.019486815914430355, -0.4554155650244652853 ) ) ;
#143315 = CARTESIAN_POINT ( 'NONE',  ( -1.499999999999997780, 5.400000000000022560, 1.214306433183764966E-14 ) ) ;
#143316 = CARTESIAN_POINT ( 'NONE',  ( 5.172658500931742509, -1.761684834526537680, -0.6294727512598657926 ) ) ;
#143317 = CARTESIAN_POINT ( 'NONE',  ( 1.646812808029130215, -1.543121136568927243, 0.9753659028155501343 ) ) ;
#143319 = CARTESIAN_POINT ( 'NONE',  ( 4.678042868546113731, 8.270637144445508682, 0.5573067791126932180 ) ) ;
#143318 = CARTESIAN_POINT ( 'NONE',  ( 5.321004863918796346, 2.037934703285459115, 0.8473243778325880715 ) ) ;
#143320 = CARTESIAN_POINT ( 'NONE',  ( -1.364683531250010295, 5.551041667008087543, -0.7879004041258300672 ) ) ;
#143321 = CARTESIAN_POINT ( 'NONE',  ( 3.437984354829794142, 1.306305779046763149, 1.596332929251530253 ) ) ;
#143323 = CARTESIAN_POINT ( 'NONE',  ( -7.226659571283968297, 8.389856573708110332, 1.199719254218450271 ) ) ;
#143322 = CIRCLE ( 'NONE', #32565, 0.08000000000000020983 ) ;
#143324 = CARTESIAN_POINT ( 'NONE',  ( -11.48243876534946040, 11.29999999999999893, -3.200000000000001510 ) ) ;
#143325 = CARTESIAN_POINT ( 'NONE',  ( 1.265302052550089540, 3.921372892477353655, -0.4993130731308050296 ) ) ;
#143326 = CARTESIAN_POINT ( 'NONE',  ( 5.505492895601038938, 8.580769590579979678, -1.199719254218452047 ) ) ;
#143327 = ORIENTED_EDGE ( 'NONE', *, *, #41574, .T. ) ;
#143328 = CARTESIAN_POINT ( 'NONE',  ( 5.881320641815353412, -0.05461762546566179682, 2.069818975884097689 ) ) ;
#143330 = CARTESIAN_POINT ( 'NONE',  ( -1.364683531250014514, -0.1572916663252435232, 0.7879004041258379498 ) ) ;
#143329 = CIRCLE ( 'NONE', #160442, 9.616019636405020776 ) ;
#143331 = CARTESIAN_POINT ( 'NONE',  ( 3.110779230992101407, 1.568002374463087989, -1.488160049990403078 ) ) ;
#143332 = CARTESIAN_POINT ( 'NONE',  ( -4.603423314590644466, 8.384863137925270493, -0.01591256823598764802 ) ) ;
#143333 = CARTESIAN_POINT ( 'NONE',  ( 2.860025901456241471, 0.7249204854099660089, -1.885284610270787642 ) ) ;
#143334 = CARTESIAN_POINT ( 'NONE',  ( 6.620655732516649294, 0.5674144795907026806, 2.226195167976598110 ) ) ;
#143337 = CARTESIAN_POINT ( 'NONE',  ( 7.212574532790092974, 9.437756259720353924, -1.443375672974057666 ) ) ;
#143336 = CARTESIAN_POINT ( 'NONE',  ( 1.737499999999999378, -2.216666666666665453, -3.009438278150925683 ) ) ;
#143335 = SURFACE_STYLE_FILL_AREA ( #108729 ) ;
#143338 = CARTESIAN_POINT ( 'NONE',  ( -7.957709816578236506, 8.248692638954882028, 0.7998128361456341429 ) ) ;
#143339 = CARTESIAN_POINT ( 'NONE',  ( 0.9015777671340443611, -1.966303774932298021, 0.4465067697373495403 ) ) ;
#143341 = CARTESIAN_POINT ( 'NONE',  ( 6.515165533258342023, -2.126321577054360201, 0.5302794918827999915 ) ) ;
#143340 = CARTESIAN_POINT ( 'NONE',  ( -4.120788623549732854, 6.895004929861607401, -1.199719254218452047 ) ) ;
#143342 = CARTESIAN_POINT ( 'NONE',  ( -1.001543065824772872E-14, 4.243750000682819490, 1.732050807568877637 ) ) ;
#143343 = CARTESIAN_POINT ( 'NONE',  ( 5.150612376422202487, 1.885107930906554152, 0.3209214958604587054 ) ) ;
#143344 = CARTESIAN_POINT ( 'NONE',  ( -3.521367211247373508, 5.131347717920458962, -1.599625672291256295 ) ) ;
#143345 = CARTESIAN_POINT ( 'NONE',  ( 5.450014562569148957, 9.302174723065263606, 1.040834085586084257E-14 ) ) ;
#143347 = CARTESIAN_POINT ( 'NONE',  ( 3.198842376697589085, 1.824128004127192337, 0.8596145101084637918 ) ) ;
#143346 = CARTESIAN_POINT ( 'NONE',  ( -9.937763408692600109, 10.69640485300394417, -0.7216878364870267237 ) ) ;
#143348 = CARTESIAN_POINT ( 'NONE',  ( 1.364683531250000303, 13.81770833367473017, -0.7879004041258355073 ) ) ;
#143349 = CARTESIAN_POINT ( 'NONE',  ( -6.180537922983287302, 8.303989891604203422, -1.599625672291271394 ) ) ;
#143350 = CARTESIAN_POINT ( 'NONE',  ( 4.875862107049974803, 0.9950566627994448243, 1.408581599115072747 ) ) ;
#143351 = CARTESIAN_POINT ( 'NONE',  ( 6.713222337422018349, 7.861122810861019161, -1.199719254218452047 ) ) ;
#143352 = CARTESIAN_POINT ( 'NONE',  ( 10.38518247838791986, 11.21839376764850726, 0.7216878364870438212 ) ) ;
#143353 = CARTESIAN_POINT ( 'NONE',  ( -10.91970695577495398, -6.134628647623513231, -0.07999999999999153621 ) ) ;
#143354 = CARTESIAN_POINT ( 'NONE',  ( 4.903500725120335524, -0.5004011548357701900, 1.802273645872286334 ) ) ;
#143355 = CARTESIAN_POINT ( 'NONE',  ( 1.358353136502857161, -2.070434559563800736, -0.003889755252693693176 ) ) ;
#143356 = CARTESIAN_POINT ( 'NONE',  ( 11.01135777277262306, 10.89999999999998259, 1.399999999999998579 ) ) ;
#143357 = ORIENTED_EDGE ( 'NONE', *, *, #117333, .T. ) ;
#143358 = CARTESIAN_POINT ( 'NONE',  ( 6.358062532015329005, 0.6862230018901045447, -1.676680497432983641 ) ) ;
#143359 = CARTESIAN_POINT ( 'NONE',  ( 5.551137550152489553, 5.441024994791534120, 0.7998128361456352531 ) ) ;
#143360 = CARTESIAN_POINT ( 'NONE',  ( -5.204170427930421283E-14, 3.949999999999960654, -4.683753385137379155E-14 ) ) ;
#143361 = CARTESIAN_POINT ( 'NONE',  ( -0.1231740688493014324, -1.618022042794277748, -0.8147913963296258277 ) ) ;
#143362 = CARTESIAN_POINT ( 'NONE',  ( 4.055297343818923039, 7.745280977848496562, 0.7216878364870257245 ) ) ;
#143363 = CARTESIAN_POINT ( 'NONE',  ( 11.97035325917572379, 7.690326957080006132, -0.8713173324656824370 ) ) ;
#143364 = CARTESIAN_POINT ( 'NONE',  ( 2.642740014504705748, -1.821389600533462216, 1.218302608185666491 ) ) ;
#143365 = ORIENTED_EDGE ( 'NONE', *, *, #83013, .F. ) ;
#143367 = CARTESIAN_POINT ( 'NONE',  ( 9.738834413317897898, 10.25639499182604730, 0.000000000000000000 ) ) ;
#143366 = CARTESIAN_POINT ( 'NONE',  ( 0.8187140321147531319, -1.423520202335259999, 1.350257566363553208 ) ) ;
#143368 = CARTESIAN_POINT ( 'NONE',  ( 4.675340500466128368, 1.422229311605049507, 1.283493733622777189 ) ) ;
#143369 = DIRECTION ( 'NONE',  ( -1.000000000000000000, 7.771561172376097755E-16, 4.440892098500627148E-16 ) ) ;
#143370 = CARTESIAN_POINT ( 'NONE',  ( -5.425839481171796486, 7.540841100536294306, 1.248335065278019629 ) ) ;
#143371 = AXIS2_PLACEMENT_3D ( 'NONE', #98438, #13959, #97389 ) ;
#143372 = CARTESIAN_POINT ( 'NONE',  ( -1.402160292154681736E-14, 0.07187500034142156602, 1.575800808251672791 ) ) ;
#143374 = ORIENTED_EDGE ( 'NONE', *, *, #76686, .F. ) ;
#143373 = CARTESIAN_POINT ( 'NONE',  ( 6.168596704537822717, 6.299043698156668647, 1.040834085586084257E-14 ) ) ;
#143375 = CARTESIAN_POINT ( 'NONE',  ( -7.700668062882059850, 11.92793714009701311, -0.7216878364870267237 ) ) ;
#143376 = CARTESIAN_POINT ( 'NONE',  ( 2.272554088390315030, -1.330374092946192688, 1.703740541667747133 ) ) ;
#143377 = CARTESIAN_POINT ( 'NONE',  ( -3.122120512896910505, 6.864500708346841229, 0.7998128361456352531 ) ) ;
#143378 = CIRCLE ( 'NONE', #32630, 0.08000000000000025147 ) ;
#143379 = CARTESIAN_POINT ( 'NONE',  ( 6.319508997745523438, 9.426492026461511742, -1.082531754730548412 ) ) ;
#143380 = CARTESIAN_POINT ( 'NONE',  ( 5.069292194207453583, 0.1776299070984053985, -1.816928125296768393 ) ) ;
#143381 = CARTESIAN_POINT ( 'NONE',  ( 8.523843703926681670, 12.47051211315569574, -8.417911888829477718 ) ) ;
#143382 = CARTESIAN_POINT ( 'NONE',  ( 0.7374959811429316892, -1.390993636481972606, -1.397171308748794250 ) ) ;
#143383 = CARTESIAN_POINT ( 'NONE',  ( 3.603681638446740720, 1.388520161702249567, 1.315275747533505069 ) ) ;
#143384 = ORIENTED_EDGE ( 'NONE', *, *, #101370, .T. ) ;
#143385 =( REPRESENTATION_RELATIONSHIP ('NONE','NONE', #84563, #142805 ) REPRESENTATION_RELATIONSHIP_WITH_TRANSFORMATION ( #154367 )SHAPE_REPRESENTATION_RELATIONSHIP( ) );
#143386 = CARTESIAN_POINT ( 'NONE',  ( 4.017982430692658369, 1.954955499905395522, -0.2386041268068790633 ) ) ;
#143387 = ORIENTED_EDGE ( 'NONE', *, *, #140872, .F. ) ;
#143388 = CARTESIAN_POINT ( 'NONE',  ( 6.216353431943378638, 1.813724785205795609, 0.6947406154040984827 ) ) ;
#143389 = VERTEX_POINT ( 'NONE', #583 ) ;
#143390 = CARTESIAN_POINT ( 'NONE',  ( -6.934069218746458318, 7.054445274817795486, -0.7998128361456362523 ) ) ;
#143392 = CARTESIAN_POINT ( 'NONE',  ( 7.057683771862822475, -6.583723166013057515, -6.531918710724782251 ) ) ;
#143391 = CARTESIAN_POINT ( 'NONE',  ( -4.878955176071358757, 6.785476686873604280, -1.599625672291271394 ) ) ;
#143394 = EDGE_CURVE ( 'NONE', #163825, #91840, #30004, .T. ) ;
#143393 = CARTESIAN_POINT ( 'NONE',  ( 7.960045584554727327, 8.459343734834927631, 0.7216878364870267237 ) ) ;
#143395 = CARTESIAN_POINT ( 'NONE',  ( 4.371672787583542608, 0.4156390277068115480, -1.866406306929219605 ) ) ;
#143396 = CARTESIAN_POINT ( 'NONE',  ( 4.912861335034773624, 6.872882102868723919, -1.423633489635463878 ) ) ;
#143397 = CARTESIAN_POINT ( 'NONE',  ( 0.000000000000000000, -5.166862915010159263, 0.000000000000000000 ) ) ;
#143398 = CARTESIAN_POINT ( 'NONE',  ( 0.1654306582001447423, -1.972458130798220299, -0.9897840116655575171 ) ) ;
#143399 = SURFACE_STYLE_USAGE ( .BOTH. , #49854 ) ;
#143400 = CARTESIAN_POINT ( 'NONE',  ( 5.496744759480266751, -1.964553546248495541, -0.4387526145827134183 ) ) ;
#143401 = CARTESIAN_POINT ( 'NONE',  ( 0.1331565106231328843, 0.003911343561965873426, -1.946049565259087455 ) ) ;
#143403 = CARTESIAN_POINT ( 'NONE',  ( 5.594935472981866553, 1.780666063871166882, 0.9463038388278843804 ) ) ;
#143402 = CARTESIAN_POINT ( 'NONE',  ( 6.516225534515442952, -0.8655890497146904172, -1.607451055071248636 ) ) ;
#143404 = CARTESIAN_POINT ( 'NONE',  ( 1.979048004138800998, 1.930994533390210544, 0.7472069620131777112 ) ) ;
#143405 = CARTESIAN_POINT ( 'NONE',  ( -8.215877900201387973, 8.687538426430837291, 0.7216878364870578100 ) ) ;
#143406 = CARTESIAN_POINT ( 'NONE',  ( -6.357087581413799704, 6.851358791993434671, -0.6307199548913413611 ) ) ;
#143407 = CARTESIAN_POINT ( 'NONE',  ( -9.336326716892640931, -1.000000000000000888, -2.500000000000000444 ) ) ;
#143408 = CARTESIAN_POINT ( 'NONE',  ( -1.642778471874998480, -3.201041666188710000, 2.845375778867863303 ) ) ;
#143409 = CARTESIAN_POINT ( 'NONE',  ( 6.425674737872927089, 9.584038729905381970, -1.199719254218440723 ) ) ;
#143410 = CARTESIAN_POINT ( 'NONE',  ( 0.000000000000000000, 11.37999999999999901, 0.000000000000000000 ) ) ;
#143411 = CARTESIAN_POINT ( 'NONE',  ( 4.692530564105613422, 7.528350520548263702, -1.082531754730548412 ) ) ;
#143412 = CARTESIAN_POINT ( 'NONE',  ( 4.376584659113025744, 4.000436945253625254, 0.7998128361456341429 ) ) ;
#143413 = CARTESIAN_POINT ( 'NONE',  ( 0.6823417656249934904, 11.50520833367473017, 1.181850606188764807 ) ) ;
#143414 = CARTESIAN_POINT ( 'NONE',  ( -5.298539104842322267, 5.076050465271134016, 0.7998128361456341429 ) ) ;
#143416 = CARTESIAN_POINT ( 'NONE',  ( -6.688968683495758683, 8.897159112202094988, -1.599625672291271394 ) ) ;
#143415 = CARTESIAN_POINT ( 'NONE',  ( -4.207966135563104615, 7.175396087857926375, -2.420000000000000373 ) ) ;
#143417 = CARTESIAN_POINT ( 'NONE',  ( 3.814867129904021770, 0.9234608866974923780, -1.467580195302587986 ) ) ;
#143418 = CARTESIAN_POINT ( 'NONE',  ( -4.765854690403601879, 5.518917546014321829, 1.199719254218462483 ) ) ;
#143419 = CARTESIAN_POINT ( 'NONE',  ( 1.147426569842596722, 1.827566109494669577, -0.9725325914680116313 ) ) ;
#143420 = EDGE_CURVE ( 'NONE', #21442, #8341, #55730, .T. ) ;
#143421 = CARTESIAN_POINT ( 'NONE',  ( 3.761412437133329068, 1.992871936191454418, -0.7152352101782408766 ) ) ;
#143422 = CARTESIAN_POINT ( 'NONE',  ( 8.599949509769960088, 8.927695937686774386, 1.040834085586084257E-14 ) ) ;
#143423 = CARTESIAN_POINT ( 'NONE',  ( 0.02006731904125590854, 6.417555505232583002, 3.190074006977743792 ) ) ;
#143424 = CARTESIAN_POINT ( 'NONE',  ( 6.895378825052528526, -1.852007112603266670, 0.9253362530580526712 ) ) ;
#143425 = CARTESIAN_POINT ( 'NONE',  ( 4.699069518069377338, 7.059409271092678573, 1.379435410134820295 ) ) ;
#143426 = CARTESIAN_POINT ( 'NONE',  ( 3.389175213736285386, 6.897862149426897460, 0.7216878364870317197 ) ) ;
#143428 = DIRECTION ( 'NONE',  ( 0.000000000000000000, -1.000000000000000000, 0.000000000000000000 ) ) ;
#143427 = CARTESIAN_POINT ( 'NONE',  ( 1.001543065824772753E-15, -0.9624999999999998002, 4.012584370867899430 ) ) ;
#143429 = CARTESIAN_POINT ( 'NONE',  ( 3.591970686985697547, -2.289577047158963374, -0.1132367156824985732 ) ) ;
#143430 = CARTESIAN_POINT ( 'NONE',  ( 0.1701549220758866166, -1.195335944658926230, 1.380069390326914336 ) ) ;
#143431 = CARTESIAN_POINT ( 'NONE',  ( 3.603681638446740720, 1.388520161702249567, 1.315275747533505069 ) ) ;
#143432 = CARTESIAN_POINT ( 'NONE',  ( 5.936491157937257235, 8.019268665717216749, 1.599625672291268286 ) ) ;
#143433 = CARTESIAN_POINT ( 'NONE',  ( 5.599154252319471503, 9.476171027773981237, -0.7216878364870267237 ) ) ;
#143434 = CARTESIAN_POINT ( 'NONE',  ( -9.806625181386236179, 10.33548422123910449, -0.7998128361456291469 ) ) ;
#143435 = CARTESIAN_POINT ( 'NONE',  ( 1.810793108869549917, -0.5408357282137785660, -1.939109541719201912 ) ) ;
#143436 = CARTESIAN_POINT ( 'NONE',  ( 2.043732491806522056, 1.349072470436333715, 1.424505092005624807 ) ) ;
#143437 = CARTESIAN_POINT ( 'NONE',  ( -9.297140650669053485, 11.86975006391249643, 1.599625672291281386 ) ) ;
#143438 = CARTESIAN_POINT ( 'NONE',  ( -7.400052914960538963, 7.527816577075747695, 1.040834085586084257E-14 ) ) ;
#143439 = CARTESIAN_POINT ( 'NONE',  ( -11.81718632094301746, 7.791935455490584417, 1.824594704062737271 ) ) ;
#143441 = CARTESIAN_POINT ( 'NONE',  ( 3.590472238826939666, -0.3446705786002961514, -1.735762067166376710 ) ) ;
#143440 = CARTESIAN_POINT ( 'NONE',  ( 5.261704619121490900, 1.029696775897260830, 1.819396322279245304 ) ) ;
#143442 = CARTESIAN_POINT ( 'NONE',  ( -3.501245407925564823, 14.00000000000089173, 11.28115623562654513 ) ) ;
#143444 = CARTESIAN_POINT ( 'NONE',  ( 0.05887529153619439071, -1.959562692596405364, -0.9812908054248059564 ) ) ;
#143443 = FACE_OUTER_BOUND ( 'NONE', #103100, .T. ) ;
#143445 = CARTESIAN_POINT ( 'NONE',  ( 6.035049474595155949, -1.265358352104806183, -1.195092038424966363 ) ) ;
#143446 = CARTESIAN_POINT ( 'NONE',  ( 8.762647353133951711, 9.117510088278095282, 1.040834085586084257E-14 ) ) ;
#143447 = CARTESIAN_POINT ( 'NONE',  ( -7.341412881700131621, -6.244189044378193110, 6.724721492623497276 ) ) ;
#143448 = CARTESIAN_POINT ( 'NONE',  ( 4.798016402085652388, -1.585019518093808699, 0.7031974489903334291 ) ) ;
#143449 = CARTESIAN_POINT ( 'NONE',  ( 6.373493056145338009, -0.2723341383174918695, 2.153988726128319264 ) ) ;
#143450 = CARTESIAN_POINT ( 'NONE',  ( -0.6125000000000123679, 2.958333333333326820, -1.060881119635965764 ) ) ;
#143451 = CARTESIAN_POINT ( 'NONE',  ( 0.5677576367011258895, 1.426771234092726104, 1.564575111376417915 ) ) ;
#143452 = CARTESIAN_POINT ( 'NONE',  ( 5.656250000000004441, -1.895863743163955339, 0.7852924748302813063 ) ) ;
#143453 = CARTESIAN_POINT ( 'NONE',  ( -3.337985173046072340, 6.383183490859034137, 0.8077998227833966816 ) ) ;
#143454 = CARTESIAN_POINT ( 'NONE',  ( 3.311465173828963326, -0.3771673786017637475, 1.888946036755128288 ) ) ;
#143455 = CARTESIAN_POINT ( 'NONE',  ( -1.500000000000001110, 11.55208333401612997, 0.8660254037844419273 ) ) ;
#143456 = CARTESIAN_POINT ( 'NONE',  ( 0.3115808214643934204, 1.843292235811417878, -1.239274738845694390 ) ) ;
#143457 = ORIENTED_EDGE ( 'NONE', *, *, #13041, .F. ) ;
#143458 = CARTESIAN_POINT ( 'NONE',  ( -0.1408020194050146334, 0.2351808081714431564, -2.134421755367508666 ) ) ;
#143459 = CARTESIAN_POINT ( 'NONE',  ( -1.499999999999997780, 2.650000000000020339, 1.214306433183764966E-14 ) ) ;
#143460 = CARTESIAN_POINT ( 'NONE',  ( 6.419949431270806528, 7.448694743692793274, 1.199719254218462483 ) ) ;
#143461 = CARTESIAN_POINT ( 'NONE',  ( 3.141495721539554697, 0.05644213937440466927, 2.220748567232306847 ) ) ;
#143462 = PRESENTATION_STYLE_ASSIGNMENT (( #156483 ) ) ;
#143463 = ADVANCED_FACE ( 'NONE', ( #17912 ), #168366, .F. ) ;
#143464 = CARTESIAN_POINT ( 'NONE',  ( 7.958272981541723468, 8.386999354661243800, 1.040834085586084257E-14 ) ) ;
#143465 = DIRECTION ( 'NONE',  ( -1.000000000000000000, -3.451266460341926649E-31, -8.638326563840809144E-31 ) ) ;
#143466 = VECTOR ( 'NONE', #103148, 1000.000000000000000 ) ;
#143467 = CARTESIAN_POINT ( 'NONE',  ( 3.770049233051776749, 6.556085317605844232, 1.199719254218451159 ) ) ;
#143468 = CARTESIAN_POINT ( 'NONE',  ( 0.1764080092822375156, 1.496053712750060383, 1.352152247781977179 ) ) ;
#143470 = CARTESIAN_POINT ( 'NONE',  ( 5.529752758335351182, 1.988887524167002985, -0.5466100825702590038 ) ) ;
#143469 = CARTESIAN_POINT ( 'NONE',  ( 9.725276259704228821, 10.24057714594344048, 0.7998128361456462443 ) ) ;
#143471 = CARTESIAN_POINT ( 'NONE',  ( 3.686212053427321056, 6.121915856213854923, 1.284222742053100941 ) ) ;
#143472 = CARTESIAN_POINT ( 'NONE',  ( -2.578021764892882040, 6.159442492350315490, 0.7998128361456341429 ) ) ;
#143473 = VECTOR ( 'NONE', #40258, 1000.000000000000114 ) ;
#143474 = SURFACE_STYLE_USAGE ( .BOTH. , #77360 ) ;
#143475 = CARTESIAN_POINT ( 'NONE',  ( 1.364683531249986537, 0.6552083336747522857, -0.7879004041258239610 ) ) ;
#143476 = CARTESIAN_POINT ( 'NONE',  ( 0.7722622890447777833, -1.663610408097391691, -0.6040080933595278756 ) ) ;
#143477 = CARTESIAN_POINT ( 'NONE',  ( 5.713412806352172524, 1.673543110082301721, 0.4542079487798825199 ) ) ;
#143478 = CARTESIAN_POINT ( 'NONE',  ( 5.302228144868663229, 1.312797389530523162, -1.142775443803839108 ) ) ;
#143479 = CARTESIAN_POINT ( 'NONE',  ( 3.544716187562162446, -1.873399702441876480, 1.320855843532109608 ) ) ;
#143480 = CARTESIAN_POINT ( 'NONE',  ( 1.364683531249986537, -0.8864583329919110133, 0.7879004041258500513 ) ) ;
#143481 = CARTESIAN_POINT ( 'NONE',  ( 1.974305314296275649, -0.08955604370030831318, -1.839086841257123073 ) ) ;
#143482 = CARTESIAN_POINT ( 'NONE',  ( 8.829384350997564468, 11.32403438096243775, 1.599625672291281386 ) ) ;
#143483 = CARTESIAN_POINT ( 'NONE',  ( 0.000000000000000000, 3.999999999999996447, 0.000000000000000000 ) ) ;
#143484 = CARTESIAN_POINT ( 'NONE',  ( 1.975362765405625609, 1.747911882041437659, -0.5268472171036930884 ) ) ;
#143485 = CARTESIAN_POINT ( 'NONE',  ( 3.006482587178582300, -1.942541511447487990, 0.5404910644229294903 ) ) ;
#143486 = CARTESIAN_POINT ( 'NONE',  ( -2.589244150085650009, 5.964609241834465614, 0.7216878364870317197 ) ) ;
#143487 = CARTESIAN_POINT ( 'NONE',  ( 7.320801413324473650, 15.00000000000000000, -10.35317664616355771 ) ) ;
#143488 = CARTESIAN_POINT ( 'NONE',  ( 4.753012104044548991, -1.692955597047377747, 1.252381512178860401 ) ) ;
#143489 = CARTESIAN_POINT ( 'NONE',  ( -5.713871673155502151, 8.753601821068331290, 1.199719254218452047 ) ) ;
#143490 = CARTESIAN_POINT ( 'NONE',  ( 6.978632775467555227, 14.99421780237605795, 9.366897188349161851 ) ) ;
#143491 = AXIS2_PLACEMENT_3D ( 'NONE', #112083, #131506, #163971 ) ;
#143492 = CARTESIAN_POINT ( 'NONE',  ( 2.471216696211364638, 1.848302923701108158, 0.9330170062570308787 ) ) ;
#143493 = CARTESIAN_POINT ( 'NONE',  ( 3.344057444064992168, 7.053150784717805877, 1.040834085586084257E-14 ) ) ;
#143494 = CARTESIAN_POINT ( 'NONE',  ( 0.6801582343749726922, 0.7552083336747339448, 1.178068619123784355 ) ) ;
#143495 = CARTESIAN_POINT ( 'NONE',  ( 4.565154201998150363, -1.702539431995837349, 1.263830167178958463 ) ) ;
#143496 = CARTESIAN_POINT ( 'NONE',  ( 0.01214912391013078102, -0.8215866570660257384, -1.740624652096602221 ) ) ;
#143497 = B_SPLINE_CURVE_WITH_KNOTS ( 'NONE', 3,
 ( #104015, #1144, #36857, #35795, #70404, #182035, #18472, #102941, #87753, #69341 ),
 .UNSPECIFIED., .F., .F.,
 ( 4, 3, 3, 4 ),
 ( 0.000000000000000000, 4.502046072368973497E-05, 9.004093402560359031E-05, 0.0001800865003231039206 ),
 .UNSPECIFIED. ) ;
#143498 = ORIENTED_EDGE ( 'NONE', *, *, #164027, .F. ) ;
#143499 = CARTESIAN_POINT ( 'NONE',  ( -5.492988512192097161, 6.437516681426083132, 1.199719254218452935 ) ) ;
#143500 = CARTESIAN_POINT ( 'NONE',  ( 7.750457368506414646, 12.19395069656619945, 0.7998128361456462443 ) ) ;
#143501 = CARTESIAN_POINT ( 'NONE',  ( 1.737499999999999378, -1.122916665710751882, -3.009438278150925683 ) ) ;
#143502 = CARTESIAN_POINT ( 'NONE',  ( -5.229694566569281555, 7.124396299129368337, 1.599625672291267398 ) ) ;
#143503 = CARTESIAN_POINT ( 'NONE',  ( 6.363548717301088509, -1.704009271243651868, -1.262090224194649446 ) ) ;
#143504 = CARTESIAN_POINT ( 'NONE',  ( 1.553890309278640025, 0.6119248022173563450, -2.015079113363055452 ) ) ;
#143505 = CARTESIAN_POINT ( 'NONE',  ( -4.630991987519598396, 7.560518531151607213, 1.199719254218452935 ) ) ;
#143506 = CARTESIAN_POINT ( 'NONE',  ( 7.567422294721922960, 11.98040977715095323, 0.7998128361456462443 ) ) ;
#143507 = CARTESIAN_POINT ( 'NONE',  ( 6.438329693799461850, -0.9962124079390155540, 1.571646734037221105 ) ) ;
#143508 = CARTESIAN_POINT ( 'NONE',  ( 7.076466111328892694, 10.34329533227067799, -1.199719254218441611 ) ) ;
#143509 =( BOUNDED_SURFACE ( )  B_SPLINE_SURFACE ( 3, 2, ( 
 ( #66493, #16690, #85980 ),
 ( #83835, #197587, #115350 ),
 ( #53475, #185597, #165099 ),
 ( #181341, #36147, #200767 ),
 ( #148848, #34025, #132633 ),
 ( #32968, #421, #149926 ) ),
 .UNSPECIFIED., .F., .F., .F. ) 
 B_SPLINE_SURFACE_WITH_KNOTS ( ( 4, 2, 4 ),
 ( 3, 3 ),
 ( 0.000000000000000000, 0.0003766405729503174787, 0.0007532811459006349573 ),
 ( 0.000000000000000000, 1.000000000000000000 ),
 .UNSPECIFIED. ) 
 GEOMETRIC_REPRESENTATION_ITEM ( )  RATIONAL_B_SPLINE_SURFACE ( (
 ( 1.000000000000000000, 0.7071067811865551223, 1.000000000000000000),
 ( 1.000000000000000000, 0.7211294902953826469, 1.000000000000000000),
 ( 1.000000000000000000, 0.7311181975230335306, 1.000000000000000000),
 ( 1.000000000000000000, 0.7429553055061443034, 1.000000000000000000),
 ( 1.000000000000000000, 0.7451698531058299491, 1.000000000000000000),
 ( 1.000000000000000000, 0.7452309222762957264, 1.000000000000000000) ) ) 
 REPRESENTATION_ITEM ( '' )  SURFACE ( )  );
#143510 = DIRECTION ( 'NONE',  ( 1.665334536937734811E-16, 0.000000000000000000, 1.000000000000000000 ) ) ;
#143511 = CARTESIAN_POINT ( 'NONE',  ( -4.309512724297390740, 6.121127159803966933, 1.599625672291270506 ) ) ;
#143512 = CARTESIAN_POINT ( 'NONE',  ( -8.188761592974033832, 12.49737959187099179, -0.7216878364870267237 ) ) ;
#143513 = CARTESIAN_POINT ( 'NONE',  ( 0.3168469074051638024, -0.7203255543706194031, -1.994627023381766673 ) ) ;
#143514 = CARTESIAN_POINT ( 'NONE',  ( 0.8145602173408479363, -4.140925090156039268, 0.5891403177412622982 ) ) ;
#143516 = CARTESIAN_POINT ( 'NONE',  ( 2.594135478747404022, 0.9273930874063830432, -1.728848471177657942 ) ) ;
#143515 = CARTESIAN_POINT ( 'NONE',  ( -5.371001409308059138, 9.417918744168066070, -0.7998128361456231517 ) ) ;
#143517 = CARTESIAN_POINT ( 'NONE',  ( 1.587033755777764510, -0.3173376132806354222, -2.138153673666403964 ) ) ;
#143518 = CIRCLE ( 'NONE', #84547, 0.08000000000000012657 ) ;
#143520 = CARTESIAN_POINT ( 'NONE',  ( -6.126358594793636314, 6.003181085514223803, -0.2003443317756918585 ) ) ;
#143519 = CARTESIAN_POINT ( 'NONE',  ( -4.599959256786493533, 8.588645909551377855, 0.000000000000000000 ) ) ;
#143521 = CARTESIAN_POINT ( 'NONE',  ( 1.364683531249986537, 1.905208333674750287, -0.7879004041258239610 ) ) ;
#143522 = CARTESIAN_POINT ( 'NONE',  ( 2.987300135396570688, 1.631410314640189929, 0.5874552976607245736 ) ) ;
#143523 = CARTESIAN_POINT ( 'NONE',  ( 2.167524683544871600, -1.071679988950867024, 1.371128027196461208 ) ) ;
#143524 = CARTESIAN_POINT ( 'NONE',  ( 7.348156068926750883, 8.635565504245116486, -1.082531754730537976 ) ) ;
#143525 = CARTESIAN_POINT ( 'NONE',  ( -11.04445182892037813, 5.143275749589305335, -4.203165840917552742 ) ) ;
#143526 = EDGE_CURVE ( 'NONE', #52099, #162079, #62325, .T. ) ;
#143527 = CARTESIAN_POINT ( 'NONE',  ( 6.925078400183549476, 6.033022220673083247, 2.839235739982972184 ) ) ;
#143528 = CARTESIAN_POINT ( 'NONE',  ( -5.144392941742557568, 4.966489618313220333, -0.7998128361456362523 ) ) ;
#143529 = CARTESIAN_POINT ( 'NONE',  ( 1.516417288619626769, 1.325465413702779482, -1.459542524610158098 ) ) ;
#143530 = COLOUR_RGB ( '', 0.31764706, 0.68627451, 0.89019608) ;
#143532 = CARTESIAN_POINT ( 'NONE',  ( -5.804299160426242388, 6.904675454319632699, -1.082531754730549967 ) ) ;
#143531 = CARTESIAN_POINT ( 'NONE',  ( 5.994389040191065554, -1.017321598621454548, 1.619163160827830517 ) ) ;
#143533 = CARTESIAN_POINT ( 'NONE',  ( -5.763624699140883934, 6.857221916153382502, -1.082531754730549967 ) ) ;
#143534 = CARTESIAN_POINT ( 'NONE',  ( 5.363132282657546490, 8.414682208812571673, -1.199719254218452047 ) ) ;
#143536 = ADVANCED_FACE ( 'NONE', ( #52570 ), #87204, .F. ) ;
#143535 = AXIS2_PLACEMENT_3D ( 'NONE', #122419, #9627, #28016 ) ;
#143537 = CARTESIAN_POINT ( 'NONE',  ( -5.607179047703544583, 8.699403434699558346, 1.199719254218454489 ) ) ;
#143538 = CARTESIAN_POINT ( 'NONE',  ( 1.471359524643547134, -1.733428207583002756, -1.036219422855472194 ) ) ;
#143539 = CARTESIAN_POINT ( 'NONE',  ( 2.007420792093927986E-08, -6.938893903907228378E-15, -1.225000000000033396 ) ) ;
#143540 = CARTESIAN_POINT ( 'NONE',  ( 6.106511577925135548, -0.8227651472764373475, -2.156109995086146647 ) ) ;
#143541 = CARTESIAN_POINT ( 'NONE',  ( 6.408651779211167465, 0.6141799454031526828, 1.863335524608072502 ) ) ;
#143542 = CARTESIAN_POINT ( 'NONE',  ( 2.905073028004667712, -1.633678134795817360, 1.085783093053994453 ) ) ;
#143543 = CARTESIAN_POINT ( 'NONE',  ( 7.910292558569346433, 11.31609285405122556, -1.199719254218446718 ) ) ;
#143544 = CARTESIAN_POINT ( 'NONE',  ( 0.9498425221252141393, -1.824119990893595888, -0.8596288560165298298 ) ) ;
#143545 = VERTEX_POINT ( 'NONE', #132794 ) ;
#143546 = CARTESIAN_POINT ( 'NONE',  ( 0.9544967768389999163, -1.338301201188813572, 1.640804622059524043 ) ) ;
#143548 = CARTESIAN_POINT ( 'NONE',  ( -6.672584156219988571, 10.93643194889866521, -0.7998128361456291469 ) ) ;
#143547 = CARTESIAN_POINT ( 'NONE',  ( -3.598799709423620374, 6.286017863381107240, 1.199719254218464037 ) ) ;
#143549 = CARTESIAN_POINT ( 'NONE',  ( 2.501689010688646242, -0.7045654096689784041, -1.701190496055771550 ) ) ;
#143550 = ORIENTED_EDGE ( 'NONE', *, *, #26050, .F. ) ;
#143551 = CARTESIAN_POINT ( 'NONE',  ( 11.27771153926699377, 8.828701344599535261, -4.118830345813656812 ) ) ;
#143552 = CARTESIAN_POINT ( 'NONE',  ( 2.478903650112133317, -1.459102030866548994, 1.539066919819010781 ) ) ;
#143553 = CARTESIAN_POINT ( 'NONE',  ( -0.7500000000000215383, 3.972916667349481123, 1.299038105676671107 ) ) ;
#143554 = CARTESIAN_POINT ( 'NONE',  ( 7.426115451983150706, 9.686887332112256388, -1.599625672291262513 ) ) ;
#143555 = CARTESIAN_POINT ( 'NONE',  ( 6.933015448541703485, 9.181880338089085214, 1.599625672291268286 ) ) ;
#143556 = CARTESIAN_POINT ( 'NONE',  ( 2.899741356312244722, -0.6498117751948685461, 1.955694574617524495 ) ) ;
#143558 = CARTESIAN_POINT ( 'NONE',  ( 0.7316835000789992938, 1.813914744281470925, 0.3150931809976220133 ) ) ;
#143557 = CARTESIAN_POINT ( 'NONE',  ( -6.503107236049161521, 10.73870887536603291, 0.7998128361456481317 ) ) ;
#143559 = CARTESIAN_POINT ( 'NONE',  ( -1.364683531249997417, 4.759375000341424133, 1.214306433183764966E-14 ) ) ;
#143560 = CARTESIAN_POINT ( 'NONE',  ( -0.02224634325200240681, 0.6689394325187210111, -2.369055395299427769 ) ) ;
#143561 = CARTESIAN_POINT ( 'NONE',  ( 1.355678468426070982, 3.764857968299145430, 0.6419787906858488435 ) ) ;
#143562 =( BOUNDED_CURVE ( )  B_SPLINE_CURVE ( 2, ( #197310, #94516, #78233, #96652, #144356, #47907, #213539 ),
 .UNSPECIFIED., .F., .T. ) 
 B_SPLINE_CURVE_WITH_KNOTS ( ( 3, 2, 2, 3 ),
 ( 0.1375000000000000111, 0.1416666666666667462, 0.1458333333333334814, 0.1500000000000002165 ),
 .UNSPECIFIED. ) 
 CURVE ( )  GEOMETRIC_REPRESENTATION_ITEM ( )  RATIONAL_B_SPLINE_CURVE ( ( 1.000000000000000000, 0.8660254037844387076, 1.000000000000000000, 0.8660254037844387076, 1.000000000000000000, 0.8660254037844316022, 1.000000000000007105 ) ) 
 REPRESENTATION_ITEM ( '' )  );
#143563 = CARTESIAN_POINT ( 'NONE',  ( 0.3115100037339203487, 1.922317768103290803, 1.083863418116323807 ) ) ;
#143564 = CARTESIAN_POINT ( 'NONE',  ( 2.425404053729601550, -0.002036344795489434568, 2.262578821637390547 ) ) ;
#143565 = CARTESIAN_POINT ( 'NONE',  ( -9.991996023591624976, 10.75967623705280296, 1.040834085586084257E-14 ) ) ;
#143567 = ADVANCED_FACE ( 'NONE', ( #103458 ), #77872, .T. ) ;
#143566 = CARTESIAN_POINT ( 'NONE',  ( 2.460951123861610412, -1.504080979915609628, 1.009397298678058164 ) ) ;
#143568 = CARTESIAN_POINT ( 'NONE',  ( 3.081152777801674958, 1.513245778044673306, 1.174690267158661872 ) ) ;
#143569 = CARTESIAN_POINT ( 'NONE',  ( 4.738769824615551407, -2.007376682328159134, -0.5062664373569197851 ) ) ;
#143570 = CARTESIAN_POINT ( 'NONE',  ( -0.6823417656250212460, 2.363541667008084435, 1.181850606188767472 ) ) ;
#143571 = CARTESIAN_POINT ( 'NONE',  ( 2.061341786089391004, 0.3389245507335619245, -1.941969530725436766 ) ) ;
#143572 = CARTESIAN_POINT ( 'NONE',  ( 0.4461525089796612997, 1.920980128883168714, 0.1452595308072956448 ) ) ;
#143573 = CARTESIAN_POINT ( 'NONE',  ( 2.781945002432617997, -0.9632652739061451364, 1.603442845774772474 ) ) ;
#143575 = CARTESIAN_POINT ( 'NONE',  ( 4.672271667806711548, 8.395315985019093930, 0.5582388282892002396 ) ) ;
#143574 = CARTESIAN_POINT ( 'NONE',  ( 2.561488099217507308, -2.008522245525693695, -1.136227173556729975 ) ) ;
#143576 = CARTESIAN_POINT ( 'NONE',  ( 2.822522581191502677, -1.285663882657582580, 1.345810825326615223 ) ) ;
#143577 = CARTESIAN_POINT ( 'NONE',  ( -1.201851678989727383E-14, 3.196875000341420137, -1.575800808251660134 ) ) ;
#143578 = CARTESIAN_POINT ( 'NONE',  ( 6.338341894567316892, -1.106718111279564543, 1.740473967980406655 ) ) ;
#143579 = CARTESIAN_POINT ( 'NONE',  ( -3.086452525405351643, 6.752611712948207057, 0.7998128361456341429 ) ) ;
#143580 = CARTESIAN_POINT ( 'NONE',  ( 7.122110765880372618, 7.203550736482235095, 0.7998128361456341429 ) ) ;
#143581 = CARTESIAN_POINT ( 'NONE',  ( -1.409285775387294715, 3.485450175183121946, 0.5173959003036648907 ) ) ;
#143582 = CARTESIAN_POINT ( 'NONE',  ( 0.2058769709349675681, -0.5595275159893696726, 2.030311192619388638 ) ) ;
#143583 = ADVANCED_FACE ( 'NONE', ( #139169 ), #8079, .F. ) ;
#143584 = CARTESIAN_POINT ( 'NONE',  ( -1.201851678989727383E-14, 4.259375000341417028, -1.575800808251660134 ) ) ;
#143585 = CARTESIAN_POINT ( 'NONE',  ( 5.624359561864977763, 1.292596479719224645, -1.732379065785584871 ) ) ;
#143586 = CARTESIAN_POINT ( 'NONE',  ( 6.516272353977101695, -2.019191618876531091, 0.05163682429563941356 ) ) ;
#143587 = CARTESIAN_POINT ( 'NONE',  ( -0.6823417656250003738, -1.032291666325242607, -1.181850606188749264 ) ) ;
#143588 = CARTESIAN_POINT ( 'NONE',  ( -5.260200412422220140, 5.239248024021764039, -0.7216878364870207285 ) ) ;
#143589 = ADVANCED_FACE ( 'NONE', ( #71994 ), #204116, .T. ) ;
#143592 = CARTESIAN_POINT ( 'NONE',  ( 5.341549334104194635, 6.294524313618772737, 1.082531754730558626 ) ) ;
#143591 = CARTESIAN_POINT ( 'NONE',  ( 0.000000000000000000, -0.8968749995220406390, -3.793834371823813001 ) ) ;
#143590 = CARTESIAN_POINT ( 'NONE',  ( 6.496291879603339758, 7.608037276739255006, 1.199719254218452935 ) ) ;
#143593 = CARTESIAN_POINT ( 'NONE',  ( -9.367496997901325173, 14.48154074412966175, -7.499999999620646562 ) ) ;
#143594 = CARTESIAN_POINT ( 'NONE',  ( 4.417204035549080920, -1.841734835922325120, 0.8216704330437707426 ) ) ;
#143595 = CARTESIAN_POINT ( 'NONE',  ( -6.828502922777144768, 11.11833717654868892, 0.7998128361456481317 ) ) ;
#143597 = CARTESIAN_POINT ( 'NONE',  ( -6.414416072596845986, 8.576847732820027659, -1.443375672974066548 ) ) ;
#143596 = CARTESIAN_POINT ( 'NONE',  ( -9.056483424248693126, 10.62861408545402675, 1.082531754730558626 ) ) ;
#143598 = CARTESIAN_POINT ( 'NONE',  ( 4.941190227301914817, 4.729419784799151927, -0.4099107353478681492 ) ) ;
#143600 = CARTESIAN_POINT ( 'NONE',  ( -1.364683531250010740, 9.630208333674735499, 0.7879004041258445001 ) ) ;
#143599 = CARTESIAN_POINT ( 'NONE',  ( 6.262596564776618635, -1.532251275270900326, 1.525113613579494709 ) ) ;
#143601 = DIRECTION ( 'NONE',  ( 0.000000000000000000, 0.000000000000000000, 1.000000000000000000 ) ) ;
#143602 = CARTESIAN_POINT ( 'NONE',  ( -9.541187415715041809, 12.15447128979948310, -1.599625672291263179 ) ) ;
#143604 = CARTESIAN_POINT ( 'NONE',  ( 0.3685665480608457667, -0.2352240095614567816, -1.901051784579368187 ) ) ;
#143603 = CARTESIAN_POINT ( 'NONE',  ( -6.846504384776765484, 8.050305206070113684, -1.082531754730543083 ) ) ;
#143605 = CARTESIAN_POINT ( 'NONE',  ( -0.6823417656250246877, 0.3635416670080895973, 1.181850606188755259 ) ) ;
#143606 = CARTESIAN_POINT ( 'NONE',  ( 1.445103857048100515, 8.688264192037886247, 2.625611233228254182 ) ) ;
#143607 = CARTESIAN_POINT ( 'NONE',  ( 1.963112949512689553, 0.2966733001828375516, -1.698991974238444946 ) ) ;
#143608 = CARTESIAN_POINT ( 'NONE',  ( 2.898410978271408922, 6.603506251283770112, -0.7998128361456362523 ) ) ;
#143609 = CARTESIAN_POINT ( 'NONE',  ( 5.397027666691686321, 8.454226823519094935, 1.199719254218451159 ) ) ;
#143610 = CARTESIAN_POINT ( 'NONE',  ( -11.16739129266794350, 7.275426543628465303, -4.398590771924178355 ) ) ;
#143611 = CARTESIAN_POINT ( 'NONE',  ( 1.422737370818322633, -0.05026339470881428795, 1.769212045163440106 ) ) ;
#143612 = CARTESIAN_POINT ( 'NONE',  ( 1.559240971068908355, -1.699445492770943478, 1.078823074066703747 ) ) ;
#143613 = CARTESIAN_POINT ( 'NONE',  ( -5.608478439449225306, 5.609308656285654671, -0.4224404339892348093 ) ) ;
#143614 = CARTESIAN_POINT ( 'NONE',  ( 3.856632026064894525, 0.7917978285330304900, 2.060012427959257764 ) ) ;
#143615 = CARTESIAN_POINT ( 'NONE',  ( 5.155217109558853039, 1.808899791667990753, -1.200326510068568497 ) ) ;
#143616 = VERTEX_POINT ( 'NONE', #55768 ) ;
#143617 = CARTESIAN_POINT ( 'NONE',  ( -0.7500000000000006661, -0.3916666666666443475, -1.299038105676652011 ) ) ;
#143618 = CARTESIAN_POINT ( 'NONE',  ( 9.056483423804305488, 9.668244870634271848, 1.040834085586084257E-14 ) ) ;
#143620 = CARTESIAN_POINT ( 'NONE',  ( 2.776970437579088014, 1.727991955821889025, -1.039012595151635354 ) ) ;
#143619 = CARTESIAN_POINT ( 'NONE',  ( 3.651137946248568689, 0.3127203024623700367, 2.097190470537732221 ) ) ;
#143622 = ORIENTED_EDGE ( 'NONE', *, *, #189993, .F. ) ;
#143621 = CARTESIAN_POINT ( 'NONE',  ( 3.058660868685322498, 0.4446918012569016643, 1.755998500949424113 ) ) ;
#143623 = CARTESIAN_POINT ( 'NONE',  ( 5.037736595929563244, 8.035053907629919223, -1.199719254218452047 ) ) ;
#143624 = ORIENTED_EDGE ( 'NONE', *, *, #128773, .T. ) ;
#143625 = CARTESIAN_POINT ( 'NONE',  ( -10.91970695577496997, -5.907420853759282053, 5.204170427930421283E-15 ) ) ;
#143626 = AXIS2_PLACEMENT_3D ( 'NONE', #123502, #42174, #108290 ) ;
#143627 = CARTESIAN_POINT ( 'NONE',  ( 5.311043488251262268, 7.219303374425030562, -1.599625672291256295 ) ) ;
#143628 = CARTESIAN_POINT ( 'NONE',  ( 5.971303284387838417, 0.1295235881030691594, -1.821162830480331563 ) ) ;
#143630 = CARTESIAN_POINT ( 'NONE',  ( 0.9541331885446997507, -1.212804274533643145, 1.482964625430952976 ) ) ;
#143629 = CARTESIAN_POINT ( 'NONE',  ( -3.079673448598517549, 6.744702790006905424, 1.040834085586084257E-14 ) ) ;
#143631 = CARTESIAN_POINT ( 'NONE',  ( -9.409940793360268785, 3.999985931113709814, -6.919963696468023784 ) ) ;
#143632 = CARTESIAN_POINT ( 'NONE',  ( 1.499999999999822586, 7.388542872122531691, 4.154462424328221104 ) ) ;
#143633 = CIRCLE ( 'NONE', #63959, 0.08000000000000012657 ) ;
#143634 = CARTESIAN_POINT ( 'NONE',  ( -1.364683531250000748, 1.071875000341421247, 0.000000000000000000 ) ) ;
#143635 = DIRECTION ( 'NONE',  ( 5.578564026256490882E-16, 1.000000000000000000, 9.066213480720158442E-32 ) ) ;
#143636 = CARTESIAN_POINT ( 'NONE',  ( -7.537443334193545397, 10.88110209227943770, -1.199719254218446718 ) ) ;
#143637 = ORIENTED_EDGE ( 'NONE', *, *, #4338, .T. ) ;
#143638 = CARTESIAN_POINT ( 'NONE',  ( 5.172814640947125397, -2.034155943344346795, -0.7319064324283753864 ) ) ;
#143639 = CARTESIAN_POINT ( 'NONE',  ( -5.316205630334263965, 7.295602216847000498, -1.443375672974066548 ) ) ;
#143640 = CARTESIAN_POINT ( 'NONE',  ( -6.400331034103001748, 9.624747418832267698, 1.199719254218452935 ) ) ;
#143641 = CARTESIAN_POINT ( 'NONE',  ( 2.900754761704402274, -2.089926006748676457, -0.3584049868644647585 ) ) ;
#143643 = CARTESIAN_POINT ( 'NONE',  ( -11.47199464713663453, 5.776720398841780124, 5.393175811422019628 ) ) ;
#143642 = FACE_OUTER_BOUND ( 'NONE', #109429, .T. ) ;
#143644 = CARTESIAN_POINT ( 'NONE',  ( 4.042224286460029958, 1.961553563453529492, 0.1965975345302218569 ) ) ;
#143645 = CARTESIAN_POINT ( 'NONE',  ( 0.1936082253880376802, 1.876963271429439750, -0.7284200309826213138 ) ) ;
#143646 = ORIENTED_EDGE ( 'NONE', *, *, #89086, .F. ) ;
#143647 = CARTESIAN_POINT ( 'NONE',  ( 5.928941916292417957, -1.787427330561262906, 1.134758347235584885 ) ) ;
#143648 = CARTESIAN_POINT ( 'NONE',  ( 0.4849360239999983557, 1.980737741294085419, 0.6024896509310638804 ) ) ;
#143649 = CARTESIAN_POINT ( 'NONE',  ( 2.238135065718354078, 0.4255327557451081266, 1.894600943326588238 ) ) ;
#143650 = ORIENTED_EDGE ( 'NONE', *, *, #181542, .F. ) ;
#143651 = CARTESIAN_POINT ( 'NONE',  ( 2.325000000000005063, 0.000000000000000000, -0.5000000000000004441 ) ) ;
#143652 = CARTESIAN_POINT ( 'NONE',  ( 5.365994935958575240, 9.482354201918870018, 0.7998128361456341429 ) ) ;
#143654 = CARTESIAN_POINT ( 'NONE',  ( 5.632522751473472589, 8.658694745772667289, -1.199719254218440723 ) ) ;
#143653 = CARTESIAN_POINT ( 'NONE',  ( 3.169954053886741008, -1.245012139812958996, 1.679338519663716500 ) ) ;
#143656 = EDGE_CURVE ( 'NONE', #141526, #102037, #188905, .T. ) ;
#143655 = CARTESIAN_POINT ( 'NONE',  ( 4.055297343818933697, 5.824542549245813383, 1.443375672974058777 ) ) ;
#143658 = VERTEX_POINT ( 'NONE', #172739 ) ;
#143657 = CARTESIAN_POINT ( 'NONE',  ( 0.8733459280946423986, 0.3543511941397787801, -1.776278655377810489 ) ) ;
#143659 = CARTESIAN_POINT ( 'NONE',  ( 5.268293329372571776, 1.085216321637239023, 1.921556908365213312 ) ) ;
#143660 = CARTESIAN_POINT ( 'NONE',  ( 5.346851039111009563, 6.199209027673978412, 2.419999999999999485 ) ) ;
#143661 = CARTESIAN_POINT ( 'NONE',  ( 2.714145368365259436, -2.182908968410116834, 0.3227909207665635716 ) ) ;
#143662 = CARTESIAN_POINT ( 'NONE',  ( 7.086107841436786181, 11.41887624831828418, 1.040834085586084257E-14 ) ) ;
#143663 = DIRECTION ( 'NONE',  ( -0.6507913734559658270, -0.7592566023652989049, 0.000000000000000000 ) ) ;
#143664 = CARTESIAN_POINT ( 'NONE',  ( 2.156764536687346467, 0.4205103164258168769, 1.865301821287323136 ) ) ;
#143665 = CARTESIAN_POINT ( 'NONE',  ( 7.723341061279088038, 12.16231500480096983, -0.7998128361456291469 ) ) ;
#143666 = CARTESIAN_POINT ( 'NONE',  ( 5.037584538744971141, 1.933038169019934527, -0.7419538039311264210 ) ) ;
#143667 = CIRCLE ( 'NONE', #70906, 0.2999999999999999334 ) ;
#143669 = CARTESIAN_POINT ( 'NONE',  ( 3.397504326804317909, 1.702965868850464082, 1.331369057855802174 ) ) ;
#143668 = CARTESIAN_POINT ( 'NONE',  ( 1.538487831126108762, 8.695753106490483830, -2.511613306591210293 ) ) ;
#143670 = CARTESIAN_POINT ( 'NONE',  ( 4.405938146338868933, -0.9375679901368579872, -1.981035393479456008 ) ) ;
#143671 = ORIENTED_EDGE ( 'NONE', *, *, #33554, .T. ) ;
#143672 = CARTESIAN_POINT ( 'NONE',  ( 8.886479618753304166, 12.45497775759917758, -1.199719254218446718 ) ) ;
#143673 = DIRECTION ( 'NONE',  ( 2.220446049250312341E-16, -1.000000000000000000, 0.000000000000000000 ) ) ;
#143674 = CARTESIAN_POINT ( 'NONE',  ( -3.104766810201186278, 15.44820807305922195, 11.55390834459370097 ) ) ;
#143675 = CARTESIAN_POINT ( 'NONE',  ( 6.886615681098613884, 6.999082814228660077, 0.000000000000000000 ) ) ;
#143676 = CARTESIAN_POINT ( 'NONE',  ( -1.364683531250014514, 15.40104166700806765, -0.7879004041258335089 ) ) ;
#143677 = CARTESIAN_POINT ( 'NONE',  ( 0.000000000000000000, 3.799999999999998046, 0.000000000000000000 ) ) ;
#143678 = CARTESIAN_POINT ( 'NONE',  ( 0.4225002777262388265, -1.427939226333583500, -1.423959630194884696 ) ) ;
#143680 = CARTESIAN_POINT ( 'NONE',  ( -7.971831135155409420, 11.28392484344787405, 1.082531754730549967 ) ) ;
#143679 = VECTOR ( 'NONE', #139608, 1000.000000000000000 ) ;
#143681 = CARTESIAN_POINT ( 'NONE',  ( 5.306037014901791693, 7.283738832175834510, 1.599625672291269396 ) ) ;
#143682 = CARTESIAN_POINT ( 'NONE',  ( 6.315297747118990834, -1.772576088781053327, -1.069364167438614732 ) ) ;
#143683 = CARTESIAN_POINT ( 'NONE',  ( 4.635331898966036590, -1.760702172612697458, 0.7822757977788937778 ) ) ;
#143684 = CARTESIAN_POINT ( 'NONE',  ( 0.3511856949766634095, 0.1948183440376727305, -2.006963311255556714 ) ) ;
#143685 = CARTESIAN_POINT ( 'NONE',  ( -1.040834085586084257E-14, -6.796015482748913428, 10.25773349932951461 ) ) ;
#143686 = CARTESIAN_POINT ( 'NONE',  ( 6.159481859310094620, 6.080483678816896109, 1.040834085586084257E-14 ) ) ;
#143687 = CARTESIAN_POINT ( 'NONE',  ( 0.4019237886466847653, 13.07366454968462932, 1.499999999999997113 ) ) ;
#143688 = CARTESIAN_POINT ( 'NONE',  ( 3.590635625024854338, 1.920399590389043620, 0.4359694148904534328 ) ) ;
#143689 = CARTESIAN_POINT ( 'NONE',  ( 0.4104466507391414387, 1.508250410577081979, -1.590083307377434974 ) ) ;
#143690 = CARTESIAN_POINT ( 'NONE',  ( 3.580510235063854019, -1.759844519496515325, -0.4856381957471164745 ) ) ;
#143691 = AXIS2_PLACEMENT_3D ( 'NONE', #117348, #116278, #210775 ) ;
#143692 = CARTESIAN_POINT ( 'NONE',  ( 7.349928672384120176, 7.747540670635879145, 0.7216878364870267237 ) ) ;
#143693 = CARTESIAN_POINT ( 'NONE',  ( 3.619663824724254741, 6.206396314611513532, -1.082531754730543971 ) ) ;
#143694 = CARTESIAN_POINT ( 'NONE',  ( -6.119526231721793330, 8.232809585132461194, 1.599625672291263179 ) ) ;
#143695 = CARTESIAN_POINT ( 'NONE',  ( 5.415556014015861841, 5.282846535965431300, -0.7998128361456481317 ) ) ;
#143696 = ORIENTED_EDGE ( 'NONE', *, *, #3649, .F. ) ;
#143698 = CARTESIAN_POINT ( 'NONE',  ( 4.904545999335794271, -1.998481532559828189, -0.2423253454618880809 ) ) ;
#143697 = CARTESIAN_POINT ( 'NONE',  ( 1.891909123491273492, -0.4922293657834125313, -1.774144672653771293 ) ) ;
#143699 = CARTESIAN_POINT ( 'NONE',  ( 0.6678281019706671096, -0.7765434158916887375, -2.163364592831273470 ) ) ;
#143700 = CARTESIAN_POINT ( 'NONE',  ( 5.190269257085567745, 1.011813749630154691, -1.680575076195559792 ) ) ;
#143701 = CARTESIAN_POINT ( 'NONE',  ( -4.934277840369690971, 7.844075682818238526, -1.199719254218452047 ) ) ;
#143702 = DIRECTION ( 'NONE',  ( -5.551115123125764829E-17, 0.000000000000000000, 1.000000000000000000 ) ) ;
#143703 = CARTESIAN_POINT ( 'NONE',  ( -2.923754682041362241, 6.562797562356882608, 0.7998128361456341429 ) ) ;
#143704 = CARTESIAN_POINT ( 'NONE',  ( 0.2388460773940295212, -2.007853281042128568, -0.5044432775610437902 ) ) ;
#143705 = CARTESIAN_POINT ( 'NONE',  ( -4.930325137224961907, 5.781076077297750970, -1.199719254218453823 ) ) ;
#143707 = CARTESIAN_POINT ( 'NONE',  ( 6.737169288263022082, -1.578518636041785994, 0.8004799088773879578 ) ) ;
#143706 = CARTESIAN_POINT ( 'NONE',  ( 1.294599682487684422, 1.707161730183017534, -1.206694161613943272 ) ) ;
#143708 = CARTESIAN_POINT ( 'NONE',  ( -8.917737905728749581, 3.038492715500545671, -8.029567276306263324 ) ) ;
#143709 = CARTESIAN_POINT ( 'NONE',  ( -0.2104748580754201015, 5.720428293583295520, -2.697747842008205943 ) ) ;
#143710 = CARTESIAN_POINT ( 'NONE',  ( 1.979654113181174901, -1.706931329119738772, -0.3388794841660112689 ) ) ;
#143711 = CARTESIAN_POINT ( 'NONE',  ( 6.471319392424407901, 6.444294134116939077, 0.7998128361456341429 ) ) ;
#143713 = CARTESIAN_POINT ( 'NONE',  ( 11.33772463945037146, 12.69999999999998153, 3.679999999999999272 ) ) ;
#143712 = CYLINDRICAL_SURFACE ( 'NONE', #141435, 0.09999999999999971412 ) ;
#143714 = CARTESIAN_POINT ( 'NONE',  ( 1.611479353654057034, -1.712177798104688620, 0.2083697849032482008 ) ) ;
#143715 = CARTESIAN_POINT ( 'NONE',  ( 1.927518781310177509, -1.434474475899261581, -1.656937093973806396 ) ) ;
#143716 = CARTESIAN_POINT ( 'NONE',  ( 3.756632125300945368, 0.7937082651479386852, 2.059386989456575279 ) ) ;
#143717 = CARTESIAN_POINT ( 'NONE',  ( 4.000000000000001776, -3.469446951953614189E-15, -2.024999999999994582 ) ) ;
#143718 = CARTESIAN_POINT ( 'NONE',  ( 3.028372864778381413, 1.157752252206078358, 1.836431199091348665 ) ) ;
#143719 = CARTESIAN_POINT ( 'NONE',  ( 1.594096589105632011, -1.816728215151931058, -0.1805768397986490248 ) ) ;
#143720 = CARTESIAN_POINT ( 'NONE',  ( 2.940728227222836111, -1.600293368184166898, 1.386485470145684351 ) ) ;
#143721 = CARTESIAN_POINT ( 'NONE',  ( 6.539320575229279342, 6.038407674219216759, 2.491644695858772796 ) ) ;
#143722 = ORIENTED_EDGE ( 'NONE', *, *, #214235, .T. ) ;
#143724 = CARTESIAN_POINT ( 'NONE',  ( 0.6823417656249899377, 0.9052083336747520637, 1.181850606188755259 ) ) ;
#143723 = CARTESIAN_POINT ( 'NONE',  ( 3.685359659257981146, 1.661040094275951340, 1.580089079255690088 ) ) ;
#143725 = CARTESIAN_POINT ( 'NONE',  ( 0.07755575628183573877, 1.325091491099144259, -2.441202027401535357 ) ) ;
#143726 = CARTESIAN_POINT ( 'NONE',  ( 2.706824224222692088, 6.309712028235118453, 0.7998128361456362523 ) ) ;
#143727 = CARTESIAN_POINT ( 'NONE',  ( 6.533822986070857652, -2.155494434802426973, 0.5362405526610786177 ) ) ;
#143728 = CARTESIAN_POINT ( 'NONE',  ( -7.700668062882084719, 8.086460282891644979, -0.7216878364870278340 ) ) ;
#143729 = ADVANCED_FACE ( 'NONE', ( #70923 ), #57905, .F. ) ;
#143730 = CARTESIAN_POINT ( 'NONE',  ( 3.877268743828258479, 7.467304601200877023, 0.7216878364870298324 ) ) ;
#143731 = AXIS2_PLACEMENT_3D ( 'NONE', #132316, #68315, #66169 ) ;
#143732 = CARTESIAN_POINT ( 'NONE',  ( -7.022760381754429737, 7.295567988242705582, 1.040834085586084257E-14 ) ) ;
#143733 = CARTESIAN_POINT ( 'NONE',  ( 6.825078400183548055, 2.461594334264828987, 2.239602747093616841 ) ) ;
#143734 = ORIENTED_EDGE ( 'NONE', *, *, #209881, .F. ) ;
#143735 = CARTESIAN_POINT ( 'NONE',  ( 3.850232551101365086, 0.2440307281281335616, -2.001511205109906655 ) ) ;
#143737 = CARTESIAN_POINT ( 'NONE',  ( 2.500897397093455155, 0.4475292293845704594, 2.013297154094250807 ) ) ;
#143736 = CARTESIAN_POINT ( 'NONE',  ( 6.287230548435207567, 8.358188277972981695, -1.599625672291262513 ) ) ;
#143738 = CARTESIAN_POINT ( 'NONE',  ( 6.750000000000007994, 7.629137130509070275, 2.600000000000001421 ) ) ;
#143739 = CARTESIAN_POINT ( 'NONE',  ( 3.390947816749319443, 6.970206529600588397, -1.734723475976807094E-15 ) ) ;
#143740 = CARTESIAN_POINT ( 'NONE',  ( 0.000000000000000000, -2.996874999522043392, -3.793834371823813001 ) ) ;
#143741 = CARTESIAN_POINT ( 'NONE',  ( -0.6823417656250212460, 5.551041667008087543, 1.181850606188767472 ) ) ;
#143742 = CARTESIAN_POINT ( 'NONE',  ( 5.630878078874809844, -1.982435003639994031, 0.9343296635366815650 ) ) ;
#143743 = CARTESIAN_POINT ( 'NONE',  ( 2.443982611291168450, -1.755769474653746665, -0.9913988478210812305 ) ) ;
#143744 = CARTESIAN_POINT ( 'NONE',  ( 2.384105128782065819, -0.3166398734758494315, -1.813660976904336808 ) ) ;
#143745 = CARTESIAN_POINT ( 'NONE',  ( 6.765682348419287173, 7.852049813699357728, 1.199719254218462483 ) ) ;
#143746 = CARTESIAN_POINT ( 'NONE',  ( 6.633835642106551411, -1.195214757176918496, -1.380038946949893486 ) ) ;
#143747 = CARTESIAN_POINT ( 'NONE',  ( 0.3351808223112633933, 0.7127874033420987798, -2.185478155228081754 ) ) ;
#143748 = CARTESIAN_POINT ( 'NONE',  ( -6.679363233026820446, 10.94434087183997129, 0.000000000000000000 ) ) ;
#143750 = CARTESIAN_POINT ( 'NONE',  ( -4.118644803501354978, 8.027112380718707030, 0.7998128361456352531 ) ) ;
#143749 = CARTESIAN_POINT ( 'NONE',  ( 5.454102184832422928, 2.260192964246518166, -0.1051519175162188013 ) ) ;
#143751 = CARTESIAN_POINT ( 'NONE',  ( 1.401149585966605882, 1.720815086091964652, -1.213930111015694369 ) ) ;
#143752 = CARTESIAN_POINT ( 'NONE',  ( -5.901542003698421190, 10.10715911428198055, 0.000000000000000000 ) ) ;
#143753 = CARTESIAN_POINT ( 'NONE',  ( 6.916630921265960019, 11.22115317478565188, 0.7998128361456462443 ) ) ;
#143754 = CARTESIAN_POINT ( 'NONE',  ( 7.363486825553451354, 8.723727730301414240, -1.082531754730548412 ) ) ;
#143755 = DIRECTION ( 'NONE',  ( 0.8516084350226855726, 0.000000000000000000, -0.5241784747566542446 ) ) ;
#143756 = CARTESIAN_POINT ( 'NONE',  ( -8.688077508258798431, 9.030511935923748013, -0.7998128361456291469 ) ) ;
#143757 = CARTESIAN_POINT ( 'NONE',  ( 7.453913518772580460, -5.212532583863424662, 8.072398248062489401 ) ) ;
#143758 = CARTESIAN_POINT ( 'NONE',  ( 6.927853306458739979, 10.06595070996845642, 1.082531754730558626 ) ) ;
#143759 = CARTESIAN_POINT ( 'NONE',  ( 4.260617097460324132, 7.265790484119571957, -0.9368387426427534637 ) ) ;
#143760 = CARTESIAN_POINT ( 'NONE',  ( -9.002250809794000830, 11.52571191622492464, -1.443375672974059665 ) ) ;
#143762 = CARTESIAN_POINT ( 'NONE',  ( 3.041495853084168921, 0.05845243686668395028, 2.220815690970390222 ) ) ;
#143761 = CARTESIAN_POINT ( 'NONE',  ( 1.775790443353560732, 0.3575140072833470906, -2.090081039791711337 ) ) ;
#143763 = CARTESIAN_POINT ( 'NONE',  ( 6.883263157960393563, 4.695771316066229772, 2.508818740863460572 ) ) ;
#143764 = CARTESIAN_POINT ( 'NONE',  ( -5.088052786878465739, 9.158088361325352977, 0.000000000000000000 ) ) ;
#143765 = CARTESIAN_POINT ( 'NONE',  ( 5.660692828905515839, 6.562895374266609849, -1.199719254218445830 ) ) ;
#143766 = CARTESIAN_POINT ( 'NONE',  ( 3.947668504265917644, 1.419370528949075005, 1.354593381527373186 ) ) ;
#143767 = CARTESIAN_POINT ( 'NONE',  ( 9.134442807305049428, 11.67993591332117376, 1.599625672291281386 ) ) ;
#143768 = CARTESIAN_POINT ( 'NONE',  ( -4.588080609115144703, 6.965600104441714180, 1.189663598451236926 ) ) ;
#143769 = CARTESIAN_POINT ( 'NONE',  ( 5.034155109375821446, 4.767602470560229122, -0.7998128361456221525 ) ) ;
#143770 = CARTESIAN_POINT ( 'NONE',  ( 0.6823417656249882723, 0.3427083336747516196, 1.181850606188755259 ) ) ;
#143771 = CARTESIAN_POINT ( 'NONE',  ( -4.014622883422329203, 6.737458226417744278, -1.082531754730546636 ) ) ;
#143773 = ORIENTED_EDGE ( 'NONE', *, *, #116113, .F. ) ;
#143772 = CARTESIAN_POINT ( 'NONE',  ( -6.073689629242151611, 10.02979563418376685, -0.7216878364870278340 ) ) ;
#143774 = CARTESIAN_POINT ( 'NONE',  ( 3.305043459179863419, -0.4174351347619070229, -2.078937965663613774 ) ) ;
#143775 = CARTESIAN_POINT ( 'NONE',  ( -4.716257332707368910, 6.595662536282280719, -1.599625672291271394 ) ) ;
#143776 = CARTESIAN_POINT ( 'NONE',  ( 4.645497774645744649, -1.668943667408796294, -1.373881373981879594 ) ) ;
#143777 = CARTESIAN_POINT ( 'NONE',  ( 4.300242120186610784, 1.420457692841030850, -1.171515996850613694 ) ) ;
#143778 = CARTESIAN_POINT ( 'NONE',  ( -5.108350220830032207, 6.531958715577594887, 1.215759808322430136 ) ) ;
#143779 = CARTESIAN_POINT ( 'NONE',  ( -1.364683531250000748, 0.3218750003414205807, 0.000000000000000000 ) ) ;
#143780 = CARTESIAN_POINT ( 'NONE',  ( 5.947135546971048292, 0.4987507408355364991, -1.667328318302605528 ) ) ;
#143781 = CARTESIAN_POINT ( 'NONE',  ( 1.499999999999989120, 3.303247596591511126, 0.1248075943439479751 ) ) ;
#143782 = CARTESIAN_POINT ( 'NONE',  ( 3.389175213736292047, 5.937492935125556315, 1.082531754730558626 ) ) ;
#143783 = CARTESIAN_POINT ( 'NONE',  ( -5.826449692766521693, 7.206545609186315815, -1.206671273860264515 ) ) ;
#143784 = CARTESIAN_POINT ( 'NONE',  ( 3.344745324850742385, 0.5235245934552492653, 2.097234944377385002 ) ) ;
#143785 = CARTESIAN_POINT ( 'NONE',  ( 5.378279760196133630, -0.2985789616767355326, 1.993766414912321316 ) ) ;
#143786 = CARTESIAN_POINT ( 'NONE',  ( -9.042925270190641740, 11.57316545335434199, 1.443375672974064550 ) ) ;
#143787 = CARTESIAN_POINT ( 'NONE',  ( 2.501032641837992454, 1.736685530831501456, -1.287010829427559289 ) ) ;
#143788 = CARTESIAN_POINT ( 'NONE',  ( 3.462146415373760444, 0.8834382129937996542, 1.762370924576799114 ) ) ;
#143789 = FILL_AREA_STYLE ('',( #125442 ) ) ;
#143790 = CARTESIAN_POINT ( 'NONE',  ( 4.370608360784649093, -0.003437861098648780072, -1.942234966449083000 ) ) ;
#143793 = VERTEX_POINT ( 'NONE', #125131 ) ;
#143792 =( NAMED_UNIT ( * ) PLANE_ANGLE_UNIT ( ) SI_UNIT ( $, .RADIAN. ) );
#143791 = CARTESIAN_POINT ( 'NONE',  ( -8.717529583462656717, 11.19353715217169309, 1.443375672974064550 ) ) ;
#143794 = CARTESIAN_POINT ( 'NONE',  ( -4.945692173934974178, 8.992000979557944973, 0.000000000000000000 ) ) ;
#143795 = CARTESIAN_POINT ( 'NONE',  ( 11.89321938400720491, 9.837447216393373495, 1.599605898944226334 ) ) ;
#143796 = EDGE_CURVE ( 'NONE', #147554, #72330, #23154, .T. ) ;
#143798 = EDGE_LOOP ( 'NONE', ( #45592, #74361, #23550, #52219 ) ) ;
#143797 = CARTESIAN_POINT ( 'NONE',  ( -5.517242166118370150, 5.401480380085008193, 0.7998128361456281477 ) ) ;
#143799 = CARTESIAN_POINT ( 'NONE',  ( -9.151390499099978371, 9.778969791812544443, 0.7216878364870438212 ) ) ;
#143800 = CARTESIAN_POINT ( 'NONE',  ( 1.923171073188837843, 2.059116738528983692, 0.7940920450543451636 ) ) ;
#143801 = CARTESIAN_POINT ( 'NONE',  ( 3.285556943749998737, -0.9552083328553737651, -1.896917185911906500 ) ) ;
#143802 = CARTESIAN_POINT ( 'NONE',  ( 6.508651776674191147, 0.6122461511635870490, 1.863871573545019533 ) ) ;
#143803 = CARTESIAN_POINT ( 'NONE',  ( 1.364683531249990311, 4.926041667008083991, 0.7879004041258500513 ) ) ;
#143804 = CARTESIAN_POINT ( 'NONE',  ( -0.7500000000000215383, 4.722916667349482012, 1.299038105676671107 ) ) ;
#143805 = CARTESIAN_POINT ( 'NONE',  ( 4.808669324434905690, 6.961940934708692019, -1.409791361277392241 ) ) ;
#143807 = CARTESIAN_POINT ( 'NONE',  ( -5.742041750587549842, 6.657802449562273850, 1.199719254218450271 ) ) ;
#143806 = CARTESIAN_POINT ( 'NONE',  ( 6.235036409211808461, 0.2120174297785166195, 2.196685143856290878 ) ) ;
#143808 = CARTESIAN_POINT ( 'NONE',  ( 5.033073903806924321, -1.304366766181121573, -1.299653785596634137 ) ) ;
#143809 = ORIENTED_EDGE ( 'NONE', *, *, #156015, .F. ) ;
#143810 = CARTESIAN_POINT ( 'NONE',  ( -5.758872628492444169E-14, -0.1718749996585747786, -1.570758158831818241 ) ) ;
#143811 = CARTESIAN_POINT ( 'NONE',  ( -6.669721502918952716, 9.868759955792373972, 1.199719254218452047 ) ) ;
#143812 = DIRECTION ( 'NONE',  ( 0.000000000000000000, 0.000000000000000000, -1.000000000000000000 ) ) ;
#143813 = CARTESIAN_POINT ( 'NONE',  ( 6.416280414004661203, -2.120105685773795212, 0.05337830808049835035 ) ) ;
#143814 = CARTESIAN_POINT ( 'NONE',  ( 11.79269373152572342, 6.877189549381032663, -1.951281263922989950 ) ) ;
#143815 = CARTESIAN_POINT ( 'NONE',  ( 6.173040012923759257, 6.096301524699504704, -0.7998128361456281477 ) ) ;
#143816 = CARTESIAN_POINT ( 'NONE',  ( 0.1982117360312448395, -2.060432452642831702, -0.05102901230808094130 ) ) ;
#143819 = CARTESIAN_POINT ( 'NONE',  ( 3.509164994824386596, -1.813400730843343966, 0.3181347684400454012 ) ) ;
#143818 = CARTESIAN_POINT ( 'NONE',  ( 1.961162895873772127, 1.544969826164013238, 1.037258533166736996 ) ) ;
#143817 = FILL_AREA_STYLE ('',( #11622 ) ) ;
#143820 = CARTESIAN_POINT ( 'NONE',  ( 6.337546739384100292, 9.481222731668410120, 1.199719254218460707 ) ) ;
#143821 = CARTESIAN_POINT ( 'NONE',  ( -9.088333505345289609, 15.51845924943720867, 7.848675090006571153 ) ) ;
#143822 = CARTESIAN_POINT ( 'NONE',  ( -5.284646014276622950, 9.387447126623207794, -0.7998128361456362523 ) ) ;
#143824 = ORIENTED_EDGE ( 'NONE', *, *, #39783, .F. ) ;
#143823 = DIRECTION ( 'NONE',  ( 0.000000000000000000, 0.000000000000000000, 1.000000000000000000 ) ) ;
#143825 = CARTESIAN_POINT ( 'NONE',  ( 3.545738602337618506, -1.670889076328873069, -1.441789439710974063 ) ) ;
#143826 = CARTESIAN_POINT ( 'NONE',  ( 5.852851842114176861, -1.788828801601877849, 1.385077142625196434 ) ) ;
#143827 = CARTESIAN_POINT ( 'NONE',  ( -6.887178846062128379, 7.137389529935019183, -0.7216878364870278340 ) ) ;
#143828 = CARTESIAN_POINT ( 'NONE',  ( 6.170143040141627289, 1.806061762467878751, -0.1426304505553182556 ) ) ;
#143829 = B_SPLINE_CURVE_WITH_KNOTS ( 'NONE', 3,
 ( #6411, #54126, #185166, #152686 ),
 .UNSPECIFIED., .F., .F.,
 ( 4, 4 ),
 ( 0.003282510000513595011, 0.004028258324140119966 ),
 .UNSPECIFIED. ) ;
#143830 = CARTESIAN_POINT ( 'NONE',  ( -0.2351498743046881446, -0.1506043639611966134, -1.983733596389973597 ) ) ;
#143831 = CARTESIAN_POINT ( 'NONE',  ( -4.566062713072708057, 5.367758147946414482, 1.229400682838634573 ) ) ;
#143832 = CARTESIAN_POINT ( 'NONE',  ( 6.491075539335432687, 1.626419376453295706, -0.9240138038444989377 ) ) ;
#143833 = CARTESIAN_POINT ( 'NONE',  ( 6.041656841763191288, -1.799011877964010520, 0.6487133288125003228 ) ) ;
#143834 = DIRECTION ( 'NONE',  ( 0.6507913734559640506, -0.7592566023653004592, 0.000000000000000000 ) ) ;
#143835 = CARTESIAN_POINT ( 'NONE',  ( 1.006479672118578916, 1.419055151971573059, -1.218976214888117804 ) ) ;
#143836 = COLOUR_RGB ( '', 0.31764706, 0.68627451, 0.89019608) ;
#143837 = CARTESIAN_POINT ( 'NONE',  ( 1.569546381206438967, 1.394087592100446971, 1.457234012747665508 ) ) ;
#143839 = CARTESIAN_POINT ( 'NONE',  ( 4.336618311946851101, 2.065336219181472366, 0.4112933666130594301 ) ) ;
#143838 = CARTESIAN_POINT ( 'NONE',  ( -8.533967624797991647, 12.04371376465130439, -1.199719254218446718 ) ) ;
#143840 = ADVANCED_FACE ( 'NONE', ( #178072 ), #12342, .F. ) ;
#143841 = CARTESIAN_POINT ( 'NONE',  ( 8.422639742587595180, 10.84949900448412130, -1.599625672291268286 ) ) ;
#143843 = CARTESIAN_POINT ( 'NONE',  ( -7.991641480251377772, 11.41099992934688956, 1.199719254218453823 ) ) ;
#143842 = CARTESIAN_POINT ( 'NONE',  ( -0.7500000000000006661, -0.6416666666666446250, -1.299038105676652011 ) ) ;
#143844 = CARTESIAN_POINT ( 'NONE',  ( -11.84101807917483740, 11.11021500260875250, 1.444039656437077879 ) ) ;
#143845 = CARTESIAN_POINT ( 'NONE',  ( 3.480727363932310414, -1.353466037422011992, 1.499425228245174102 ) ) ;
#143846 = CARTESIAN_POINT ( 'NONE',  ( -1.364683531250012516, 3.238541667008084879, -0.7879004041258289570 ) ) ;
#143847 = ADVANCED_FACE ( 'NONE', ( #30762 ), #133342, .F. ) ;
#143848 = CARTESIAN_POINT ( 'NONE',  ( 10.39874063200158893, 11.23421161353111586, 0.000000000000000000 ) ) ;
#143849 = CARTESIAN_POINT ( 'NONE',  ( 2.759224924868249662, -1.879262701025650850, -1.068020781904190253 ) ) ;
#143850 = CARTESIAN_POINT ( 'NONE',  ( 6.620655732516647518, 7.053381450551401421, 2.424417106520880161 ) ) ;
#143851 = CARTESIAN_POINT ( 'NONE',  ( -1.500000000000011324, 4.670833333333353821, 0.8660254037844403729 ) ) ;
#143853 = FACE_OUTER_BOUND ( 'NONE', #188744, .T. ) ;
#143852 = CARTESIAN_POINT ( 'NONE',  ( 7.506374323821472849, 8.786466794993730289, -1.199719254218452047 ) ) ;
#143854 = CARTESIAN_POINT ( 'NONE',  ( 8.175203438916005538, 11.52119253116861586, -1.082531754730543083 ) ) ;
#143856 = CARTESIAN_POINT ( 'NONE',  ( 8.021163746898499980, 15.29143580044878625, -8.926870001462752668 ) ) ;
#143855 = CARTESIAN_POINT ( 'NONE',  ( 1.170657403521972562, -0.9760459728485239017, -1.939464792355448663 ) ) ;
#143857 = CARTESIAN_POINT ( 'NONE',  ( -5.910991785878165317, 8.879612269291090598, -1.082531754730538864 ) ) ;
#143858 = CARTESIAN_POINT ( 'NONE',  ( -1.402160292154681736E-14, 1.946875000341422579, -1.575800808251660134 ) ) ;
#143859 = CARTESIAN_POINT ( 'NONE',  ( 2.279091853667324141, 2.002311374866962979, -0.8913168663882904408 ) ) ;
#143860 = CARTESIAN_POINT ( 'NONE',  ( 6.883263157960363365, 3.690127339433949327, 2.567897385111846731 ) ) ;
#143861 = CARTESIAN_POINT ( 'NONE',  ( 2.184789616947193203, -2.218938341775698042, -0.4411300470171536370 ) ) ;
#143862 = CARTESIAN_POINT ( 'NONE',  ( -6.856673000209188906, 9.022537805042615489, 1.599625672291283607 ) ) ;
#143863 = CARTESIAN_POINT ( 'NONE',  ( -0.6823417656249969321, 4.280208333674755394, -1.181850606188749264 ) ) ;
#143864 = CARTESIAN_POINT ( 'NONE',  ( 5.931307043615195340, 7.129970210930432373, 1.110187140972586306 ) ) ;
#143865 = CARTESIAN_POINT ( 'NONE',  ( -6.009258394948636914E-15, 12.43750000000000178, -1.732050807568875195 ) ) ;
#143866 = CARTESIAN_POINT ( 'NONE',  ( 6.861835142292147083, 7.178098218861903135, 0.7216878364870328300 ) ) ;
#143867 = EDGE_CURVE ( 'NONE', #185175, #162324, #84840, .T. ) ;
#143868 = CARTESIAN_POINT ( 'NONE',  ( 4.551851636600127371, 1.769384361346277856, -0.04241240985469392488 ) ) ;
#143869 = CARTESIAN_POINT ( 'NONE',  ( 7.736899214892750010, 12.17813285068358020, 1.040834085586084257E-14 ) ) ;
#143870 = CARTESIAN_POINT ( 'NONE',  ( 0.4992256481273240065, 1.750750569696429171, -1.170121261866068130 ) ) ;
#143872 = CARTESIAN_POINT ( 'NONE',  ( 1.499999999999987121, 0.5041666666666856367, 0.8660254037844524744 ) ) ;
#143871 = CARTESIAN_POINT ( 'NONE',  ( 1.364683531249997417, 8.734375000341396245, 2.602085213965210642E-15 ) ) ;
#143873 = CARTESIAN_POINT ( 'NONE',  ( -5.971440312176176768, 5.931378217152456500, 0.000000000000000000 ) ) ;
#143874 = CARTESIAN_POINT ( 'NONE',  ( 6.433220217788329087, -1.621194592471734364, -1.198847091081943539 ) ) ;
#143876 = ORIENTED_EDGE ( 'NONE', *, *, #80770, .T. ) ;
#143875 = CARTESIAN_POINT ( 'NONE',  ( 5.132992444152020717, 1.676870426783064083, 0.6860526005390086279 ) ) ;
#143877 = CARTESIAN_POINT ( 'NONE',  ( 8.940712233207955606, 12.51824914112961729, 1.199719254218450271 ) ) ;
#143878 = CARTESIAN_POINT ( 'NONE',  ( 3.783945140921864070, -0.9226758061156097313, 1.627204332209288395 ) ) ;
#143879 = CARTESIAN_POINT ( 'NONE',  ( 4.786024367859083029, -1.269482053145968514, -1.635305934682528717 ) ) ;
#143880 = CARTESIAN_POINT ( 'NONE',  ( -7.404161286394468355, 7.810812053647902431, 0.000000000000000000 ) ) ;
#143881 = CARTESIAN_POINT ( 'NONE',  ( -0.4340280775911248834, 3.713184418947140575, 0.4851569899464777125 ) ) ;
#143882 = CARTESIAN_POINT ( 'NONE',  ( 7.228468454380276853, 11.58496363008569574, 1.040834085586084257E-14 ) ) ;
#143883 = CARTESIAN_POINT ( 'NONE',  ( -1.534377212605050333, 8.695787254938599276, 2.514108538948842675 ) ) ;
#143884 = CARTESIAN_POINT ( 'NONE',  ( -5.032355315092804204, 6.712689635018381118, 1.249972437814668380 ) ) ;
#143885 = CARTESIAN_POINT ( 'NONE',  ( -4.909967638851771454, 4.671257834700952571, -0.2941531795261614346 ) ) ;
#143886 = CARTESIAN_POINT ( 'NONE',  ( 0.6823417656249917140, 5.155208333674749177, 1.181850606188765695 ) ) ;
#143887 = CARTESIAN_POINT ( 'NONE',  ( 4.264078424595136418, -1.956757550135434620, 0.1421211968542570592 ) ) ;
#143888 = CARTESIAN_POINT ( 'NONE',  ( 0.6146109705059289441, 0.6351056948852469297, -1.913509406280079705 ) ) ;
#143889 = CARTESIAN_POINT ( 'NONE',  ( 1.123270288254022198, 2.908552654332631437, -0.7749999999939810591 ) ) ;
#143891 = CARTESIAN_POINT ( 'NONE',  ( 7.779015489124649463, -5.502990254781787272, 7.777446446097295407 ) ) ;
#143890 = CARTESIAN_POINT ( 'NONE',  ( 7.099665995050449041, 11.43469409420089455, 0.7998128361456462443 ) ) ;
#143892 = CARTESIAN_POINT ( 'NONE',  ( 1.211929638205839765, -0.8359089839212189288, -1.673436591668895579 ) ) ;
#143893 = CARTESIAN_POINT ( 'NONE',  ( -1.364683531249997417, 3.509375000341423245, 1.214306433183764966E-14 ) ) ;
#143894 = CARTESIAN_POINT ( 'NONE',  ( 2.724860606552154785, 1.455292111517191511, -1.391298800531393765 ) ) ;
#143896 = CARTESIAN_POINT ( 'NONE',  ( 2.284896850813819213, 1.698563897025050506, -1.263734059995786030 ) ) ;
#143895 = CARTESIAN_POINT ( 'NONE',  ( -6.561783159334141580, 7.718130443053708767, -1.082531754730544860 ) ) ;
#143897 = CARTESIAN_POINT ( 'NONE',  ( 0.000000000000000000, -9.919999999999998153, 0.000000000000000000 ) ) ;
#143898 = CARTESIAN_POINT ( 'NONE',  ( 4.088381982606685838, 1.110138344689771239, -1.747393465062855533 ) ) ;
#143899 = B_SPLINE_CURVE_WITH_KNOTS ( 'NONE', 3,
 ( #121878, #192114, #9112, #10174, #24271, #40562, #191048 ),
 .UNSPECIFIED., .F., .F.,
 ( 4, 3, 4 ),
 ( 3.315837474970910530E-05, 0.0009000000035470257127, 0.001929259801299068556 ),
 .UNSPECIFIED. ) ;
#143900 = CARTESIAN_POINT ( 'NONE',  ( 4.435452530326143616, 5.203724702582467998, -1.199719254218452047 ) ) ;
#143902 = CARTESIAN_POINT ( 'NONE',  ( 4.539282502477016479, 4.190251095844947926, 0.7998128361456341429 ) ) ;
#143901 = CARTESIAN_POINT ( 'NONE',  ( 6.456985077987440924, 0.3587005216530990692, -2.059463350302393359 ) ) ;
#143904 = EDGE_LOOP ( 'NONE', ( #112999, #119220 ) ) ;
#143903 = CARTESIAN_POINT ( 'NONE',  ( 5.772426501671443333, -1.156275361458743545, 1.412693073426966262 ) ) ;
#143905 = CARTESIAN_POINT ( 'NONE',  ( 9.725276259704228821, 10.24057714594344048, 0.7998128361456462443 ) ) ;
#143906 = CARTESIAN_POINT ( 'NONE',  ( 2.456316247939560160, 8.205176026796141997, -2.499999999999995115 ) ) ;
#143907 = CARTESIAN_POINT ( 'NONE',  ( 10.13422073961231185, 13.69230262657889874, -7.310424441678322616 ) ) ;
#143908 = CARTESIAN_POINT ( 'NONE',  ( 6.317417574511640765, -0.2763070477263400715, 2.189352377801502936 ) ) ;
#143909 = CARTESIAN_POINT ( 'NONE',  ( 0.6823417656249934904, 12.00520833367473017, 1.181850606188764807 ) ) ;
#143910 = CARTESIAN_POINT ( 'NONE',  ( 4.635362334195573197, -0.09024504784891507203, 1.910265517452472084 ) ) ;
#143911 = CARTESIAN_POINT ( 'NONE',  ( -9.158696461231359720, 10.64389961198009615, 1.199719254218462483 ) ) ;
#143912 = CARTESIAN_POINT ( 'NONE',  ( 7.481401836642521452, 7.622723652371411696, 1.040834085586084257E-14 ) ) ;
#143913 = CARTESIAN_POINT ( 'NONE',  ( -6.760415694317216410E-14, 2.234375000341476625, 1.570758158831744300 ) ) ;
#143914 = CARTESIAN_POINT ( 'NONE',  ( 9.500338091956020747, -7.818966704647656307, 0.03919461954078456989 ) ) ;
#143915 = CARTESIAN_POINT ( 'NONE',  ( 4.847203612085560387, 5.613824621309978724, -1.199719254218452047 ) ) ;
#143916 = ORIENTED_EDGE ( 'NONE', *, *, #34251, .T. ) ;
#143917 = CARTESIAN_POINT ( 'NONE',  ( 0.000000000000000000, 8.499999999999996447, 0.000000000000000000 ) ) ;
#143918 = CARTESIAN_POINT ( 'NONE',  ( 0.07680821025391608436, 0.2560392329899116026, -1.846278364303982178 ) ) ;
#143919 = CARTESIAN_POINT ( 'NONE',  ( 6.692885107001518286, 7.837396042037102717, -1.199719254218452047 ) ) ;
#143920 = CONICAL_SURFACE ( 'NONE', #206177, 10.99999999999998934, 0.7853981633974533860 ) ;
#143921 = FACE_OUTER_BOUND ( 'NONE', #23822, .T. ) ;
#143922 = CARTESIAN_POINT ( 'NONE',  ( -5.157723666773176063, 7.780300641499326098, 1.171761296108381201 ) ) ;
#143923 = CARTESIAN_POINT ( 'NONE',  ( -5.097502569058207200, 8.890910730635814829, -0.7216878364870207285 ) ) ;
#143924 = AXIS2_PLACEMENT_3D ( 'NONE', #198575, #2498, #118483 ) ;
#143925 = CARTESIAN_POINT ( 'NONE',  ( 3.147464216666835402, 6.823792019419957278, -0.7998128361456291469 ) ) ;
#143926 = CARTESIAN_POINT ( 'NONE',  ( 2.588665490599820096, 1.909050991929973629, 0.4833708566103470661 ) ) ;
#143927 = CARTESIAN_POINT ( 'NONE',  ( 3.585564690064909854, -0.5826378547920657569, 1.930424337232887977 ) ) ;
#143928 = CARTESIAN_POINT ( 'NONE',  ( -8.532158741701643123, 8.848606708273724308, 0.7998128361456462443 ) ) ;
#143929 = CARTESIAN_POINT ( 'NONE',  ( 5.903649544107831382, 5.852288987739402870, -0.7998128361456481317 ) ) ;
#143930 = CARTESIAN_POINT ( 'NONE',  ( 6.727182134110199385, 7.052145554274142469, 2.687205589382557491 ) ) ;
#143931 = CARTESIAN_POINT ( 'NONE',  ( 4.101666331917613206, -2.185647184384610586, 0.1603006067264350909 ) ) ;
#143932 = DIRECTION ( 'NONE',  ( -0.000000000000000000, -1.000000000000000000, -0.000000000000000000 ) ) ;
#143933 = CARTESIAN_POINT ( 'NONE',  ( 1.799704718893188282, -0.6512145186477935610, 1.813102765825167273 ) ) ;
#143934 = CARTESIAN_POINT ( 'NONE',  ( -8.784793466650835825, 12.33634391347959713, 1.199719254218462483 ) ) ;
#143935 = CARTESIAN_POINT ( 'NONE',  ( 1.177110729581195780, 3.085371626218851748, 0.7750000000000065725 ) ) ;
#143936 = CARTESIAN_POINT ( 'NONE',  ( 0.1329588055935578272, 2.045323036463253086, -2.262667038281248377 ) ) ;
#143937 = CARTESIAN_POINT ( 'NONE',  ( 4.773879485787624333, 4.742149952939897162, -0.7216878364870357165 ) ) ;
#143938 = CARTESIAN_POINT ( 'NONE',  ( 6.272618624616828953, 10.46980549536166016, 1.040834085586084257E-14 ) ) ;
#143939 = FACE_OUTER_BOUND ( 'NONE', #149447, .T. ) ;
#143940 = CARTESIAN_POINT ( 'NONE',  ( 6.211043768836185031, 6.418841616496599123, 0.7216878364870328300 ) ) ;
#143941 = ORIENTED_EDGE ( 'NONE', *, *, #12956, .F. ) ;
#143943 = CARTESIAN_POINT ( 'NONE',  ( 1.910792991191323065, -0.5388759818002909485, -1.939549710442307839 ) ) ;
#143942 = CARTESIAN_POINT ( 'NONE',  ( 6.216338285296751920, 1.720575329815833943, 0.6561210673821931127 ) ) ;
#143944 = CARTESIAN_POINT ( 'NONE',  ( 3.919517222396780909, 0.8229245375931023565, 2.146178768164926254 ) ) ;
#143946 = CARTESIAN_POINT ( 'NONE',  ( 2.588518228195731741, 1.803668244214111871, 0.4575444346353977898 ) ) ;
#143945 = CARTESIAN_POINT ( 'NONE',  ( -0.1291982275798911617, 0.2270562610647832436, -2.107042122458637756 ) ) ;
#143947 = CARTESIAN_POINT ( 'NONE',  ( -3.285556943749998737, -2.530208332855374831, 1.896917185911908499 ) ) ;
#143948 = CARTESIAN_POINT ( 'NONE',  ( -15.75000000000000000, 10.89999999999998259, 1.799999999999999600 ) ) ;
#143949 = CARTESIAN_POINT ( 'NONE',  ( 5.097880177178074845, 1.288836597028759634, 1.412999258680311510 ) ) ;
#143950 = CARTESIAN_POINT ( 'NONE',  ( -6.509886312855995172, 10.74661779830734254, -0.7998128361456291469 ) ) ;
#143951 = CARTESIAN_POINT ( 'NONE',  ( -4.489158259900630554, 8.251452046610447510, 0.000000000000000000 ) ) ;
#143953 = CARTESIAN_POINT ( 'NONE',  ( 3.467518583331068438, 1.825290416974333807, -0.4087457676540603990 ) ) ;
#143952 = CARTESIAN_POINT ( 'NONE',  ( 5.302318524065624317, 1.582279558761565452, -1.366676729786527211 ) ) ;
#143954 = CARTESIAN_POINT ( 'NONE',  ( 6.317736394288135493, 8.393778431468064127, 1.443375672974076540 ) ) ;
#143955 = VERTEX_POINT ( 'NONE', #109935 ) ;
#143956 = EDGE_CURVE ( 'NONE', #211051, #197321, #5831, .T. ) ;
#143957 = DIRECTION ( 'NONE',  ( -9.912705607951403669E-16, -1.000000000000000000, -8.227696745425610178E-32 ) ) ;
#143958 = CARTESIAN_POINT ( 'NONE',  ( 0.1645940602202164704, -7.825441678136432877, -10.99897937609837761 ) ) ;
#143959 = CARTESIAN_POINT ( 'NONE',  ( 5.936138232048088881, 0.8439337091313244832, -1.504256470664022238 ) ) ;
#143960 = CARTESIAN_POINT ( 'NONE',  ( -5.065942953000576843, 9.062017211809330064, -0.7998128361456231517 ) ) ;
#143961 = CARTESIAN_POINT ( 'NONE',  ( 1.142726939315736656, 0.7017603364856840331, 1.586018014115580188 ) ) ;
#143962 = CARTESIAN_POINT ( 'NONE',  ( 1.913201741516640464, 3.249623237789940333, 0.4478572873796038967 ) ) ;
#143963 = TOROIDAL_SURFACE ( 'NONE', #71222, 9.580000000000001847, 0.08000000000000000167 ) ;
#143964 = DIRECTION ( 'NONE',  ( 8.638326563840814399E-31, 0.000000000000000000, 1.000000000000000000 ) ) ;
#143965 = CARTESIAN_POINT ( 'NONE',  ( 5.928641807120487606, -1.383276364288194893, 1.673324517764721575 ) ) ;
#143966 = CARTESIAN_POINT ( 'NONE',  ( 3.896943178251357054, 1.541351720387572843, -0.9781566455248569270 ) ) ;
#143967 = CARTESIAN_POINT ( 'NONE',  ( 1.762477828903946442, -0.7011357286515782494, -1.832381215946830011 ) ) ;
#143968 = CARTESIAN_POINT ( 'NONE',  ( 0.5271635063940235399, -1.813475876746664772, 1.092501443452270404 ) ) ;
#143969 = EDGE_CURVE ( 'NONE', #197571, #21610, #63974, .T. ) ;
#143970 = CARTESIAN_POINT ( 'NONE',  ( -8.696665468161981494, 12.23352791524263239, -1.199719254218446718 ) ) ;
#143971 = CARTESIAN_POINT ( 'NONE',  ( 8.613507663383630941, 8.943513783569379427, -0.7998128361456221525 ) ) ;
#143972 = CARTESIAN_POINT ( 'NONE',  ( 2.754661888675050019, 2.104750880745378083, 0.2572054321872129790 ) ) ;
#143973 = CARTESIAN_POINT ( 'NONE',  ( -4.772106882330241717, 5.630174786549132726, -1.082531754730544860 ) ) ;
#143974 = ADVANCED_FACE ( 'NONE', ( #100795 ), #195385, .T. ) ;
#143975 = CARTESIAN_POINT ( 'NONE',  ( 0.4358566159019752195, -8.896924251528579575, -9.793384314894453269 ) ) ;
#143976 = AXIS2_PLACEMENT_3D ( 'NONE', #102879, #185170, #135390 ) ;
#143977 = CARTESIAN_POINT ( 'NONE',  ( -4.932901803036217281, 6.667582871412107259, -1.248097486420626900 ) ) ;
#143978 = CARTESIAN_POINT ( 'NONE',  ( 1.129834432590616000, 1.996231214973245516, -0.5485114149718294252 ) ) ;
#143980 = CARTESIAN_POINT ( 'NONE',  ( -0.7500000000000006661, 14.48958333401613530, -1.299038105676657340 ) ) ;
#143979 = CARTESIAN_POINT ( 'NONE',  ( -11.68720892159070601, 1.016282880930321930, 3.797404372613820911 ) ) ;
#143982 = ORIENTED_EDGE ( 'NONE', *, *, #126069, .F. ) ;
#143981 = CARTESIAN_POINT ( 'NONE',  ( 3.088771134150660735, -1.321542420002120855, 1.785288483701172657 ) ) ;
#143983 = CARTESIAN_POINT ( 'NONE',  ( 0.3878286276588240877, -0.7819352795844608517, -2.161732420081037720 ) ) ;
#143985 = CARTESIAN_POINT ( 'NONE',  ( 5.910998778867512016, -1.629530645011644463, 1.264396865911474821 ) ) ;
#143984 = CARTESIAN_POINT ( 'NONE',  ( 3.979481780810941949, 4.601482484822914998, 1.199719254218464037 ) ) ;
#143987 = CARTESIAN_POINT ( 'NONE',  ( -3.475000000000000533, -1.399999999999998579, 0.000000000000000000 ) ) ;
#143986 = CARTESIAN_POINT ( 'NONE',  ( 5.041653019435334393, 6.975290837464928728, -1.599625672291269396 ) ) ;
#143988 = CARTESIAN_POINT ( 'NONE',  ( 0.1329588055935214397, 0.7520877941899367647, -1.931583167801545819 ) ) ;
#143989 = CARTESIAN_POINT ( 'NONE',  ( 5.899929530298204661, -0.6689130865737795695, -1.715630562827724637 ) ) ;
#143991 = CARTESIAN_POINT ( 'NONE',  ( 5.575758015699216585, 5.849789923344298259, -0.7899890411014517388 ) ) ;
#143990 = AXIS2_PLACEMENT_3D ( 'NONE', #39008, #90975, #171131 ) ;
#143992 = CARTESIAN_POINT ( 'NONE',  ( 4.273844736805816780, 6.009238164405336313, 1.599625672291267398 ) ) ;
#143993 = CARTESIAN_POINT ( 'NONE',  ( 3.188212539307228699, -1.698978696193183202, -0.2961410920078124676 ) ) ;
#143994 = CARTESIAN_POINT ( 'NONE',  ( 0.9718890779336667451, -0.9023411006064323558, 1.803417998987096427 ) ) ;
#143995 = CARTESIAN_POINT ( 'NONE',  ( 2.725512391864647999, 2.281683302435618010, 0.2785734649361614745 ) ) ;
#143996 = CARTESIAN_POINT ( 'NONE',  ( -1.201851678989727383E-14, 3.634375000341422357, 1.575800808251672791 ) ) ;
#143997 = CARTESIAN_POINT ( 'NONE',  ( 2.460583821258513382, 0.9655243699240693145, 2.046139933455006776 ) ) ;
#143998 = CARTESIAN_POINT ( 'NONE',  ( 5.742829910930518977, 0.4094298153964996967, 2.065706902019475599 ) ) ;
#143999 = CARTESIAN_POINT ( 'NONE',  ( -5.790741006812557323, 9.769965251341050205, 0.000000000000000000 ) ) ;
#144000 = CARTESIAN_POINT ( 'NONE',  ( 3.145496161269778046, 0.6404232447230692182, -1.649968755877039506 ) ) ;
#144001 = CARTESIAN_POINT ( 'NONE',  ( 4.774442650306744085, 8.721933525333202653, -0.7998128361456281477 ) ) ;
#144003 = CARTESIAN_POINT ( 'NONE',  ( 0.09422489544355044933, -2.291893678819735491, -0.04953789299679511871 ) ) ;
#144002 = CARTESIAN_POINT ( 'NONE',  ( 3.065552130021340194, 6.590578228417936835, 0.000000000000000000 ) ) ;
#144004 = CARTESIAN_POINT ( 'NONE',  ( 4.822110771479974467, 1.762745816080556915, 0.5315184756640098929 ) ) ;
#144005 = CARTESIAN_POINT ( 'NONE',  ( -3.978428010606240850, 6.728917548094202949, -1.199719254218452047 ) ) ;
#144006 = CARTESIAN_POINT ( 'NONE',  ( 4.636525345749193505, 8.353103970108639587, 1.040834085586084257E-14 ) ) ;
#144007 = CARTESIAN_POINT ( 'NONE',  ( -1.500000000000011324, 4.170833333333359150, 0.8660254037844403729 ) ) ;
#144008 = CARTESIAN_POINT ( 'NONE',  ( 4.101666331917613206, -2.185647184384610586, 0.1603006067264350909 ) ) ;
#144009 = CARTESIAN_POINT ( 'NONE',  ( -3.598799709423620374, 6.286017863381107240, 1.199719254218464037 ) ) ;
#144010 = CARTESIAN_POINT ( 'NONE',  ( 0.5021762176675715894, 7.740673110510241983, -1.993154341637451088 ) ) ;
#144011 = CARTESIAN_POINT ( 'NONE',  ( -3.418820436464110379, -0.03388596222681408004, -0.09792497310439811364 ) ) ;
#144012 = CARTESIAN_POINT ( 'NONE',  ( 1.364683531249990311, 4.134375000341417028, 1.214306433183764966E-14 ) ) ;
#144013 = CARTESIAN_POINT ( 'NONE',  ( 2.947785801820240970, 0.6929415146892035082, -1.797737524126517217 ) ) ;
#144014 = CARTESIAN_POINT ( 'NONE',  ( -1.364683531250014514, 9.338541667008062319, -0.7879004041258335089 ) ) ;
#144015 = CARTESIAN_POINT ( 'NONE',  ( -5.124618876285560454, 5.081069565195661220, 0.7216878364870317197 ) ) ;
#144016 = CARTESIAN_POINT ( 'NONE',  ( 0.5807245924134795123, 1.101748585799481095, 1.928910967146231004 ) ) ;
#144017 = VERTEX_POINT ( 'NONE', #27540 ) ;
#144018 = CARTESIAN_POINT ( 'NONE',  ( -3.933273961740340496, 5.682181936820735579, 1.443375672974065660 ) ) ;
#144019 = CARTESIAN_POINT ( 'NONE',  ( 4.111146893441827821, 5.819424013814004759, 1.599625672291267398 ) ) ;
#144020 = CARTESIAN_POINT ( 'NONE',  ( -4.858757509019059562, 5.629766575900002401, 2.420000000000000373 ) ) ;
#144021 = CARTESIAN_POINT ( 'NONE',  ( 0.000000000000000000, 0.7999999999999951594, 0.000000000000000000 ) ) ;
#144022 = CARTESIAN_POINT ( 'NONE',  ( 0.1815159415691200706, 7.045075310427906246, -3.942267139059067560 ) ) ;
#144023 = CARTESIAN_POINT ( 'NONE',  ( 4.284013352238246419, 6.021101549076499637, -1.443375672974051449 ) ) ;
#144024 = CARTESIAN_POINT ( 'NONE',  ( 0.7500000000000006661, 10.86458333401613174, 1.299038105676657340 ) ) ;
#144025 = CARTESIAN_POINT ( 'NONE',  ( -1.364683531250014514, 1.551041667008084435, -0.7879004041258289570 ) ) ;
#144026 = CARTESIAN_POINT ( 'NONE',  ( 6.666866396406604167, -1.974176978123330040, -0.8811043787171415342 ) ) ;
#144027 = CARTESIAN_POINT ( 'NONE',  ( 5.301206097546149465, -1.683542251207278628, 1.007010407901312465 ) ) ;
#144028 = CARTESIAN_POINT ( 'NONE',  ( -7.811469059767924605, 12.26513100303794168, -0.7998128361456281477 ) ) ;
#144029 = CARTESIAN_POINT ( 'NONE',  ( -4.894130264408862452, 7.693273827576896373, -1.082531754730548412 ) ) ;
#144030 = CARTESIAN_POINT ( 'NONE',  ( 5.295850518597075229, -0.7817450549502875656, 2.015575934489414411 ) ) ;
#144032 = VERTEX_POINT ( 'NONE', #159677 ) ;
#144031 = CARTESIAN_POINT ( 'NONE',  ( -1.499999999999964029, 7.750000000000000000, 10.64483442802189117 ) ) ;
#144033 = CARTESIAN_POINT ( 'NONE',  ( -1.364683531250010295, 4.780208333674755394, 0.7879004041258379498 ) ) ;
#144034 = CARTESIAN_POINT ( 'NONE',  ( 0.2626887844769665303, -1.667795467377327423, -0.8471929967568125885 ) ) ;
#144035 = CARTESIAN_POINT ( 'NONE',  ( 5.940742354060237318, 1.035569694170878519, 1.390440122839208703 ) ) ;
#144037 = CARTESIAN_POINT ( 'NONE',  ( 2.929422067023911502, -1.473737196803912797, -1.622193633833472814 ) ) ;
#144036 = CARTESIAN_POINT ( 'NONE',  ( -3.355169270512988773E-14, 0.9531250003414385441, 1.570758158831740303 ) ) ;
#144038 = CARTESIAN_POINT ( 'NONE',  ( 3.575485986712009456, 0.05928947047922557279, -2.306987226281012049 ) ) ;
#144039 = CARTESIAN_POINT ( 'NONE',  ( 5.747358702077526971, -1.621750911093680081, -1.271367298817957181 ) ) ;
#144040 = CARTESIAN_POINT ( 'NONE',  ( 1.113109651085980811, -1.894741734565345004, 0.4249041608528710823 ) ) ;
#144041 = CARTESIAN_POINT ( 'NONE',  ( -6.358410854684789726, 8.441231968597481483, -1.443375672974058777 ) ) ;
#144042 = PRODUCT_DEFINITION_SHAPE ( 'NONE', 'NONE',  #214412 ) ;
#144043 = DIRECTION ( 'NONE',  ( -0.000000000000000000, -0.000000000000000000, 1.000000000000000000 ) ) ;
#144044 = CARTESIAN_POINT ( 'NONE',  ( 11.84668730067608600, 10.89999999999998259, 1.399999999999998579 ) ) ;
#144045 = EDGE_CURVE ( 'NONE', #141934, #66184, #127029, .T. ) ;
#144046 = CARTESIAN_POINT ( 'NONE',  ( 5.572555445586866441, 0.8612648569810870125, 1.938019255899057658 ) ) ;
#144047 = FACE_OUTER_BOUND ( 'NONE', #15928, .T. ) ;
#144048 = CARTESIAN_POINT ( 'NONE',  ( 2.074842474778653134, -0.8596299393073093542, 1.824119475507138821 ) ) ;
#144049 = CARTESIAN_POINT ( 'NONE',  ( -5.870317324592821073, 6.911420302522161663, -1.082531754730543083 ) ) ;
#144050 = CARTESIAN_POINT ( 'NONE',  ( 5.930760676324511316, 2.125237774816424619, 0.5940772278362898007 ) ) ;
#144051 = CARTESIAN_POINT ( 'NONE',  ( 3.285556943750000514, -1.101041666188710355, 1.896917185911906500 ) ) ;
#144052 = B_SPLINE_CURVE_WITH_KNOTS ( 'NONE', 3,
 ( #107360, #59606, #8717, #42318 ),
 .UNSPECIFIED., .F., .F.,
 ( 4, 4 ),
 ( 0.000000000000000000, 2.032232339065676875E-05 ),
 .UNSPECIFIED. ) ;
#144053 = CARTESIAN_POINT ( 'NONE',  ( -10.14641618983896976, 3.870538056096199497, 5.683069686889705707 ) ) ;
#144054 = CARTESIAN_POINT ( 'NONE',  ( 0.1701549220758866166, -1.195335944658926230, 1.380069390326914336 ) ) ;
#144055 = CARTESIAN_POINT ( 'NONE',  ( -6.129167961829681488, 9.308390501180058507, -1.199719254218452047 ) ) ;
#144057 = CARTESIAN_POINT ( 'NONE',  ( -0.07926560466948139039, 15.51761135634724198, 11.99972816967691891 ) ) ;
#144056 = CARTESIAN_POINT ( 'NONE',  ( -5.289925464687482481, 7.757115612407050165, 1.311310741419260628 ) ) ;
#144058 = CARTESIAN_POINT ( 'NONE',  ( -9.410012541129075814, 4.000000000000001776, 6.919867902370715917 ) ) ;
#144059 = VERTEX_POINT ( 'NONE', #50993 ) ;
#144060 = CARTESIAN_POINT ( 'NONE',  ( 4.434483769945627429, 2.020730376925969018, 0.4039503012724340869 ) ) ;
#144061 = CARTESIAN_POINT ( 'NONE',  ( -5.000000000000013323, 8.499999999999996447, 0.7750000000000004663 ) ) ;
#144062 = CARTESIAN_POINT ( 'NONE',  ( 0.01138762994429960880, -7.792108994756127061, 9.500479199177402023 ) ) ;
#144063 = CARTESIAN_POINT ( 'NONE',  ( -5.229694566569281555, 7.124396299129368337, 1.599625672291267398 ) ) ;
#144064 = CARTESIAN_POINT ( 'NONE',  ( -4.679499295372141709, 5.488445928469455559, 1.199719254218452935 ) ) ;
#144065 = CARTESIAN_POINT ( 'NONE',  ( 4.195966715351859833, 1.320990344651201021, 1.527833845825769643 ) ) ;
#144066 = CARTESIAN_POINT ( 'NONE',  ( -0.7500000000000215383, 0.6916666666666876351, 1.299038105676659116 ) ) ;
#144068 = CARTESIAN_POINT ( 'NONE',  ( 10.08690309888728187, 10.87040115823107911, -0.7216878364870257245 ) ) ;
#144067 = CARTESIAN_POINT ( 'NONE',  ( -5.113360211009450040, 5.994616996712990975, -1.199719254218453823 ) ) ;
#144069 = CARTESIAN_POINT ( 'NONE',  ( 6.470265622219697477, 8.571729197388226140, -1.599625672291262513 ) ) ;
#144070 = CARTESIAN_POINT ( 'NONE',  ( 3.028252848896676674, 1.146099369071330143, -1.712595011064410366 ) ) ;
#144071 = CARTESIAN_POINT ( 'NONE',  ( 2.760388869050140137, 1.913803604375517109, -0.6351994527180188088 ) ) ;
#144072 = ORIENTED_EDGE ( 'NONE', *, *, #213257, .T. ) ;
#144073 = EDGE_CURVE ( 'NONE', #3126, #197889, #80351, .T. ) ;
#144074 = CARTESIAN_POINT ( 'NONE',  ( 4.542145155778077203, 5.257923088951247159, -1.199719254218452047 ) ) ;
#144076 = ORIENTED_EDGE ( 'NONE', *, *, #85474, .F. ) ;
#144075 = CARTESIAN_POINT ( 'NONE',  ( -0.4020909550004448385, 7.366597533580868884, -1.962779437971320595 ) ) ;
#144077 = CARTESIAN_POINT ( 'NONE',  ( 3.163435312993330140, -0.5825663732807913053, -1.930122257003751063 ) ) ;
#144078 = CARTESIAN_POINT ( 'NONE',  ( 1.921575063125853022, 1.060747535801230379, -1.504664925706208578 ) ) ;
#144079 = CARTESIAN_POINT ( 'NONE',  ( 0.6632354941851228425, -1.667548007495605944, 1.595465711622134242 ) ) ;
#144080 = CARTESIAN_POINT ( 'NONE',  ( 5.520104819419390907, 6.469152373191302985, 1.199719254218452935 ) ) ;
#144081 = CARTESIAN_POINT ( 'NONE',  ( 2.284651837757902371, -2.119410549416993916, -0.4241055355862289877 ) ) ;
#144082 = CARTESIAN_POINT ( 'NONE',  ( -5.215082642750900277, 9.236013516518044142, 0.000000000000000000 ) ) ;
#144083 = CARTESIAN_POINT ( 'NONE',  ( 2.618911895557019420, 0.6142130902007210125, -2.214721005821191024 ) ) ;
#144084 = ORIENTED_EDGE ( 'NONE', *, *, #80961, .F. ) ;
#144085 = CARTESIAN_POINT ( 'NONE',  ( -11.86145016429273724, 11.00587408513255561, -1.100000000000002531 ) ) ;
#144086 = CARTESIAN_POINT ( 'NONE',  ( 1.164687902950040321, -1.689591380799923215, -0.8031939614948147010 ) ) ;
#144087 = CARTESIAN_POINT ( 'NONE',  ( 5.260604563723265237, -1.428518960016441186, 1.358918391201448417 ) ) ;
#144088 = VECTOR ( 'NONE', #28840, 1000.000000000000000 ) ;
#144090 = CARTESIAN_POINT ( 'NONE',  ( 7.551528372687370094, 11.75394083486988528, -0.7216878364870267237 ) ) ;
#144089 = CARTESIAN_POINT ( 'NONE',  ( 0.6823417656249917140, 3.592708333674754506, 1.181850606188765695 ) ) ;
#144092 = CARTESIAN_POINT ( 'NONE',  ( 0.2587985324217950689, 0.8487602207661277820, 2.037339956011212649 ) ) ;
#144091 = CARTESIAN_POINT ( 'NONE',  ( -5.038826645773246682, 9.030381520044109322, 0.7998128361456481317 ) ) ;
#144093 = EDGE_CURVE ( 'NONE', #3699, #210323, #81937, .T. ) ;
#144094 = CARTESIAN_POINT ( 'NONE',  ( 6.373496627357888578, -0.2573980274669443458, 2.054251119134167691 ) ) ;
#144095 = CARTESIAN_POINT ( 'NONE',  ( 4.808338034340912337, 8.761478140039733020, 1.040834085586084257E-14 ) ) ;
#144096 = CARTESIAN_POINT ( 'NONE',  ( -6.087774667736030487, 7.061157519568837415, 1.199719254218450271 ) ) ;
#144097 = CARTESIAN_POINT ( 'NONE',  ( 6.639320575229294086, 7.051910277135648997, 2.801414343313723965 ) ) ;
#144098 = CARTESIAN_POINT ( 'NONE',  ( 5.418811373015061328, 1.821287777658405549, 0.7551675066918785983 ) ) ;
#144099 = CARTESIAN_POINT ( 'NONE',  ( 6.416272379866970965, -2.019260422740985828, 0.05364450914858465147 ) ) ;
#144100 = CARTESIAN_POINT ( 'NONE',  ( -1.500000000000001332, 0.1812500006828157706, 0.000000000000000000 ) ) ;
#144101 = CARTESIAN_POINT ( 'NONE',  ( 4.934332944283116973, 1.189700906406887082, -1.977258547338469841 ) ) ;
#144102 = EDGE_CURVE ( 'NONE', #157452, #20719, #209613, .T. ) ;
#144103 = CARTESIAN_POINT ( 'NONE',  ( 1.657159287258206604, 1.688608613550081516, -1.184165042645689558 ) ) ;
#144104 = CARTESIAN_POINT ( 'NONE',  ( 8.283668668269706714, 8.766627655843892697, 1.040834085586084257E-14 ) ) ;
#144105 = CARTESIAN_POINT ( 'NONE',  ( 4.369470645354133431, 8.319742529546998000, 0.7998128361456271485 ) ) ;
#144106 = CARTESIAN_POINT ( 'NONE',  ( 3.898851692381625877, 6.706354853490643642, -1.199719254218452047 ) ) ;
#144107 = CARTESIAN_POINT ( 'NONE',  ( -0.6823417656250212460, 2.113541667008083991, 1.181850606188767472 ) ) ;
#144108 = CARTESIAN_POINT ( 'NONE',  ( 3.444653546323793947, 6.176457016423196222, 1.199719254218451159 ) ) ;
#144109 = CARTESIAN_POINT ( 'NONE',  ( 4.961921032477176752, 8.732732271291288484, 1.040834085586084257E-14 ) ) ;
#144110 = CARTESIAN_POINT ( 'NONE',  ( 4.439989079487234314, 1.414935287217274684, 1.646911713943682409 ) ) ;
#144112 = CARTESIAN_POINT ( 'NONE',  ( 4.054132754448328768, -1.361571661076573792, 1.239656203754435193 ) ) ;
#144111 = CARTESIAN_POINT ( 'NONE',  ( -4.012850279964973232, 4.744375417122949301, 1.082531754730560403 ) ) ;
#144114 = DIRECTION ( 'NONE',  ( -1.000000000000000000, 0.000000000000000000, 0.000000000000000000 ) ) ;
#144113 = DIRECTION ( 'NONE',  ( -1.276756478318932585E-15, 1.000000000000000000, -1.665334536937738262E-16 ) ) ;
#144115 = CARTESIAN_POINT ( 'NONE',  ( 5.144143540903125533, 0.6357783856077160456, 2.097287126430439130 ) ) ;
#144116 = CARTESIAN_POINT ( 'NONE',  ( 0.4663757142498895503, 3.020629270880486494, 1.944911959762657627 ) ) ;
#144117 = CARTESIAN_POINT ( 'NONE',  ( 5.700151306344448443, -2.262689076517818254, -0.006432940626173094985 ) ) ;
#144118 = ORIENTED_EDGE ( 'NONE', *, *, #208749, .T. ) ;
#144119 = CARTESIAN_POINT ( 'NONE',  ( -4.119491766144414591, 7.660190618428146081, -0.8001636830725885607 ) ) ;
#144120 = CARTESIAN_POINT ( 'NONE',  ( 11.52460864928264783, 11.38000000000000078, -3.346683403123526190 ) ) ;
#144121 = CARTESIAN_POINT ( 'NONE',  ( 4.650542599771462449, 8.421518672640367242, 0.4769741307986720136 ) ) ;
#144122 = CARTESIAN_POINT ( 'NONE',  ( -5.438229012412903352, 6.477593614970734492, -1.082531754730549967 ) ) ;
#144123 = CARTESIAN_POINT ( 'NONE',  ( 0.000000000000000000, 3.447199233515649386, 12.00000000000000178 ) ) ;
#144124 = CARTESIAN_POINT ( 'NONE',  ( 0.8832604684265840111, 1.184483277375179666, 1.315230855816750921 ) ) ;
#144125 = CIRCLE ( 'NONE', #157857, 11.99999999999999112 ) ;
#144126 = CARTESIAN_POINT ( 'NONE',  ( 4.881498389339896882, 0.1952109149471596417, -2.003590356478464507 ) ) ;
#144127 = CARTESIAN_POINT ( 'NONE',  ( 5.795220594837462436, 8.848508896363995291, -1.199719254218440723 ) ) ;
#144128 = CARTESIAN_POINT ( 'NONE',  ( 3.838982076996471982, 0.3068427722541127722, 2.083350420514245016 ) ) ;
#144129 = CARTESIAN_POINT ( 'NONE',  ( 2.671383988363975170, 1.356552116283934240, 1.352788525452413237 ) ) ;
#144130 = CARTESIAN_POINT ( 'NONE',  ( 0.000000000000000000, 12.22000000000000064, 0.000000000000000000 ) ) ;
#144131 = CARTESIAN_POINT ( 'NONE',  ( 3.560960244297206589, 1.554118163632215444, -1.209804376587125807 ) ) ;
#144132 = CARTESIAN_POINT ( 'NONE',  ( 5.554946522049384328, 0.3980760423633997180, 1.979986811436624805 ) ) ;
#144133 = CARTESIAN_POINT ( 'NONE',  ( 1.920565142479381038, 1.744437793965779582, 0.6759427408406930571 ) ) ;
#144136 = ORIENTED_EDGE ( 'NONE', *, *, #199668, .F. ) ;
#144135 = CARTESIAN_POINT ( 'NONE',  ( 1.670022949053862948, 1.907054940702714863, -0.1439945843566131367 ) ) ;
#144134 = CARTESIAN_POINT ( 'NONE',  ( 5.057137062068671973, -1.459852279745242010, -0.9183987515692086934 ) ) ;
#144138 = CARTESIAN_POINT ( 'NONE',  ( 3.389175213736285386, 6.897862149426897460, 0.7216878364870317197 ) ) ;
#144137 = CARTESIAN_POINT ( 'NONE',  ( 1.770444396619451632, 1.136427050704125419, 1.891651738277564831 ) ) ;
#144139 = AXIS2_PLACEMENT_3D ( 'NONE', #68042, #85392, #31326 ) ;
#144140 = CARTESIAN_POINT ( 'NONE',  ( -1.201851678989727383E-14, 2.134375000341423689, 1.575800808251672791 ) ) ;
#144141 = CARTESIAN_POINT ( 'NONE',  ( 9.413438726589914651, 9.876766690643398405, 0.000000000000000000 ) ) ;
#144142 = CARTESIAN_POINT ( 'NONE',  ( 11.33772467203874612, 12.59267152018150426, -3.600000000000000977 ) ) ;
#144143 = PRESENTATION_STYLE_ASSIGNMENT (( #160343 ) ) ;
#144144 = CARTESIAN_POINT ( 'NONE',  ( -0.01652817808797454532, 2.595569970836366203, -2.081186177183739883 ) ) ;
#144145 = CARTESIAN_POINT ( 'NONE',  ( -1.416814887940403000, 7.999555336178692855, 9.899480522462175358 ) ) ;
#144146 = CARTESIAN_POINT ( 'NONE',  ( 2.049362625460974030, 1.802418521853879962, -1.018503948505583789 ) ) ;
#144147 = CARTESIAN_POINT ( 'NONE',  ( -1.500000000000013101, 1.920833333333356263, 0.8660254037844403729 ) ) ;
#144148 = CARTESIAN_POINT ( 'NONE',  ( 6.959412922516382771, 7.013736585890911535, 0.7998128361456341429 ) ) ;
#144149 = CARTESIAN_POINT ( 'NONE',  ( -5.879432169820529630, 10.01108796476595764, -0.7998128361456221525 ) ) ;
#144150 = CARTESIAN_POINT ( 'NONE',  ( 3.379725431556547477, 7.165039780116438273, -1.734723475976807094E-15 ) ) ;
#144151 = CARTESIAN_POINT ( 'NONE',  ( 6.076833508651091620, -1.499762292660647311, 1.499315088411487640 ) ) ;
#144152 = FACE_OUTER_BOUND ( 'NONE', #79017, .T. ) ;
#144153 = CARTESIAN_POINT ( 'NONE',  ( 1.364683531249990311, 2.884375000341422801, 1.214306433183764966E-14 ) ) ;
#144154 = ORIENTED_EDGE ( 'NONE', *, *, #134567, .T. ) ;
#144155 = AXIS2_PLACEMENT_3D ( 'NONE', #62433, #162083, #13672 ) ;
#144157 = CARTESIAN_POINT ( 'NONE',  ( 3.871016551901614200, 4.474939717762034697, -1.199719254218446718 ) ) ;
#144156 = FACE_OUTER_BOUND ( 'NONE', #51780, .T. ) ;
#144158 = CARTESIAN_POINT ( 'NONE',  ( 4.815779736370030761, -1.620933320526974031, 1.198678058543983571 ) ) ;
#144159 = CARTESIAN_POINT ( 'NONE',  ( 4.258935762849770157, -0.005977556496831581273, -1.915903398800692159 ) ) ;
#144160 = CARTESIAN_POINT ( 'NONE',  ( 3.034921719543516971, -1.931671641359738567, 1.035203715903771915 ) ) ;
#144161 = CARTESIAN_POINT ( 'NONE',  ( -1.963827086952256051, 3.753930767994497764, 0.3999999999999835909 ) ) ;
#144162 = CARTESIAN_POINT ( 'NONE',  ( 0.7499999999999885647, 0.7645833340161543035, 1.299038105676657340 ) ) ;
#144163 = CARTESIAN_POINT ( 'NONE',  ( 5.045186288489547977, 0.1525188484602090777, 2.007510047055609093 ) ) ;
#144164 = CARTESIAN_POINT ( 'NONE',  ( -7.555971681517696936, 7.709721804725773175, 0.7998128361456462443 ) ) ;
#144165 = EDGE_CURVE ( 'NONE', #101393, #82918, #3273, .T. ) ;
#144167 = CARTESIAN_POINT ( 'NONE',  ( 6.028941913163482269, -1.788401068206580957, 1.133005349186385402 ) ) ;
#144166 = CARTESIAN_POINT ( 'NONE',  ( -2.318081078256692518, 5.648252324700675508, 1.040834085586084257E-14 ) ) ;
#144168 = CARTESIAN_POINT ( 'NONE',  ( -0.6823417656250039265, 9.630208333674728394, -1.181850606188755259 ) ) ;
#144170 = CARTESIAN_POINT ( 'NONE',  ( -5.986807348886189040, 9.142303119412650503, -1.199719254218452047 ) ) ;
#144169 = CARTESIAN_POINT ( 'NONE',  ( 3.316043925569078787, 1.324660045548868181, -1.617576387421674866 ) ) ;
#144172 = ORIENTED_EDGE ( 'NONE', *, *, #211621, .F. ) ;
#144171 = CARTESIAN_POINT ( 'NONE',  ( 1.887319702290214840, 1.186364228098319762, 1.252193311579427482 ) ) ;
#144173 = CARTESIAN_POINT ( 'NONE',  ( 5.080389167821143026, 1.047295930500062866, 1.843893106414703054 ) ) ;
#144174 = CARTESIAN_POINT ( 'NONE',  ( 4.611744806942754238, 8.532119374741881757, -0.7998128361456231517 ) ) ;
#144175 = CARTESIAN_POINT ( 'NONE',  ( -5.608633734226008194, 5.643391804966442216, 0.4859901473732997079 ) ) ;
#144176 = CARTESIAN_POINT ( 'NONE',  ( 3.834746474454188013E-15, 10.59375000068279604, 1.500000000000001554 ) ) ;
#144177 = CARTESIAN_POINT ( 'NONE',  ( -0.007565906569761434060, -9.598697202504085979, 9.591786056756831158 ) ) ;
#144178 = CARTESIAN_POINT ( 'NONE',  ( 6.982612806237943559, 8.105135347821125436, -1.199719254218446718 ) ) ;
#144179 = ORIENTED_EDGE ( 'NONE', *, *, #132056, .F. ) ;
#144181 =( BOUNDED_SURFACE ( )  B_SPLINE_SURFACE ( 3, 2, ( 
 ( #201646, #50102, #67375 ),
 ( #238, #168116, #68454 ),
 ( #19716, #99918, #133517 ),
 ( #116223, #98858, #120509 ),
 ( #182214, #53294, #103117 ),
 ( #117290, #165979, #100964 ),
 ( #149735, #85795, #151875 ),
 ( #164909, #198458, #3449 ) ),
 .UNSPECIFIED., .F., .F., .F. ) 
 B_SPLINE_SURFACE_WITH_KNOTS ( ( 4, 2, 2, 4 ),
 ( 3, 3 ),
 ( 0.000000000000000000, 0.0002575597274893386048, 0.0005151194549786772096, 0.001030238909957354419 ),
 ( 0.000000000000000000, 1.000000000000000000 ),
 .UNSPECIFIED. ) 
 GEOMETRIC_REPRESENTATION_ITEM ( )  RATIONAL_B_SPLINE_SURFACE ( (
 ( 1.000000000000000000, 0.9238795325112795220, 1.000000000000000000),
 ( 1.000000000000000000, 0.9228594682462778476, 1.000000000000000000),
 ( 1.000000000000000000, 0.9150875845228949590, 1.000000000000000000),
 ( 1.000000000000000000, 0.8905471774190931722, 1.000000000000000000),
 ( 1.000000000000000000, 0.8740340839247475735, 1.000000000000000000),
 ( 1.000000000000000000, 0.8160099319848322930, 1.000000000000000000),
 ( 1.000000000000000000, 0.7673743911477570734, 1.000000000000000000),
 ( 1.000000000000000000, 0.7100530722070661493, 1.000000000000000000) ) ) 
 REPRESENTATION_ITEM ( '' )  SURFACE ( )  );
#144180 = DIRECTION ( 'NONE',  ( -0.8660254037844397068, 0.4999999999999978906, 0.000000000000000000 ) ) ;
#144182 = ADVANCED_FACE ( 'NONE', ( #88840, #202540 ), #36856, .F. ) ;
#144184 = CARTESIAN_POINT ( 'NONE',  ( 1.840194262915356260, 1.042575051921472040, -1.481162322861505620 ) ) ;
#144183 = CARTESIAN_POINT ( 'NONE',  ( 4.993145711582793744, 9.047363440147082159, -0.7998128361456481317 ) ) ;
#144185 = CARTESIAN_POINT ( 'NONE',  ( -7.366157530926372488, 7.488271962369228874, -0.7998128361456291469 ) ) ;
#144186 = CARTESIAN_POINT ( 'NONE',  ( 5.054492339796319733, 4.791329239384148231, -0.7998128361456211532 ) ) ;
#144187 = EDGE_LOOP ( 'NONE', ( #83406, #2199, #180729, #125668, #42928, #107432, #31613, #203946 ) ) ;
#144188 = CARTESIAN_POINT ( 'NONE',  ( 4.929271367020211514, 7.908511140569038922, 1.199719254218452047 ) ) ;
#144189 = CARTESIAN_POINT ( 'NONE',  ( 2.262115610809340094, 1.811117530136572285, 0.04320712765945587674 ) ) ;
#144190 = CARTESIAN_POINT ( 'NONE',  ( 6.639320575229258559, 7.629137130509072051, 2.496737603865983424 ) ) ;
#144191 = CARTESIAN_POINT ( 'NONE',  ( -10.98974895236974092, -7.729832900979438648, 0.4787367839866840669 ) ) ;
#144192 = CARTESIAN_POINT ( 'NONE',  ( 4.799922300691145338, 6.743925459469453543, 1.247687964948118733 ) ) ;
#144193 = CARTESIAN_POINT ( 'NONE',  ( 4.351900876113290018, -0.7134228844126557778, 1.719084262507431182 ) ) ;
#144194 = CARTESIAN_POINT ( 'NONE',  ( 1.827608144986846206, 0.7312883373844185630, -1.770730004348388453 ) ) ;
#144195 = CARTESIAN_POINT ( 'NONE',  ( 0.7975364289293709330, -0.6616875547802402169, 1.701626729119443127 ) ) ;
#144196 = DIRECTION ( 'NONE',  ( 0.000000000000000000, -1.000000000000000000, 0.000000000000000000 ) ) ;
#144197 = DIRECTION ( 'NONE',  ( 0.6507913734559708230, 0.7592566023652946861, 2.465190328815661618E-32 ) ) ;
#144198 = CARTESIAN_POINT ( 'NONE',  ( 4.739057715201537846, 8.198473722472776615, 0.7146191656044629248 ) ) ;
#144199 = DIRECTION ( 'NONE',  ( 0.000000000000000000, 0.000000000000000000, -1.000000000000000000 ) ) ;
#144200 = CARTESIAN_POINT ( 'NONE',  ( -3.633221978782299910, 5.261844946711204507, -1.443375672974053447 ) ) ;
#144201 = CARTESIAN_POINT ( 'NONE',  ( 8.771762198361678031, 9.336070107617867819, 1.040834085586084257E-14 ) ) ;
#144202 = CARTESIAN_POINT ( 'NONE',  ( 5.735196696812420392, -0.04448252213613138051, -1.969098798407813433 ) ) ;
#144203 = CARTESIAN_POINT ( 'NONE',  ( -4.985647801523292344, 6.839675073242382553, -1.599625672291256295 ) ) ;
#144204 = CARTESIAN_POINT ( 'NONE',  ( -11.97302537858672444, 9.801240101919498571, -0.8111997896468137181 ) ) ;
#144205 = CARTESIAN_POINT ( 'NONE',  ( 0.07627643479381736313, -2.028408900457449704, -0.5058713263092640133 ) ) ;
#144206 = DIRECTION ( 'NONE',  ( -0.7592566023653004592, 0.6507913734559639396, 0.000000000000000000 ) ) ;
#144207 = CARTESIAN_POINT ( 'NONE',  ( 5.526370178063710448, 1.147270165450631207, -1.547347761420419188 ) ) ;
#144208 = CARTESIAN_POINT ( 'NONE',  ( -7.203459687562382641, 7.298457811777897319, -0.7998128361456291469 ) ) ;
#144209 = CARTESIAN_POINT ( 'NONE',  ( 0.7975364289293709330, -0.6616875547802402169, 1.701626729119443127 ) ) ;
#144210 = CARTESIAN_POINT ( 'NONE',  ( 2.684424123961434816, -1.133677649706768431, 1.893296980138805319 ) ) ;
#144211 = CARTESIAN_POINT ( 'NONE',  ( -6.047232192207364854, 7.062196034744411932, 1.031126814801977432 ) ) ;
#144212 = CARTESIAN_POINT ( 'NONE',  ( 4.947799714344386146, 4.737130853015369958, -0.7998128361456481317 ) ) ;
#144213 = ORIENTED_EDGE ( 'NONE', *, *, #60938, .T. ) ;
#144214 = CARTESIAN_POINT ( 'NONE',  ( 0.6780957659633795043, -1.050550344063156061, -1.665771736420356808 ) ) ;
#144215 = CARTESIAN_POINT ( 'NONE',  ( 2.700647863620793121, 1.641916212795376806, 1.036879047414513755 ) ) ;
#144216 = CONICAL_SURFACE ( 'NONE', #168282, 10.99999999999998934, 0.7853981633974533860 ) ;
#144217 = ORIENTED_EDGE ( 'NONE', *, *, #85154, .F. ) ;
#144218 = CARTESIAN_POINT ( 'NONE',  ( 0.3685172633814579601, -0.5404119286356176000, 1.942243004588292354 ) ) ;
#144220 = CARTESIAN_POINT ( 'NONE',  ( 5.576953945496859966, 1.718729505308995931, 0.7139912403442708611 ) ) ;
#144219 = CARTESIAN_POINT ( 'NONE',  ( -6.466312919074983512, 6.508729591867735031, -0.7998128361456362523 ) ) ;
#144221 = CARTESIAN_POINT ( 'NONE',  ( 6.737475991348287785, 6.825086509519945999, -0.7998128361456481317 ) ) ;
#144222 = DIRECTION ( 'NONE',  ( 0.000000000000000000, 1.000000000000000000, 0.000000000000000000 ) ) ;
#144223 = FACE_OUTER_BOUND ( 'NONE', #162588, .T. ) ;
#144224 = CARTESIAN_POINT ( 'NONE',  ( -5.037017762676898158, 5.835274463666530131, -1.199719254218446718 ) ) ;
#144225 = CARTESIAN_POINT ( 'NONE',  ( -6.563028877466991595, 9.814561569423593923, 1.199719254218452935 ) ) ;
#144226 = CARTESIAN_POINT ( 'NONE',  ( 1.259612756803454525, 2.158328104161820526, -0.3793702838810895095 ) ) ;
#144227 = CARTESIAN_POINT ( 'NONE',  ( 3.036663219780971978, 6.486598156479028709, -0.7216878364870267237 ) ) ;
#144228 = CARTESIAN_POINT ( 'NONE',  ( 8.025500584646550806, 8.327781868367935658, 0.000000000000000000 ) ) ;
#144229 = CARTESIAN_POINT ( 'NONE',  ( 11.48243876534946217, 9.799999999999982947, 3.199999999999997957 ) ) ;
#144230 = CARTESIAN_POINT ( 'NONE',  ( 3.017977635683791071, -0.9002817137206723386, -1.588204215665294461 ) ) ;
#144231 = CARTESIAN_POINT ( 'NONE',  ( -1.403499169903686727, 7.376709478542852416, 4.304123474984240083 ) ) ;
#144232 = CARTESIAN_POINT ( 'NONE',  ( -5.101945877444165944, 4.846691699973280976, 0.000000000000000000 ) ) ;
#144233 = CARTESIAN_POINT ( 'NONE',  ( -5.696549332702473656, 7.414053552612095643, -1.332310987329322183 ) ) ;
#144234 = LINE ( 'NONE', #209156, #8437 ) ;
#144235 = CARTESIAN_POINT ( 'NONE',  ( 10.05067194643221207, 10.62020544712608938, 0.7998128361456462443 ) ) ;
#144236 = CARTESIAN_POINT ( 'NONE',  ( 0.9262474005801927257, 1.148234195015400694, -1.546785173711192840 ) ) ;
#144237 = CARTESIAN_POINT ( 'NONE',  ( 5.805508902378371694, -1.544246397408255866, -1.209716981170713357 ) ) ;
#144238 = ADVANCED_FACE ( 'NONE', ( #102940 ), #123530, .T. ) ;
#144239 = CARTESIAN_POINT ( 'NONE',  ( -7.739006755302186846, 7.923262724141010516, 0.7998128361456462443 ) ) ;
#144240 = CARTESIAN_POINT ( 'NONE',  ( 4.137209430464448445, 7.978494768850520558, 1.040834085586084257E-14 ) ) ;
#144241 = CARTESIAN_POINT ( 'NONE',  ( 5.566036750361066154, -1.391122746885119499, 1.693456055751572986 ) ) ;
#144242 = CIRCLE ( 'NONE', #2372, 0.08000000000000020983 ) ;
#144243 = COLOUR_RGB ( '', 0.08235294, 0.09019608, 0.10196078) ;
#144244 = DIRECTION ( 'NONE',  ( -1.000000000000000000, 0.000000000000000000, 0.000000000000000000 ) ) ;
#144245 = CARTESIAN_POINT ( 'NONE',  ( 4.311429529933403337, -1.718370896367764411, -1.154329086688666184 ) ) ;
#144247 = CARTESIAN_POINT ( 'NONE',  ( -1.364683531250012516, 1.342708333674755616, 0.7879004041258379498 ) ) ;
#144246 =( NAMED_UNIT ( * ) SI_UNIT ( $, .STERADIAN. ) SOLID_ANGLE_UNIT ( ) );
#144248 = EDGE_LOOP ( 'NONE', ( #97567, #100729, #122750, #206538, #48338, #11680, #183697, #4495, #57733, #187981, #59041 ) ) ;
#144249 = CARTESIAN_POINT ( 'NONE',  ( 4.114144448104863017, 0.1132377192244668207, 2.296027709189680799 ) ) ;
#144251 = ORIENTED_EDGE ( 'NONE', *, *, #138683, .F. ) ;
#144250 = CARTESIAN_POINT ( 'NONE',  ( 7.375272376154084597, 9.627570410311676596, -1.443375672974057666 ) ) ;
#144253 = CARTESIAN_POINT ( 'NONE',  ( -1.642778471874998480, -1.451041666188708446, 2.845375778867863303 ) ) ;
#144252 = CARTESIAN_POINT ( 'NONE',  ( 5.885648082108200896, 6.039213315313952002, 0.7216878364870328300 ) ) ;
#144254 = CARTESIAN_POINT ( 'NONE',  ( -7.681496476274705110, -5.295524846228442328, -7.873959529867720519 ) ) ;
#144255 = LINE ( 'NONE', #177777, #19768 ) ;
#144256 = CARTESIAN_POINT ( 'NONE',  ( 3.908095550721983447, 1.372505747409875632, -1.374073360379985065 ) ) ;
#144257 = VERTEX_POINT ( 'NONE', #171133 ) ;
#144258 = CARTESIAN_POINT ( 'NONE',  ( 10.35806617071623315, 11.18675807536486566, 0.000000000000000000 ) ) ;
#144259 = EDGE_CURVE ( 'NONE', #138814, #204988, #123471, .T. ) ;
#144260 = ORIENTED_EDGE ( 'NONE', *, *, #129599, .T. ) ;
#144261 = CARTESIAN_POINT ( 'NONE',  ( 4.851772015791367743, -1.356534033432246211, -1.348250844427544282 ) ) ;
#144262 = CARTESIAN_POINT ( 'NONE',  ( -3.174173815459254477, 6.085887121384163656, -0.9314628722868825150 ) ) ;
#144263 = CARTESIAN_POINT ( 'NONE',  ( 6.739270712165630783, -1.537707103621160476, 0.7812997327944263271 ) ) ;
#144264 = CARTESIAN_POINT ( 'NONE',  ( 4.417204035549080920, -1.841734835922325120, 0.8216704330437708537 ) ) ;
#144265 = CARTESIAN_POINT ( 'NONE',  ( -1.115562610750309283E-14, 11.06250000000000178, 1.500000000000001554 ) ) ;
#144266 = CARTESIAN_POINT ( 'NONE',  ( 1.559489335033688251, -1.894147805384650995, -1.132260830144316888 ) ) ;
#144268 = DIRECTION ( 'NONE',  ( -0.5994789404140901112, 2.055006554627987857E-15, 0.8003905296791060664 ) ) ;
#144267 = CARTESIAN_POINT ( 'NONE',  ( -9.561524646135538319, 12.17819805862340310, -1.599625672291263179 ) ) ;
#144270 = CARTESIAN_POINT ( 'NONE',  ( 0.1273423419134401269, -1.083036363347224418, -1.400124042496312615 ) ) ;
#144269 = CARTESIAN_POINT ( 'NONE',  ( 1.183663948672460942, -0.9384196385337481017, 1.868258235111931898 ) ) ;
#144271 = CARTESIAN_POINT ( 'NONE',  ( 6.328750030911493241, 0.7691242348151774433, -1.864167186630163009 ) ) ;
#144273 = CARTESIAN_POINT ( 'NONE',  ( 2.801036929584544311, 1.937030572335847856, 1.225446795713614589 ) ) ;
#144272 = CARTESIAN_POINT ( 'NONE',  ( 5.061990249855835344, 6.999017606288844284, -1.599625672291273171 ) ) ;
#144274 = CARTESIAN_POINT ( 'NONE',  ( 0.5502397958263847144, -1.467719461762364341, -0.9348402994967041080 ) ) ;
#144275 = CARTESIAN_POINT ( 'NONE',  ( 6.772456105771886392, -7.184999792969689381, 6.662120174140257589 ) ) ;
#144276 = CARTESIAN_POINT ( 'NONE',  ( 1.440355836138224932, 1.027696236922505557, 1.396268056379332378 ) ) ;
#144277 = CARTESIAN_POINT ( 'NONE',  ( 1.360316468749989793, 0.8177083336747339448, -0.7853790794159001276 ) ) ;
#144278 = CARTESIAN_POINT ( 'NONE',  ( 1.311231623020674419, -1.711955697424736744, 1.335301017299495685 ) ) ;
#144279 = CARTESIAN_POINT ( 'NONE',  ( 2.676970549635893537, 1.727063564601112100, -1.040793759654296213 ) ) ;
#144281 = VECTOR ( 'NONE', #106083, 1000.000000000000000 ) ;
#144280 = CARTESIAN_POINT ( 'NONE',  ( 4.250000000000002665, 2.550977938801684432E-13, 2.052068128417944948 ) ) ;
#144282 = CARTESIAN_POINT ( 'NONE',  ( -1.499999999999997780, 1.931250000682817269, 0.000000000000000000 ) ) ;
#144283 = CARTESIAN_POINT ( 'NONE',  ( 0.2703664580724125521, -1.260843473572888396, 1.456531361591931972 ) ) ;
#144284 = CARTESIAN_POINT ( 'NONE',  ( 0.6823417656249934904, 12.69270833367473017, 1.181850606188764807 ) ) ;
#144285 = CARTESIAN_POINT ( 'NONE',  ( 2.935994361307178391, -2.139806239105252583, 0.5962572732955830901 ) ) ;
#144286 = ORIENTED_EDGE ( 'NONE', *, *, #87710, .T. ) ;
#144287 = CARTESIAN_POINT ( 'NONE',  ( 6.444907381559374926, -8.233136965322506384, 6.980013479859862535 ) ) ;
#144288 = CARTESIAN_POINT ( 'NONE',  ( -1.500000000000001332, -1.099999999999976108, 0.000000000000000000 ) ) ;
#144289 = CARTESIAN_POINT ( 'NONE',  ( 6.726816770674637347, 10.99970333242910669, -0.7998128361456291469 ) ) ;
#144290 = CARTESIAN_POINT ( 'NONE',  ( 5.970193594734433340, -1.655480682217812083, -0.5374289683400793605 ) ) ;
#144292 = CARTESIAN_POINT ( 'NONE',  ( 4.984793487045196869, 1.876812866478014596, 0.5713181500588762063 ) ) ;
#144291 = AXIS2_PLACEMENT_3D ( 'NONE', #97414, #148289, #163469 ) ;
#144294 = CARTESIAN_POINT ( 'NONE',  ( -6.236387472606158333, 7.338502141871059870, -1.082531754730544860 ) ) ;
#144293 = CARTESIAN_POINT ( 'NONE',  ( 4.142179624174931796, 4.791296635414242111, 1.199719254218464037 ) ) ;
#144295 = CARTESIAN_POINT ( 'NONE',  ( -1.495015925693001790, 4.335188216343587086, 0.1395187543289083953 ) ) ;
#144296 = CARTESIAN_POINT ( 'NONE',  ( 4.323666171361133514, -2.166671669000098444, 0.6512573085333557277 ) ) ;
#144297 = CARTESIAN_POINT ( 'NONE',  ( 2.559094272886554666, 1.658201776010211459, -1.226620081234103266 ) ) ;
#144298 = CARTESIAN_POINT ( 'NONE',  ( -7.691553217654356622, 7.867900263551875994, -0.7998128361456291469 ) ) ;
#144299 = VERTEX_POINT ( 'NONE', #6480 ) ;
#144300 = CARTESIAN_POINT ( 'NONE',  ( 0.7499999999999885647, 0.8479166673494853423, -1.299038105676652899 ) ) ;
#144301 = CARTESIAN_POINT ( 'NONE',  ( 3.145614842782416432, 0.6765965015090926737, -1.744060075730607950 ) ) ;
#144302 = CARTESIAN_POINT ( 'NONE',  ( 2.513978358999646723, -1.617321061556979300, 0.6262005117416250544 ) ) ;
#144303 = CARTESIAN_POINT ( 'NONE',  ( 6.146043800834426918, 0.6857851511376764631, 2.081541312870714311 ) ) ;
#144304 = CARTESIAN_POINT ( 'NONE',  ( 0.6224627697807674220, -1.182292326766160251, -1.863150505713019989 ) ) ;
#144305 = CARTESIAN_POINT ( 'NONE',  ( 3.819328725847204620, -0.1613130240520690706, 2.155748724213396361 ) ) ;
#144306 = CARTESIAN_POINT ( 'NONE',  ( 4.488185891274095063, -0.4267898533511414461, -1.894319381339019559 ) ) ;
#144307 = CARTESIAN_POINT ( 'NONE',  ( -3.755245360860931303, 5.404205559136275205, -1.443375672974051449 ) ) ;
#144308 = CARTESIAN_POINT ( 'NONE',  ( 6.966220764712143243, 6.002124920821316323, -2.420000000000000373 ) ) ;
#144309 = CARTESIAN_POINT ( 'NONE',  ( 4.943270704524102221, 6.626842455454077907, 1.245637569283185586 ) ) ;
#144310 = CARTESIAN_POINT ( 'NONE',  ( 3.919715808126649659, 7.587102519540811940, 0.000000000000000000 ) ) ;
#144311 = EDGE_CURVE ( 'NONE', #204270, #134155, #57678, .T. ) ;
#144312 = CARTESIAN_POINT ( 'NONE',  ( -1.360316468750008667, 2.369791667008076974, -0.7853790794159001276 ) ) ;
#144313 = CARTESIAN_POINT ( 'NONE',  ( 6.205703963786828758, 1.882472927010571118, 0.7231429968634556227 ) ) ;
#144314 = CARTESIAN_POINT ( 'NONE',  ( -8.143643823302737061, 12.65266822716189843, 0.000000000000000000 ) ) ;
#144315 = CARTESIAN_POINT ( 'NONE',  ( 6.747154001095143627, 11.02343010125301959, -0.7998128361456291469 ) ) ;
#144316 = CARTESIAN_POINT ( 'NONE',  ( 2.679285714285720044, -0.4970443252110337551, -0.09999999999999592548 ) ) ;
#144317 = CARTESIAN_POINT ( 'NONE',  ( 2.859763506297557711, 1.816872213737670938, -0.1792109616642542924 ) ) ;
#144318 = CARTESIAN_POINT ( 'NONE',  ( 2.028631293930313717, 1.270571802522667992, -1.804104215285810886 ) ) ;
#144319 = VERTEX_POINT ( 'NONE', #85616 ) ;
#144320 = CARTESIAN_POINT ( 'NONE',  ( -5.777182852754558340, 5.912670547734647286, 0.000000000000000000 ) ) ;
#144321 = CARTESIAN_POINT ( 'NONE',  ( 0.000000000000000000, -4.134374999522041350, -3.793834371823813001 ) ) ;
#144322 = CARTESIAN_POINT ( 'NONE',  ( -6.832419346282942563, 10.05857410638369487, 1.199719254218453823 ) ) ;
#144323 = CARTESIAN_POINT ( 'NONE',  ( 0.5451830133551841540, 0.1527301869948919366, 2.014097447171578903 ) ) ;
#144324 = CARTESIAN_POINT ( 'NONE',  ( 1.102369588802411426, -0.9501182663193027400, 1.895776817140030213 ) ) ;
#144325 = CARTESIAN_POINT ( 'NONE',  ( -6.120580001926503755, 6.105374521861167914, -0.7998128361456362523 ) ) ;
#144326 = CARTESIAN_POINT ( 'NONE',  ( 2.078732565759545903, 1.734175166166322501, 0.6755533923482255343 ) ) ;
#144327 = CARTESIAN_POINT ( 'NONE',  ( 3.506755287428983792, 7.242964935309132990, 1.040834085586084257E-14 ) ) ;
#144328 = CARTESIAN_POINT ( 'NONE',  ( 0.2335756976950612018, -1.975703151049061024, 0.8776370805363906680 ) ) ;
#144329 = CARTESIAN_POINT ( 'NONE',  ( -3.895595285070201808, 2.800000000000024691, 0.7750000000000135669 ) ) ;
#144330 = ORIENTED_EDGE ( 'NONE', *, *, #195285, .T. ) ;
#144331 = VERTEX_POINT ( 'NONE', #56326 ) ;
#144332 = CARTESIAN_POINT ( 'NONE',  ( -10.64723070543352712, 11.31619066596094392, 0.7998128361456462443 ) ) ;
#144333 = CARTESIAN_POINT ( 'NONE',  ( 3.598116246361187542, -1.823677485248562435, -0.08826725125678223927 ) ) ;
#144335 = CARTESIAN_POINT ( 'NONE',  ( -5.495703055830178485, 6.420018438214686540, -1.282350674470073448 ) ) ;
#144334 = CARTESIAN_POINT ( 'NONE',  ( -5.829079699232685208, 5.765290835385048496, 0.000000000000000000 ) ) ;
#144336 = CARTESIAN_POINT ( 'NONE',  ( 5.644368669187761256, 7.458116220610145675, 1.329639117314229235 ) ) ;
#144337 = CARTESIAN_POINT ( 'NONE',  ( 5.958361200765043719, 1.524811557412728114, 1.319025083221535333 ) ) ;
#144338 = CARTESIAN_POINT ( 'NONE',  ( 6.070224334863941529, -1.749758606415029449, -0.5730458292283467925 ) ) ;
#144339 = CARTESIAN_POINT ( 'NONE',  ( 0.07700591528349286230, 5.724620991219308230, -2.504819247423330175 ) ) ;
#144340 = CARTESIAN_POINT ( 'NONE',  ( 4.002764008144163554, -0.7221186334790052896, -2.191863981390995253 ) ) ;
#144341 = CARTESIAN_POINT ( 'NONE',  ( 4.505052181490820651, 8.477920988373101707, -0.7998128361456381397 ) ) ;
#144342 = CARTESIAN_POINT ( 'NONE',  ( 6.485629946217342123, 1.485420011660616657, 1.570608065930901187 ) ) ;
#144343 = CARTESIAN_POINT ( 'NONE',  ( 1.241630701082994559, 1.939900434848752964, 0.09377332689292780521 ) ) ;
#144344 = ORIENTED_EDGE ( 'NONE', *, *, #193336, .T. ) ;
#144345 = CARTESIAN_POINT ( 'NONE',  ( 4.235939456923387247, -2.142719978266393710, -0.8318502446633867509 ) ) ;
#144346 = CARTESIAN_POINT ( 'NONE',  ( -11.86145016429273014, 19.00000000000000000, -1.180000000000002158 ) ) ;
#144347 = CARTESIAN_POINT ( 'NONE',  ( -6.400331034103001748, 9.624747418832267698, 1.199719254218452935 ) ) ;
#144348 = CARTESIAN_POINT ( 'NONE',  ( 4.539837415608827698, 0.7997722286730184482, -1.691214532891088362 ) ) ;
#144349 = VERTEX_POINT ( 'NONE', #122486 ) ;
#144352 = CARTESIAN_POINT ( 'NONE',  ( -5.960744811863571968, 6.983232364376142698, 1.199719254218452935 ) ) ;
#144351 = CARTESIAN_POINT ( 'NONE',  ( -1.500000000000015099, 0.9104166673494835660, -0.8660254037844313801 ) ) ;
#144350 = CARTESIAN_POINT ( 'NONE',  ( 2.672007700615218528, 1.902801012812182169, -0.1915479950082218386 ) ) ;
#144353 = CARTESIAN_POINT ( 'NONE',  ( 4.389439674793148782, 1.972019932058775016, -0.9908447712502415072 ) ) ;
#144354 = EDGE_CURVE ( 'NONE', #78710, #21552, #101051, .T. ) ;
#144355 = CARTESIAN_POINT ( 'NONE',  ( -4.263518483283433191, 7.399640243518209815, 1.003058986863963220 ) ) ;
#144356 = CARTESIAN_POINT ( 'NONE',  ( 4.650083499362875017, 5.487814173087225633, 1.082531754730560403 ) ) ;
#144357 = CARTESIAN_POINT ( 'NONE',  ( 6.712695452097489301, 7.964471127936110229, -1.082531754730548412 ) ) ;
#144358 = CARTESIAN_POINT ( 'NONE',  ( -6.577113915960849155, 6.845923454808663600, -0.7216878364870338292 ) ) ;
#144359 = CARTESIAN_POINT ( 'NONE',  ( 1.528526583484477230, 1.898816187374774200, 0.5295601200957336108 ) ) ;
#144360 = CARTESIAN_POINT ( 'NONE',  ( 1.554236647822554218, 0.6679093176565461532, -2.208796357520240949 ) ) ;
#144361 = CARTESIAN_POINT ( 'NONE',  ( 2.348037267531626338, -0.8415878996531295231, 1.772339229757218471 ) ) ;
#144362 = CARTESIAN_POINT ( 'NONE',  ( 11.44786932348564257, 11.29999999999998117, 3.303370173849760061 ) ) ;
#144363 = CARTESIAN_POINT ( 'NONE',  ( 4.838768981748684972, -1.999376597400838174, -0.5061158833775216692 ) ) ;
#144364 = CARTESIAN_POINT ( 'NONE',  ( 3.389175213736285386, 6.897862149426897460, 0.7216878364870317197 ) ) ;
#144365 = CARTESIAN_POINT ( 'NONE',  ( 4.016958651398847557, 7.908478536599129249, -0.7998128361456362523 ) ) ;
#144366 = ORIENTED_EDGE ( 'NONE', *, *, #127165, .F. ) ;
#144367 =( BOUNDED_SURFACE ( )  B_SPLINE_SURFACE ( 3, 3, ( 
 ( #89085, #155141, #4574, #41406, #7793, #70648, #73886, #69582, #120579, #186556, #38185, #6722, #104257, #56573, #122732, #178865, #91222, #144271, #190813, #93358, #92302, #74951, #191879, #12072, #112849, #157283, #60829, #61902, #27251, #158346, #110716, #13134, #46737, #44601, #129124, #210264, #109662, #29408, #175664, #79211, #128063, #145329, #159395, #10994, #176716, #77069, #143199, #28329, #43539, #141062, #124847, #209189, #192949, #8872, #161547, #126990, #194019, #208131, #207069, #45669, #95500, #58699, #142118, #42473, #108583, #94425, #160464, #174611, #62955, #111786, #26187, #177792, #9940, #76015, #59760, #125920, #78140, #211330, #195101, #85339, #121134, #30476, #86411, #133058, #35511, #34446, #14184, #134128, #168722, #54981, #96561, #2994, #4058, #183900, #100521, #52837, #169787, #203328, #201197, #71196, #152478, #51790, #186022, #117907, #21376, #70128, #87484, #101589, #167657, #118973, #19257, #151421, #184951, #200137, #80277, #66917, #69062, #135182, #162608, #103736, #36578, #136241, #150356, #146375, #202262, #37659, #18184, #50705, #53912, #120048, #1926, #67985, #153550, #137312, #102664, #20325, #199059, #852, #116829, #182831, #5120, #166595, #84270, #73343, #187097, #104812, #140535, #175148, #109135, #142661, #74435, #155684, #26734, #92836, #170857, #124336, #206547, #22447, #6198, #158880, #10476, #56048, #91771, #38731, #72267, #208671, #125390, #60302, #156762, #190294, #41952, #122204, #205480, #139445, #108064, #57112, #106987, #138375, #174090, #40882, #204393, #25662, #157828, #173012, #90700, #8350, #23525, #105906, #58176, #9424, #88559, #188166, #154619, #191356, #39799, #75494, #141606, #207614, #171931, #123281, #189242, #59232, #24593, #43021, #89632, #76551, #7266, #11550, #129664, #195651, #46213, #29952, #162089, #177266, #45151, #96037, #147968, #28882, #213980, #27808, #128601, #13679, #176207, #98163, #163154, #110197, #80830, #192424, #93906, #44078, #77620, #112329, #146919, #196707, #178343, #126460, #159946, #179406, #143743, #194567, #127538, #209737, #12608, #47286, #61381, #193510, #79750, #97102, #62438, #111263, #145866, #48347, #81883, #211873, #164210, #31026, #144807, #64574, #210813, #114458, #14738, #180458, #63512, #113398, #212937, #130716, #32075, #15797, #78680, #94965, #161013, #51521, #167402, #131749, #135970, #67720, #168458, #182563, #65600, #20056, #69861, #50451, #82939, #86146, #152217, #34186, #100260, #102391, #169526, #84003, #166327, #165263, #153274, #21106, #33134, #201986, #133871, #3786, #17917, #197754, #49393, #18992, #53643, #119776, #87210, #85074, #150093, #185756, #37389, #115512, #2728, #151159, #181505, #99214, #103464, #16858, #149012, #199878, #66654, #588, #1664, #200927, #132800, #198803, #35245, #36312, #117646, #116569, #68801, #183639, #101320, #134921, #52575, #184692, #118704, #157567, #23252, #141346, #57910, #207361, #6996, #73074, #24321, #89365, #155413, #156496, #105626, #54709, #38465, #205206, #106719, #70930, #75236, #139175, #107802, #121931, #4851, #173827, #9160, #204122, #22171, #25404, #91506, #187898, #39528, #41691, #108870, #56848, #171655, #104541, #92583, #174893, #186833, #58981, #123020, #125137, #188971, #137039, #203066, #172746, #191094, #42763, #26473, #90427, #40615, #120860, #170586 ),
 ( #88286, #154350, #5928, #8085, #74174, #140266, #72000, #206286, #124075, #190039, #138111, #55774, #109940, #95778, #12347, #43823, #161834, #13422, #78427, #62192, #194315, #209473, #77363, #128348, #180207, #61115, #31829, #60046, #160752, #45956, #208412, #130464, #195392, #142404, #113137, #10222, #126201, #76296, #175949, #144549, #179144, #14477, #210556, #158625, #192163, #211612, #27545, #64320, #93640, #63248, #159683, #11284, #143477, #96847, #127275, #112077, #79497, #145616, #193247, #177005, #111000, #129409, #44894, #178078, #28622, #47022, #29696, #94710, #30767, #162894, #80566, #146665, #212679, #196454, #48097, #114209, #119529, #148768, #185515, #213729, #100016, #133623, #147711, #69619, #134681, #81626, #52335, #163965, #65352, #15541, #49146, #17668, #118463, #168215, #149846, #97904, #131499, #150916, #197503, #166080, #98959, #115262, #198554, #18743, #181255, #32882, #132555, #33941, #1415, #165010, #3549, #16605, #101069, #82686, #337, #84828, #184449, #83754, #117395, #67477, #199625, #51271, #183392, #135729, #66410, #201751, #34997, #50203, #116321, #182312, #167156, #2478, #68554, #200684, #36067, #102149, #19814, #85901, #151975, #53392, #121687, #186590, #153034, #154105, #169280, #103220, #55532, #156250, #25155, #123830, #155174, #21924, #24082, #88033, #120613, #70682, #187654, #37139, #202820, #136795, #41443, #73920, #172496, #72833, #20866, #5674, #39280, #105375, #138936, #140013, #204957, #38218, #86965, #54469, #206038, #104291, #6758, #171414, #4608, #23002, #89120, #170339, #71752, #189792, #74987, #203888, #137868, #56605, #57672, #107551, #122769, #157316, #188729, #40367, #106469, #90187, #7828, #173585, #91256, #8907, #141095, #207107, #58734, #124886, #96593, #42511, #125954, #11028, #127023, #28364, #108617, #162642, #158379, #194052, #190850, #191910, #177825, #145366, #192982, #210295, #44636, #94459, #12104, #160499, #14216, #27286, #80311, #61936, #9972, #93392, #92337, #59797, #95533, #78174, #144302, #128094, #45704, #76050, #174644, #111823, #29442, #60862, #43573, #142151, #159429, #26221, #208166, #209220, #161582, #178898, #62990, #13169, #175696, #79247, #77106, #109692, #143230, #110751, #176749, #211365, #129159, #195136, #46772, #112886, #30512, #146411, #212424, #64066, #148520, #165828, #166900, #83496, #131261, #47845, #15291, #196203, #163709, #16350, #115006, #82430, #32624, #31575, #197248, #132296, #3295, #181004, #179952, #98701, #51013, #84571, #130210, #35815, #167957, #97650, #81376, #86, #116064, #49943, #199367, #134429, #149578, #113956, #147460, #213481, #198302, #65105, #99760, #100815, #66151, #48887, #1162, #52079, #85637, #67225, #19561, #34742, #182054, #68296, #33684, #118206, #183137, #184193, #17412, #133360, #117134, #18492, #150658, #2221, #200432, #164760, #101892, #151723, #171153, #135472, #139753, #71500, #172237, #186327, #69363, #23825, #73654, #54213, #86706, #89930, #155981, #37962, #104035, #106211, #173311, #87775, #170081, #169020, #157058, #24890, #36879, #205778, #137611, #7568, #21668, #201493, #53139, #22743, #57406, #123572, #90995, #88861, #153850, #189534, #41182, #119270, #6500, #154916, #185255, #102961, #107289, #20618, #152775, #188467, #4357, #70425, #136542, #202561, #120351, #39029, #72575, #138675, #5421 ),
 ( #203627, #204695, #55278, #121427, #187397, #105112, #56345, #122506, #40099, #93131, #9715, #92066, #95266, #46500, #175438, #125690, #60598, #29176, #177564, #109432, #128886, #159170, #158124, #27023, #10770, #25961, #191648, #43313, #76844, #62725, #161314, #112624, #12898, #75791, #126756, #142963, #8647, #208965, #192717, #141899, #207909, #78977, #178634, #44371, #110494, #176493, #145097, #211101, #28104, #194867, #94199, #59530, #160239, #11838, #77916, #144035, #210031, #61672, #30246, #96330, #74726, #127840, #140831, #206844, #193792, #45441, #111555, #58476, #124631, #190589, #42246, #108359, #174381, #163449, #149322, #116879, #164507, #181801, #98442, #65901, #198056, #214268, #134173, #213231, #68033, #33434, #129958, #64863, #63800, #31315, #66968, #132047, #49686, #115813, #99511, #195946, #80047, #83237, #165568, #32377, #97393, #47582, #131008, #146150, #13963, #180750, #133107, #150401, #34494, #17163, #147206, #900, #197000, #15029, #113696, #16091, #162385, #179700, #81121, #166641, #199105, #50750, #182878, #212166, #48635, #82175, #148269, #100568, #18232, #84316, #114752, #1969, #200181, #51834, #117952, #183947, #35557, #202308, #4107, #3040, #102710, #103784, #192206, #152522, #151469, #70176, #22493, #56095, #101637, #7314, #139496, #69109, #135231, #120096, #87531, #21422, #170901, #105956, #55028, #167703, #186073, #168768, #185001, #188210, #205524, #53958, #136288, #153598, #122251, #39849, #37708, #73393, #169835, #36626, #5169, #71243, #119020, #137359, #203376, #121177, #155730, #171980, #57158, #88605, #126246, #19305, #20373, #187146, #38775, #104857, #85385, #201244, #52885, #154661, #86458, #6247, #72316, #23572, #138421, #204441, #89681, #161878, #79541, #95819, #15579, #94752, #164003, #63293, #11327, #160800, #159728, #127320, #162938, #13465, #145659, #211655, #129453, #77405, #175994, #179186, #195436, #128390, #193290, #143522, #12391, #27588, #109984, #62232, #14519, #31870, #130507, #47065, #28667, #30809, #78470, #44935, #209518, #194357, #43868, #61158, #111043, #48136, #80613, #96889, #113182, #93686, #144589, #46000, #112119, #146706, #212722, #64361, #177050, #210603, #178122, #29737, #196494, #114250, #180246, #97949, #81666, #147752, #213770, #65391, #131538, #33978, #32921, #100053, #118500, #152009, #197540, #103255, #20900, #98997, #165052, #1449, #183429, #117431, #52371, #201787, #150951, #70716, #3581, #198592, #101104, #51306, #49185, #35030, #16644, #115304, #199660, #82728, #167190, #168251, #133659, #50239, #2515, #119564, #153069, #68588, #86996, #102184, #67514, #135764, #18777, #185551, #36099, #37180, #84863, #134713, #200720, #184482, #19850, #85937, #83789, #148805, #374, #69656, #53427, #181294, #169316, #4646, #66448, #166117, #132590, #116359, #182349, #17702, #149884, #91296, #25192, #39318, #105413, #173620, #26254, #155209, #171451, #21962, #10008, #92371, #104327, #58768, #138973, #75023, #23040, #136829, #54503, #90219, #124922, #190884, #158408, #24116, #89156, #42550, #108653, #120647, #73955, #156283, #186626, #170375, #174681, #202855, #5711, #41477, #38253, #88070, #154143, #141135, #71788, #106505, #140047, #206072, #137903, #6790, #72867, #57706, #204996, #56640, #203922, #123863, #122804, #55570, #189828, #107587, #188763, #40403, #172532 ),
 ( #157354, #121724, #8943, #187689, #7867, #207145, #27326, #210337, #96630, #146449, #128130, #163748, #76084, #129200, #175733, #78214, #77145, #59833, #159467, #195177, #45743, #111861, #29478, #95569, #109726, #208200, #211403, #161619, #160535, #11066, #191943, #193022, #125986, #142185, #94497, #46810, #64108, #162684, #194093, #60901, #63033, #127060, #143266, #93428, #12141, #43608, #209256, #44674, #80349, #112924, #178937, #177866, #110786, #176788, #144337, #61976, #13212, #30551, #79285, #28403, #145403, #14258, #212464, #130250, #196241, #47884, #113997, #179992, #31615, #97690, #17453, #103001, #66193, #65142, #132338, #150699, #184229, #15327, #135509, #53180, #131298, #197289, #33724, #1201, #149619, #84610, #19603, #183177, #81417, #35853, #16391, #133402, #83537, #147498, #67263, #99802, #82470, #98741, #101931, #119308, #182093, #198344, #199407, #167997, #85675, #116102, #201532, #165867, #164799, #51052, #117175, #32662, #49984, #34781, #100855, #69402, #151763, #185294, #2261, #36918, #213519, #148560, #166940, #18533, #68337, #48929, #115048, #181046, #134469, #126, #200472, #52119, #3332, #118247, #188506, #105152, #72616, #204732, #6538, #140870, #5458, #74767, #40137, #136580, #71538, #70463, #56382, #86744, #137648, #171192, #187438, #122545, #205817, #106250, #170119, #152814, #54253, #20654, #202600, #55317, #153889, #121468, #203668, #120390, #21705, #22782, #42286, #39066, #4392, #88899, #89968, #123610, #169057, #206882, #58514, #186365, #38000, #154953, #138715, #172274, #23861, #173351, #156020, #104072, #189573, #87817, #7608, #73692, #139790, #57449, #41221, #107326, #24932, #91036, #124669, #157096, #8685, #190626, #177605, #111596, #159207, #145135, #143003, #59571, #10808, #76883, #207949, #27065, #175478, #209001, #79018, #29217, #62763, #144077, #211141, #174422, #125729, #93172, #60638, #192756, #25998, #128925, #9753, #11880, #108398, #126800, #193830, #95307, #44413, #77956, #110532, #28144, #160278, #176532, #194904, #94239, #46541, #210073, #191690, #61712, #141936, #43350, #161356, #127880, #45480, #12939, #92107, #109470, #75829, #158162, #172974, #171891, #22412, #203295, #204352, #5083, #153514, #105865, #206509, #75458, #174053, #205440, #72229, #74398, #138336, #170821, #121094, #23488, #87445, #38694, #187061, #91738, #124299, #8313, #39760, #56010, #139406, #108027, #41916, #188129, #207579, #89595, #88521, #155644, #7228, #104772, #122162, #73304, #57076, #141571, #25626, #125355, #140499, #59199, #71158, #154583, #123240, #189205, #40842, #137275, #191318, #54942, #90660, #6160, #106951, #58140, #157791, #24553, #156722, #190258, #9387, #42986, #109096, #175112, #193969, #192895, #111734, #60779, #9888, #208082, #160414, #61848, #26138, #30427, #176667, #62904, #77016, #174562, #129074, #178814, #159345, #191828, #195045, #46683, #143145, #209140, #211281, #63981, #44551, #126938, #59709, #47761, #130134, #142068, #96513, #28279, #112801, #110667, #92251, #158297, #128015, #162562, #14134, #196123, #45617, #94373, #80227, #146325, #75965, #177740, #29355, #125869, #43491, #212340, #109611, #175616, #79159, #27203, #93310, #10942, #12019, #78091, #144218, #95449, #161499, #210212, #13079, #145275, #183048, #6, #33604, #65024, #50926, #181973, #213403, #117051, #34663 ),
 ( #149493, #163627, #85546, #16263, #15208, #197169, #18406, #83411, #1076, #67141, #133275, #147376, #31495, #100733, #199283, #198222, #48805, #81299, #82347, #97570, #179870, #132213, #84482, #101802, #200346, #17330, #98617, #166812, #164678, #114922, #131179, #49858, #113875, #180921, #32542, #118121, #150572, #2134, #68210, #148438, #66071, #115985, #99674, #134341, #51995, #184106, #165744, #35726, #167871, #19469, #151636, #3203, #69272, #135386, #201407, #168932, #54125, #55189, #140744, #103949, #102874, #169991, #188373, #7480, #53046, #173223, #90904, #20535, #86617, #71407, #38939, #187312, #122414, #57320, #6410, #119179, #73562, #120262, #171061, #121336, #185165, #105022, #137519, #186237, #136454, #139663, #156967, #5327, #21577, #22657, #205684, #123485, #153756, #24802, #203536, #202472, #88768, #154825, #70337, #87683, #72482, #138583, #107198, #189448, #8558, #40011, #74637, #36789, #37871, #204606, #56257, #106122, #152685, #4267, #172145, #23737, #89843, #155892, #41090, #161219, #208874, #11748, #142872, #110402, #178537, #174293, #177472, #25868, #112524, #77823, #91978, #43226, #75700, #158036, #60504, #206755, #9623, #141814, #211007, #29086, #127746, #28012, #124542, #175353, #126664, #10680, #94110, #95170, #160151, #207817, #190499, #59445, #58386, #125602, #93041, #191562, #159083, #109343, #108272, #26933, #192629, #79952, #76751, #42157, #44281, #193703, #12806, #176406, #30147, #96236, #143944, #209940, #61578, #45347, #111466, #78879, #62630, #145002, #128790, #194771, #46408, #162286, #13874, #146055, #214175, #15995, #147113, #14930, #18131, #183851, #98346, #48543, #197960, #166543, #100468, #32280, #51736, #82081, #81025, #164411, #148173, #163355, #114661, #180655, #65802, #200087, #84220, #35463, #66865, #117859, #212069, #213139, #131949, #49589, #115713, #63707, #101541, #113598, #149222, #129864, #64769, #133010, #150308, #181703, #165469, #33333, #99415, #167610, #179601, #116781, #31222, #19208, #17065, #97296, #83144, #47488, #130911, #50655, #797, #199010, #182778, #34396, #196903, #195847, #1874, #67934, #134079, #20275, #201148, #202211, #2942, #151373, #103689, #204341, #73293, #171881, #203284, #70079, #72218, #135131, #118925, #71147, #187050, #69014, #155634, #87434, #188118, #53865, #85287, #39749, #89585, #136193, #102616, #105854, #23478, #119998, #185975, #122150, #189196, #169738, #37608, #184905, #172965, #40833, #52786, #7219, #153502, #139396, #21327, #36529, #168671, #38682, #205429, #57067, #106942, #104761, #5072, #123231, #86359, #152430, #22401, #170810, #4009, #137264, #54931, #121083, #88510, #55999, #154572, #6148, #138325, #177222, #112284, #208624, #176164, #93860, #174044, #42977, #191309, #159898, #125346, #158836, #190249, #27764, #92791, #124290, #11505, #77576, #10433, #142616, #60258, #75449, #157780, #126415, #46170, #141562, #24544, #140489, #26689, #192378, #74388, #210772, #61335, #8304, #193465, #90652, #206500, #156713, #41907, #76505, #45109, #94923, #44033, #58131, #108018, #143699, #25617, #110151, #91729, #9378, #207570, #59191, #209691, #109087, #127494, #111219, #175102, #28835, #160972, #12562, #194522, #78636, #62392, #144761, #128557, #119477, #196662, #103164, #19763, #169225, #49353, #163111, #65560, #197711, #48303, #118411, #64529 ),
 ( #102095, #135675, #178300, #86913, #4556, #79708, #145823, #114414, #164170, #98118, #36016, #185465, #131707, #54418, #201700, #179361, #81839, #32032, #29907, #15755, #180414, #30983, #47241, #53343, #70630, #130674, #80787, #147923, #37085, #20817, #213939, #152981, #184396, #113356, #168165, #85845, #195606, #146877, #212897, #151922, #136741, #202768, #95992, #3495, #162045, #13635, #97058, #69565, #211828, #63465, #129620, #14692, #87980, #123775, #120559, #121632, #107498, #74932, #122714, #139959, #56554, #24027, #92283, #154054, #91201, #5621, #26165, #205982, #71702, #22951, #21873, #203833, #25099, #90130, #156197, #73864, #57618, #137814, #38166, #41387, #189735, #204900, #55479, #187601, #89065, #104239, #186537, #138882, #157262, #108563, #207049, #7773, #105320, #173526, #171357, #39228, #155123, #188676, #170285, #6705, #72782, #124828, #8853, #141042, #58681, #40310, #106417, #172440, #190795, #42455, #174591, #158328, #9921, #75995, #142100, #208113, #93340, #80258, #130159, #111764, #147404, #59742, #112829, #159376, #61878, #60808, #43520, #27232, #191859, #128043, #10975, #29386, #30456, #210242, #126969, #79191, #196151, #15238, #13113, #97597, #178845, #78119, #212370, #144249, #47791, #96542, #113905, #145306, #44583, #161528, #211311, #193998, #62936, #160444, #109643, #77048, #45647, #129104, #125901, #179900, #177771, #162589, #176696, #175646, #14163, #64011, #110696, #143178, #146357, #31523, #28309, #94405, #163656, #81325, #95480, #12051, #209170, #192927, #195078, #46716, #135418, #1111, #151669, #99706, #213430, #131209, #166844, #201439, #53080, #168963, #100762, #182002, #119215, #185198, #197197, #150605, #18440, #48836, #32573, #36823, #102904, #82379, #118154, #65053, #98649, #20567, #3240, #86650, #183081, #2165, #68242, #148470, #17361, #165778, #134376, #83445, #133307, #164706, #200380, #67172, #16294, #52028, #184138, #199312, #117082, #34693, #49892, #132244, #84517, #114950, #116016, #180950, #38, #50958, #35762, #66102, #198252, #101837, #33633, #167905, #149525, #19503, #85579, #69306, #72521, #190537, #105060, #55224, #204640, #173259, #107238, #38974, #58423, #22689, #21611, #171098, #88802, #170025, #121370, #187345, #154861, #206791, #24840, #42193, #73596, #124576, #4300, #87719, #6443, #138617, #56291, #70371, #108308, #120297, #155929, #152718, #153792, #139698, #90939, #122451, #172182, #188410, #40047, #174328, #186270, #123519, #37906, #25904, #23772, #103982, #106156, #54158, #5361, #57356, #89877, #7514, #205721, #189483, #71443, #136486, #41126, #157005, #8591, #137555, #203573, #74673, #202508, #140776, #110439, #211042, #79991, #178577, #209974, #76788, #78917, #142910, #175385, #125637, #28053, #92014, #43260, #191598, #96275, #128827, #12843, #127785, #9660, #60544, #94146, #176441, #193740, #194809, #45386, #93076, #75736, #109378, #158072, #26971, #192663, #208910, #44317, #126702, #207854, #159118, #160185, #179642, #11786, #141849, #77860, #145039, #46445, #59480, #212106, #129902, #10719, #143983, #61615, #111502, #177508, #161256, #162325, #29120, #95207, #112566, #62668, #30185, #13909, #146095, #63743, #195886, #47524, #113637, #117898, #67976, #166586, #66908, #163394, #214214, #181743, #49627, #133048, #134119, #199050, #32317, #14968, #130952, #97336 ),
 ( #148212, #18175, #200128, #31262, #151412, #69053, #147151, #213176, #115752, #17103, #165511, #100511, #35503, #50696, #118964, #51781, #98385, #149264, #99454, #81065, #83181, #33373, #164449, #114698, #183891, #135173, #198001, #65843, #843, #101580, #167648, #131992, #2986, #116820, #180692, #182822, #34438, #48582, #84262, #150347, #1917, #85329, #19249, #201188, #52827, #64805, #196942, #16036, #82119, #121124, #22438, #36569, #90691, #152469, #188157, #184942, #186013, #171921, #139436, #187088, #204383, #38722, #88549, #156753, #4049, #155675, #70119, #8342, #56039, #136230, #87475, #86402, #53904, #89623, #154610, #6189, #138366, #122195, #202253, #102655, #105897, #39790, #54972, #120039, #37649, #153541, #168712, #20316, #203321, #7257, #173003, #57103, #72258, #169778, #23517, #21367, #103727, #5110, #104803, #71187, #137304, #170848, #189234, #73333, #205471, #123272, #40873, #106978, #24584, #74427, #140527, #206539, #58169, #208663, #59224, #25654, #26726, #41944, #190287, #142653, #28872, #112320, #210805, #27800, #109126, #111255, #175140, #207605, #157820, #60294, #124327, #75487, #9416, #128593, #161005, #45143, #159937, #108057, #92828, #126452, #192415, #11542, #12600, #77612, #125382, #174082, #141598, #91764, #191348, #10468, #158872, #76542, #44070, #43013, #110189, #176199, #211864, #93898, #143735, #209729, #177258, #78672, #61372, #29944, #162080, #127530, #193502, #94957, #144798, #62430, #194559, #46204, #178335, #96029, #13669, #79741, #145858, #131741, #63503, #197746, #147959, #64565, #146911, #150084, #101312, #15789, #180449, #115503, #83995, #17909, #164202, #183630, #213972, #212929, #81875, #65592, #80821, #32066, #98155, #49384, #117638, #1655, #167393, #198794, #35237, #129657, #130708, #97092, #33126, #199870, #82931, #51513, #18984, #16848, #85065, #182555, #181498, #67712, #99206, #151151, #116562, #195641, #149004, #48339, #165255, #580, #66646, #132791, #50443, #113389, #34179, #114450, #100251, #166320, #133863, #47277, #179398, #31018, #163145, #14729, #196699, #68792, #73067, #4841, #105618, #119767, #2720, #171647, #6987, #201978, #20049, #23244, #89356, #185747, #37380, #39518, #106710, #21098, #103455, #102383, #90418, #172736, #184684, #139166, #70920, #155404, #169517, #134912, #200919, #170578, #205197, #56838, #24312, #104532, #87201, #123011, #188963, #52567, #154341, #22161, #118698, #36304, #40605, #168450, #86137, #121923, #152208, #3778, #69852, #135962, #53634, #186825, #5919, #71991, #153266, #137031, #203058, #138103, #54701, #120851, #38455, #204113, #88276, #55765, #187890, #159674, #76287, #60038, #192154, #207353, #75229, #126191, #178069, #58973, #29687, #57902, #158616, #43817, #206279, #128341, #193239, #140257, #110992, #8076, #124066, #74164, #107795, #142396, #176997, #12339, #208404, #156487, #190031, #209465, #41684, #10213, #157559, #173820, #25398, #91498, #109932, #9152, #125128, #141339, #175941, #78419, #27537, #144541, #112068, #93632, #194307, #61108, #174885, #94703, #26465, #210548, #127268, #62184, #28613, #191086, #42755, #108859, #92574, #11276, #160744, #45948, #77355, #143468, #44886, #148762, #195382, #97898, #96839, #79489, #63240, #13414, #163957, #129402, #146657, #47014, #65345, #17662, #115255, #83747, #51265, #49139, #133617 ) ),
 .UNSPECIFIED., .T., .F., .T. ) 
 B_SPLINE_SURFACE_WITH_KNOTS ( ( 4, 3, 4 ),
 ( 4, 1, 1, 1, 1, 1, 1, 1, 1, 1, 1, 1, 1, 1, 1, 1, 1, 1, 1, 1, 1, 1, 1, 1, 1, 1, 1, 1, 1, 1, 1, 1, 1, 1, 1, 1, 1, 1, 1, 1, 1, 1, 1, 1, 1, 1, 1, 1, 1, 1, 1, 1, 1, 1, 1, 1, 1, 1, 1, 1, 1, 1, 1, 1, 1, 1, 1, 1, 1, 1, 1, 1, 1, 1, 1, 1, 1, 1, 1, 1, 1, 1, 1, 1, 1, 1, 1, 1, 1, 1, 1, 1, 1, 1, 1, 1, 1, 1, 1, 1, 1, 1, 1, 1, 1, 1, 1, 1, 1, 1, 1, 1, 1, 1, 1, 1, 1, 1, 1, 1, 1, 1, 1, 1, 1, 1, 1, 1, 1, 1, 1, 1, 1, 1, 1, 1, 1, 1, 1, 1, 1, 1, 1, 1, 1, 1, 1, 1, 1, 1, 1, 1, 1, 1, 1, 1, 1, 1, 1, 1, 1, 1, 1, 1, 1, 1, 1, 1, 1, 1, 1, 1, 1, 1, 1, 1, 1, 1, 1, 1, 1, 1, 1, 1, 1, 1, 1, 1, 1, 1, 1, 1, 1, 1, 1, 1, 1, 1, 1, 1, 1, 1, 1, 1, 1, 1, 1, 1, 1, 1, 1, 1, 1, 1, 1, 1, 1, 1, 1, 1, 1, 1, 1, 1, 1, 1, 1, 1, 1, 1, 1, 1, 1, 1, 1, 1, 1, 1, 1, 1, 1, 1, 1, 1, 1, 1, 1, 1, 1, 1, 1, 1, 1, 1, 1, 1, 1, 1, 1, 1, 1, 1, 1, 1, 1, 1, 1, 1, 1, 1, 1, 1, 1, 1, 1, 1, 1, 1, 1, 1, 1, 1, 1, 1, 1, 1, 1, 1, 1, 1, 1, 1, 1, 1, 1, 1, 1, 1, 1, 1, 1, 1, 1, 1, 1, 1, 1, 1, 1, 1, 1, 1, 1, 1, 1, 1, 1, 1, 1, 1, 1, 1, 1, 1, 1, 1, 1, 1, 1, 1, 1, 1, 1, 1, 1, 1, 1, 1, 1, 1, 1, 1, 1, 1, 1, 1, 1, 1, 1, 1, 1, 1, 1, 1, 1, 1, 1, 1, 1, 1, 1, 1, 1, 1, 1, 1, 1, 1, 1, 1, 1, 1, 1, 1, 1, 1, 1, 1, 1, 1, 1, 1, 1, 1, 4 ),
 ( 0.000000000000000000, 0.5000000000000000000, 1.000000000000000000 ),
 ( 0.000000000000000000, 0.002600033395298661284, 0.005208813367820810773, 0.007813200023264601363, 0.01041635779573905213, 0.01302082523971277370, 0.01562491580351430334, 0.01822918961192645723, 0.02083333155136493989, 0.02343746137460561707, 0.02604174567981391505, 0.02864576082122225614, 0.03125012338981237453, 0.03385410379569547823, 0.03645843966640821554, 0.03906250599122108869, 0.04166672065998115043, 0.04427093656960304907, 0.04687500111868234121, 0.04947933663890847350, 0.05208331727515622817, 0.05468767913406928638, 0.05729168951085979872, 0.05989597295159828499, 0.06250011041458469752, 0.06510424634142775169, 0.06770853038940542745, 0.07031253939703428768, 0.07291690072920921362, 0.07552088074063932621, 0.07812521459448035221, 0.08072927904253822395, 0.08333349217322323643, 0.08593770650149938628, 0.08854176936806532061, 0.09114610329512429221, 0.09375008230893774885, 0.09635444258075796797, 0.09895845137230636912, 0.1015627332241899466, 0.1041668691376404637, 0.1067710034717011397, 0.1093752859901425123, 0.1119792934252105548, 0.1145836532378000650, 0.1171876317139315254, 0.1197919640503514460, 0.1223960270027875247, 0.1250002386107842423, 0.1276044514713231270, 0.1302085128224930721, 0.1328128452953424854, 0.1354168228245230532, 0.1380211816480703679, 0.1406251889951717071, 0.1432294693974442978, 0.1458336039016293884, 0.1484377367829480265, 0.1510420179109137340, 0.1536460239143070949, 0.1562503823458506746, 0.1588543594276481397, 0.1614586903853630351, 0.1640627519827278502, 0.1666669622076225599, 0.1692711737400035832, 0.1718752337163205746, 0.1744795648736557347, 0.1770835410591554138, 0.1796878985729436218, 0.1822919046164021839, 0.1848961837081005144, 0.1875003169431251615, 0.1901044485118078553, 0.1927087283883223978, 0.1953127331008320255, 0.1979170902898210183, 0.2005210661182068033, 0.2031253958358791578, 0.2057294562186703923, 0.2083336651999991573, 0.2109378755437518183, 0.2135419342857080849, 0.2161462642661750033, 0.2187502392488957503, 0.2213545955913898966, 0.2239586004719608947, 0.2265628783920732026, 0.2291670104979939837, 0.2317711408940984485, 0.2343754196581391558, 0.2369794232205082452, 0.2395837793053874898, 0.2421877540212369617, 0.2447920826374832270, 0.2473961419461526701, 0.2500003498234057431, 0.2526045591180144934, 0.2552086167660569949, 0.2578129457082574683, 0.2604169196290564980, 0.2630212749386780513, 0.2656252787970727613, 0.2682295556845439854, 0.2708336868013750398, 0.2734378161649161920, 0.2760420939554183439, 0.2786460965083475960, 0.2812504516275206035, 0.2838544253716674404, 0.2864587530250631842, 0.2890628114000217685, 0.2916670183126490179, 0.2942712266975582858, 0.2968752833920936807, 0.2994796114345903981, 0.3020835844342854570, 0.3046879388494173613, 0.3072919418263086455, 0.3098962178200457829, 0.3125003480877632800, 0.3151044765587182606, 0.3177087535145803887, 0.3203127551987332566, 0.3229171094905676220, 0.3255210824038090589, 0.3281254092328941829, 0.3307294668145174810, 0.3333336729019333866, 0.3359378805165532667, 0.3385419363979534357, 0.3411462636792753078, 0.3437502358986498918, 0.3463545895576419231, 0.3489585917936692261, 0.3515628670325462446, 0.3541669965910940188, 0.3567711243094072171, 0.3593754005694961839, 0.3619794015255044517, 0.3645837551283364619, 0.3671877273514386752, 0.3697920534947228832, 0.3723961104233561858, 0.3750003158249449187, 0.3776045228086560845, 0.3802085780172632101, 0.3828129046759103926, 0.3854168762557192984, 0.3880212292968930887, 0.3906252309326675998, 0.3932295055555311003, 0.3958336345448258409, 0.3984377616504144459, 0.4010420373535708016, 0.4036460377220391638, 0.4062503907741795706, 0.4088543624478828686, 0.4114586880438503846, 0.4140627444598136697, 0.4166669493149349202, 0.4192711558070936761, 0.4218752104832254046, 0.4244795366576747386, 0.4270835077386489487, 0.4296878603003031483, 0.4322918614764136302, 0.4348961356220873986, 0.4375002641820237570, 0.4401043908147829753, 0.4427086660998260093, 0.4453126660213379551, 0.4479170186610768045, 0.4505209899261007900, 0.4531253151132156320, 0.4557293711568096706, 0.4583335756048029785, 0.4609377817447468106, 0.4635418360287018591, 0.4661461618574116450, 0.4687501325802634344, 0.4713544848006788190, 0.4739584856576960492, 0.4765627594649867738, 0.4791668877354426925, 0.4817710140352507997, 0.4843752890409837031, 0.4869792886561065681, 0.4895836410217184742, 0.4921876120187673176, 0.4947919369354787933, 0.4973959927469893683, 0.5000001969271801183, 0.5026044028542325792, 0.5052084568862954539, 0.5078127825077110025, 0.5104167530131399344, 0.5130211050305848453, 0.5156251057090676104, 0.5182293793167697116, 0.5208335074376115870, 0.5234376335443351458, 0.5260419084095501185, 0.5286459078588399141, 0.5312502600885893322, 0.5338542309583571566, 0.5364585557431046370, 0.5390626114628084276, 0.5416668155145124564, 0.5442710213679887721, 0.5468750752884355970, 0.5494794008409938924, 0.5520833712696913143, 0.5546877232224267651, 0.5572917238629264691, 0.5598959974098275394, 0.5625001255209155504, 0.5651042515744146844, 0.5677085264378984863, 0.5703125258619060611, 0.5729168780940517847, 0.5755208489772277725, 0.5781251737684461878, 0.5807292295366155432, 0.5833334335991446906, 0.5859376395183565345, 0.5885416934674594369, 0.5911460190895951872, 0.5937499895822500040, 0.5963543416085342885, 0.5989583423516006144, 0.6015626159764864145, 0.6041667442176794633, 0.6067708703578130747, 0.6093751453583519107, 0.6119791448976270587, 0.6145834972704286026, 0.6171874683077025470, 0.6197917932438269384, 0.6223958492007358734, 0.6250000534134032559, 0.6276042595376638555, 0.6302083136556971832, 0.6328126394858472059, 0.6354166101831504321, 0.6380209624212449526, 0.6406249634074311361, 0.6432292372490908683, 0.6458333657602520761, 0.6484374921268833969, 0.6510417674032679125, 0.6536457671983656459, 0.6562501198500874100, 0.6588540911821543222, 0.6614584164016259482, 0.6640624726875546946, 0.6666666771896793131, 0.6692708836583093346, 0.6718749380855545406, 0.6744792642621626477, 0.6770832353048136243, 0.6796875878929879988, 0.6822915892628557133, 0.6848958634600870177, 0.6874999923810890534, 0.6901041191140900866, 0.6927083948051209195, 0.6953123949966061312, 0.6979167480655225075, 0.7005207198330885010, 0.7031250454743595002, 0.7057291022295995031, 0.7083333071605121267, 0.7109375141128444486, 0.7135415689895947544, 0.7161458956511181917, 0.7187498671798290273, 0.7213542202563657524, 0.7239582221504904380, 0.7265624968421051655, 0.7291666263128349090, 0.7317707535520923123, 0.7343750297965853102, 0.7369790305250381035, 0.7395833841494394711, 0.7421873564932268685, 0.7447916826947649227, 0.7473957400596251688, 0.7499999455586733310, 0.7526041531340577073, 0.7552082086006238759, 0.7578125358855373195, 0.7604165080410384414, 0.7630208617442386654, 0.7656248643032155243, 0.7682291396280439555, 0.7708332697884082707, 0.7734373976738285750, 0.7760416746106194585, 0.7786456760166404756, 0.7812500303348380859, 0.7838540033955903041, 0.7864583302958847444, 0.7890623884106959807, 0.7916665946172487534, 0.7942708029550582527, 0.7968748591517740287, 0.7994791871985751364, 0.8020831601216208417, 0.8046875145898089166, 0.8072915179542569097, 0.8098957940511537501, 0.8124999250410844809, 0.8151040537125986418, 0.8177083314805486669, 0.8203123337047645292, 0.8229166888550945025, 0.8255206627735817149, 0.8281249905111484066, 0.8307290495162685806, 0.8333332565697225691, 0.8359374658093579047, 0.8385415228765847884, 0.8411458518237998616, 0.8437498256551729803, 0.8463541810267020127, 0.8489581853372698550, 0.8515624623451190089, 0.8541665943045783083, 0.8567707239021479237, 0.8593750026401490993, 0.8619790058232168484, 0.8645833619440471685, 0.8671873368610717447, 0.8697916655744575287, 0.8723957256102774505, 0.8749999336500613456, 0.8776041439309557601, 0.8802082020090884473, 0.8828125319952765393, 0.8854165068757942070, 0.8880208632890512765, 0.8906248686864229880, 0.8932291467441429988, 0.8958332798131283248, 0.8984374104767501867, 0.9010416903237299380, 0.9036456946063434748, 0.9062500518360779855, 0.9088540278924787108, 0.9114583577202677311, 0.9140624189272162914, 0.9166666280927961985, 0.9192708395544209043, 0.9218748987838942810, 0.9244792299476556341, 0.9270832060181642964, 0.9296875636115721209, 0.9322915702365133228, 0.9348958494830461596, 0.9374999838014769216, 0.9401041156712998115, 0.9427083967663798525, 0.9453124022892170908, 0.9479167607665550666, 0.9505207380999710631, 0.9531250691809918241, 0.9557291317261836783, 0.9583333421310490374, 0.9609375547886240820, 0.9635416155522130710, 0.9661459483928183101, 0.9687499245033458495, 0.9713542829945021051, 0.9739582954330652242, 0.9765625745907361432, 0.9791667024412501474, 0.9817708385604039245, 0.9843751096149007118, 0.9869791944699233266, 0.9895836584107432499, 0.9921868132917668337, 0.9947911946869415489, 0.9973999724172807335, 1.000000000000000000 ),
 .UNSPECIFIED. ) 
 GEOMETRIC_REPRESENTATION_ITEM ( )  RATIONAL_B_SPLINE_SURFACE ( (
 ( 1.000000000000000000, 1.000000000000000000, 1.000000000000000000, 0.9999999999999997780, 1.000000000000000000, 1.000000000000000000, 1.000000000000000000, 1.000000000000000222, 1.000000000000000000, 1.000000000000000000, 1.000000000000000222, 0.9999999999999997780, 1.000000000000000222, 1.000000000000000222, 1.000000000000000000, 1.000000000000000000, 1.000000000000000000, 0.9999999999999997780, 1.000000000000000222, 0.9999999999999996669, 1.000000000000000222, 1.000000000000000000, 1.000000000000000000, 0.9999999999999996669, 1.000000000000000444, 0.9999999999999996669, 1.000000000000000444, 1.000000000000000000, 1.000000000000000000, 0.9999999999999997780, 1.000000000000000222, 0.9999999999999994449, 1.000000000000000444, 1.000000000000000000, 1.000000000000000000, 1.000000000000000000, 1.000000000000000000, 1.000000000000000444, 0.9999999999999997780, 1.000000000000000000, 1.000000000000000000, 1.000000000000000000, 1.000000000000000000, 1.000000000000000000, 1.000000000000000000, 0.9999999999999997780, 1.000000000000000000, 1.000000000000000444, 0.9999999999999997780, 1.000000000000000444, 0.9999999999999997780, 0.9999999999999997780, 1.000000000000000000, 1.000000000000000222, 1.000000000000000000, 1.000000000000000000, 1.000000000000000000, 1.000000000000000000, 0.9999999999999997780, 1.000000000000000444, 0.9999999999999997780, 1.000000000000000000, 1.000000000000000222, 0.9999999999999997780, 1.000000000000000000, 1.000000000000000222, 0.9999999999999997780, 1.000000000000000222, 1.000000000000000000, 1.000000000000000222, 1.000000000000000000, 1.000000000000000222, 0.9999999999999997780, 1.000000000000000000, 1.000000000000000222, 1.000000000000000000, 1.000000000000000222, 0.9999999999999997780, 1.000000000000000222, 0.9999999999999997780, 1.000000000000000222, 0.9999999999999997780, 1.000000000000000222, 1.000000000000000222, 0.9999999999999997780, 1.000000000000000222, 1.000000000000000222, 0.9999999999999997780, 1.000000000000000222, 1.000000000000000000, 1.000000000000000000, 1.000000000000000222, 0.9999999999999996669, 1.000000000000000444, 0.9999999999999997780, 0.9999999999999997780, 1.000000000000000000, 1.000000000000000000, 1.000000000000000000, 0.9999999999999996669, 1.000000000000000444, 1.000000000000000000, 1.000000000000000222, 1.000000000000000000, 0.9999999999999997780, 1.000000000000000222, 0.9999999999999997780, 1.000000000000000222, 1.000000000000000000, 1.000000000000000000, 1.000000000000000222, 1.000000000000000000, 1.000000000000000222, 0.9999999999999994449, 1.000000000000000444, 1.000000000000000000, 0.9999999999999996669, 1.000000000000000222, 0.9999999999999997780, 1.000000000000000222, 0.9999999999999997780, 1.000000000000000000, 1.000000000000000000, 1.000000000000000000, 1.000000000000000000, 1.000000000000000000, 1.000000000000000444, 1.000000000000000000, 1.000000000000000000, 1.000000000000000222, 1.000000000000000000, 1.000000000000000000, 0.9999999999999997780, 1.000000000000000000, 1.000000000000000222, 1.000000000000000000, 1.000000000000000222, 0.9999999999999997780, 1.000000000000000000, 0.9999999999999997780, 0.9999999999999997780, 1.000000000000000222, 0.9999999999999997780, 1.000000000000000444, 0.9999999999999997780, 1.000000000000000000, 1.000000000000000222, 1.000000000000000000, 1.000000000000000000, 0.9999999999999997780, 1.000000000000000222, 1.000000000000000000, 1.000000000000000000, 1.000000000000000000, 1.000000000000000222, 0.9999999999999996669, 1.000000000000000222, 1.000000000000000222, 0.9999999999999996669, 1.000000000000000444, 0.9999999999999996669, 1.000000000000000000, 1.000000000000000222, 0.9999999999999996669, 1.000000000000000222, 1.000000000000000000, 1.000000000000000222, 1.000000000000000000, 1.000000000000000222, 0.9999999999999997780, 1.000000000000000444, 0.9999999999999997780, 0.9999999999999997780, 1.000000000000000222, 0.9999999999999996669, 1.000000000000000222, 1.000000000000000000, 1.000000000000000000, 1.000000000000000000, 0.9999999999999997780, 1.000000000000000222, 1.000000000000000222, 0.9999999999999997780, 1.000000000000000222, 0.9999999999999997780, 1.000000000000000222, 1.000000000000000000, 1.000000000000000444, 1.000000000000000000, 1.000000000000000222, 0.9999999999999996669, 1.000000000000000444, 0.9999999999999993339, 1.000000000000000444, 0.9999999999999997780, 1.000000000000000444, 0.9999999999999997780, 1.000000000000000000, 1.000000000000000000, 0.9999999999999997780, 1.000000000000000222, 0.9999999999999997780, 0.9999999999999996669, 1.000000000000000444, 1.000000000000000222, 1.000000000000000000, 0.9999999999999997780, 1.000000000000000222, 0.9999999999999996669, 1.000000000000000222, 0.9999999999999997780, 1.000000000000000222, 1.000000000000000000, 1.000000000000000000, 1.000000000000000000, 1.000000000000000000, 0.9999999999999997780, 1.000000000000000000, 1.000000000000000000, 0.9999999999999997780, 1.000000000000000000, 1.000000000000000000, 1.000000000000000000, 1.000000000000000222, 1.000000000000000000, 1.000000000000000444, 1.000000000000000222, 1.000000000000000000, 1.000000000000000000, 0.9999999999999997780, 1.000000000000000222, 1.000000000000000000, 1.000000000000000000, 1.000000000000000000, 0.9999999999999997780, 1.000000000000000222, 0.9999999999999997780, 1.000000000000000222, 1.000000000000000444, 0.9999999999999997780, 1.000000000000000222, 1.000000000000000000, 1.000000000000000000, 1.000000000000000000, 0.9999999999999997780, 1.000000000000000444, 0.9999999999999997780, 1.000000000000000222, 0.9999999999999997780, 1.000000000000000222, 0.9999999999999994449, 1.000000000000000222, 1.000000000000000000, 1.000000000000000222, 1.000000000000000000, 0.9999999999999997780, 1.000000000000000222, 1.000000000000000000, 0.9999999999999997780, 1.000000000000000444, 0.9999999999999996669, 1.000000000000000222, 1.000000000000000000, 1.000000000000000000, 1.000000000000000222, 0.9999999999999997780, 0.9999999999999997780, 1.000000000000000444, 1.000000000000000222, 1.000000000000000000, 0.9999999999999997780, 0.9999999999999997780, 1.000000000000000222, 1.000000000000000000, 1.000000000000000222, 1.000000000000000000, 0.9999999999999997780, 1.000000000000000000, 1.000000000000000000, 1.000000000000000000, 1.000000000000000222, 0.9999999999999997780, 1.000000000000000222, 1.000000000000000000, 1.000000000000000000, 1.000000000000000000, 0.9999999999999997780, 1.000000000000000000, 1.000000000000000222, 1.000000000000000222, 0.9999999999999996669, 1.000000000000000444, 0.9999999999999996669, 1.000000000000000222, 1.000000000000000000, 1.000000000000000222, 0.9999999999999997780, 1.000000000000000444, 1.000000000000000000, 1.000000000000000444, 0.9999999999999994449, 1.000000000000000222, 0.9999999999999997780, 0.9999999999999997780, 1.000000000000000000, 1.000000000000000222, 1.000000000000000000, 1.000000000000000000, 1.000000000000000000, 1.000000000000000222, 0.9999999999999996669, 1.000000000000000222, 1.000000000000000000, 0.9999999999999996669, 1.000000000000000444, 1.000000000000000000, 1.000000000000000000, 1.000000000000000000, 0.9999999999999996669, 1.000000000000000222, 1.000000000000000000, 1.000000000000000000, 1.000000000000000222, 0.9999999999999997780, 0.9999999999999997780, 1.000000000000000000, 1.000000000000000000, 1.000000000000000222, 0.9999999999999997780, 1.000000000000000222, 1.000000000000000000, 1.000000000000000000, 0.9999999999999996669, 1.000000000000000222, 1.000000000000000000, 1.000000000000000222, 1.000000000000000000, 1.000000000000000000, 1.000000000000000000, 0.9999999999999997780, 1.000000000000000222, 0.9999999999999996669, 1.000000000000000444, 1.000000000000000000, 0.9999999999999997780, 1.000000000000000000, 1.000000000000000222, 1.000000000000000222, 0.9999999999999996669, 1.000000000000000000, 1.000000000000000000, 0.9999999999999997780, 1.000000000000000222, 1.000000000000000000, 1.000000000000000222, 0.9999999999999996669, 1.000000000000000444, 1.000000000000000000, 1.000000000000000000, 1.000000000000000000, 1.000000000000000222, 1.000000000000000000, 0.9999999999999997780, 1.000000000000000444, 1.000000000000000000, 1.000000000000000444, 0.9999999999999997780, 1.000000000000000444, 1.000000000000000000, 1.000000000000000222, 1.000000000000000222, 1.000000000000000000, 0.9999999999999996669, 1.000000000000000000, 1.000000000000000000, 1.000000000000000000, 1.000000000000000000, 1.000000000000000222, 0.9999999999999996669, 1.000000000000000000, 1.000000000000000222, 0.9999999999999997780, 0.9999999999999997780, 1.000000000000000000, 1.000000000000000000, 1.000000000000000000, 1.000000000000000000),
 ( 0.3333333333333333703, 0.3333333333333333703, 0.3333333333333333703, 0.3333333333333333148, 0.3333333333333333703, 0.3333333333333333148, 0.3333333333333333703, 0.3333333333333334259, 0.3333333333333333703, 0.3333333333333333148, 0.3333333333333334259, 0.3333333333333332593, 0.3333333333333334259, 0.3333333333333333703, 0.3333333333333333703, 0.3333333333333332593, 0.3333333333333334259, 0.3333333333333333148, 0.3333333333333334259, 0.3333333333333333148, 0.3333333333333334259, 0.3333333333333334259, 0.3333333333333333148, 0.3333333333333333148, 0.3333333333333334814, 0.3333333333333332593, 0.3333333333333334259, 0.3333333333333334259, 0.3333333333333333703, 0.3333333333333333703, 0.3333333333333334814, 0.3333333333333332038, 0.3333333333333334814, 0.3333333333333333703, 0.3333333333333334259, 0.3333333333333333148, 0.3333333333333334259, 0.3333333333333334814, 0.3333333333333333703, 0.3333333333333332593, 0.3333333333333334259, 0.3333333333333333148, 0.3333333333333333148, 0.3333333333333333703, 0.3333333333333333703, 0.3333333333333334259, 0.3333333333333333148, 0.3333333333333335369, 0.3333333333333333148, 0.3333333333333334259, 0.3333333333333333703, 0.3333333333333332038, 0.3333333333333334259, 0.3333333333333334259, 0.3333333333333333148, 0.3333333333333334259, 0.3333333333333333703, 0.3333333333333333703, 0.3333333333333334259, 0.3333333333333334259, 0.3333333333333333703, 0.3333333333333334259, 0.3333333333333334259, 0.3333333333333333148, 0.3333333333333333703, 0.3333333333333333703, 0.3333333333333333148, 0.3333333333333334259, 0.3333333333333333148, 0.3333333333333334814, 0.3333333333333333703, 0.3333333333333334259, 0.3333333333333333148, 0.3333333333333333703, 0.3333333333333334259, 0.3333333333333333703, 0.3333333333333333703, 0.3333333333333333148, 0.3333333333333334259, 0.3333333333333333148, 0.3333333333333334259, 0.3333333333333333703, 0.3333333333333334259, 0.3333333333333334814, 0.3333333333333333148, 0.3333333333333334259, 0.3333333333333334259, 0.3333333333333333148, 0.3333333333333333703, 0.3333333333333333703, 0.3333333333333333148, 0.3333333333333334814, 0.3333333333333332593, 0.3333333333333334259, 0.3333333333333333703, 0.3333333333333333148, 0.3333333333333333703, 0.3333333333333333703, 0.3333333333333334259, 0.3333333333333333148, 0.3333333333333334259, 0.3333333333333333148, 0.3333333333333334814, 0.3333333333333333148, 0.3333333333333333148, 0.3333333333333334259, 0.3333333333333333148, 0.3333333333333333703, 0.3333333333333333703, 0.3333333333333334259, 0.3333333333333333703, 0.3333333333333334259, 0.3333333333333333703, 0.3333333333333332593, 0.3333333333333334259, 0.3333333333333333703, 0.3333333333333333148, 0.3333333333333334814, 0.3333333333333333148, 0.3333333333333334259, 0.3333333333333334259, 0.3333333333333333148, 0.3333333333333333703, 0.3333333333333334259, 0.3333333333333333703, 0.3333333333333333703, 0.3333333333333334259, 0.3333333333333333703, 0.3333333333333334259, 0.3333333333333333703, 0.3333333333333334259, 0.3333333333333333148, 0.3333333333333333703, 0.3333333333333333703, 0.3333333333333333703, 0.3333333333333333703, 0.3333333333333335369, 0.3333333333333332593, 0.3333333333333333703, 0.3333333333333333703, 0.3333333333333332593, 0.3333333333333333703, 0.3333333333333333703, 0.3333333333333334259, 0.3333333333333332593, 0.3333333333333333703, 0.3333333333333333703, 0.3333333333333333703, 0.3333333333333333703, 0.3333333333333333703, 0.3333333333333334259, 0.3333333333333333148, 0.3333333333333334259, 0.3333333333333333703, 0.3333333333333334814, 0.3333333333333332593, 0.3333333333333333703, 0.3333333333333334814, 0.3333333333333332038, 0.3333333333333334259, 0.3333333333333333148, 0.3333333333333333703, 0.3333333333333334814, 0.3333333333333332038, 0.3333333333333334259, 0.3333333333333333703, 0.3333333333333333703, 0.3333333333333333703, 0.3333333333333334259, 0.3333333333333333703, 0.3333333333333335369, 0.3333333333333333148, 0.3333333333333333148, 0.3333333333333334259, 0.3333333333333333148, 0.3333333333333333703, 0.3333333333333333703, 0.3333333333333334259, 0.3333333333333333148, 0.3333333333333334259, 0.3333333333333332593, 0.3333333333333334814, 0.3333333333333333703, 0.3333333333333333703, 0.3333333333333333703, 0.3333333333333333703, 0.3333333333333333703, 0.3333333333333334259, 0.3333333333333333703, 0.3333333333333334259, 0.3333333333333333148, 0.3333333333333335369, 0.3333333333333332038, 0.3333333333333335369, 0.3333333333333333148, 0.3333333333333334259, 0.3333333333333333703, 0.3333333333333333148, 0.3333333333333334259, 0.3333333333333333148, 0.3333333333333334259, 0.3333333333333332593, 0.3333333333333333148, 0.3333333333333334259, 0.3333333333333334814, 0.3333333333333333703, 0.3333333333333333703, 0.3333333333333334259, 0.3333333333333333148, 0.3333333333333333703, 0.3333333333333333148, 0.3333333333333334259, 0.3333333333333333148, 0.3333333333333333703, 0.3333333333333333703, 0.3333333333333334259, 0.3333333333333333148, 0.3333333333333334259, 0.3333333333333333703, 0.3333333333333333148, 0.3333333333333332593, 0.3333333333333334259, 0.3333333333333333148, 0.3333333333333334259, 0.3333333333333334259, 0.3333333333333334814, 0.3333333333333334259, 0.3333333333333333703, 0.3333333333333333703, 0.3333333333333333148, 0.3333333333333334259, 0.3333333333333333703, 0.3333333333333334259, 0.3333333333333333148, 0.3333333333333333703, 0.3333333333333333703, 0.3333333333333332593, 0.3333333333333334259, 0.3333333333333335369, 0.3333333333333333148, 0.3333333333333334814, 0.3333333333333333703, 0.3333333333333333148, 0.3333333333333334259, 0.3333333333333332593, 0.3333333333333334814, 0.3333333333333333148, 0.3333333333333333703, 0.3333333333333333148, 0.3333333333333334259, 0.3333333333333333148, 0.3333333333333334259, 0.3333333333333333148, 0.3333333333333333703, 0.3333333333333333703, 0.3333333333333333148, 0.3333333333333334259, 0.3333333333333333703, 0.3333333333333333703, 0.3333333333333335369, 0.3333333333333332038, 0.3333333333333334814, 0.3333333333333333148, 0.3333333333333334259, 0.3333333333333334259, 0.3333333333333333703, 0.3333333333333333148, 0.3333333333333334814, 0.3333333333333333703, 0.3333333333333333703, 0.3333333333333333703, 0.3333333333333333703, 0.3333333333333333703, 0.3333333333333334259, 0.3333333333333333703, 0.3333333333333334259, 0.3333333333333333148, 0.3333333333333333703, 0.3333333333333334259, 0.3333333333333334259, 0.3333333333333333703, 0.3333333333333333703, 0.3333333333333334259, 0.3333333333333333703, 0.3333333333333333148, 0.3333333333333333148, 0.3333333333333333703, 0.3333333333333333703, 0.3333333333333334259, 0.3333333333333334259, 0.3333333333333333703, 0.3333333333333333703, 0.3333333333333333703, 0.3333333333333333703, 0.3333333333333333703, 0.3333333333333333148, 0.3333333333333334259, 0.3333333333333334259, 0.3333333333333333703, 0.3333333333333335369, 0.3333333333333332038, 0.3333333333333334814, 0.3333333333333332593, 0.3333333333333333703, 0.3333333333333332593, 0.3333333333333334814, 0.3333333333333333148, 0.3333333333333333703, 0.3333333333333334259, 0.3333333333333334259, 0.3333333333333332593, 0.3333333333333334259, 0.3333333333333333148, 0.3333333333333333703, 0.3333333333333334259, 0.3333333333333334814, 0.3333333333333333148, 0.3333333333333334259, 0.3333333333333333148, 0.3333333333333334814, 0.3333333333333334259, 0.3333333333333333703, 0.3333333333333334259, 0.3333333333333332593, 0.3333333333333333148, 0.3333333333333333703, 0.3333333333333333703, 0.3333333333333334259, 0.3333333333333333703, 0.3333333333333334259, 0.3333333333333333703, 0.3333333333333334259, 0.3333333333333333148, 0.3333333333333333703, 0.3333333333333334259, 0.3333333333333334259, 0.3333333333333333703, 0.3333333333333333703, 0.3333333333333333703, 0.3333333333333333148, 0.3333333333333333703, 0.3333333333333333148, 0.3333333333333334259, 0.3333333333333334259, 0.3333333333333333148, 0.3333333333333333703, 0.3333333333333334259, 0.3333333333333333703, 0.3333333333333333148, 0.3333333333333333703, 0.3333333333333333148, 0.3333333333333333703, 0.3333333333333334259, 0.3333333333333333148, 0.3333333333333334259, 0.3333333333333332593, 0.3333333333333334814, 0.3333333333333334814, 0.3333333333333333148, 0.3333333333333333703, 0.3333333333333334814, 0.3333333333333333148, 0.3333333333333333703, 0.3333333333333334814, 0.3333333333333333703, 0.3333333333333334259, 0.3333333333333334259, 0.3333333333333334814, 0.3333333333333333703, 0.3333333333333333703, 0.3333333333333333703, 0.3333333333333333148, 0.3333333333333333148, 0.3333333333333333703, 0.3333333333333333703, 0.3333333333333333703, 0.3333333333333334259, 0.3333333333333334259, 0.3333333333333333148, 0.3333333333333333148, 0.3333333333333334814, 0.3333333333333333148, 0.3333333333333333148, 0.3333333333333333703, 0.3333333333333333703, 0.3333333333333333703, 0.3333333333333333703),
 ( 0.3333333333333333703, 0.3333333333333333703, 0.3333333333333333703, 0.3333333333333333148, 0.3333333333333333703, 0.3333333333333333148, 0.3333333333333333703, 0.3333333333333334259, 0.3333333333333333703, 0.3333333333333333148, 0.3333333333333334259, 0.3333333333333332593, 0.3333333333333334259, 0.3333333333333333703, 0.3333333333333333703, 0.3333333333333332593, 0.3333333333333334259, 0.3333333333333333148, 0.3333333333333334259, 0.3333333333333333148, 0.3333333333333334259, 0.3333333333333334259, 0.3333333333333333148, 0.3333333333333333148, 0.3333333333333334814, 0.3333333333333332593, 0.3333333333333334259, 0.3333333333333334259, 0.3333333333333333703, 0.3333333333333333703, 0.3333333333333334814, 0.3333333333333332038, 0.3333333333333334814, 0.3333333333333333703, 0.3333333333333334259, 0.3333333333333333148, 0.3333333333333334259, 0.3333333333333334814, 0.3333333333333333703, 0.3333333333333332593, 0.3333333333333334259, 0.3333333333333333148, 0.3333333333333333148, 0.3333333333333333703, 0.3333333333333333703, 0.3333333333333334259, 0.3333333333333333148, 0.3333333333333335369, 0.3333333333333333148, 0.3333333333333334259, 0.3333333333333333703, 0.3333333333333332038, 0.3333333333333334259, 0.3333333333333334259, 0.3333333333333333148, 0.3333333333333334259, 0.3333333333333333703, 0.3333333333333333703, 0.3333333333333334259, 0.3333333333333334259, 0.3333333333333333703, 0.3333333333333334259, 0.3333333333333334259, 0.3333333333333333148, 0.3333333333333333703, 0.3333333333333333703, 0.3333333333333333148, 0.3333333333333334259, 0.3333333333333333148, 0.3333333333333334814, 0.3333333333333333703, 0.3333333333333334259, 0.3333333333333333148, 0.3333333333333333703, 0.3333333333333334259, 0.3333333333333333703, 0.3333333333333333703, 0.3333333333333333148, 0.3333333333333334259, 0.3333333333333333148, 0.3333333333333334259, 0.3333333333333333703, 0.3333333333333334259, 0.3333333333333334814, 0.3333333333333333148, 0.3333333333333334259, 0.3333333333333334259, 0.3333333333333333148, 0.3333333333333333703, 0.3333333333333333703, 0.3333333333333333148, 0.3333333333333334814, 0.3333333333333332593, 0.3333333333333334259, 0.3333333333333333703, 0.3333333333333333148, 0.3333333333333333703, 0.3333333333333333703, 0.3333333333333334259, 0.3333333333333333148, 0.3333333333333334259, 0.3333333333333333148, 0.3333333333333334814, 0.3333333333333333148, 0.3333333333333333148, 0.3333333333333334259, 0.3333333333333333148, 0.3333333333333333703, 0.3333333333333333703, 0.3333333333333334259, 0.3333333333333333703, 0.3333333333333334259, 0.3333333333333333703, 0.3333333333333332593, 0.3333333333333334259, 0.3333333333333333703, 0.3333333333333333148, 0.3333333333333334814, 0.3333333333333333148, 0.3333333333333334259, 0.3333333333333334259, 0.3333333333333333148, 0.3333333333333333703, 0.3333333333333334259, 0.3333333333333333703, 0.3333333333333333703, 0.3333333333333334259, 0.3333333333333333703, 0.3333333333333334259, 0.3333333333333333703, 0.3333333333333334259, 0.3333333333333333148, 0.3333333333333333703, 0.3333333333333333703, 0.3333333333333333703, 0.3333333333333333703, 0.3333333333333335369, 0.3333333333333332593, 0.3333333333333333703, 0.3333333333333333703, 0.3333333333333332593, 0.3333333333333333703, 0.3333333333333333703, 0.3333333333333334259, 0.3333333333333332593, 0.3333333333333333703, 0.3333333333333333703, 0.3333333333333333703, 0.3333333333333333703, 0.3333333333333333703, 0.3333333333333334259, 0.3333333333333333148, 0.3333333333333334259, 0.3333333333333333703, 0.3333333333333334814, 0.3333333333333332593, 0.3333333333333333703, 0.3333333333333334814, 0.3333333333333332038, 0.3333333333333334259, 0.3333333333333333148, 0.3333333333333333703, 0.3333333333333334814, 0.3333333333333332038, 0.3333333333333334259, 0.3333333333333333703, 0.3333333333333333703, 0.3333333333333333703, 0.3333333333333334259, 0.3333333333333333703, 0.3333333333333335369, 0.3333333333333333148, 0.3333333333333333148, 0.3333333333333334259, 0.3333333333333333148, 0.3333333333333333703, 0.3333333333333333703, 0.3333333333333334259, 0.3333333333333333148, 0.3333333333333334259, 0.3333333333333332593, 0.3333333333333334814, 0.3333333333333333703, 0.3333333333333333703, 0.3333333333333333703, 0.3333333333333333703, 0.3333333333333333703, 0.3333333333333334259, 0.3333333333333333703, 0.3333333333333334259, 0.3333333333333333148, 0.3333333333333335369, 0.3333333333333332038, 0.3333333333333335369, 0.3333333333333333148, 0.3333333333333334259, 0.3333333333333333703, 0.3333333333333333148, 0.3333333333333334259, 0.3333333333333333148, 0.3333333333333334259, 0.3333333333333332593, 0.3333333333333333148, 0.3333333333333334259, 0.3333333333333334814, 0.3333333333333333703, 0.3333333333333333703, 0.3333333333333334259, 0.3333333333333333148, 0.3333333333333333703, 0.3333333333333333148, 0.3333333333333334259, 0.3333333333333333148, 0.3333333333333333703, 0.3333333333333333703, 0.3333333333333334259, 0.3333333333333333148, 0.3333333333333334259, 0.3333333333333333703, 0.3333333333333333148, 0.3333333333333332593, 0.3333333333333334259, 0.3333333333333333148, 0.3333333333333334259, 0.3333333333333334259, 0.3333333333333334814, 0.3333333333333334259, 0.3333333333333333703, 0.3333333333333333703, 0.3333333333333333148, 0.3333333333333334259, 0.3333333333333333703, 0.3333333333333334259, 0.3333333333333333148, 0.3333333333333333703, 0.3333333333333333703, 0.3333333333333332593, 0.3333333333333334259, 0.3333333333333335369, 0.3333333333333333148, 0.3333333333333334814, 0.3333333333333333703, 0.3333333333333333148, 0.3333333333333334259, 0.3333333333333332593, 0.3333333333333334814, 0.3333333333333333148, 0.3333333333333333703, 0.3333333333333333148, 0.3333333333333334259, 0.3333333333333333148, 0.3333333333333334259, 0.3333333333333333148, 0.3333333333333333703, 0.3333333333333333703, 0.3333333333333333148, 0.3333333333333334259, 0.3333333333333333703, 0.3333333333333333703, 0.3333333333333335369, 0.3333333333333332038, 0.3333333333333334814, 0.3333333333333333148, 0.3333333333333334259, 0.3333333333333334259, 0.3333333333333333703, 0.3333333333333333148, 0.3333333333333334814, 0.3333333333333333703, 0.3333333333333333703, 0.3333333333333333703, 0.3333333333333333703, 0.3333333333333333703, 0.3333333333333334259, 0.3333333333333333703, 0.3333333333333334259, 0.3333333333333333148, 0.3333333333333333703, 0.3333333333333334259, 0.3333333333333334259, 0.3333333333333333703, 0.3333333333333333703, 0.3333333333333334259, 0.3333333333333333703, 0.3333333333333333148, 0.3333333333333333148, 0.3333333333333333703, 0.3333333333333333703, 0.3333333333333334259, 0.3333333333333334259, 0.3333333333333333703, 0.3333333333333333703, 0.3333333333333333703, 0.3333333333333333703, 0.3333333333333333703, 0.3333333333333333148, 0.3333333333333334259, 0.3333333333333334259, 0.3333333333333333703, 0.3333333333333335369, 0.3333333333333332038, 0.3333333333333334814, 0.3333333333333332593, 0.3333333333333333703, 0.3333333333333332593, 0.3333333333333334814, 0.3333333333333333148, 0.3333333333333333703, 0.3333333333333334259, 0.3333333333333334259, 0.3333333333333332593, 0.3333333333333334259, 0.3333333333333333148, 0.3333333333333333703, 0.3333333333333334259, 0.3333333333333334814, 0.3333333333333333148, 0.3333333333333334259, 0.3333333333333333148, 0.3333333333333334814, 0.3333333333333334259, 0.3333333333333333703, 0.3333333333333334259, 0.3333333333333332593, 0.3333333333333333148, 0.3333333333333333703, 0.3333333333333333703, 0.3333333333333334259, 0.3333333333333333703, 0.3333333333333334259, 0.3333333333333333703, 0.3333333333333334259, 0.3333333333333333148, 0.3333333333333333703, 0.3333333333333334259, 0.3333333333333334259, 0.3333333333333333703, 0.3333333333333333703, 0.3333333333333333703, 0.3333333333333333148, 0.3333333333333333703, 0.3333333333333333148, 0.3333333333333334259, 0.3333333333333334259, 0.3333333333333333148, 0.3333333333333333703, 0.3333333333333334259, 0.3333333333333333703, 0.3333333333333333148, 0.3333333333333333703, 0.3333333333333333148, 0.3333333333333333703, 0.3333333333333334259, 0.3333333333333333148, 0.3333333333333334259, 0.3333333333333332593, 0.3333333333333334814, 0.3333333333333334814, 0.3333333333333333148, 0.3333333333333333703, 0.3333333333333334814, 0.3333333333333333148, 0.3333333333333333703, 0.3333333333333334814, 0.3333333333333333703, 0.3333333333333334259, 0.3333333333333334259, 0.3333333333333334814, 0.3333333333333333703, 0.3333333333333333703, 0.3333333333333333703, 0.3333333333333333148, 0.3333333333333333148, 0.3333333333333333703, 0.3333333333333333703, 0.3333333333333333703, 0.3333333333333334259, 0.3333333333333334259, 0.3333333333333333148, 0.3333333333333333148, 0.3333333333333334814, 0.3333333333333333148, 0.3333333333333333148, 0.3333333333333333703, 0.3333333333333333703, 0.3333333333333333703, 0.3333333333333333703),
 ( 1.000000000000000000, 1.000000000000000000, 1.000000000000000000, 0.9999999999999997780, 1.000000000000000000, 1.000000000000000000, 1.000000000000000000, 1.000000000000000222, 1.000000000000000000, 1.000000000000000000, 1.000000000000000222, 0.9999999999999997780, 1.000000000000000222, 1.000000000000000222, 1.000000000000000000, 1.000000000000000000, 1.000000000000000000, 0.9999999999999997780, 1.000000000000000222, 0.9999999999999996669, 1.000000000000000222, 1.000000000000000000, 1.000000000000000000, 0.9999999999999996669, 1.000000000000000444, 0.9999999999999996669, 1.000000000000000444, 1.000000000000000000, 1.000000000000000000, 0.9999999999999997780, 1.000000000000000222, 0.9999999999999994449, 1.000000000000000444, 1.000000000000000000, 1.000000000000000000, 1.000000000000000000, 1.000000000000000000, 1.000000000000000444, 0.9999999999999997780, 1.000000000000000000, 1.000000000000000000, 1.000000000000000000, 1.000000000000000000, 1.000000000000000000, 1.000000000000000000, 0.9999999999999997780, 1.000000000000000000, 1.000000000000000444, 0.9999999999999997780, 1.000000000000000444, 0.9999999999999997780, 0.9999999999999997780, 1.000000000000000000, 1.000000000000000222, 1.000000000000000000, 1.000000000000000000, 1.000000000000000000, 1.000000000000000000, 0.9999999999999997780, 1.000000000000000444, 0.9999999999999997780, 1.000000000000000000, 1.000000000000000222, 0.9999999999999997780, 1.000000000000000000, 1.000000000000000222, 0.9999999999999997780, 1.000000000000000222, 1.000000000000000000, 1.000000000000000222, 1.000000000000000000, 1.000000000000000222, 0.9999999999999997780, 1.000000000000000000, 1.000000000000000222, 1.000000000000000000, 1.000000000000000222, 0.9999999999999997780, 1.000000000000000222, 0.9999999999999997780, 1.000000000000000222, 0.9999999999999997780, 1.000000000000000222, 1.000000000000000222, 0.9999999999999997780, 1.000000000000000222, 1.000000000000000222, 0.9999999999999997780, 1.000000000000000222, 1.000000000000000000, 1.000000000000000000, 1.000000000000000222, 0.9999999999999996669, 1.000000000000000444, 0.9999999999999997780, 0.9999999999999997780, 1.000000000000000000, 1.000000000000000000, 1.000000000000000000, 0.9999999999999996669, 1.000000000000000444, 1.000000000000000000, 1.000000000000000222, 1.000000000000000000, 0.9999999999999997780, 1.000000000000000222, 0.9999999999999997780, 1.000000000000000222, 1.000000000000000000, 1.000000000000000000, 1.000000000000000222, 1.000000000000000000, 1.000000000000000222, 0.9999999999999994449, 1.000000000000000444, 1.000000000000000000, 0.9999999999999996669, 1.000000000000000222, 0.9999999999999997780, 1.000000000000000222, 0.9999999999999997780, 1.000000000000000000, 1.000000000000000000, 1.000000000000000000, 1.000000000000000000, 1.000000000000000000, 1.000000000000000444, 1.000000000000000000, 1.000000000000000000, 1.000000000000000222, 1.000000000000000000, 1.000000000000000000, 0.9999999999999997780, 1.000000000000000000, 1.000000000000000222, 1.000000000000000000, 1.000000000000000222, 0.9999999999999997780, 1.000000000000000000, 0.9999999999999997780, 0.9999999999999997780, 1.000000000000000222, 0.9999999999999997780, 1.000000000000000444, 0.9999999999999997780, 1.000000000000000000, 1.000000000000000222, 1.000000000000000000, 1.000000000000000000, 0.9999999999999997780, 1.000000000000000222, 1.000000000000000000, 1.000000000000000000, 1.000000000000000000, 1.000000000000000222, 0.9999999999999996669, 1.000000000000000222, 1.000000000000000222, 0.9999999999999996669, 1.000000000000000444, 0.9999999999999996669, 1.000000000000000000, 1.000000000000000222, 0.9999999999999996669, 1.000000000000000222, 1.000000000000000000, 1.000000000000000222, 1.000000000000000000, 1.000000000000000222, 0.9999999999999997780, 1.000000000000000444, 0.9999999999999997780, 0.9999999999999997780, 1.000000000000000222, 0.9999999999999996669, 1.000000000000000222, 1.000000000000000000, 1.000000000000000000, 1.000000000000000000, 0.9999999999999997780, 1.000000000000000222, 1.000000000000000222, 0.9999999999999997780, 1.000000000000000222, 0.9999999999999997780, 1.000000000000000222, 1.000000000000000000, 1.000000000000000444, 1.000000000000000000, 1.000000000000000222, 0.9999999999999996669, 1.000000000000000444, 0.9999999999999993339, 1.000000000000000444, 0.9999999999999997780, 1.000000000000000444, 0.9999999999999997780, 1.000000000000000000, 1.000000000000000000, 0.9999999999999997780, 1.000000000000000222, 0.9999999999999997780, 0.9999999999999996669, 1.000000000000000444, 1.000000000000000222, 1.000000000000000000, 0.9999999999999997780, 1.000000000000000222, 0.9999999999999996669, 1.000000000000000222, 0.9999999999999997780, 1.000000000000000222, 1.000000000000000000, 1.000000000000000000, 1.000000000000000000, 1.000000000000000000, 0.9999999999999997780, 1.000000000000000000, 1.000000000000000000, 0.9999999999999997780, 1.000000000000000000, 1.000000000000000000, 1.000000000000000000, 1.000000000000000222, 1.000000000000000000, 1.000000000000000444, 1.000000000000000222, 1.000000000000000000, 1.000000000000000000, 0.9999999999999997780, 1.000000000000000222, 1.000000000000000000, 1.000000000000000000, 1.000000000000000000, 0.9999999999999997780, 1.000000000000000222, 0.9999999999999997780, 1.000000000000000222, 1.000000000000000444, 0.9999999999999997780, 1.000000000000000222, 1.000000000000000000, 1.000000000000000000, 1.000000000000000000, 0.9999999999999997780, 1.000000000000000444, 0.9999999999999997780, 1.000000000000000222, 0.9999999999999997780, 1.000000000000000222, 0.9999999999999994449, 1.000000000000000222, 1.000000000000000000, 1.000000000000000222, 1.000000000000000000, 0.9999999999999997780, 1.000000000000000222, 1.000000000000000000, 0.9999999999999997780, 1.000000000000000444, 0.9999999999999996669, 1.000000000000000222, 1.000000000000000000, 1.000000000000000000, 1.000000000000000222, 0.9999999999999997780, 0.9999999999999997780, 1.000000000000000444, 1.000000000000000222, 1.000000000000000000, 0.9999999999999997780, 0.9999999999999997780, 1.000000000000000222, 1.000000000000000000, 1.000000000000000222, 1.000000000000000000, 0.9999999999999997780, 1.000000000000000000, 1.000000000000000000, 1.000000000000000000, 1.000000000000000222, 0.9999999999999997780, 1.000000000000000222, 1.000000000000000000, 1.000000000000000000, 1.000000000000000000, 0.9999999999999997780, 1.000000000000000000, 1.000000000000000222, 1.000000000000000222, 0.9999999999999996669, 1.000000000000000444, 0.9999999999999996669, 1.000000000000000222, 1.000000000000000000, 1.000000000000000222, 0.9999999999999997780, 1.000000000000000444, 1.000000000000000000, 1.000000000000000444, 0.9999999999999994449, 1.000000000000000222, 0.9999999999999997780, 0.9999999999999997780, 1.000000000000000000, 1.000000000000000222, 1.000000000000000000, 1.000000000000000000, 1.000000000000000000, 1.000000000000000222, 0.9999999999999996669, 1.000000000000000222, 1.000000000000000000, 0.9999999999999996669, 1.000000000000000444, 1.000000000000000000, 1.000000000000000000, 1.000000000000000000, 0.9999999999999996669, 1.000000000000000222, 1.000000000000000000, 1.000000000000000000, 1.000000000000000222, 0.9999999999999997780, 0.9999999999999997780, 1.000000000000000000, 1.000000000000000000, 1.000000000000000222, 0.9999999999999997780, 1.000000000000000222, 1.000000000000000000, 1.000000000000000000, 0.9999999999999996669, 1.000000000000000222, 1.000000000000000000, 1.000000000000000222, 1.000000000000000000, 1.000000000000000000, 1.000000000000000000, 0.9999999999999997780, 1.000000000000000222, 0.9999999999999996669, 1.000000000000000444, 1.000000000000000000, 0.9999999999999997780, 1.000000000000000000, 1.000000000000000222, 1.000000000000000222, 0.9999999999999996669, 1.000000000000000000, 1.000000000000000000, 0.9999999999999997780, 1.000000000000000222, 1.000000000000000000, 1.000000000000000222, 0.9999999999999996669, 1.000000000000000444, 1.000000000000000000, 1.000000000000000000, 1.000000000000000000, 1.000000000000000222, 1.000000000000000000, 0.9999999999999997780, 1.000000000000000444, 1.000000000000000000, 1.000000000000000444, 0.9999999999999997780, 1.000000000000000444, 1.000000000000000000, 1.000000000000000222, 1.000000000000000222, 1.000000000000000000, 0.9999999999999996669, 1.000000000000000000, 1.000000000000000000, 1.000000000000000000, 1.000000000000000000, 1.000000000000000222, 0.9999999999999996669, 1.000000000000000000, 1.000000000000000222, 0.9999999999999997780, 0.9999999999999997780, 1.000000000000000000, 1.000000000000000000, 1.000000000000000000, 1.000000000000000000),
 ( 0.3333333333333333703, 0.3333333333333333703, 0.3333333333333333703, 0.3333333333333333148, 0.3333333333333333703, 0.3333333333333333148, 0.3333333333333333703, 0.3333333333333334259, 0.3333333333333333703, 0.3333333333333333148, 0.3333333333333334259, 0.3333333333333332593, 0.3333333333333334259, 0.3333333333333333703, 0.3333333333333333703, 0.3333333333333332593, 0.3333333333333334259, 0.3333333333333333148, 0.3333333333333334259, 0.3333333333333333148, 0.3333333333333334259, 0.3333333333333334259, 0.3333333333333333148, 0.3333333333333333148, 0.3333333333333334814, 0.3333333333333332593, 0.3333333333333334259, 0.3333333333333334259, 0.3333333333333333703, 0.3333333333333333703, 0.3333333333333334814, 0.3333333333333332038, 0.3333333333333334814, 0.3333333333333333703, 0.3333333333333334259, 0.3333333333333333148, 0.3333333333333334259, 0.3333333333333334814, 0.3333333333333333703, 0.3333333333333332593, 0.3333333333333334259, 0.3333333333333333148, 0.3333333333333333148, 0.3333333333333333703, 0.3333333333333333703, 0.3333333333333334259, 0.3333333333333333148, 0.3333333333333335369, 0.3333333333333333148, 0.3333333333333334259, 0.3333333333333333703, 0.3333333333333332038, 0.3333333333333334259, 0.3333333333333334259, 0.3333333333333333148, 0.3333333333333334259, 0.3333333333333333703, 0.3333333333333333703, 0.3333333333333334259, 0.3333333333333334259, 0.3333333333333333703, 0.3333333333333334259, 0.3333333333333334259, 0.3333333333333333148, 0.3333333333333333703, 0.3333333333333333703, 0.3333333333333333148, 0.3333333333333334259, 0.3333333333333333148, 0.3333333333333334814, 0.3333333333333333703, 0.3333333333333334259, 0.3333333333333333148, 0.3333333333333333703, 0.3333333333333334259, 0.3333333333333333703, 0.3333333333333333703, 0.3333333333333333148, 0.3333333333333334259, 0.3333333333333333148, 0.3333333333333334259, 0.3333333333333333703, 0.3333333333333334259, 0.3333333333333334814, 0.3333333333333333148, 0.3333333333333334259, 0.3333333333333334259, 0.3333333333333333148, 0.3333333333333333703, 0.3333333333333333703, 0.3333333333333333148, 0.3333333333333334814, 0.3333333333333332593, 0.3333333333333334259, 0.3333333333333333703, 0.3333333333333333148, 0.3333333333333333703, 0.3333333333333333703, 0.3333333333333334259, 0.3333333333333333148, 0.3333333333333334259, 0.3333333333333333148, 0.3333333333333334814, 0.3333333333333333148, 0.3333333333333333148, 0.3333333333333334259, 0.3333333333333333148, 0.3333333333333333703, 0.3333333333333333703, 0.3333333333333334259, 0.3333333333333333703, 0.3333333333333334259, 0.3333333333333333703, 0.3333333333333332593, 0.3333333333333334259, 0.3333333333333333703, 0.3333333333333333148, 0.3333333333333334814, 0.3333333333333333148, 0.3333333333333334259, 0.3333333333333334259, 0.3333333333333333148, 0.3333333333333333703, 0.3333333333333334259, 0.3333333333333333703, 0.3333333333333333703, 0.3333333333333334259, 0.3333333333333333703, 0.3333333333333334259, 0.3333333333333333703, 0.3333333333333334259, 0.3333333333333333148, 0.3333333333333333703, 0.3333333333333333703, 0.3333333333333333703, 0.3333333333333333703, 0.3333333333333335369, 0.3333333333333332593, 0.3333333333333333703, 0.3333333333333333703, 0.3333333333333332593, 0.3333333333333333703, 0.3333333333333333703, 0.3333333333333334259, 0.3333333333333332593, 0.3333333333333333703, 0.3333333333333333703, 0.3333333333333333703, 0.3333333333333333703, 0.3333333333333333703, 0.3333333333333334259, 0.3333333333333333148, 0.3333333333333334259, 0.3333333333333333703, 0.3333333333333334814, 0.3333333333333332593, 0.3333333333333333703, 0.3333333333333334814, 0.3333333333333332038, 0.3333333333333334259, 0.3333333333333333148, 0.3333333333333333703, 0.3333333333333334814, 0.3333333333333332038, 0.3333333333333334259, 0.3333333333333333703, 0.3333333333333333703, 0.3333333333333333703, 0.3333333333333334259, 0.3333333333333333703, 0.3333333333333335369, 0.3333333333333333148, 0.3333333333333333148, 0.3333333333333334259, 0.3333333333333333148, 0.3333333333333333703, 0.3333333333333333703, 0.3333333333333334259, 0.3333333333333333148, 0.3333333333333334259, 0.3333333333333332593, 0.3333333333333334814, 0.3333333333333333703, 0.3333333333333333703, 0.3333333333333333703, 0.3333333333333333703, 0.3333333333333333703, 0.3333333333333334259, 0.3333333333333333703, 0.3333333333333334259, 0.3333333333333333148, 0.3333333333333335369, 0.3333333333333332038, 0.3333333333333335369, 0.3333333333333333148, 0.3333333333333334259, 0.3333333333333333703, 0.3333333333333333148, 0.3333333333333334259, 0.3333333333333333148, 0.3333333333333334259, 0.3333333333333332593, 0.3333333333333333148, 0.3333333333333334259, 0.3333333333333334814, 0.3333333333333333703, 0.3333333333333333703, 0.3333333333333334259, 0.3333333333333333148, 0.3333333333333333703, 0.3333333333333333148, 0.3333333333333334259, 0.3333333333333333148, 0.3333333333333333703, 0.3333333333333333703, 0.3333333333333334259, 0.3333333333333333148, 0.3333333333333334259, 0.3333333333333333703, 0.3333333333333333148, 0.3333333333333332593, 0.3333333333333334259, 0.3333333333333333148, 0.3333333333333334259, 0.3333333333333334259, 0.3333333333333334814, 0.3333333333333334259, 0.3333333333333333703, 0.3333333333333333703, 0.3333333333333333148, 0.3333333333333334259, 0.3333333333333333703, 0.3333333333333334259, 0.3333333333333333148, 0.3333333333333333703, 0.3333333333333333703, 0.3333333333333332593, 0.3333333333333334259, 0.3333333333333335369, 0.3333333333333333148, 0.3333333333333334814, 0.3333333333333333703, 0.3333333333333333148, 0.3333333333333334259, 0.3333333333333332593, 0.3333333333333334814, 0.3333333333333333148, 0.3333333333333333703, 0.3333333333333333148, 0.3333333333333334259, 0.3333333333333333148, 0.3333333333333334259, 0.3333333333333333148, 0.3333333333333333703, 0.3333333333333333703, 0.3333333333333333148, 0.3333333333333334259, 0.3333333333333333703, 0.3333333333333333703, 0.3333333333333335369, 0.3333333333333332038, 0.3333333333333334814, 0.3333333333333333148, 0.3333333333333334259, 0.3333333333333334259, 0.3333333333333333703, 0.3333333333333333148, 0.3333333333333334814, 0.3333333333333333703, 0.3333333333333333703, 0.3333333333333333703, 0.3333333333333333703, 0.3333333333333333703, 0.3333333333333334259, 0.3333333333333333703, 0.3333333333333334259, 0.3333333333333333148, 0.3333333333333333703, 0.3333333333333334259, 0.3333333333333334259, 0.3333333333333333703, 0.3333333333333333703, 0.3333333333333334259, 0.3333333333333333703, 0.3333333333333333148, 0.3333333333333333148, 0.3333333333333333703, 0.3333333333333333703, 0.3333333333333334259, 0.3333333333333334259, 0.3333333333333333703, 0.3333333333333333703, 0.3333333333333333703, 0.3333333333333333703, 0.3333333333333333703, 0.3333333333333333148, 0.3333333333333334259, 0.3333333333333334259, 0.3333333333333333703, 0.3333333333333335369, 0.3333333333333332038, 0.3333333333333334814, 0.3333333333333332593, 0.3333333333333333703, 0.3333333333333332593, 0.3333333333333334814, 0.3333333333333333148, 0.3333333333333333703, 0.3333333333333334259, 0.3333333333333334259, 0.3333333333333332593, 0.3333333333333334259, 0.3333333333333333148, 0.3333333333333333703, 0.3333333333333334259, 0.3333333333333334814, 0.3333333333333333148, 0.3333333333333334259, 0.3333333333333333148, 0.3333333333333334814, 0.3333333333333334259, 0.3333333333333333703, 0.3333333333333334259, 0.3333333333333332593, 0.3333333333333333148, 0.3333333333333333703, 0.3333333333333333703, 0.3333333333333334259, 0.3333333333333333703, 0.3333333333333334259, 0.3333333333333333703, 0.3333333333333334259, 0.3333333333333333148, 0.3333333333333333703, 0.3333333333333334259, 0.3333333333333334259, 0.3333333333333333703, 0.3333333333333333703, 0.3333333333333333703, 0.3333333333333333148, 0.3333333333333333703, 0.3333333333333333148, 0.3333333333333334259, 0.3333333333333334259, 0.3333333333333333148, 0.3333333333333333703, 0.3333333333333334259, 0.3333333333333333703, 0.3333333333333333148, 0.3333333333333333703, 0.3333333333333333148, 0.3333333333333333703, 0.3333333333333334259, 0.3333333333333333148, 0.3333333333333334259, 0.3333333333333332593, 0.3333333333333334814, 0.3333333333333334814, 0.3333333333333333148, 0.3333333333333333703, 0.3333333333333334814, 0.3333333333333333148, 0.3333333333333333703, 0.3333333333333334814, 0.3333333333333333703, 0.3333333333333334259, 0.3333333333333334259, 0.3333333333333334814, 0.3333333333333333703, 0.3333333333333333703, 0.3333333333333333703, 0.3333333333333333148, 0.3333333333333333148, 0.3333333333333333703, 0.3333333333333333703, 0.3333333333333333703, 0.3333333333333334259, 0.3333333333333334259, 0.3333333333333333148, 0.3333333333333333148, 0.3333333333333334814, 0.3333333333333333148, 0.3333333333333333148, 0.3333333333333333703, 0.3333333333333333703, 0.3333333333333333703, 0.3333333333333333703),
 ( 0.3333333333333333703, 0.3333333333333333703, 0.3333333333333333703, 0.3333333333333333148, 0.3333333333333333703, 0.3333333333333333148, 0.3333333333333333703, 0.3333333333333334259, 0.3333333333333333703, 0.3333333333333333148, 0.3333333333333334259, 0.3333333333333332593, 0.3333333333333334259, 0.3333333333333333703, 0.3333333333333333703, 0.3333333333333332593, 0.3333333333333334259, 0.3333333333333333148, 0.3333333333333334259, 0.3333333333333333148, 0.3333333333333334259, 0.3333333333333334259, 0.3333333333333333148, 0.3333333333333333148, 0.3333333333333334814, 0.3333333333333332593, 0.3333333333333334259, 0.3333333333333334259, 0.3333333333333333703, 0.3333333333333333703, 0.3333333333333334814, 0.3333333333333332038, 0.3333333333333334814, 0.3333333333333333703, 0.3333333333333334259, 0.3333333333333333148, 0.3333333333333334259, 0.3333333333333334814, 0.3333333333333333703, 0.3333333333333332593, 0.3333333333333334259, 0.3333333333333333148, 0.3333333333333333148, 0.3333333333333333703, 0.3333333333333333703, 0.3333333333333334259, 0.3333333333333333148, 0.3333333333333335369, 0.3333333333333333148, 0.3333333333333334259, 0.3333333333333333703, 0.3333333333333332038, 0.3333333333333334259, 0.3333333333333334259, 0.3333333333333333148, 0.3333333333333334259, 0.3333333333333333703, 0.3333333333333333703, 0.3333333333333334259, 0.3333333333333334259, 0.3333333333333333703, 0.3333333333333334259, 0.3333333333333334259, 0.3333333333333333148, 0.3333333333333333703, 0.3333333333333333703, 0.3333333333333333148, 0.3333333333333334259, 0.3333333333333333148, 0.3333333333333334814, 0.3333333333333333703, 0.3333333333333334259, 0.3333333333333333148, 0.3333333333333333703, 0.3333333333333334259, 0.3333333333333333703, 0.3333333333333333703, 0.3333333333333333148, 0.3333333333333334259, 0.3333333333333333148, 0.3333333333333334259, 0.3333333333333333703, 0.3333333333333334259, 0.3333333333333334814, 0.3333333333333333148, 0.3333333333333334259, 0.3333333333333334259, 0.3333333333333333148, 0.3333333333333333703, 0.3333333333333333703, 0.3333333333333333148, 0.3333333333333334814, 0.3333333333333332593, 0.3333333333333334259, 0.3333333333333333703, 0.3333333333333333148, 0.3333333333333333703, 0.3333333333333333703, 0.3333333333333334259, 0.3333333333333333148, 0.3333333333333334259, 0.3333333333333333148, 0.3333333333333334814, 0.3333333333333333148, 0.3333333333333333148, 0.3333333333333334259, 0.3333333333333333148, 0.3333333333333333703, 0.3333333333333333703, 0.3333333333333334259, 0.3333333333333333703, 0.3333333333333334259, 0.3333333333333333703, 0.3333333333333332593, 0.3333333333333334259, 0.3333333333333333703, 0.3333333333333333148, 0.3333333333333334814, 0.3333333333333333148, 0.3333333333333334259, 0.3333333333333334259, 0.3333333333333333148, 0.3333333333333333703, 0.3333333333333334259, 0.3333333333333333703, 0.3333333333333333703, 0.3333333333333334259, 0.3333333333333333703, 0.3333333333333334259, 0.3333333333333333703, 0.3333333333333334259, 0.3333333333333333148, 0.3333333333333333703, 0.3333333333333333703, 0.3333333333333333703, 0.3333333333333333703, 0.3333333333333335369, 0.3333333333333332593, 0.3333333333333333703, 0.3333333333333333703, 0.3333333333333332593, 0.3333333333333333703, 0.3333333333333333703, 0.3333333333333334259, 0.3333333333333332593, 0.3333333333333333703, 0.3333333333333333703, 0.3333333333333333703, 0.3333333333333333703, 0.3333333333333333703, 0.3333333333333334259, 0.3333333333333333148, 0.3333333333333334259, 0.3333333333333333703, 0.3333333333333334814, 0.3333333333333332593, 0.3333333333333333703, 0.3333333333333334814, 0.3333333333333332038, 0.3333333333333334259, 0.3333333333333333148, 0.3333333333333333703, 0.3333333333333334814, 0.3333333333333332038, 0.3333333333333334259, 0.3333333333333333703, 0.3333333333333333703, 0.3333333333333333703, 0.3333333333333334259, 0.3333333333333333703, 0.3333333333333335369, 0.3333333333333333148, 0.3333333333333333148, 0.3333333333333334259, 0.3333333333333333148, 0.3333333333333333703, 0.3333333333333333703, 0.3333333333333334259, 0.3333333333333333148, 0.3333333333333334259, 0.3333333333333332593, 0.3333333333333334814, 0.3333333333333333703, 0.3333333333333333703, 0.3333333333333333703, 0.3333333333333333703, 0.3333333333333333703, 0.3333333333333334259, 0.3333333333333333703, 0.3333333333333334259, 0.3333333333333333148, 0.3333333333333335369, 0.3333333333333332038, 0.3333333333333335369, 0.3333333333333333148, 0.3333333333333334259, 0.3333333333333333703, 0.3333333333333333148, 0.3333333333333334259, 0.3333333333333333148, 0.3333333333333334259, 0.3333333333333332593, 0.3333333333333333148, 0.3333333333333334259, 0.3333333333333334814, 0.3333333333333333703, 0.3333333333333333703, 0.3333333333333334259, 0.3333333333333333148, 0.3333333333333333703, 0.3333333333333333148, 0.3333333333333334259, 0.3333333333333333148, 0.3333333333333333703, 0.3333333333333333703, 0.3333333333333334259, 0.3333333333333333148, 0.3333333333333334259, 0.3333333333333333703, 0.3333333333333333148, 0.3333333333333332593, 0.3333333333333334259, 0.3333333333333333148, 0.3333333333333334259, 0.3333333333333334259, 0.3333333333333334814, 0.3333333333333334259, 0.3333333333333333703, 0.3333333333333333703, 0.3333333333333333148, 0.3333333333333334259, 0.3333333333333333703, 0.3333333333333334259, 0.3333333333333333148, 0.3333333333333333703, 0.3333333333333333703, 0.3333333333333332593, 0.3333333333333334259, 0.3333333333333335369, 0.3333333333333333148, 0.3333333333333334814, 0.3333333333333333703, 0.3333333333333333148, 0.3333333333333334259, 0.3333333333333332593, 0.3333333333333334814, 0.3333333333333333148, 0.3333333333333333703, 0.3333333333333333148, 0.3333333333333334259, 0.3333333333333333148, 0.3333333333333334259, 0.3333333333333333148, 0.3333333333333333703, 0.3333333333333333703, 0.3333333333333333148, 0.3333333333333334259, 0.3333333333333333703, 0.3333333333333333703, 0.3333333333333335369, 0.3333333333333332038, 0.3333333333333334814, 0.3333333333333333148, 0.3333333333333334259, 0.3333333333333334259, 0.3333333333333333703, 0.3333333333333333148, 0.3333333333333334814, 0.3333333333333333703, 0.3333333333333333703, 0.3333333333333333703, 0.3333333333333333703, 0.3333333333333333703, 0.3333333333333334259, 0.3333333333333333703, 0.3333333333333334259, 0.3333333333333333148, 0.3333333333333333703, 0.3333333333333334259, 0.3333333333333334259, 0.3333333333333333703, 0.3333333333333333703, 0.3333333333333334259, 0.3333333333333333703, 0.3333333333333333148, 0.3333333333333333148, 0.3333333333333333703, 0.3333333333333333703, 0.3333333333333334259, 0.3333333333333334259, 0.3333333333333333703, 0.3333333333333333703, 0.3333333333333333703, 0.3333333333333333703, 0.3333333333333333703, 0.3333333333333333148, 0.3333333333333334259, 0.3333333333333334259, 0.3333333333333333703, 0.3333333333333335369, 0.3333333333333332038, 0.3333333333333334814, 0.3333333333333332593, 0.3333333333333333703, 0.3333333333333332593, 0.3333333333333334814, 0.3333333333333333148, 0.3333333333333333703, 0.3333333333333334259, 0.3333333333333334259, 0.3333333333333332593, 0.3333333333333334259, 0.3333333333333333148, 0.3333333333333333703, 0.3333333333333334259, 0.3333333333333334814, 0.3333333333333333148, 0.3333333333333334259, 0.3333333333333333148, 0.3333333333333334814, 0.3333333333333334259, 0.3333333333333333703, 0.3333333333333334259, 0.3333333333333332593, 0.3333333333333333148, 0.3333333333333333703, 0.3333333333333333703, 0.3333333333333334259, 0.3333333333333333703, 0.3333333333333334259, 0.3333333333333333703, 0.3333333333333334259, 0.3333333333333333148, 0.3333333333333333703, 0.3333333333333334259, 0.3333333333333334259, 0.3333333333333333703, 0.3333333333333333703, 0.3333333333333333703, 0.3333333333333333148, 0.3333333333333333703, 0.3333333333333333148, 0.3333333333333334259, 0.3333333333333334259, 0.3333333333333333148, 0.3333333333333333703, 0.3333333333333334259, 0.3333333333333333703, 0.3333333333333333148, 0.3333333333333333703, 0.3333333333333333148, 0.3333333333333333703, 0.3333333333333334259, 0.3333333333333333148, 0.3333333333333334259, 0.3333333333333332593, 0.3333333333333334814, 0.3333333333333334814, 0.3333333333333333148, 0.3333333333333333703, 0.3333333333333334814, 0.3333333333333333148, 0.3333333333333333703, 0.3333333333333334814, 0.3333333333333333703, 0.3333333333333334259, 0.3333333333333334259, 0.3333333333333334814, 0.3333333333333333703, 0.3333333333333333703, 0.3333333333333333703, 0.3333333333333333148, 0.3333333333333333148, 0.3333333333333333703, 0.3333333333333333703, 0.3333333333333333703, 0.3333333333333334259, 0.3333333333333334259, 0.3333333333333333148, 0.3333333333333333148, 0.3333333333333334814, 0.3333333333333333148, 0.3333333333333333148, 0.3333333333333333703, 0.3333333333333333703, 0.3333333333333333703, 0.3333333333333333703),
 ( 1.000000000000000000, 1.000000000000000000, 1.000000000000000000, 0.9999999999999997780, 1.000000000000000000, 1.000000000000000000, 1.000000000000000000, 1.000000000000000222, 1.000000000000000000, 1.000000000000000000, 1.000000000000000222, 0.9999999999999997780, 1.000000000000000222, 1.000000000000000222, 1.000000000000000000, 1.000000000000000000, 1.000000000000000000, 0.9999999999999997780, 1.000000000000000222, 0.9999999999999996669, 1.000000000000000222, 1.000000000000000000, 1.000000000000000000, 0.9999999999999996669, 1.000000000000000444, 0.9999999999999996669, 1.000000000000000444, 1.000000000000000000, 1.000000000000000000, 0.9999999999999997780, 1.000000000000000222, 0.9999999999999994449, 1.000000000000000444, 1.000000000000000000, 1.000000000000000000, 1.000000000000000000, 1.000000000000000000, 1.000000000000000444, 0.9999999999999997780, 1.000000000000000000, 1.000000000000000000, 1.000000000000000000, 1.000000000000000000, 1.000000000000000000, 1.000000000000000000, 0.9999999999999997780, 1.000000000000000000, 1.000000000000000444, 0.9999999999999997780, 1.000000000000000444, 0.9999999999999997780, 0.9999999999999997780, 1.000000000000000000, 1.000000000000000222, 1.000000000000000000, 1.000000000000000000, 1.000000000000000000, 1.000000000000000000, 0.9999999999999997780, 1.000000000000000444, 0.9999999999999997780, 1.000000000000000000, 1.000000000000000222, 0.9999999999999997780, 1.000000000000000000, 1.000000000000000222, 0.9999999999999997780, 1.000000000000000222, 1.000000000000000000, 1.000000000000000222, 1.000000000000000000, 1.000000000000000222, 0.9999999999999997780, 1.000000000000000000, 1.000000000000000222, 1.000000000000000000, 1.000000000000000222, 0.9999999999999997780, 1.000000000000000222, 0.9999999999999997780, 1.000000000000000222, 0.9999999999999997780, 1.000000000000000222, 1.000000000000000222, 0.9999999999999997780, 1.000000000000000222, 1.000000000000000222, 0.9999999999999997780, 1.000000000000000222, 1.000000000000000000, 1.000000000000000000, 1.000000000000000222, 0.9999999999999996669, 1.000000000000000444, 0.9999999999999997780, 0.9999999999999997780, 1.000000000000000000, 1.000000000000000000, 1.000000000000000000, 0.9999999999999996669, 1.000000000000000444, 1.000000000000000000, 1.000000000000000222, 1.000000000000000000, 0.9999999999999997780, 1.000000000000000222, 0.9999999999999997780, 1.000000000000000222, 1.000000000000000000, 1.000000000000000000, 1.000000000000000222, 1.000000000000000000, 1.000000000000000222, 0.9999999999999994449, 1.000000000000000444, 1.000000000000000000, 0.9999999999999996669, 1.000000000000000222, 0.9999999999999997780, 1.000000000000000222, 0.9999999999999997780, 1.000000000000000000, 1.000000000000000000, 1.000000000000000000, 1.000000000000000000, 1.000000000000000000, 1.000000000000000444, 1.000000000000000000, 1.000000000000000000, 1.000000000000000222, 1.000000000000000000, 1.000000000000000000, 0.9999999999999997780, 1.000000000000000000, 1.000000000000000222, 1.000000000000000000, 1.000000000000000222, 0.9999999999999997780, 1.000000000000000000, 0.9999999999999997780, 0.9999999999999997780, 1.000000000000000222, 0.9999999999999997780, 1.000000000000000444, 0.9999999999999997780, 1.000000000000000000, 1.000000000000000222, 1.000000000000000000, 1.000000000000000000, 0.9999999999999997780, 1.000000000000000222, 1.000000000000000000, 1.000000000000000000, 1.000000000000000000, 1.000000000000000222, 0.9999999999999996669, 1.000000000000000222, 1.000000000000000222, 0.9999999999999996669, 1.000000000000000444, 0.9999999999999996669, 1.000000000000000000, 1.000000000000000222, 0.9999999999999996669, 1.000000000000000222, 1.000000000000000000, 1.000000000000000222, 1.000000000000000000, 1.000000000000000222, 0.9999999999999997780, 1.000000000000000444, 0.9999999999999997780, 0.9999999999999997780, 1.000000000000000222, 0.9999999999999996669, 1.000000000000000222, 1.000000000000000000, 1.000000000000000000, 1.000000000000000000, 0.9999999999999997780, 1.000000000000000222, 1.000000000000000222, 0.9999999999999997780, 1.000000000000000222, 0.9999999999999997780, 1.000000000000000222, 1.000000000000000000, 1.000000000000000444, 1.000000000000000000, 1.000000000000000222, 0.9999999999999996669, 1.000000000000000444, 0.9999999999999993339, 1.000000000000000444, 0.9999999999999997780, 1.000000000000000444, 0.9999999999999997780, 1.000000000000000000, 1.000000000000000000, 0.9999999999999997780, 1.000000000000000222, 0.9999999999999997780, 0.9999999999999996669, 1.000000000000000444, 1.000000000000000222, 1.000000000000000000, 0.9999999999999997780, 1.000000000000000222, 0.9999999999999996669, 1.000000000000000222, 0.9999999999999997780, 1.000000000000000222, 1.000000000000000000, 1.000000000000000000, 1.000000000000000000, 1.000000000000000000, 0.9999999999999997780, 1.000000000000000000, 1.000000000000000000, 0.9999999999999997780, 1.000000000000000000, 1.000000000000000000, 1.000000000000000000, 1.000000000000000222, 1.000000000000000000, 1.000000000000000444, 1.000000000000000222, 1.000000000000000000, 1.000000000000000000, 0.9999999999999997780, 1.000000000000000222, 1.000000000000000000, 1.000000000000000000, 1.000000000000000000, 0.9999999999999997780, 1.000000000000000222, 0.9999999999999997780, 1.000000000000000222, 1.000000000000000444, 0.9999999999999997780, 1.000000000000000222, 1.000000000000000000, 1.000000000000000000, 1.000000000000000000, 0.9999999999999997780, 1.000000000000000444, 0.9999999999999997780, 1.000000000000000222, 0.9999999999999997780, 1.000000000000000222, 0.9999999999999994449, 1.000000000000000222, 1.000000000000000000, 1.000000000000000222, 1.000000000000000000, 0.9999999999999997780, 1.000000000000000222, 1.000000000000000000, 0.9999999999999997780, 1.000000000000000444, 0.9999999999999996669, 1.000000000000000222, 1.000000000000000000, 1.000000000000000000, 1.000000000000000222, 0.9999999999999997780, 0.9999999999999997780, 1.000000000000000444, 1.000000000000000222, 1.000000000000000000, 0.9999999999999997780, 0.9999999999999997780, 1.000000000000000222, 1.000000000000000000, 1.000000000000000222, 1.000000000000000000, 0.9999999999999997780, 1.000000000000000000, 1.000000000000000000, 1.000000000000000000, 1.000000000000000222, 0.9999999999999997780, 1.000000000000000222, 1.000000000000000000, 1.000000000000000000, 1.000000000000000000, 0.9999999999999997780, 1.000000000000000000, 1.000000000000000222, 1.000000000000000222, 0.9999999999999996669, 1.000000000000000444, 0.9999999999999996669, 1.000000000000000222, 1.000000000000000000, 1.000000000000000222, 0.9999999999999997780, 1.000000000000000444, 1.000000000000000000, 1.000000000000000444, 0.9999999999999994449, 1.000000000000000222, 0.9999999999999997780, 0.9999999999999997780, 1.000000000000000000, 1.000000000000000222, 1.000000000000000000, 1.000000000000000000, 1.000000000000000000, 1.000000000000000222, 0.9999999999999996669, 1.000000000000000222, 1.000000000000000000, 0.9999999999999996669, 1.000000000000000444, 1.000000000000000000, 1.000000000000000000, 1.000000000000000000, 0.9999999999999996669, 1.000000000000000222, 1.000000000000000000, 1.000000000000000000, 1.000000000000000222, 0.9999999999999997780, 0.9999999999999997780, 1.000000000000000000, 1.000000000000000000, 1.000000000000000222, 0.9999999999999997780, 1.000000000000000222, 1.000000000000000000, 1.000000000000000000, 0.9999999999999996669, 1.000000000000000222, 1.000000000000000000, 1.000000000000000222, 1.000000000000000000, 1.000000000000000000, 1.000000000000000000, 0.9999999999999997780, 1.000000000000000222, 0.9999999999999996669, 1.000000000000000444, 1.000000000000000000, 0.9999999999999997780, 1.000000000000000000, 1.000000000000000222, 1.000000000000000222, 0.9999999999999996669, 1.000000000000000000, 1.000000000000000000, 0.9999999999999997780, 1.000000000000000222, 1.000000000000000000, 1.000000000000000222, 0.9999999999999996669, 1.000000000000000444, 1.000000000000000000, 1.000000000000000000, 1.000000000000000000, 1.000000000000000222, 1.000000000000000000, 0.9999999999999997780, 1.000000000000000444, 1.000000000000000000, 1.000000000000000444, 0.9999999999999997780, 1.000000000000000444, 1.000000000000000000, 1.000000000000000222, 1.000000000000000222, 1.000000000000000000, 0.9999999999999996669, 1.000000000000000000, 1.000000000000000000, 1.000000000000000000, 1.000000000000000000, 1.000000000000000222, 0.9999999999999996669, 1.000000000000000000, 1.000000000000000222, 0.9999999999999997780, 0.9999999999999997780, 1.000000000000000000, 1.000000000000000000, 1.000000000000000000, 1.000000000000000000) ) ) 
 REPRESENTATION_ITEM ( '' )  SURFACE ( )  );
#144368 = CARTESIAN_POINT ( 'NONE',  ( 0.6823417656249899377, 5.738541667008087543, -1.181850606188754593 ) ) ;
#144369 = CARTESIAN_POINT ( 'NONE',  ( 6.580818069394648973, -6.606405293530493772, 7.011678565220734960 ) ) ;
#144370 = CARTESIAN_POINT ( 'NONE',  ( 2.860407222358963608, 5.320596945185329218, 1.082531754730548412 ) ) ;
#144371 = CARTESIAN_POINT ( 'NONE',  ( 1.639757756142570244, 2.007014814066264474, -0.8283606533975582664 ) ) ;
#144372 = CARTESIAN_POINT ( 'NONE',  ( -11.41381675112453564, 19.00000000000000000, 3.704697986577180746 ) ) ;
#144373 = EDGE_CURVE ( 'NONE', #41882, #47264, #170889, .T. ) ;
#144374 = CARTESIAN_POINT ( 'NONE',  ( 11.43190902327453529, 11.15522128257866363, -3.649704988378122739 ) ) ;
#144375 = CARTESIAN_POINT ( 'NONE',  ( -2.299988384273672803, 2.756689234775647979, -2.499999999999998668 ) ) ;
#144376 = CARTESIAN_POINT ( 'NONE',  ( 2.758895227446885645, -1.625506345271657604, -0.9254698705311247275 ) ) ;
#144377 = CARTESIAN_POINT ( 'NONE',  ( 0.2982115315293157320, -2.060280707965747027, -0.05303618902755858483 ) ) ;
#144379 = CARTESIAN_POINT ( 'NONE',  ( 6.827182134110246103, 3.705739211453745074, 2.325493694733235195 ) ) ;
#144378 = CARTESIAN_POINT ( 'NONE',  ( -0.02224634325196597762, 7.629137130509080045, -2.889100442546748582 ) ) ;
#144380 = CARTESIAN_POINT ( 'NONE',  ( 0.6823417656249882723, -0.07395833299191079124, -1.181850606188749264 ) ) ;
#144381 = CARTESIAN_POINT ( 'NONE',  ( 2.086439996564274146, -1.175226666667992914, 1.508458442701497315 ) ) ;
#144382 = CARTESIAN_POINT ( 'NONE',  ( 4.627684317651063139, -1.090007866362858291, -1.394274008033623113 ) ) ;
#144383 = CARTESIAN_POINT ( 'NONE',  ( 1.980978873585538480, -1.748965405663160944, -0.7736543689686598002 ) ) ;
#144384 = CARTESIAN_POINT ( 'NONE',  ( -6.091691091241777656, 6.001394449403842479, 0.7998128361456341429 ) ) ;
#144386 = CARTESIAN_POINT ( 'NONE',  ( 5.360912872498101223, -0.05169663686300975808, -1.915091480415902048 ) ) ;
#144385 = DIRECTION ( 'NONE',  ( -3.491481338843133355E-15, 0.000000000000000000, -1.000000000000000000 ) ) ;
#144387 = CARTESIAN_POINT ( 'NONE',  ( -0.7500000000000215383, 0.4416666666666874130, 1.299038105676659116 ) ) ;
#144388 = CARTESIAN_POINT ( 'NONE',  ( 6.566861343609567747, 1.460344857008318398, -1.321773145083295464 ) ) ;
#144389 = CARTESIAN_POINT ( 'NONE',  ( -1.001543065824772872E-14, 5.712500000000021672, 1.732050807568877637 ) ) ;
#144390 = FACE_OUTER_BOUND ( 'NONE', #41397, .T. ) ;
#144391 = CARTESIAN_POINT ( 'NONE',  ( 5.366025703835962446, 0.9229158262306772498, 1.627043297953718382 ) ) ;
#144393 = ORIENTED_EDGE ( 'NONE', *, *, #93332, .T. ) ;
#144392 = CARTESIAN_POINT ( 'NONE',  ( 1.242498012622397674, 0.3540479964400863877, 1.790853789395550955 ) ) ;
#144395 = CARTESIAN_POINT ( 'NONE',  ( 4.746850994788568201, 8.189453717816405742, 0.7312505120831546135 ) ) ;
#144394 = CARTESIAN_POINT ( 'NONE',  ( 4.811249113497881424, 1.919052844561389692, 1.089612025192594258 ) ) ;
#144396 = CARTESIAN_POINT ( 'NONE',  ( -1.402160292154681736E-14, -0.9281249996585830830, 1.575800808251672791 ) ) ;
#144397 = CARTESIAN_POINT ( 'NONE',  ( 3.279784535431028658, -1.988673744353728123, 0.5473864365612387539 ) ) ;
#144398 = CARTESIAN_POINT ( 'NONE',  ( -7.316596452869116973, 11.68777962832266049, 0.7998128361456481317 ) ) ;
#144399 = PLANE ( 'NONE',  #15973 ) ;
#144400 = CARTESIAN_POINT ( 'NONE',  ( 8.703444544968814256, 12.24143683818393313, -1.199719254218446718 ) ) ;
#144401 = CARTESIAN_POINT ( 'NONE',  ( 1.449478204280065352, 3.367485310445687663, 0.3909668688984510587 ) ) ;
#144402 = CARTESIAN_POINT ( 'NONE',  ( 7.834948825496932834, -6.134628647623485698, 7.720982897393586342 ) ) ;
#144403 = CARTESIAN_POINT ( 'NONE',  ( 7.178115983792402233, 7.339166500704784823, 0.7998128361456281477 ) ) ;
#144404 = MECHANICAL_DESIGN_GEOMETRIC_PRESENTATION_REPRESENTATION (  '', ( #50797 ), #113192 ) ;
#144405 = VERTEX_POINT ( 'NONE', #188448 ) ;
#144406 = CARTESIAN_POINT ( 'NONE',  ( 5.195788487752976081, -1.461605715988937515, -1.466586839339318882 ) ) ;
#144407 = CARTESIAN_POINT ( 'NONE',  ( -1.364683531250000748, 0.07187500034142035865, 0.000000000000000000 ) ) ;
#144408 = CARTESIAN_POINT ( 'NONE',  ( 2.161604200734370096, 0.3718190433680613749, -2.129227089361292791 ) ) ;
#144409 = CARTESIAN_POINT ( 'NONE',  ( -4.976059700032323896, 7.958698620104867061, 1.042642055368933285 ) ) ;
#144410 = CARTESIAN_POINT ( 'NONE',  ( 3.598311091834342612, -0.9934155151001385908, 1.758370388466141465 ) ) ;
#144411 = CARTESIAN_POINT ( 'NONE',  ( 6.620655732516650183, 4.692022689331314389, 2.636326274693585159 ) ) ;
#144413 = CARTESIAN_POINT ( 'NONE',  ( 6.304178240674458422, 10.29869901418813782, 1.040834085586084257E-14 ) ) ;
#144412 = CARTESIAN_POINT ( 'NONE',  ( 0.000000000000000000, -0.7875000000000005329, -4.012584370867899430 ) ) ;
#144414 = CARTESIAN_POINT ( 'NONE',  ( -4.950135482320929370, 5.908151163196758482, -1.082531754730549967 ) ) ;
#144415 = CARTESIAN_POINT ( 'NONE',  ( 1.112517963266421939, 1.944731545904467396, 0.5331650539944567946 ) ) ;
#144416 = CARTESIAN_POINT ( 'NONE',  ( 5.636325218313963603, 0.4264374063192889475, 2.149501299143250055 ) ) ;
#144417 = CARTESIAN_POINT ( 'NONE',  ( -1.500000000000011324, 4.202083334016156080, 0.8660254037844403729 ) ) ;
#144418 = CARTESIAN_POINT ( 'NONE',  ( 5.045129621168108258, 0.1466893748028278155, 1.906852434080000824 ) ) ;
#144419 = CARTESIAN_POINT ( 'NONE',  ( -2.981903720001798597, 5.566305875722335372, -1.199719254218446718 ) ) ;
#144420 = CARTESIAN_POINT ( 'NONE',  ( 6.927853306458749749, 8.145212281365775908, 1.082531754730558626 ) ) ;
#144422 = CARTESIAN_POINT ( 'NONE',  ( 3.286732619643798703, 1.587825416925658262, -1.242744175535138940 ) ) ;
#144421 = CARTESIAN_POINT ( 'NONE',  ( -8.744645890690007306, 12.18554205823825498, 1.082531754730558626 ) ) ;
#144423 = CARTESIAN_POINT ( 'NONE',  ( -1.364683531250000748, 14.17187500034140157, 0.000000000000000000 ) ) ;
#144424 = CARTESIAN_POINT ( 'NONE',  ( -4.329849954717889915, 6.144853928627882489, 1.599625672291270506 ) ) ;
#144425 = CARTESIAN_POINT ( 'NONE',  ( 5.790025292147505276, -0.7713913475298206368, 1.542752225890047679 ) ) ;
#144426 = CARTESIAN_POINT ( 'NONE',  ( 7.374709211190586089, 7.568525266002632534, 0.000000000000000000 ) ) ;
#144427 = CARTESIAN_POINT ( 'NONE',  ( 4.356247428692526569, 3.976710176429713250, 0.7998128361456341429 ) ) ;
#144428 = DIRECTION ( 'NONE',  ( 1.000000000000000000, 0.000000000000000000, -0.000000000000000000 ) ) ;
#144429 = CARTESIAN_POINT ( 'NONE',  ( 5.510910596163088569E-16, 1.000000000000000888, 4.500000000000000000 ) ) ;
#144430 = CARTESIAN_POINT ( 'NONE',  ( 0.5321919801732944988, 1.189095644551215525, 1.694524325727378322 ) ) ;
#144431 = CARTESIAN_POINT ( 'NONE',  ( -1.490514837427310058, 7.209629588552702195, -4.246172784736847561 ) ) ;
#144432 = ORIENTED_EDGE ( 'NONE', *, *, #119884, .F. ) ;
#144433 = CARTESIAN_POINT ( 'NONE',  ( 5.320911890206324379, 1.367686037040320768, -1.187891890861958899 ) ) ;
#144434 = CARTESIAN_POINT ( 'NONE',  ( 4.193214648376505593, 8.114110533073061404, 0.000000000000000000 ) ) ;
#144435 = CARTESIAN_POINT ( 'NONE',  ( -1.452583904633382383, 1.374772708486763806, 1.500000000000001332 ) ) ;
#144436 = CARTESIAN_POINT ( 'NONE',  ( 6.604213110542080045, -0.7679849629102013520, 1.639316308541746592 ) ) ;
#144437 = CARTESIAN_POINT ( 'NONE',  ( 6.183927461164522299, 6.387205924212962849, 0.000000000000000000 ) ) ;
#144438 = CARTESIAN_POINT ( 'NONE',  ( 11.34721833292158699, 8.766100218939394395, 3.908682455922633192 ) ) ;
#144439 = CARTESIAN_POINT ( 'NONE',  ( 2.730644157659181559, 0.2691629481662433099, 2.174792594416566249 ) ) ;
#144440 = EDGE_LOOP ( 'NONE', ( #87771, #66024, #123784, #156635 ) ) ;
#144441 = STYLED_ITEM ( 'NONE', ( #120677 ), #151177 ) ;
#144443 = CARTESIAN_POINT ( 'NONE',  ( 9.576136569953906275, 10.06658084123472641, 0.000000000000000000 ) ) ;
#144442 = CARTESIAN_POINT ( 'NONE',  ( 0.3265133270617843197, -1.284392789319420913, 1.483054880892266114 ) ) ;
#144444 = CARTESIAN_POINT ( 'NONE',  ( 4.640194291141960470, 0.7370120463812566136, 1.768359169405645304 ) ) ;
#144445 = DIRECTION ( 'NONE',  ( -0.9885327375000381167, 0.000000000000000000, 0.1510067114093955609 ) ) ;
#144446 = CARTESIAN_POINT ( 'NONE',  ( -6.496151039430258400, 6.761311432142845135, -0.1280508955800782056 ) ) ;
#144447 = DIRECTION ( 'NONE',  ( 7.105427357601001859E-15, 0.000000000000000000, 1.000000000000000000 ) ) ;
#144448 = CARTESIAN_POINT ( 'NONE',  ( -1.364683531250014514, -0.01145833299191483488, -0.7879004041258359514 ) ) ;
#144450 = ORIENTED_EDGE ( 'NONE', *, *, #22894, .T. ) ;
#144449 = CARTESIAN_POINT ( 'NONE',  ( 5.178851490740196795, 7.065079377328788546, 1.443375672974062551 ) ) ;
#144451 = CARTESIAN_POINT ( 'NONE',  ( -9.680158490477310806, 10.39586578175276266, 0.7216878364870438212 ) ) ;
#144452 = CARTESIAN_POINT ( 'NONE',  ( 2.413140945657660907, 1.930630709398067246, 0.9725960170764782475 ) ) ;
#144453 = CARTESIAN_POINT ( 'NONE',  ( -4.634908411025374875, 6.500755460986618495, 1.599625672291263179 ) ) ;
#144454 = CARTESIAN_POINT ( 'NONE',  ( 6.048345925472166762, 10.07050432311064903, 0.7216878364870317197 ) ) ;
#144455 = CARTESIAN_POINT ( 'NONE',  ( 1.676486011727536418, -1.732352342712149440, -0.5761224636358779350 ) ) ;
#144456 = CARTESIAN_POINT ( 'NONE',  ( -0.1929003719821283658, -0.4722129235960636495, -2.074948700427194481 ) ) ;
#144457 = CARTESIAN_POINT ( 'NONE',  ( 4.207882836062684540, -1.820678405428953095, 0.1343838851760314757 ) ) ;
#144458 = CARTESIAN_POINT ( 'NONE',  ( 9.809883170912574002, 12.88719579058855125, -8.001885615786651584 ) ) ;
#144459 = CARTESIAN_POINT ( 'NONE',  ( 2.830216799141628492, -0.9462872844297947061, -1.661813493071498726 ) ) ;
#144460 = VERTEX_POINT ( 'NONE', #61653 ) ;
#144461 = CARTESIAN_POINT ( 'NONE',  ( 3.525798893484650254, 1.922080780809858114, -0.4290687576708405726 ) ) ;
#144462 = EDGE_LOOP ( 'NONE', ( #144758, #136874, #37097, #23067 ) ) ;
#144463 = CARTESIAN_POINT ( 'NONE',  ( 5.829623785595809515, 0.9536246560681378437, -1.691722214391349732 ) ) ;
#144464 = ORIENTED_EDGE ( 'NONE', *, *, #20907, .F. ) ;
#144465 = CARTESIAN_POINT ( 'NONE',  ( -6.557303570864871034, 7.679217583210999010, -1.199719254218452047 ) ) ;
#144467 = CARTESIAN_POINT ( 'NONE',  ( 6.469000917296717112, -1.638331675554663747, 1.346054232038436105 ) ) ;
#144466 = CARTESIAN_POINT ( 'NONE',  ( -4.797606254389363833, 6.690569611577942943, 1.599625672291263179 ) ) ;
#144468 = CARTESIAN_POINT ( 'NONE',  ( 6.983858524370772258, 9.241197259889668558, 1.443375672974063439 ) ) ;
#144469 = CARTESIAN_POINT ( 'NONE',  ( 3.897043152223302886, -0.1904361752127527174, -1.902785305300330743 ) ) ;
#144470 = CARTESIAN_POINT ( 'NONE',  ( 4.566373025097719029, 7.183545020864719355, -1.317121582780217404 ) ) ;
#144471 = CARTESIAN_POINT ( 'NONE',  ( -1.685698123273788429, -1.500000000000000000, 1.979500400907064916 ) ) ;
#144472 = CARTESIAN_POINT ( 'NONE',  ( -2.128168088883454642E-12, -3.089410100848593466, 3.428390338093493028 ) ) ;
#144473 = CARTESIAN_POINT ( 'NONE',  ( 5.567046518764520613, -1.585636444731153061, 1.240160563295252372 ) ) ;
#144474 = CARTESIAN_POINT ( 'NONE',  ( 0.07933194151889190471, -9.902237888914267927, 9.499668754386327407 ) ) ;
#144475 = CARTESIAN_POINT ( 'NONE',  ( 6.551389018236878137, -1.469694460105780642, -1.082916835497591324 ) ) ;
#144476 = CARTESIAN_POINT ( 'NONE',  ( 0.8364851226981102617, -1.151554295457988930, 1.720357586142134076 ) ) ;
#144477 = CARTESIAN_POINT ( 'NONE',  ( -8.541273586929371220, 9.067166727613487964, 0.7216878364870438212 ) ) ;
#144478 = CARTESIAN_POINT ( 'NONE',  ( -5.543397514969483630, 7.443247485022737031, -1.247832777738608678 ) ) ;
#144479 = PLANE ( 'NONE',  #91496 ) ;
#144480 = CARTESIAN_POINT ( 'NONE',  ( 3.285556943749998737, -2.705208332855374209, -1.896917185911906722 ) ) ;
#144481 = CARTESIAN_POINT ( 'NONE',  ( 6.287230548435207567, 8.358188277972981695, -1.599625672291262513 ) ) ;
#144482 = SURFACE_STYLE_USAGE ( .BOTH. , #192094 ) ;
#144483 = EDGE_CURVE ( 'NONE', #89251, #154238, #206397, .T. ) ;
#144484 = CARTESIAN_POINT ( 'NONE',  ( -0.6823417656250003738, 11.96354166700806765, 1.181850606188754593 ) ) ;
#144485 = CARTESIAN_POINT ( 'NONE',  ( -5.623934791570306402, 5.455678766453782913, 0.7998128361456341429 ) ) ;
#144487 = CARTESIAN_POINT ( 'NONE',  ( -5.759181390754928742, 9.941071732514568993, 0.000000000000000000 ) ) ;
#144486 = CARTESIAN_POINT ( 'NONE',  ( -15.75000000000000000, 12.69999999999998153, 1.399999999999998579 ) ) ;
#144488 = CARTESIAN_POINT ( 'NONE',  ( 3.920349067101033036, -1.199671410015031192, -1.252466492151423694 ) ) ;
#144489 = CARTESIAN_POINT ( 'NONE',  ( -4.229253852459088137, 7.021547696922494808, 1.199719254218464037 ) ) ;
#144490 = CARTESIAN_POINT ( 'NONE',  ( 1.657173498210939622, 1.694793865239911712, -1.188712540599102141 ) ) ;
#144491 = CARTESIAN_POINT ( 'NONE',  ( 2.284896850813819213, 1.698563897025050506, -1.263734059995786030 ) ) ;
#144492 = CARTESIAN_POINT ( 'NONE',  ( 3.330499290451326200, 7.037332938835193730, -0.7998128361456291469 ) ) ;
#144493 = CARTESIAN_POINT ( 'NONE',  ( 7.293396569147545527, 10.59638086639245280, 1.199719254218460707 ) ) ;
#144494 = CARTESIAN_POINT ( 'NONE',  ( 5.736508392357904107, 5.865217010605237924, 0.000000000000000000 ) ) ;
#144495 = CARTESIAN_POINT ( 'NONE',  ( 0.3386328343033001564, -1.908876393446774955, -0.4841592594212947298 ) ) ;
#144497 = B_SPLINE_CURVE_WITH_KNOTS ( 'NONE', 3,
 ( #30261, #212181, #109446, #95283, #96347, #161331 ),
 .UNSPECIFIED., .F., .F.,
 ( 4, 2, 4 ),
 ( 0.000000000000000000, 0.0003767011250903909642, 0.0007534022501807819284 ),
 .UNSPECIFIED. ) ;
#144496 = CARTESIAN_POINT ( 'NONE',  ( 4.798800619506367049, 6.970516071510092893, 1.407892184351482889 ) ) ;
#144498 = CARTESIAN_POINT ( 'NONE',  ( 3.375617060122621194, 6.882044303544283537, 1.040834085586084257E-14 ) ) ;
#144500 = CARTESIAN_POINT ( 'NONE',  ( 3.189213936345665523, 2.817530495244580102, 2.450448857954567572 ) ) ;
#144499 = CARTESIAN_POINT ( 'NONE',  ( 3.475000000000000533, -1.545833333333334503, -2.006292185433951047 ) ) ;
#144501 = CARTESIAN_POINT ( 'NONE',  ( 2.062813984423640612, -2.096776522422974409, -0.9266714075790563054 ) ) ;
#144502 = CARTESIAN_POINT ( 'NONE',  ( 0.7502976729042536430, 0.5272139720400963459, 1.747899773703022408 ) ) ;
#144503 = CARTESIAN_POINT ( 'NONE',  ( 3.181800181368432678, 1.864768544494728175, -0.4233684943922080834 ) ) ;
#144504 = CARTESIAN_POINT ( 'NONE',  ( 6.180537922983273091, 8.303989891604203422, -1.599625672291281386 ) ) ;
#144505 = CARTESIAN_POINT ( 'NONE',  ( 6.602457619730756733, 9.686322408785807525, 1.082531754730558626 ) ) ;
#144506 = CARTESIAN_POINT ( 'NONE',  ( -7.296259222448620463, 11.66405285949874759, 0.7998128361456481317 ) ) ;
#144507 = CARTESIAN_POINT ( 'NONE',  ( 1.670183121039736207, 2.007516039388768991, -0.1524388337148015193 ) ) ;
#144508 = CARTESIAN_POINT ( 'NONE',  ( 1.692165188054130187, 0.9715730843921737137, -1.704227633833883759 ) ) ;
#144509 = CARTESIAN_POINT ( 'NONE',  ( -8.646349277213090545, 11.11049346154719508, 1.599625672291269396 ) ) ;
#144510 = CARTESIAN_POINT ( 'NONE',  ( -8.213542131780492639, 8.476887330032372603, 1.040834085586084257E-14 ) ) ;
#144511 = CARTESIAN_POINT ( 'NONE',  ( -7.501945787865621718, -5.223163706540480788, -8.013579835756324599 ) ) ;
#144513 = CARTESIAN_POINT ( 'NONE',  ( 2.922431196026415101, 1.665835785064853969, 0.5981315555363684311 ) ) ;
#144512 = CARTESIAN_POINT ( 'NONE',  ( 4.751946794759532189, 0.7997392584290877737, 1.931828438813171456 ) ) ;
#144514 = CARTESIAN_POINT ( 'NONE',  ( 0.3554123170485725680, 15.00000000000058265, 12.67999999502907649 ) ) ;
#144516 = CARTESIAN_POINT ( 'NONE',  ( 6.650320093084655326, -1.776417932240816011, 1.448308594842239838 ) ) ;
#144515 = DIRECTION ( 'NONE',  ( -5.551115123125758667E-17, 0.000000000000000000, 1.000000000000000000 ) ) ;
#144517 = CARTESIAN_POINT ( 'NONE',  ( 4.417713501739753745, 1.067903927642421591, -1.374066674465204363 ) ) ;
#144518 = CARTESIAN_POINT ( 'NONE',  ( 7.540305987494599016, 11.94877408538573427, -0.7998128361456291469 ) ) ;
#144519 = PRESENTATION_STYLE_ASSIGNMENT (( #94682 ) ) ;
#144520 = CARTESIAN_POINT ( 'NONE',  ( 4.745267847829638619, -1.681796892959321665, -0.4208994435666196798 ) ) ;
#144521 = CARTESIAN_POINT ( 'NONE',  ( 4.158752335142390955, -0.6773029245935069387, -2.062915381819859562 ) ) ;
#144522 = CARTESIAN_POINT ( 'NONE',  ( 5.020596955762157698, 4.751784624677624080, 1.040834085586084257E-14 ) ) ;
#144523 = CARTESIAN_POINT ( 'NONE',  ( 6.280482454654814362, -0.5424645211669875122, -1.942098458069536848 ) ) ;
#144524 = CARTESIAN_POINT ( 'NONE',  ( 6.312500000001141309, 1.451031289089316667, 1.451031289060858098 ) ) ;
#144525 = AXIS2_PLACEMENT_3D ( 'NONE', #175925, #9137, #40588 ) ;
#144526 = CARTESIAN_POINT ( 'NONE',  ( 11.06298660227979802, 9.843196003747330280, -0.9087478855431304625 ) ) ;
#144527 = CARTESIAN_POINT ( 'NONE',  ( 3.118101180835719521, -0.9482820236139007930, -1.676744857821835355 ) ) ;
#144528 = CARTESIAN_POINT ( 'NONE',  ( -0.7500000000000006661, 10.23958333401612997, -1.299038105676657340 ) ) ;
#144529 = CARTESIAN_POINT ( 'NONE',  ( 0.1533981569187261029, 0.3862642299664406642, 2.187325829255863940 ) ) ;
#144530 = VERTEX_POINT ( 'NONE', #74708 ) ;
#144531 = CARTESIAN_POINT ( 'NONE',  ( 6.883263157960393563, 1.268976584491373183, 2.060807272249213451 ) ) ;
#144532 = CARTESIAN_POINT ( 'NONE',  ( -1.201851678989727383E-14, 3.462500000000019895, 1.732050807568877637 ) ) ;
#144533 = CARTESIAN_POINT ( 'NONE',  ( 4.635998460869027227, 7.496083073400806818, -1.199719254218452047 ) ) ;
#144534 = CARTESIAN_POINT ( 'NONE',  ( 2.227449089350467482, 1.985603210742479252, 0.9958825451741261103 ) ) ;
#144535 = CARTESIAN_POINT ( 'NONE',  ( 0.000000000000000000, 2.000000000000001776, 0.000000000000000000 ) ) ;
#144536 = CARTESIAN_POINT ( 'NONE',  ( 6.616015773788773480, 10.66250946948817813, -0.7216878364870267237 ) ) ;
#144537 = CARTESIAN_POINT ( 'NONE',  ( -8.636180661780651135, 13.01936850547871138, -0.7216878364870257245 ) ) ;
#144538 = CARTESIAN_POINT ( 'NONE',  ( 4.848976215542928792, 5.686169002002086970, 1.199719254218452047 ) ) ;
#144540 = CIRCLE ( 'NONE', #47737, 0.08000000000000020983 ) ;
#144539 = AXIS2_PLACEMENT_3D ( 'NONE', #72195, #157757, #92769 ) ;
#144541 = CARTESIAN_POINT ( 'NONE',  ( 0.5279704824466545654, -1.728000714500482982, 1.038995864524896673 ) ) ;
#144543 = CARTESIAN_POINT ( 'NONE',  ( 5.283662074727401681, -1.959763400824132251, 0.6436608119341418188 ) ) ;
#144542 = CARTESIAN_POINT ( 'NONE',  ( 9.185812768458653466, 10.67553530374532045, 1.199719254218453823 ) ) ;
#144544 = SURFACE_STYLE_USAGE ( .BOTH. , #28616 ) ;
#144545 = CARTESIAN_POINT ( 'NONE',  ( -5.101945877444165944, 4.846691699973280976, 0.000000000000000000 ) ) ;
#144546 = CARTESIAN_POINT ( 'NONE',  ( -1.201851678989727383E-14, 5.618750000682818602, -1.732050807568863648 ) ) ;
#144547 = CARTESIAN_POINT ( 'NONE',  ( 1.364683531249986537, 0.8635416670080893198, 0.7879004041258500513 ) ) ;
#144548 = CARTESIAN_POINT ( 'NONE',  ( 6.872336254976084469, -1.150436037642876608, 1.475500831757702969 ) ) ;
#144549 = CARTESIAN_POINT ( 'NONE',  ( 5.942016496743827147, -1.492280758002052510, -0.8831153342708076837 ) ) ;
#144550 = CARTESIAN_POINT ( 'NONE',  ( 6.022986557963563747, -1.635662919198093812, 0.5951793741951169059 ) ) ;
#144551 = CARTESIAN_POINT ( 'NONE',  ( 2.472590379642979563, -2.194723544211283350, -0.6619992606377905764 ) ) ;
#144552 = CARTESIAN_POINT ( 'NONE',  ( 1.364683531249986537, -0.1364583329919154264, 0.7879004041258500513 ) ) ;
#144553 = CARTESIAN_POINT ( 'NONE',  ( 0.7965151530783078915, 1.503791256141374211, 1.061989520254283059 ) ) ;
#144554 = CARTESIAN_POINT ( 'NONE',  ( 1.347111479062088405E-15, 6.999999999999999112, 11.00000000000000000 ) ) ;
#144555 = CARTESIAN_POINT ( 'NONE',  ( 1.729251940891060713, -1.720190037149814444, 0.6116943438041824166 ) ) ;
#144556 = CARTESIAN_POINT ( 'NONE',  ( 1.166276502169643070, -1.387892208999995436, 1.695937554688830451 ) ) ;
#144557 = CARTESIAN_POINT ( 'NONE',  ( 8.793960880499607669, 13.45135513836973296, -7.698180313484015436 ) ) ;
#144558 = CARTESIAN_POINT ( 'NONE',  ( 4.858481695672255185, 0.8034365979220282616, 1.946882858121199211 ) ) ;
#144559 = CARTESIAN_POINT ( 'NONE',  ( -5.038826645773246682, 9.030381520044109322, 0.7998128361456481317 ) ) ;
#144560 = CARTESIAN_POINT ( 'NONE',  ( 8.800798923547361596, 13.41831251038806982, 7.690207505967889823 ) ) ;
#144561 = CARTESIAN_POINT ( 'NONE',  ( 1.750525128138082254, -2.060206210462053988, -0.2049951091474821463 ) ) ;
#144562 = CARTESIAN_POINT ( 'NONE',  ( 4.306686350635271054, 8.176217842383143974, -0.7998128361456221525 ) ) ;
#144563 = CARTESIAN_POINT ( 'NONE',  ( -3.956095110007852622E-14, -0.1406249996585586248, -1.570758158831808249 ) ) ;
#144564 = CARTESIAN_POINT ( 'NONE',  ( 4.336665864168765872, 1.303721989063952424, -1.672289659653345639 ) ) ;
#144565 = CARTESIAN_POINT ( 'NONE',  ( 0.2055245034400269288, -0.5150763003200479195, 1.856310442892949553 ) ) ;
#144566 = ORIENTED_EDGE ( 'NONE', *, *, #199147, .T. ) ;
#144567 = CARTESIAN_POINT ( 'NONE',  ( -5.468734858265826837, 7.473552982767158070, 1.599625672291263179 ) ) ;
#144568 = CARTESIAN_POINT ( 'NONE',  ( 8.075853055234393452, 12.57357899774884658, 0.7998128361456462443 ) ) ;
#144569 = CARTESIAN_POINT ( 'NONE',  ( 5.682275777458829502, 9.643422483761748154, 0.7216878364870317197 ) ) ;
#144570 = CARTESIAN_POINT ( 'NONE',  ( 0.000000000000000000, -1.793749999044085275, -4.012584370867899430 ) ) ;
#144571 = CARTESIAN_POINT ( 'NONE',  ( -5.253948220495577637, 6.088359997788290734, 1.199719254218450271 ) ) ;
#144572 = CARTESIAN_POINT ( 'NONE',  ( 5.959260761812961604, -1.790568634313693730, 1.135864312162476297 ) ) ;
#144573 = CARTESIAN_POINT ( 'NONE',  ( 1.290213853529555976, -0.9470325862265884798, 1.881093767389901750 ) ) ;
#144574 = CARTESIAN_POINT ( 'NONE',  ( -3.644109427023046521, 7.473487774827342278, 0.000000000000000000 ) ) ;
#144575 = CARTESIAN_POINT ( 'NONE',  ( 9.240045382913317340, 10.73880668727576015, -1.199719254218446718 ) ) ;
#144576 = CARTESIAN_POINT ( 'NONE',  ( 5.383604208181901107, -1.767738693978682996, 0.5818682867176503404 ) ) ;
#144577 = CARTESIAN_POINT ( 'NONE',  ( 7.832860060393120882, 10.16142270859057462, 1.599625672291281386 ) ) ;
#144578 = CARTESIAN_POINT ( 'NONE',  ( 0.4170821662628915183, 3.033599471985643170, 0.4170821662628724225 ) ) ;
#144579 = CARTESIAN_POINT ( 'NONE',  ( -2.972980823146582186, 6.690504403638126263, 0.000000000000000000 ) ) ;
#144581 = CARTESIAN_POINT ( 'NONE',  ( -8.785320351975364872, 12.23299559640450518, 1.082531754730560403 ) ) ;
#144580 = AXIS2_PLACEMENT_3D ( 'NONE', #131027, #83257, #32395 ) ;
#144582 = CARTESIAN_POINT ( 'NONE',  ( -7.712474369503357075, -6.289226506789209914, -7.712474369503310889 ) ) ;
#144584 = CARTESIAN_POINT ( 'NONE',  ( 2.172246964874047670, -0.9220853831424129510, -1.731647142839589648 ) ) ;
#144583 = CARTESIAN_POINT ( 'NONE',  ( -6.989391883044787868, 8.113044270762433285, -1.199719254218446718 ) ) ;
#144585 = CARTESIAN_POINT ( 'NONE',  ( 0.7433210806352362754, -1.853469564684958382, 1.112228649290482263 ) ) ;
#144587 = CARTESIAN_POINT ( 'NONE',  ( -6.138273485042783584, 5.995793210058552702, 0.01269068828805425264 ) ) ;
#144586 = CARTESIAN_POINT ( 'NONE',  ( -6.310394152517827315, 6.326824364217716656, 0.7998128361456281477 ) ) ;
#144588 = CARTESIAN_POINT ( 'NONE',  ( -1.402160292154681736E-14, -0.1781249996585796136, 1.575800808251672791 ) ) ;
#144589 = CARTESIAN_POINT ( 'NONE',  ( 2.582960874182936628, 1.135899660060729399, -1.309998962497432196 ) ) ;
#144590 = CARTESIAN_POINT ( 'NONE',  ( 2.079653994411820417, -1.706432041406182654, -0.3408243062450431182 ) ) ;
#144591 = CARTESIAN_POINT ( 'NONE',  ( 6.805829924380108586, 8.963220883242035697, 1.443375672974076540 ) ) ;
#144592 = CARTESIAN_POINT ( 'NONE',  ( -10.60630588279735242, 5.715763139788331948, 4.896273837757428637 ) ) ;
#144593 = VECTOR ( 'NONE', #67100, 1000.000000000000000 ) ;
#144594 = CARTESIAN_POINT ( 'NONE',  ( 0.8255457999647041190, -1.462224166115761337, 1.388270745661695837 ) ) ;
#144595 = CARTESIAN_POINT ( 'NONE',  ( 6.925078400183597438, 7.629137130509070275, 2.744348168701661095 ) ) ;
#144596 = CARTESIAN_POINT ( 'NONE',  ( -5.659602779061863487, 5.567567761852417085, 0.7998128361456281477 ) ) ;
#144597 = CARTESIAN_POINT ( 'NONE',  ( 0.8660190917160478508, 0.9698478150794390684, 1.716334202883246229 ) ) ;
#144599 = CARTESIAN_POINT ( 'NONE',  ( -5.153507786970267013, 8.066157280557016307, -1.082531754730549967 ) ) ;
#144598 = CARTESIAN_POINT ( 'NONE',  ( 5.677967274442059953, 1.882970570262190835, -0.3333453579756898155 ) ) ;
#144600 = CARTESIAN_POINT ( 'NONE',  ( -7.282137903871469753, 8.628820655005750240, 1.082531754730549078 ) ) ;
#144601 = CARTESIAN_POINT ( 'NONE',  ( 6.873057527484919937, 6.983264968346048818, 0.7998128361456352531 ) ) ;
#144602 = CARTESIAN_POINT ( 'NONE',  ( -5.986807348886189040, 9.142303119412650503, -1.199719254218452047 ) ) ;
#144603 = CARTESIAN_POINT ( 'NONE',  ( 0.9264325174072656210, -0.9100096784926974269, -1.803132658094412477 ) ) ;
#144604 = DIRECTION ( 'NONE',  ( 0.000000000000000000, -1.000000000000000000, 0.000000000000000000 ) ) ;
#144605 = CARTESIAN_POINT ( 'NONE',  ( 4.841030633121579996, 0.3891503725830172677, 2.274395804800657839 ) ) ;
#144606 = CARTESIAN_POINT ( 'NONE',  ( 6.215287892896892430, -1.681934637451238279, -1.009743211781432670 ) ) ;
#144607 = CARTESIAN_POINT ( 'NONE',  ( 3.326955106232618586, -1.810811308836293598, -0.7551016064811162387 ) ) ;
#144608 = CARTESIAN_POINT ( 'NONE',  ( 8.075853055234393452, 12.57357899774884658, 0.7998128361456462443 ) ) ;
#144609 = CARTESIAN_POINT ( 'NONE',  ( -9.489836703312123589, 15.20205537403712093, 7.238794766165088213 ) ) ;
#144610 = VERTEX_POINT ( 'NONE', #93110 ) ;
#144611 = CARTESIAN_POINT ( 'NONE',  ( 1.587271696126206111, 1.763578281176042761, 1.171447882250826522 ) ) ;
#144613 = CARTESIAN_POINT ( 'NONE',  ( -7.751511138711140170, 10.06651563329490529, -1.599625672291263179 ) ) ;
#144612 = CARTESIAN_POINT ( 'NONE',  ( -2.449219305563052895, 6.009172956465517856, 1.040834085586084257E-14 ) ) ;
#144614 = CARTESIAN_POINT ( 'NONE',  ( 1.341482821134845738, 1.838956754096718660, 0.09199767257135618714 ) ) ;
#144615 = ORIENTED_EDGE ( 'NONE', *, *, #91785, .T. ) ;
#144616 = CARTESIAN_POINT ( 'NONE',  ( 11.87979087550123758, 7.786822373289821186, -1.749581464211011905 ) ) ;
#144618 = EDGE_CURVE ( 'NONE', #50335, #11614, #123630, .T. ) ;
#144617 = CARTESIAN_POINT ( 'NONE',  ( 2.408575119285644384, -2.115224228095522907, -0.1514441693673748146 ) ) ;
#144619 = CARTESIAN_POINT ( 'NONE',  ( 1.499999999999990896, 4.556250000682819490, 1.214306433183764966E-14 ) ) ;
#144620 = CARTESIAN_POINT ( 'NONE',  ( 9.185812768458653466, 10.67553530374532045, 1.199719254218453823 ) ) ;
#144621 = DIRECTION ( 'NONE',  ( 0.000000000000000000, 0.000000000000000000, -1.000000000000000000 ) ) ;
#144622 = CARTESIAN_POINT ( 'NONE',  ( 3.339188440279222458, -1.819168825518402199, 0.9681599264559497264 ) ) ;
#144624 = CARTESIAN_POINT ( 'NONE',  ( 0.2570343420702363435, 1.821350608449383124, -0.2692129421619017804 ) ) ;
#144623 = CARTESIAN_POINT ( 'NONE',  ( -8.528242318195895066, 9.908369778438709474, 1.199719254218462483 ) ) ;
#144625 = CARTESIAN_POINT ( 'NONE',  ( 1.364683531249990311, 3.634375000341416584, 1.214306433183764966E-14 ) ) ;
#144626 = PRESENTATION_STYLE_ASSIGNMENT (( #75316 ) ) ;
#144627 = CARTESIAN_POINT ( 'NONE',  ( 1.393530502278612637, 4.337808571543051883, -0.1277288169565287124 ) ) ;
#144628 = CARTESIAN_POINT ( 'NONE',  ( 0.2587985324217950689, 0.8487602207661277820, 2.037339956011212649 ) ) ;
#144629 = CARTESIAN_POINT ( 'NONE',  ( 2.249658590878771847, -1.816102774931172448, -1.348951556275684194 ) ) ;
#144630 = CARTESIAN_POINT ( 'NONE',  ( -8.459924665247381625, 11.85336729522185806, 1.082531754730560403 ) ) ;
#144631 = CARTESIAN_POINT ( 'NONE',  ( 2.126969254794884634, 1.619647995875729496, 0.8116002879420233240 ) ) ;
#144632 = CARTESIAN_POINT ( 'NONE',  ( 2.747180457951060362, 0.2762254639866565942, -1.895546175561702018 ) ) ;
#144633 = CARTESIAN_POINT ( 'NONE',  ( 3.719242722441223226, -1.824546119899137731, -0.9785211796824041519 ) ) ;
#144634 = CARTESIAN_POINT ( 'NONE',  ( 1.364683531249988757, 2.196875000341415252, 1.214306433183764966E-14 ) ) ;
#144635 = CARTESIAN_POINT ( 'NONE',  ( 2.149238863156129220, -1.582378584423797419, -1.175707468242733977 ) ) ;
#144636 = CARTESIAN_POINT ( 'NONE',  ( 0.3582593949469566885, 0.7340744485371183403, 1.781236698655277895 ) ) ;
#144637 = CARTESIAN_POINT ( 'NONE',  ( 2.658895327995167701, -1.626580691111865207, -0.9237732865615968514 ) ) ;
#144639 = CARTESIAN_POINT ( 'NONE',  ( 4.771426152247889796, 8.279957873513081879, -0.8122977234717634332 ) ) ;
#144638 = CARTESIAN_POINT ( 'NONE',  ( 1.102667438898880192, -2.307868968971817036, 0.004735511273680144059 ) ) ;
#144640 = CARTESIAN_POINT ( 'NONE',  ( 3.138934141195717675, -0.1340819638860979157, -1.856265897873999426 ) ) ;
#144641 = CARTESIAN_POINT ( 'NONE',  ( 0.6823417656249899377, 3.176041667008085323, -1.181850606188754593 ) ) ;
#144642 = CARTESIAN_POINT ( 'NONE',  ( 6.654736832427365911, -0.5462217193984253427, -1.988994552010774797 ) ) ;
#144643 = CARTESIAN_POINT ( 'NONE',  ( -6.410307701162927252, 6.373113827645189744, -0.7998128361456291469 ) ) ;
#144644 = CARTESIAN_POINT ( 'NONE',  ( 6.076025397218672630, 10.24044673006381245, -0.7998128361456291469 ) ) ;
#144645 = CARTESIAN_POINT ( 'NONE',  ( -1.449495214452822145, 3.367398793782839128, -0.3909641857570709811 ) ) ;
#144646 = ADVANCED_FACE ( 'NONE', ( #11821 ), #182894, .T. ) ;
#144647 = CARTESIAN_POINT ( 'NONE',  ( 5.948290813881442318, 2.103388047956732620, 0.1067411848718266276 ) ) ;
#144648 = CARTESIAN_POINT ( 'NONE',  ( 1.364683531249990311, 4.446875000341417028, 1.214306433183764966E-14 ) ) ;
#144649 = CARTESIAN_POINT ( 'NONE',  ( 5.694645791630270182, -0.5191100231263061637, -2.098234375727751733 ) ) ;
#144650 = CARTESIAN_POINT ( 'NONE',  ( 6.041667287826984811, -1.900962894602696185, 0.6825640075473203838 ) ) ;
#144651 = CARTESIAN_POINT ( 'NONE',  ( -1.364683531250014514, -1.011458332991911568, -0.7879004041258359514 ) ) ;
#144652 = CARTESIAN_POINT ( 'NONE',  ( -3.307826292054304673, 6.802955074131234348, -0.7216878364870267237 ) ) ;
#144655 = CARTESIAN_POINT ( 'NONE',  ( 5.355107487717867265, 5.349972945200037522, 1.040834085586084257E-14 ) ) ;
#144654 = CARTESIAN_POINT ( 'NONE',  ( 6.825078400183513416, 0.6012913621265563169, 1.809472532188656890 ) ) ;
#144653 = CARTESIAN_POINT ( 'NONE',  ( 7.523848900940885542, 7.742521570711348389, 0.7998128361456291469 ) ) ;
#144656 = CARTESIAN_POINT ( 'NONE',  ( -5.438755897737433287, 6.374245297895642537, -1.199719254218453823 ) ) ;
#144657 = CARTESIAN_POINT ( 'NONE',  ( 4.434779938697545276, -1.616694733667634942, 1.205040202231235869 ) ) ;
#144658 = CARTESIAN_POINT ( 'NONE',  ( -8.538937818508475885, 8.856515631215026829, 1.040834085586084257E-14 ) ) ;
#144660 = CARTESIAN_POINT ( 'NONE',  ( -7.905812970100109638, 8.396072351304486148, 0.7216878364870317197 ) ) ;
#144659 = CARTESIAN_POINT ( 'NONE',  ( -7.863365906246048809, 12.11775129068834289, -0.7216878364870267237 ) ) ;
#144661 = APPLICATION_CONTEXT ( 'automotive_design' ) ;
#144662 = CARTESIAN_POINT ( 'NONE',  ( -1.201851678989727383E-14, 4.696875000341419693, -1.575800808251660134 ) ) ;
#144664 = CARTESIAN_POINT ( 'NONE',  ( -1.364683531250010740, 8.880208333674731946, 0.7879004041258445001 ) ) ;
#144663 = CARTESIAN_POINT ( 'NONE',  ( 6.332923096303629151, 0.2067577541180857514, 2.151790036905242953 ) ) ;
#144665 = CARTESIAN_POINT ( 'NONE',  ( 10.18278199833527964, 3.974415841077570732, -5.432519183637642080 ) ) ;
#144666 = CARTESIAN_POINT ( 'NONE',  ( -11.33126667303324275, 6.586199079536864787, -3.816285274238954806 ) ) ;
#144668 = CARTESIAN_POINT ( 'NONE',  ( 6.380482474105581225, -0.5405081658083621399, -1.942537888137134461 ) ) ;
#144667 = CARTESIAN_POINT ( 'NONE',  ( -6.277061933002790362, 8.346324893301817482, 1.443375672974078761 ) ) ;
#144669 = CARTESIAN_POINT ( 'NONE',  ( -0.6823417656250003738, -0.9697916663252494907, -1.181850606188749264 ) ) ;
#144670 = CARTESIAN_POINT ( 'NONE',  ( 6.539320575229258026, 4.689551739520863904, 2.765837357486185866 ) ) ;
#144671 = CARTESIAN_POINT ( 'NONE',  ( 2.138867256381206783, -1.541494696628985528, 0.7741069473117598854 ) ) ;
#144672 = CARTESIAN_POINT ( 'NONE',  ( 7.614839552730775729, 8.913009562054615031, 1.199719254218452047 ) ) ;
#144673 = CARTESIAN_POINT ( 'NONE',  ( 6.703580607314123085, 6.785541894813420072, 0.000000000000000000 ) ) ;
#144674 = CARTESIAN_POINT ( 'NONE',  ( -11.98806725462682721, 9.050750434120253374, 0.6182873949870071328 ) ) ;
#144675 = CARTESIAN_POINT ( 'NONE',  ( 6.678970768140332304, -0.09217866350584581758, -1.868372134486769420 ) ) ;
#144676 = CARTESIAN_POINT ( 'NONE',  ( 0.8033857101962671443, 1.774305754185826034, -0.9510189173033887222 ) ) ;
#144677 = SURFACE_SIDE_STYLE ('',( #27680 ) ) ;
#144678 = CARTESIAN_POINT ( 'NONE',  ( 10.73535870392234237, 11.41900666419791399, 0.000000000000000000 ) ) ;
#144679 = CARTESIAN_POINT ( 'NONE',  ( 3.188704395469597497, -2.173853526369253331, -0.3788738375181537332 ) ) ;
#144680 = AXIS2_PLACEMENT_3D ( 'NONE', #120537, #152956, #104217 ) ;
#144681 = CARTESIAN_POINT ( 'NONE',  ( 5.787976215063657115, -1.371286462501415837, -1.683233787797025371 ) ) ;
#144682 = ORIENTED_EDGE ( 'NONE', *, *, #28619, .F. ) ;
#144683 = CARTESIAN_POINT ( 'NONE',  ( -1.402160292154681736E-14, -0.7874999999999764411, 1.732050807568877637 ) ) ;
#144684 = CARTESIAN_POINT ( 'NONE',  ( 10.03267048398825168, 10.80712977418221676, 0.000000000000000000 ) ) ;
#144686 = CARTESIAN_POINT ( 'NONE',  ( 2.653922917551009952, 1.081085551080329443, 1.701936510390425150 ) ) ;
#144685 = CARTESIAN_POINT ( 'NONE',  ( 3.563236855010095461, -1.732559338849114727, 1.222301536229251306 ) ) ;
#144688 = ORIENTED_EDGE ( 'NONE', *, *, #92489, .F. ) ;
#144687 = CARTESIAN_POINT ( 'NONE',  ( 3.041053801226344611, 0.04897401433806568977, 1.811106077260196345 ) ) ;
#144689 = CARTESIAN_POINT ( 'NONE',  ( 4.688087255275310561, 8.691461907788344377, -0.7998128361456381397 ) ) ;
#144690 = ORIENTED_EDGE ( 'NONE', *, *, #137857, .T. ) ;
#144691 = CARTESIAN_POINT ( 'NONE',  ( 0.1978467685152424937, -1.870139902624564865, -0.05068021481659244765 ) ) ;
#144692 = CARTESIAN_POINT ( 'NONE',  ( 6.287230548435207567, 8.358188277972981695, -1.599625672291262513 ) ) ;
#144694 = CARTESIAN_POINT ( 'NONE',  ( 1.235391793297924812, 0.5527703352327991704, -1.834263772151963456 ) ) ;
#144693 = CARTESIAN_POINT ( 'NONE',  ( -4.603156847039612920, 5.329103395422994716, 1.199719254218462483 ) ) ;
#144696 = AXIS2_PLACEMENT_3D ( 'NONE', #93206, #11915, #92140 ) ;
#144695 = VECTOR ( 'NONE', #98646, 1000.000000000000000 ) ;
#144697 = CARTESIAN_POINT ( 'NONE',  ( -1.201851678989727383E-14, 3.462500000000019895, 1.732050807568877637 ) ) ;
#144698 = CARTESIAN_POINT ( 'NONE',  ( 5.026856346975741019, 4.759087247760136918, -0.3692494997280463265 ) ) ;
#144699 = CARTESIAN_POINT ( 'NONE',  ( -1.364683531250014514, 1.551041667008084435, -0.7879004041258289570 ) ) ;
#144700 = CARTESIAN_POINT ( 'NONE',  ( 2.854315967138055132, 6.433244981884085334, -0.2941531795266367211 ) ) ;
#144701 = CARTESIAN_POINT ( 'NONE',  ( -8.646349277213090545, 11.11049346154719508, 1.599625672291269396 ) ) ;
#144702 = CARTESIAN_POINT ( 'NONE',  ( 5.682550338946038337, -2.108058120380253087, -0.4779004524640489415 ) ) ;
#144703 = CARTESIAN_POINT ( 'NONE',  ( -4.990809943606273613, 7.876343129965691858, -1.082531754730549967 ) ) ;
#144704 = CARTESIAN_POINT ( 'NONE',  ( -7.449279056065764237, 7.655523418356991350, 0.7998128361456341429 ) ) ;
#144705 = CARTESIAN_POINT ( 'NONE',  ( 2.707414796094851361, 1.816601298730673220, -1.093838055662835096 ) ) ;
#144707 = CARTESIAN_POINT ( 'NONE',  ( -11.38508626655161216, 5.468933214068770532, 5.576081633246319669 ) ) ;
#144706 = CARTESIAN_POINT ( 'NONE',  ( -4.815081012084855061, 4.880956980543525781, 0.4525137542755679476 ) ) ;
#144708 = CARTESIAN_POINT ( 'NONE',  ( 4.428955518335824237, 0.09376622492938446740, 1.969227427985324352 ) ) ;
#144709 = CARTESIAN_POINT ( 'NONE',  ( 6.451426615364327155, -1.705040744490589066, 0.8662930942644477827 ) ) ;
#144710 = ORIENTED_EDGE ( 'NONE', *, *, #26563, .T. ) ;
#144711 =( LENGTH_UNIT ( ) NAMED_UNIT ( * ) SI_UNIT ( .MILLI., .METRE. ) );
#144712 = CARTESIAN_POINT ( 'NONE',  ( 0.8189040078958352842, -1.500748464528355974, 1.426492703164506937 ) ) ;
#144713 = CARTESIAN_POINT ( 'NONE',  ( 3.081904124835439074, -1.913310220277367080, -0.3314154666464886323 ) ) ;
#144714 = EDGE_LOOP ( 'NONE', ( #164797, #70159, #46191, #86335 ) ) ;
#144715 = CARTESIAN_POINT ( 'NONE',  ( -2.823841133396259639, 6.516508098929413961, -0.7998128361456481317 ) ) ;
#144716 = CARTESIAN_POINT ( 'NONE',  ( 6.607619761813720238, 8.802252036906432764, 1.599625672291268286 ) ) ;
#144718 = CARTESIAN_POINT ( 'NONE',  ( 4.645640190976921602, 8.571663989448405019, 1.040834085586084257E-14 ) ) ;
#144717 = CARTESIAN_POINT ( 'NONE',  ( 2.150438955405692631, -1.615297803084648098, 1.327229747913031055 ) ) ;
#144719 = CARTESIAN_POINT ( 'NONE',  ( 3.567203813726958828, 6.215469311773181182, 1.082531754730549078 ) ) ;
#144721 = ORIENTED_EDGE ( 'NONE', *, *, #173138, .T. ) ;
#144720 = CARTESIAN_POINT ( 'NONE',  ( 0.2404698186789978875, 1.732857435387507250, 0.5278947837941138088 ) ) ;
#144722 = CARTESIAN_POINT ( 'NONE',  ( 4.864015066594513215, 2.183220759563545776, -0.3215228633955333759 ) ) ;
#144723 = FACE_OUTER_BOUND ( 'NONE', #96509, .T. ) ;
#144724 = CARTESIAN_POINT ( 'NONE',  ( 3.645738483435243982, -1.669485028154977790, -1.443228448415982079 ) ) ;
#144725 = CARTESIAN_POINT ( 'NONE',  ( 7.151035956204054855, 10.43029348462504124, 1.199719254218460707 ) ) ;
#144726 = CYLINDRICAL_SURFACE ( 'NONE', #130996, 0.3999999999999997446 ) ;
#144727 = CARTESIAN_POINT ( 'NONE',  ( 2.209489775926488431, 1.479274643242427301, 1.211860329591994745 ) ) ;
#144728 = COLOUR_RGB ( '', 0.08235294, 0.09019608, 0.10196078) ;
#144729 = CARTESIAN_POINT ( 'NONE',  ( 9.582915646760733708, 10.07448976417602893, 0.7998128361456462443 ) ) ;
#144730 = CARTESIAN_POINT ( 'NONE',  ( 3.736834853878097107, -1.994506513866915576, -0.5549897870569252545 ) ) ;
#144732 = CARTESIAN_POINT ( 'NONE',  ( 3.256853613824191029, -1.637998819981079990, 1.410756932016984377 ) ) ;
#144731 = CARTESIAN_POINT ( 'NONE',  ( 0.7499999999999902300, 3.816666666666690411, -1.299038105676658228 ) ) ;
#144733 = CARTESIAN_POINT ( 'NONE',  ( 5.267185993530860699, 2.112242253262315739, -0.5839428218426812034 ) ) ;
#144734 = CARTESIAN_POINT ( 'NONE',  ( 0.000000000000000000, -1.500000000000001332, 0.000000000000000000 ) ) ;
#144735 = AXIS2_PLACEMENT_3D ( 'NONE', #18913, #100187, #199802 ) ;
#144736 = DIRECTION ( 'NONE',  ( -3.706092522800016599E-15, 0.000000000000000000, -1.000000000000000000 ) ) ;
#144737 = CARTESIAN_POINT ( 'NONE',  ( -0.4933182949323664523, 7.812106778933141982, 1.990607459109340560 ) ) ;
#144738 = EDGE_CURVE ( 'NONE', #193157, #174327, #2818, .T. ) ;
#144739 = CARTESIAN_POINT ( 'NONE',  ( 6.249382461256315580, 6.255644057745969988, -0.7998128361456481317 ) ) ;
#144740 = CARTESIAN_POINT ( 'NONE',  ( 1.642778471875001811, -2.530208332855374387, 2.845375778867859751 ) ) ;
#144741 = CARTESIAN_POINT ( 'NONE',  ( -3.156015896931072540, 6.904045323053366268, 0.000000000000000000 ) ) ;
#144742 = CARTESIAN_POINT ( 'NONE',  ( 0.6334356698059575574, 0.5880228326464317368, 1.928751028484784413 ) ) ;
#144743 = CARTESIAN_POINT ( 'NONE',  ( -8.920901888112002354, 11.43080484092926241, 1.443375672974064550 ) ) ;
#144744 = CARTESIAN_POINT ( 'NONE',  ( 6.412080304620304538, 6.445458208337293549, -0.7998128361456481317 ) ) ;
#144745 = CARTESIAN_POINT ( 'NONE',  ( 4.205968427668831389, 0.7022645179026367757, -1.947615878368731623 ) ) ;
#144746 = CARTESIAN_POINT ( 'NONE',  ( 3.141151230849213327, -1.698683669661217754, 0.9087857633808916757 ) ) ;
#144747 = CARTESIAN_POINT ( 'NONE',  ( 0.1402502066264778580, 0.7743353953559418690, 1.862009890338502505 ) ) ;
#144748 = CARTESIAN_POINT ( 'NONE',  ( 6.498435699651741615, 6.475929825882159818, -0.7998128361456281477 ) ) ;
#144749 = CARTESIAN_POINT ( 'NONE',  ( 0.6823417656249917140, 5.592708333674749177, 1.181850606188765695 ) ) ;
#144750 = CARTESIAN_POINT ( 'NONE',  ( 4.451979310445155491, -0.7576744193203123201, 1.818072383216073007 ) ) ;
#144751 = CARTESIAN_POINT ( 'NONE',  ( -0.02900071798685524560, -0.004641455105012376459, -2.173770343569726649 ) ) ;
#144752 = CARTESIAN_POINT ( 'NONE',  ( 4.477060521952030747, -0.002618581577289170060, -1.825872481161804561 ) ) ;
#144753 = EDGE_CURVE ( 'NONE', #40908, #202176, #108804, .T. ) ;
#144754 = CARTESIAN_POINT ( 'NONE',  ( 6.699137298928145690, 8.909022496873262753, 1.443375672974065660 ) ) ;
#144755 = CARTESIAN_POINT ( 'NONE',  ( 3.009546912109283934, 6.454962464195385330, 0.000000000000000000 ) ) ;
#144756 = CARTESIAN_POINT ( 'NONE',  ( -7.605197822622922210, 7.837428646007010613, -0.7998128361456362523 ) ) ;
#144757 = CARTESIAN_POINT ( 'NONE',  ( 4.193214648376505593, 8.114110533073061404, 0.000000000000000000 ) ) ;
#144758 = ORIENTED_EDGE ( 'NONE', *, *, #171547, .F. ) ;
#144760 = CARTESIAN_POINT ( 'NONE',  ( 4.886981372429439752, -1.897129443012405936, -0.6741400253723847102 ) ) ;
#144759 = CARTESIAN_POINT ( 'NONE',  ( 1.610644152589552958, -0.2245515952020246675, 1.827417025815617935 ) ) ;
#144761 = CARTESIAN_POINT ( 'NONE',  ( 0.3514386742532841779, -1.080868183629126067, 2.028406642177064345 ) ) ;
#144762 = CARTESIAN_POINT ( 'NONE',  ( 5.893401036868160858, -1.775023410133094615, 0.8355650083611900758 ) ) ;
#144763 = CARTESIAN_POINT ( 'NONE',  ( -7.369020184227459858, 8.555943955475521889, 1.199719254218450271 ) ) ;
#144764 = CARTESIAN_POINT ( 'NONE',  ( 0.2333690889706682703, 1.352610664630080839, -2.308230059406161772 ) ) ;
#144765 = CARTESIAN_POINT ( 'NONE',  ( -3.737243898861318137, 7.511868315313511069, 0.7998128361456341429 ) ) ;
#144766 = DIRECTION ( 'NONE',  ( -0.000000000000000000, -1.000000000000000000, -0.000000000000000000 ) ) ;
#144767 = CARTESIAN_POINT ( 'NONE',  ( -5.093022980588950865, 5.970890227889075419, -1.199719254218453823 ) ) ;
#144769 = CARTESIAN_POINT ( 'NONE',  ( 6.403183007056281184, 1.474056081383187555, 0.9792082336040304202 ) ) ;
#144768 = CARTESIAN_POINT ( 'NONE',  ( 1.277023361749257457, 1.930420895987930097, -0.8034254789068133729 ) ) ;
#144770 = CARTESIAN_POINT ( 'NONE',  ( -7.755938900619411491, -5.581885079358431589, 7.800371912476625091 ) ) ;
#144771 = CARTESIAN_POINT ( 'NONE',  ( -0.1104750535120251481, 6.947232870375212421, -2.698533382536407732 ) ) ;
#144772 = CARTESIAN_POINT ( 'NONE',  ( 0.8018505195637380956, 1.319035621562004934, -1.135522575981460003 ) ) ;
#144773 = AXIS2_PLACEMENT_3D ( 'NONE', #195749, #163254, #182672 ) ;
#144774 = CARTESIAN_POINT ( 'NONE',  ( 7.610204295972345712, 7.772993188256215547, 0.7998128361456341429 ) ) ;
#144776 = CARTESIAN_POINT ( 'NONE',  ( 0.6124999999999707345, 1.729166667349485431, -1.060881119635955327 ) ) ;
#144775 = DIRECTION ( 'NONE',  ( 0.000000000000000000, 1.000000000000000000, 0.000000000000000000 ) ) ;
#144777 = CARTESIAN_POINT ( 'NONE',  ( 1.998289267358617671, -0.4583927764671858474, -1.662768097037459869 ) ) ;
#144778 =( BOUNDED_SURFACE ( )  B_SPLINE_SURFACE ( 3, 2, ( 
 ( #212798, #49261, #196570 ),
 ( #184562, #181376, #149959 ),
 ( #33000, #99077, #2599 ),
 ( #165130, #455, #36183 ),
 ( #64436, #34056, #1528 ),
 ( #67592, #66523, #100129 ),
 ( #137976, #89234, #41555 ),
 ( #202937, #140127, #169395 ) ),
 .UNSPECIFIED., .F., .F., .F. ) 
 B_SPLINE_SURFACE_WITH_KNOTS ( ( 4, 2, 2, 4 ),
 ( 3, 3 ),
 ( 0.000000000000000000, 0.0002475938981900030044, 0.0004951877963800060088, 0.0009903755927600120176 ),
 ( 0.000000000000000000, 1.000000000000000000 ),
 .UNSPECIFIED. ) 
 GEOMETRIC_REPRESENTATION_ITEM ( )  RATIONAL_B_SPLINE_SURFACE ( (
 ( 1.000000000000000000, 0.9238795325112900692, 1.000000000000000000),
 ( 1.000000000000000000, 0.9248499699755210468, 1.000000000000000000),
 ( 1.000000000000000000, 0.9171047238581204741, 1.000000000000000000),
 ( 1.000000000000000000, 0.8907236462371719288, 1.000000000000000000),
 ( 1.000000000000000000, 0.8725411758595089662, 1.000000000000000000),
 ( 1.000000000000000000, 0.8105159241142131377, 1.000000000000000000),
 ( 1.000000000000000000, 0.7599483315141056794, 1.000000000000000000),
 ( 1.000000000000000000, 0.7045118851637689472, 1.000000000000000000) ) ) 
 REPRESENTATION_ITEM ( '' )  SURFACE ( )  );
#144779 = CARTESIAN_POINT ( 'NONE',  ( 1.769323484426460480, 2.095969018468134770, -0.6401429536977767398 ) ) ;
#144780 = CARTESIAN_POINT ( 'NONE',  ( 3.580891165198408110, -2.126768340858419926, -0.5889919780145411732 ) ) ;
#144781 = CARTESIAN_POINT ( 'NONE',  ( -9.587917471435847716, 4.026361754648488223, -6.670783315233271615 ) ) ;
#144782 = CARTESIAN_POINT ( 'NONE',  ( 1.182764167570474534, 1.294921473658101840, -1.742447618606123960 ) ) ;
#144783 = CARTESIAN_POINT ( 'NONE',  ( 0.4690313652776016418, 0.1822212253758948297, -1.816563760317004395 ) ) ;
#144784 = CARTESIAN_POINT ( 'NONE',  ( 2.870428589035282751, -2.086819620220676352, -0.3573068958101219827 ) ) ;
#144785 = CARTESIAN_POINT ( 'NONE',  ( 6.639320575229255006, 7.629137130509086262, 2.396737603865983779 ) ) ;
#144786 = ADVANCED_FACE ( 'NONE', ( #32548 ), #175964, .T. ) ;
#144787 = EDGE_LOOP ( 'NONE', ( #133532, #46022 ) ) ;
#144789 = CARTESIAN_POINT ( 'NONE',  ( -1.402160292154681736E-14, 0.5093750003414236893, -1.575800808251659024 ) ) ;
#144788 = CARTESIAN_POINT ( 'NONE',  ( 3.210744404368763405, 2.073164229931067304, 0.9784878017504093917 ) ) ;
#144790 = CARTESIAN_POINT ( 'NONE',  ( 0.07755575628181145265, 6.946778278137148099, -2.783982195446454533 ) ) ;
#144791 = CARTESIAN_POINT ( 'NONE',  ( 3.032219910950674890, 6.689340329417765574, 0.7998128361456321445 ) ) ;
#144792 = CARTESIAN_POINT ( 'NONE',  ( 5.901095752275416828, -0.3235219084677161128, -2.197517257070471075 ) ) ;
#144793 = CARTESIAN_POINT ( 'NONE',  ( -7.565086526745425033, 7.928281824065535055, 0.7216878364870317197 ) ) ;
#144794 = CARTESIAN_POINT ( 'NONE',  ( 5.843201017809841247, 5.919415396974013532, 1.040834085586084257E-14 ) ) ;
#144795 = CARTESIAN_POINT ( 'NONE',  ( -7.497295758232731089, 8.809561808435409702, -1.082531754730543083 ) ) ;
#144796 = CARTESIAN_POINT ( 'NONE',  ( 5.397554552016226914, 6.430140077841320689, 1.082531754730549078 ) ) ;
#144797 = ORIENTED_EDGE ( 'NONE', *, *, #200849, .F. ) ;
#144798 = CARTESIAN_POINT ( 'NONE',  ( 3.674454069786535548, 1.462445212485608437, 1.388486266691544957 ) ) ;
#144800 = CARTESIAN_POINT ( 'NONE',  ( 1.991156689281988745, 0.1981002678682428353, 2.053003549438499054 ) ) ;
#144799 = CARTESIAN_POINT ( 'NONE',  ( 5.341022448779654930, 8.318611059296550536, 1.199719254218462483 ) ) ;
#144801 = CYLINDRICAL_SURFACE ( 'NONE', #144155, 12.00000000000000178 ) ;
#144802 = ADVANCED_FACE ( 'NONE', ( #128049 ), #211979, .T. ) ;
#144803 = CARTESIAN_POINT ( 'NONE',  ( 5.356880090730872013, 6.382686539675070492, 1.082531754730549078 ) ) ;
#144804 = CARTESIAN_POINT ( 'NONE',  ( -9.609441814500819135, -6.583711573987011789, 0.3689019803512949558 ) ) ;
#144805 = CARTESIAN_POINT ( 'NONE',  ( -1.201851678989727383E-14, 4.696875000341419693, -1.575800808251660134 ) ) ;
#144806 = CARTESIAN_POINT ( 'NONE',  ( 5.156268285673103691, -1.588865937562380148, 1.509524371192130676 ) ) ;
#144807 = CARTESIAN_POINT ( 'NONE',  ( 2.127577483945505055, 0.4445034925110411539, 1.966644524931899563 ) ) ;
#144808 = CARTESIAN_POINT ( 'NONE',  ( 2.225889136967126536, 1.786374552192676823, 0.4457033907802817052 ) ) ;
#144809 = CARTESIAN_POINT ( 'NONE',  ( 5.947222937888848371, 10.09017719417900416, 1.040834085586084257E-14 ) ) ;
#144810 = CARTESIAN_POINT ( 'NONE',  ( 5.086841682847768276, -0.2248377094848166835, -1.811598703993194670 ) ) ;
#144811 = CARTESIAN_POINT ( 'NONE',  ( 6.539686446881147752, -1.556848207870220602, 1.281141925495055123 ) ) ;
#144812 = CARTESIAN_POINT ( 'NONE',  ( -8.213542131780492639, 8.476887330032372603, 1.040834085586084257E-14 ) ) ;
#144814 = CARTESIAN_POINT ( 'NONE',  ( -6.642568916052639771, 6.714361588341672515, 0.000000000000000000 ) ) ;
#144813 = CARTESIAN_POINT ( 'NONE',  ( 5.629810878523249684, -1.430378642458853378, -1.753011776973804725 ) ) ;
#144815 = CARTESIAN_POINT ( 'NONE',  ( 0.3464870678724129016, 2.100606130083045198, 0.1525024232564754778 ) ) ;
#144816 = CARTESIAN_POINT ( 'NONE',  ( -8.086512275908061653, 8.398962174839683215, 0.000000000000000000 ) ) ;
#144817 = CARTESIAN_POINT ( 'NONE',  ( 7.618792255875527886, 10.97600916757510170, 1.199719254218460707 ) ) ;
#144818 = CARTESIAN_POINT ( 'NONE',  ( 4.076122527140082497, 7.725281555510842502, -0.6205295181239127711 ) ) ;
#144819 = DIRECTION ( 'NONE',  ( 0.000000000000000000, 0.000000000000000000, 1.000000000000000000 ) ) ;
#144820 = CARTESIAN_POINT ( 'NONE',  ( -6.690058733339450114, 9.892486724616283311, 1.199719254218452047 ) ) ;
#144821 = UNCERTAINTY_MEASURE_WITH_UNIT (LENGTH_MEASURE( 1.000000000000000082E-05 ), #173998, 'distance_accuracy_value', 'NONE');
#144822 = CYLINDRICAL_SURFACE ( 'NONE', #33603, 1.224999999999996980 ) ;
#144823 = CARTESIAN_POINT ( 'NONE',  ( 7.876360894896227371, 8.153785563659219804, -0.7998128361456341429 ) ) ;
#144824 = CARTESIAN_POINT ( 'NONE',  ( 4.003607682157598546, 7.822813005323850710, -0.1595685970469905290 ) ) ;
#144825 = CARTESIAN_POINT ( 'NONE',  ( -10.15469386695561482, 10.94949038764413096, 1.040834085586084257E-14 ) ) ;
#144826 = CARTESIAN_POINT ( 'NONE',  ( 2.443850186789862100, -2.070980460497043651, 0.8039724962528942420 ) ) ;
#144827 = CARTESIAN_POINT ( 'NONE',  ( 3.234284411020655003, 6.422206199346979894, -0.8943276771341170939 ) ) ;
#144828 = CARTESIAN_POINT ( 'NONE',  ( -4.776215253764153346, 8.794277906025310898, -0.7998128361456362523 ) ) ;
#144829 = CARTESIAN_POINT ( 'NONE',  ( 6.449928391799196525, 8.548002428564306143, -1.599625672291262513 ) ) ;
#144830 = CARTESIAN_POINT ( 'NONE',  ( 3.736726379466179804, -1.890069333072645241, -0.5255722985574098338 ) ) ;
#144831 = CARTESIAN_POINT ( 'NONE',  ( 4.801558957534076022, 8.753569217098425170, 0.7998128361456462443 ) ) ;
#144832 = CARTESIAN_POINT ( 'NONE',  ( -4.160056744896282410, 7.428205994021240599, -0.7369721661574859528 ) ) ;
#144833 = CARTESIAN_POINT ( 'NONE',  ( 3.388648328411762556, 6.040841252200647382, 1.199719254218462483 ) ) ;
#144834 = CARTESIAN_POINT ( 'NONE',  ( -5.316205630334268406, 6.335233002545657577, -1.082531754730549967 ) ) ;
#144836 = VERTEX_POINT ( 'NONE', #113910 ) ;
#144835 = CARTESIAN_POINT ( 'NONE',  ( -6.805829924380121909, 8.963220883242035697, 1.443375672974078761 ) ) ;
#144837 =( BOUNDED_CURVE ( )  B_SPLINE_CURVE ( 2, ( #121451, #24914, #91018, #105136, #175461, #157080, #187421, #39051, #171176 ),
 .UNSPECIFIED., .F., .T. ) 
 B_SPLINE_CURVE_WITH_KNOTS ( ( 3, 2, 2, 2, 3 ),
 ( 0.4910714285714285476, 0.4940476190476190688, 0.5000000000000000000, 0.5059523809523809312, 0.5089285714285713969 ),
 .UNSPECIFIED. ) 
 CURVE ( )  GEOMETRIC_REPRESENTATION_ITEM ( )  RATIONAL_B_SPLINE_CURVE ( ( 0.9330127018922194093, 0.9330127018922187432, 1.000000000000000000, 0.8660254037844387076, 1.000000000000000000, 0.8660254037844387076, 1.000000000000000000, 0.9330127018922194093, 0.9330127018922194093 ) ) 
 REPRESENTATION_ITEM ( '' )  );
#144839 = CARTESIAN_POINT ( 'NONE',  ( 2.830460552442021438, -1.048868820301660953, -1.842999677239331113 ) ) ;
#144838 = TOROIDAL_SURFACE ( 'NONE', #179283, 0.1600000000000000033, 0.08000000000000000167 ) ;
#144840 = CARTESIAN_POINT ( 'NONE',  ( -4.125423880308188629, 8.035021303660014880, -0.7998128361456481317 ) ) ;
#144841 = CARTESIAN_POINT ( 'NONE',  ( 3.907220446582274853, 1.852832235905249370, 1.113321777468062823 ) ) ;
#144842 = CARTESIAN_POINT ( 'NONE',  ( 2.735704033801298340, 1.827604811068459734, 0.2230458208379028084 ) ) ;
#144843 = CARTESIAN_POINT ( 'NONE',  ( -5.250693970737303928, 6.428279158139240224, 1.158874695820178324 ) ) ;
#144844 = CARTESIAN_POINT ( 'NONE',  ( 0.6823417656249882723, 0.4885416670080827695, -1.181850606188749264 ) ) ;
#144845 = CARTESIAN_POINT ( 'NONE',  ( 5.736210779895188239, 0.3457693788900301768, 1.705448404129115580 ) ) ;
#144846 = CARTESIAN_POINT ( 'NONE',  ( 11.41381675112453564, 10.06994333910006567, -3.704697986577182522 ) ) ;
#144847 = CARTESIAN_POINT ( 'NONE',  ( 4.365362273920238678, 7.076377838673507448, 1.082531754730558626 ) ) ;
#144848 = CARTESIAN_POINT ( 'NONE',  ( 6.620655732516621761, 0.004685112605665223660, 1.926407831898163003 ) ) ;
#144849 = CARTESIAN_POINT ( 'NONE',  ( 3.221700144506876917, -2.083771231579465866, 0.5749860669421112958 ) ) ;
#144850 = CARTESIAN_POINT ( 'NONE',  ( 4.675157572021750418, -0.8594996001172333644, -1.823839583407538267 ) ) ;
#144851 = CARTESIAN_POINT ( 'NONE',  ( -8.717529583462656717, 11.19353715217169309, 1.443375672974064550 ) ) ;
#144852 = CARTESIAN_POINT ( 'NONE',  ( 2.747127081003514881, -1.797865629537301668, 1.199965651887124896 ) ) ;
#144853 = CARTESIAN_POINT ( 'NONE',  ( 3.497303454036035930, 1.552041748764835249, 1.215357900914854516 ) ) ;
#144854 = CARTESIAN_POINT ( 'NONE',  ( 4.669442277103274641, 1.121057080241712578, 1.585637770727834850 ) ) ;
#144857 = ORIENTED_EDGE ( 'NONE', *, *, #126259, .F. ) ;
#144856 = CARTESIAN_POINT ( 'NONE',  ( 8.081892667527538876, -5.200000000000006395, -7.462104991928523390 ) ) ;
#144855 = CARTESIAN_POINT ( 'NONE',  ( -7.470179451005382276, 11.65903375957422128, 0.7216878364870458196 ) ) ;
#144858 = CARTESIAN_POINT ( 'NONE',  ( -5.433785704026946384, 9.561443431331920095, 0.000000000000000000 ) ) ;
#144859 = CARTESIAN_POINT ( 'NONE',  ( 11.92051736251533534, 9.948197562073195499, 1.381800029228856808 ) ) ;
#144861 = VERTEX_POINT ( 'NONE', #176702 ) ;
#144860 = CARTESIAN_POINT ( 'NONE',  ( -4.359828915246279024, 7.244161613499399799, -1.199719254218455378 ) ) ;
#144862 = CARTESIAN_POINT ( 'NONE',  ( -7.144783764277399030, 11.27940545839156528, 0.7216878364870458196 ) ) ;
#144863 = CARTESIAN_POINT ( 'NONE',  ( 0.6224627697807674220, -1.182292326766160251, -1.863150505713019989 ) ) ;
#144864 = CARTESIAN_POINT ( 'NONE',  ( 1.642778471875000035, -1.276041666188710400, -2.845375778867859751 ) ) ;
#144865 = CARTESIAN_POINT ( 'NONE',  ( 6.526224699197019419, 1.005635830909179074, 1.684226478273798788 ) ) ;
#144866 = CARTESIAN_POINT ( 'NONE',  ( -0.7500000000000006661, 8.958333333333332149, -1.299038105676657340 ) ) ;
#144867 = CARTESIAN_POINT ( 'NONE',  ( 0.7499999999999902300, 4.597916667349482012, -1.299038105676658228 ) ) ;
#144868 = CARTESIAN_POINT ( 'NONE',  ( 5.531458889030211878, 6.400359360821498811, -1.228567739025695493 ) ) ;
#144869 = CARTESIAN_POINT ( 'NONE',  ( 0.07499057489262526965, 5.723988098492513998, -2.549530206576706259 ) ) ;
#144870 = CARTESIAN_POINT ( 'NONE',  ( 5.261588992693945421, 0.9106475924270783784, 1.600083007495013643 ) ) ;
#144871 = ORIENTED_EDGE ( 'NONE', *, *, #105563, .F. ) ;
#144872 = CARTESIAN_POINT ( 'NONE',  ( 0.6801582343749865700, -1.026041666325229418, 1.178068619123805227 ) ) ;
#144873 = CARTESIAN_POINT ( 'NONE',  ( -8.532158741701643123, 8.848606708273724308, 0.7998128361456462443 ) ) ;
#144874 = CARTESIAN_POINT ( 'NONE',  ( 7.451274665340240411, -7.616254850791388975, -6.794158526849247259 ) ) ;
#144876 = ADVANCED_FACE ( 'NONE', ( #98654 ), #164710, .T. ) ;
#144875 = CARTESIAN_POINT ( 'NONE',  ( 6.363548717301088509, -1.704009271243651868, -1.262090224194649446 ) ) ;
#144877 = CARTESIAN_POINT ( 'NONE',  ( -2.393960638069832836, -0.2282907053230411043, -0.4203461706283347921 ) ) ;
#144878 = CARTESIAN_POINT ( 'NONE',  ( 5.684946482831785275, 5.526859072925533134, -0.7998128361456231517 ) ) ;
#144879 = CARTESIAN_POINT ( 'NONE',  ( 6.485628570817172367, 1.417799985879987901, 1.495801911481582813 ) ) ;
#144882 = CARTESIAN_POINT ( 'NONE',  ( 3.157574601152390414, 0.8305207305269333151, 1.643389852989694200 ) ) ;
#144881 = CARTESIAN_POINT ( 'NONE',  ( 2.119380567849386665, 0.3219547178687692801, -1.832826937841147252 ) ) ;
#144880 = SURFACE_STYLE_USAGE ( .BOTH. , #78756 ) ;
#144883 = CARTESIAN_POINT ( 'NONE',  ( 7.690499447449630210, 9.995335326823163058, 1.599625672291281386 ) ) ;
#144884 = SURFACE_STYLE_FILL_AREA ( #78760 ) ;
#144885 = CARTESIAN_POINT ( 'NONE',  ( -7.130662446144611977, 7.283804040115648526, 0.000000000000000000 ) ) ;
#144886 = PLANE ( 'NONE',  #36010 ) ;
#144887 = CARTESIAN_POINT ( 'NONE',  ( 3.528125218122651230, -1.314342534882004809, -1.772652456903674567 ) ) ;
#144888 = CARTESIAN_POINT ( 'NONE',  ( 5.923173471921922228, -0.06425113298673529316, 2.261675518886300473 ) ) ;
#144889 = CARTESIAN_POINT ( 'NONE',  ( -5.585596099150182958, 8.499983968108443477, -1.082531754730544860 ) ) ;
#144890 = CARTESIAN_POINT ( 'NONE',  ( 5.291193953664572902, -0.05252268709225348109, -1.811016617013387009 ) ) ;
#144891 = CARTESIAN_POINT ( 'NONE',  ( -0.1355283706049141557, -1.957205112593700003, -0.4852584411360050254 ) ) ;
#144892 = CARTESIAN_POINT ( 'NONE',  ( -4.475070042639309520, 5.445751865460756846, 1.284222742053057642 ) ) ;
#144893 = CARTESIAN_POINT ( 'NONE',  ( 6.702024585102262400, -1.870183347854617040, 0.04844413084104796929 ) ) ;
#144894 = CARTESIAN_POINT ( 'NONE',  ( -7.334597915313094241, 9.580116872663850813, 1.040834085586084257E-14 ) ) ;
#144895 = CARTESIAN_POINT ( 'NONE',  ( 6.737169288263022082, -1.578518636041785994, 0.8004799088773879578 ) ) ;
#144896 = CARTESIAN_POINT ( 'NONE',  ( 1.481658059775035952, -0.6748446255696785023, 1.900416712880992343 ) ) ;
#144898 = CARTESIAN_POINT ( 'NONE',  ( 2.526118869349633034, -1.213293402057673775, -1.721263080769465992 ) ) ;
#144897 = CARTESIAN_POINT ( 'NONE',  ( -7.967387826325084355, 12.44703623068796361, 0.7998128361456481317 ) ) ;
#144899 = CARTESIAN_POINT ( 'NONE',  ( 7.587759525142423911, 12.00413654597487501, 0.7998128361456462443 ) ) ;
#144901 = CARTESIAN_POINT ( 'NONE',  ( -7.994504133552415404, 12.47867192245318435, -0.7998128361456281477 ) ) ;
#144900 = CARTESIAN_POINT ( 'NONE',  ( 1.499999999999987566, -0.9749999999999827693, 0.000000000000000000 ) ) ;
#144902 = CARTESIAN_POINT ( 'NONE',  ( 11.35569630219391968, 9.987315607086321378, 3.554478010595061743 ) ) ;
#144903 = CARTESIAN_POINT ( 'NONE',  ( 2.566670905829854021, 0.6845714803544473703, 1.900350667086497580 ) ) ;
#144904 = CARTESIAN_POINT ( 'NONE',  ( 1.364683531249988535, 2.863541667008082658, 0.7879004041258500513 ) ) ;
#144905 = EDGE_CURVE ( 'NONE', #140322, #62112, #130571, .T. ) ;
#144906 = CARTESIAN_POINT ( 'NONE',  ( 8.581948047770334043, 12.95609712246668899, 0.000000000000000000 ) ) ;
#144907 = CARTESIAN_POINT ( 'NONE',  ( 3.515052679271633895, 1.952536648612019921, 0.9277410485990513767 ) ) ;
#144908 = CARTESIAN_POINT ( 'NONE',  ( 1.441120163477462413, 8.287694259231834337, -3.161243217722550458 ) ) ;
#144910 = DIRECTION ( 'NONE',  ( 0.000000000000000000, -1.000000000000000000, 0.000000000000000000 ) ) ;
#144909 = CARTESIAN_POINT ( 'NONE',  ( 5.830888582329017744, 8.960397891762626799, -1.199719254218452047 ) ) ;
#144911 = CARTESIAN_POINT ( 'NONE',  ( 7.714226216051361718, 11.94375498546120795, -0.7216878364870267237 ) ) ;
#144913 = CARTESIAN_POINT ( 'NONE',  ( 7.221524917713163738, 15.51845925282233196, -9.590549216876459226 ) ) ;
#144912 = CARTESIAN_POINT ( 'NONE',  ( 0.2917819264270337110, -1.984717812412156501, 0.8806528889930710369 ) ) ;
#144914 = CARTESIAN_POINT ( 'NONE',  ( -7.226132686403777150, 7.532835677000276675, 1.040834085586084257E-14 ) ) ;
#144915 = CARTESIAN_POINT ( 'NONE',  ( 0.6823417656249882723, 1.176041667008083325, -1.181850606188749264 ) ) ;
#144916 = CARTESIAN_POINT ( 'NONE',  ( 2.156058135970494227, 0.9403143569667195001, 1.979733194660021622 ) ) ;
#144917 = CARTESIAN_POINT ( 'NONE',  ( -0.03889815725003768071, -8.115420858948564131, 10.94377971103912195 ) ) ;
#144918 = CARTESIAN_POINT ( 'NONE',  ( 2.448426410784361185, 2.261989705503023806, 0.05584468559862928311 ) ) ;
#144919 = CARTESIAN_POINT ( 'NONE',  ( -7.507464373665155399, 9.781794407407920389, 1.599625672291295375 ) ) ;
#144920 = CARTESIAN_POINT ( 'NONE',  ( -2.928197990427299668, 6.360055388899728435, 1.040834085586084257E-14 ) ) ;
#144922 = AXIS2_PLACEMENT_3D ( 'NONE', #95580, #80363, #143275 ) ;
#144921 = CARTESIAN_POINT ( 'NONE',  ( 0.6823417656249899377, 2.905208333674754062, 1.181850606188765695 ) ) ;
#144923 = CARTESIAN_POINT ( 'NONE',  ( 5.840936731490688594, 7.196517624969346549, 1.161314407385056313 ) ) ;
#144924 = CARTESIAN_POINT ( 'NONE',  ( -0.7500000000000179856, 12.54166666666666607, 1.299038105676658228 ) ) ;
#144925 = CARTESIAN_POINT ( 'NONE',  ( 6.617788377246179188, 8.814115421577600529, -1.443375672974078761 ) ) ;
#144926 = CARTESIAN_POINT ( 'NONE',  ( 3.866244329565728943, -1.190307266767919536, 1.309773914726497734 ) ) ;
#144927 = CARTESIAN_POINT ( 'NONE',  ( 8.561083932025322696, 12.07534945641652158, -1.199719254218446718 ) ) ;
#144928 = CARTESIAN_POINT ( 'NONE',  ( 0.2355646933672841947, -1.925288835042149760, 0.8538303211676525617 ) ) ;
#144929 = CARTESIAN_POINT ( 'NONE',  ( -0.6823417656250003738, 9.901041667008065872, 1.181850606188754593 ) ) ;
#144930 = AXIS2_PLACEMENT_3D ( 'NONE', #96470, #162519, #47714 ) ;
#144931 = CARTESIAN_POINT ( 'NONE',  ( -6.296835998904160014, 6.311006518335105397, 0.000000000000000000 ) ) ;
#144932 = CARTESIAN_POINT ( 'NONE',  ( 6.099232498865051255, -0.2440123228986730841, 2.001514574626765075 ) ) ;
#144933 = ORIENTED_EDGE ( 'NONE', *, *, #29125, .T. ) ;
#144934 = ADVANCED_FACE ( 'NONE', ( #195084 ), #68144, .T. ) ;
#144935 = CARTESIAN_POINT ( 'NONE',  ( 8.452618703115982512, 11.94880668935564216, 1.199719254218450271 ) ) ;
#144936 = CARTESIAN_POINT ( 'NONE',  ( 4.082764389539480732, -0.1829629792115642917, -1.861669828791753467 ) ) ;
#144937 = CARTESIAN_POINT ( 'NONE',  ( 3.573154620739454668, 1.869565233029608420, 0.8895530118792621677 ) ) ;
#144938 = CARTESIAN_POINT ( 'NONE',  ( -5.275531169048895741, 9.168887107283438809, -0.7216878364870338292 ) ) ;
#144939 = DIRECTION ( 'NONE',  ( 0.7592566023653005702, 0.6507913734559639396, 0.000000000000000000 ) ) ;
#144940 = CARTESIAN_POINT ( 'NONE',  ( 6.157120911006637165, -1.851533521339579380, -1.115484332758958974 ) ) ;
#144941 = CARTESIAN_POINT ( 'NONE',  ( -1.201851678989727383E-14, 5.009375000341421469, -1.575800808251660134 ) ) ;
#144942 = CARTESIAN_POINT ( 'NONE',  ( 3.279693232472491893, -1.891448704997201302, 0.5207070127687256633 ) ) ;
#144943 = CARTESIAN_POINT ( 'NONE',  ( 0.6321852052597470850, 0.2004073784105386835, -2.006138679842318862 ) ) ;
#144944 = CARTESIAN_POINT ( 'NONE',  ( -5.171509248969888617, 4.998125310078441075, 0.7998128361456281477 ) ) ;
#144946 = CARTESIAN_POINT ( 'NONE',  ( -11.41157692552970460, 12.34089662912998620, 3.404533818002359435 ) ) ;
#144945 = CARTESIAN_POINT ( 'NONE',  ( 7.262363838414439776, 11.62450824479221900, 0.7998128361456462443 ) ) ;
#144947 = CARTESIAN_POINT ( 'NONE',  ( 0.7197278698120103124, -0.9953326032119573785, -1.583558375183778288 ) ) ;
#144948 = CARTESIAN_POINT ( 'NONE',  ( 0.6823417656249917140, 3.842708333674754506, 1.181850606188765695 ) ) ;
#144949 = CARTESIAN_POINT ( 'NONE',  ( 2.689700119490782360, 1.910346015757229177, -0.6353908363993918673 ) ) ;
#144951 = CARTESIAN_POINT ( 'NONE',  ( 2.161849840330143824, 1.305120488479810659, 1.667033946717882742 ) ) ;
#144950 = CARTESIAN_POINT ( 'NONE',  ( -4.934804725694212912, 8.701096580044490381, -0.7216878364870207285 ) ) ;
#144952 = CARTESIAN_POINT ( 'NONE',  ( 9.022614842422171932, 12.34770622016754515, -7.914810590312522542 ) ) ;
#144953 = CARTESIAN_POINT ( 'NONE',  ( 3.982925052038261526, 1.964963782255540359, 0.6523228965355857278 ) ) ;
#144954 = CARTESIAN_POINT ( 'NONE',  ( 7.991605200612358573, 8.288237253661408843, 0.7998128361456281477 ) ) ;
#144956 = CARTESIAN_POINT ( 'NONE',  ( 4.162516854595432747, 4.815023404238158555, 1.199719254218464037 ) ) ;
#144955 = CARTESIAN_POINT ( 'NONE',  ( 6.562449924160270065, -1.910870307864566575, -0.8485530564429457634 ) ) ;
#144958 = ORIENTED_EDGE ( 'NONE', *, *, #93445, .T. ) ;
#144957 = CARTESIAN_POINT ( 'NONE',  ( 4.928627555176230857, 1.747287423663802075, 0.5288322122747670662 ) ) ;
#144959 = CARTESIAN_POINT ( 'NONE',  ( 8.911787042884274257, 9.291506392986812912, 0.7998128361456462443 ) ) ;
#144960 = CARTESIAN_POINT ( 'NONE',  ( 7.720982910012531342, -6.306565840633542308, -7.834948813061516582 ) ) ;
#144961 = CARTESIAN_POINT ( 'NONE',  ( 10.14963603790778812, 13.57268984379813936, -7.272210095438468080 ) ) ;
#144962 = CARTESIAN_POINT ( 'NONE',  ( 6.633804142636003931, -1.436369002829580133, -1.675418478561958802 ) ) ;
#144963 = CARTESIAN_POINT ( 'NONE',  ( 0.6823417656249969321, 10.83854166700806765, -1.181850606188757036 ) ) ;
#144964 = CARTESIAN_POINT ( 'NONE',  ( 5.268181577278353345, 1.909906527651853425, -0.09793718704654422180 ) ) ;
#144965 = CARTESIAN_POINT ( 'NONE',  ( -10.48453286206953727, 11.12637651536962125, 0.7998128361456462443 ) ) ;
#144966 = CARTESIAN_POINT ( 'NONE',  ( 7.318703993278529829, 7.432909501780090800, 1.040834085586084257E-14 ) ) ;
#144967 = CARTESIAN_POINT ( 'NONE',  ( -2.353626204688216217E-14, 0.9843750003414547534, 1.570758158831764062 ) ) ;
#144968 = DIRECTION ( 'NONE',  ( -0.8271092603133229915, -0.5620411653108230432, -0.000000000000000000 ) ) ;
#144969 = EDGE_CURVE ( 'NONE', #45585, #16624, #94411, .T. ) ;
#144970 = CARTESIAN_POINT ( 'NONE',  ( 4.792970997630896512, 5.550553237779539018, 1.199719254218464037 ) ) ;
#144971 = EDGE_LOOP ( 'NONE', ( #203721, #82386, #176542, #108307, #39762, #44590, #163446, #1029, #125119, #140172, #21178 ) ) ;
#144972 = DIRECTION ( 'NONE',  ( 0.000000000000000000, 0.000000000000000000, -1.000000000000000000 ) ) ;
#144973 = EDGE_CURVE ( 'NONE', #180747, #58680, #97603, .T. ) ;
#144974 = CARTESIAN_POINT ( 'NONE',  ( 4.499188554602613799, 1.501106652244098116, 1.115835331622745841 ) ) ;
#144975 = CARTESIAN_POINT ( 'NONE',  ( 0.07680821025396293578, 0.7488618828427398011, -1.895266105024134839 ) ) ;
#144976 = CARTESIAN_POINT ( 'NONE',  ( 7.340813827156391191, 7.528980651296110160, 0.7998128361456281477 ) ) ;
#144977 = CARTESIAN_POINT ( 'NONE',  ( -11.07790593930098311, 13.79999999999999893, -0.7000000000000009548 ) ) ;
#144978 = AXIS2_PLACEMENT_3D ( 'NONE', #175878, #92510, #41616 ) ;
#144979 = CARTESIAN_POINT ( 'NONE',  ( -6.286530415420750195, 6.898050863092263896, 0.7571273896394186131 ) ) ;
#144980 = CARTESIAN_POINT ( 'NONE',  ( -6.073689629242165822, 7.148687991279732756, -1.082531754730544860 ) ) ;
#144981 = CARTESIAN_POINT ( 'NONE',  ( 4.792970997630896512, 5.550553237779539018, 1.199719254218464037 ) ) ;
#144982 = CARTESIAN_POINT ( 'NONE',  ( 1.305442304231837714, -1.549127766076626056, -1.215949579239549161 ) ) ;
#144983 = CARTESIAN_POINT ( 'NONE',  ( 2.935172905452135161, -1.650095542580119812, -1.158671029019647358 ) ) ;
#144984 = CARTESIAN_POINT ( 'NONE',  ( -7.751511138711140170, 10.06651563329490529, -1.599625672291263179 ) ) ;
#144985 = CARTESIAN_POINT ( 'NONE',  ( 4.044074958626150185, 7.940114228364351767, 0.7998128361456271485 ) ) ;
#144986 = FILL_AREA_STYLE_COLOUR ( '', #132326 ) ;
#144987 = CARTESIAN_POINT ( 'NONE',  ( 4.084055714405177895, -2.167483682527316713, -0.3223708474724209516 ) ) ;
#144988 = CARTESIAN_POINT ( 'NONE',  ( 9.601861804102849618, 3.883750271632767870, -7.121441872635297266 ) ) ;
#144989 = CARTESIAN_POINT ( 'NONE',  ( 2.028227463090884974, 1.110962183858194452, -1.573585318204050676 ) ) ;
#144990 = CARTESIAN_POINT ( 'NONE',  ( -8.123306592882240551, 12.62894145833798376, 0.000000000000000000 ) ) ;
#144991 = CARTESIAN_POINT ( 'NONE',  ( 0.9486429539237137831, 3.100839070649073381, 1.028101543438981080 ) ) ;
#144992 = CARTESIAN_POINT ( 'NONE',  ( 0.1331565106231363538, 7.629137130509071163, -2.545925718843544239 ) ) ;
#144993 = EDGE_CURVE ( 'NONE', #55379, #160775, #127177, .T. ) ;
#144994 = CARTESIAN_POINT ( 'NONE',  ( 5.072158865288245444, 5.090142562357324429, 0.7216878364870338292 ) ) ;
#144995 = CARTESIAN_POINT ( 'NONE',  ( 8.392660782059197189, 9.750191319612612872, 1.199719254218462483 ) ) ;
#144996 = CARTESIAN_POINT ( 'NONE',  ( 4.801558957534076022, 8.753569217098425170, 0.7998128361456462443 ) ) ;
#144997 = CARTESIAN_POINT ( 'NONE',  ( -9.508795732819944391, 15.08621132298791423, 7.212928819065541397 ) ) ;
#144998 = CARTESIAN_POINT ( 'NONE',  ( 6.224601922449876312, 6.434659462379210382, 0.000000000000000000 ) ) ;
#144999 = ORIENTED_EDGE ( 'NONE', *, *, #102377, .F. ) ;
#145001 = CARTESIAN_POINT ( 'NONE',  ( 1.559240971068908355, -1.699445492770943478, 1.078823074066703747 ) ) ;
#145000 = CARTESIAN_POINT ( 'NONE',  ( 4.493604616018744835, -1.840970053361364656, -0.04044509776383875543 ) ) ;
#145002 = CARTESIAN_POINT ( 'NONE',  ( 3.796502476701520301, -2.125173906124724343, 0.8757568767029444423 ) ) ;
#145004 = CARTESIAN_POINT ( 'NONE',  ( 2.606119654932341767, 1.860434991719280173, 0.05107381154999082046 ) ) ;
#145003 = CARTESIAN_POINT ( 'NONE',  ( -0.02900071798682749002, 0.2267074960015900975, -2.207170277039482986 ) ) ;
#145005 = CARTESIAN_POINT ( 'NONE',  ( -3.285556943749998737, -1.830208332855373987, 1.896917185911908499 ) ) ;
#145006 = DIRECTION ( 'NONE',  ( 0.000000000000000000, 0.000000000000000000, -1.000000000000000000 ) ) ;
#145007 = CARTESIAN_POINT ( 'NONE',  ( 5.467032840998240495, -1.503656711810175350, 1.181500457595338505 ) ) ;
#145008 = CARTESIAN_POINT ( 'NONE',  ( -7.100719765255177229, 9.307259030929609267, -1.599625672291263179 ) ) ;
#145009 = CARTESIAN_POINT ( 'NONE',  ( -6.292392690518214593, 7.474117906093608710, -1.082531754730549967 ) ) ;
#145011 = CARTESIAN_POINT ( 'NONE',  ( 3.889402362484274622, 1.354500474538382626, 1.290456140434749654 ) ) ;
#145010 = CARTESIAN_POINT ( 'NONE',  ( 4.581631739359020017, -0.9839878911236143999, 1.844693108308750551 ) ) ;
#145012 = CARTESIAN_POINT ( 'NONE',  ( 6.480434237652124452, 8.583592582059388576, 1.443375672974076540 ) ) ;
#145013 = CIRCLE ( 'NONE', #55151, 11.89429233241351902 ) ;
#145014 = CARTESIAN_POINT ( 'NONE',  ( 5.553597010146855695, 5.912075037831448832, 0.6282849591137803502 ) ) ;
#145015 = DIRECTION ( 'NONE',  ( -5.578564026256490882E-16, -1.000000000000000000, -9.066213480720158442E-32 ) ) ;
#145016 = CARTESIAN_POINT ( 'NONE',  ( 5.549328304323321248, -1.363462989569711681, -1.056374310239334591 ) ) ;
#145017 = CARTESIAN_POINT ( 'NONE',  ( -5.738125327081750271, 7.717565519727259904, 1.599625672291269396 ) ) ;
#145018 = CARTESIAN_POINT ( 'NONE',  ( 0.6856605700745866949, 1.416429869936095542, 1.000165270844357801 ) ) ;
#145019 = CARTESIAN_POINT ( 'NONE',  ( -1.436838838544753694, 7.449283400311743186, 4.203727439823589762 ) ) ;
#145020 = CARTESIAN_POINT ( 'NONE',  ( 1.899436509991797584, 3.291494839451057253, 0.4074537448169641696 ) ) ;
#145021 = LINE ( 'NONE', #129883, #124426 ) ;
#145022 = CARTESIAN_POINT ( 'NONE',  ( 5.506739464099510428, 0.6230791789904217559, 2.079776831526482628 ) ) ;
#145023 = CARTESIAN_POINT ( 'NONE',  ( 4.582524934692378871, -1.771534430979417429, -0.4408631061849078714 ) ) ;
#145024 = CARTESIAN_POINT ( 'NONE',  ( 1.147228161472005681, 1.732707765124143817, -0.9198407203683529598 ) ) ;
#145025 = CARTESIAN_POINT ( 'NONE',  ( 0.4216853220532343904, -1.500587716210170841, -1.493872543894637417 ) ) ;
#145026 = CARTESIAN_POINT ( 'NONE',  ( -1.201851678989727383E-14, 4.134375000341417028, 1.575800808251672791 ) ) ;
#145027 = CARTESIAN_POINT ( 'NONE',  ( 3.334942598837264960, 6.834590765378040444, 1.214306433183764966E-14 ) ) ;
#145028 = CARTESIAN_POINT ( 'NONE',  ( 8.776205506747620788, 9.133327934160710981, -0.7998128361456221525 ) ) ;
#145029 = CARTESIAN_POINT ( 'NONE',  ( 2.297662419472700002, 1.937625723843895864, -0.8618613456389671024 ) ) ;
#145030 = CARTESIAN_POINT ( 'NONE',  ( -4.785665035943912571, 4.685623418130398399, 1.214306433183764966E-14 ) ) ;
#145031 = VECTOR ( 'NONE', #34590, 1000.000000000000114 ) ;
#145032 = CARTESIAN_POINT ( 'NONE',  ( 3.715983187065167392, 7.557340494876523707, 0.6407673408501418644 ) ) ;
#145033 = CARTESIAN_POINT ( 'NONE',  ( -3.592547517496929466, 7.135129837147637488, -0.7216878364870257245 ) ) ;
#145034 = CARTESIAN_POINT ( 'NONE',  ( 0.6376584384039893916, 1.932990051301992418, -0.7417924570976216492 ) ) ;
#145036 = CARTESIAN_POINT ( 'NONE',  ( -1.500000000000015099, 13.76041666734946212, -0.8660254037844309360 ) ) ;
#145035 = CARTESIAN_POINT ( 'NONE',  ( 6.983263157960362122, 2.430545403621493072, 2.435370848939223620 ) ) ;
#145038 = ORIENTED_EDGE ( 'NONE', *, *, #55232, .T. ) ;
#145037 = CARTESIAN_POINT ( 'NONE',  ( 2.227449089350467482, 1.985603210742479252, 0.9958825451741261103 ) ) ;
#145039 = CARTESIAN_POINT ( 'NONE',  ( 0.4933721672778153544, -2.286813510910344682, 0.2336738355162761571 ) ) ;
#145041 = CARTESIAN_POINT ( 'NONE',  ( 5.348506707712929575, -2.046340616697607473, -0.2579891923277094490 ) ) ;
#145040 = CARTESIAN_POINT ( 'NONE',  ( 2.496672843210871129, 6.064535417054653266, -0.7998128361456291469 ) ) ;
#145043 = CARTESIAN_POINT ( 'NONE',  ( -1.737499999999997824, -1.691666666666667762, 3.009438278150925683 ) ) ;
#145042 = CARTESIAN_POINT ( 'NONE',  ( 4.518610335104485287, 8.493738834255713854, 0.000000000000000000 ) ) ;
#145044 = EDGE_CURVE ( 'NONE', #47756, #69090, #144255, .T. ) ;
#145045 = CARTESIAN_POINT ( 'NONE',  ( 6.496291879603339758, 7.608037276739255006, 1.199719254218452935 ) ) ;
#145046 = CARTESIAN_POINT ( 'NONE',  ( 0.1333542156527660338, 2.021264325465597977, -2.461897275464264290 ) ) ;
#145047 = CARTESIAN_POINT ( 'NONE',  ( 5.935073298327618652, -1.338256116417003927, -1.264887592264056559 ) ) ;
#145048 = EDGE_CURVE ( 'NONE', #211691, #170783, #159498, .T. ) ;
#145049 = CARTESIAN_POINT ( 'NONE',  ( 3.785751206713845018, 5.439795712631356750, 1.599625672291267398 ) ) ;
#145050 =( NAMED_UNIT ( * ) PLANE_ANGLE_UNIT ( ) SI_UNIT ( $, .RADIAN. ) );
#145051 = CARTESIAN_POINT ( 'NONE',  ( 1.658790106635851469, -1.476843439067159425, -0.8906862264850596844 ) ) ;
#145052 = CARTESIAN_POINT ( 'NONE',  ( 1.077361674225948418, 1.530160568918725872, 1.313541346884480987 ) ) ;
#145053 = CARTESIAN_POINT ( 'NONE',  ( -1.001543065824772872E-14, 4.634375000341418804, 1.575800808251672791 ) ) ;
#145054 = CARTESIAN_POINT ( 'NONE',  ( 2.232027051843707532, -1.476457111770380415, -1.714336117487671007 ) ) ;
#145055 = CARTESIAN_POINT ( 'NONE',  ( 4.037795408393930252, -1.452196710024173276, -1.525570609991099502 ) ) ;
#145056 = CARTESIAN_POINT ( 'NONE',  ( -2.823841133396259639, 6.516508098929413961, -0.7998128361456481317 ) ) ;
#145057 = CARTESIAN_POINT ( 'NONE',  ( 2.688433849602299031, -0.2980574676569973658, -1.744271549386553932 ) ) ;
#145058 = CARTESIAN_POINT ( 'NONE',  ( 5.931855901178834323, 6.879252291918818152, 1.199719254218462483 ) ) ;
#145060 = CARTESIAN_POINT ( 'NONE',  ( 6.515150198369638268, -2.224820657066893137, 0.5519656782505685255 ) ) ;
#145059 = CARTESIAN_POINT ( 'NONE',  ( 5.546694241322223107, 5.643767167730274537, -0.7216878364870458196 ) ) ;
#145061 = CARTESIAN_POINT ( 'NONE',  ( 4.224425198852012286, 0.09258891237720960621, 1.838934309869838968 ) ) ;
#145062 = CARTESIAN_POINT ( 'NONE',  ( -5.596818484342970912, 5.424043074688562172, -0.7998128361456221525 ) ) ;
#145063 = VECTOR ( 'NONE', #194649, 1000.000000000000000 ) ;
#145064 = UNCERTAINTY_MEASURE_WITH_UNIT (LENGTH_MEASURE( 1.000000000000000082E-05 ), #120361, 'distance_accuracy_value', 'NONE');
#145065 = CARTESIAN_POINT ( 'NONE',  ( 3.985733972293228344, 7.593847367743336463, 1.040834085586084257E-14 ) ) ;
#145066 = CARTESIAN_POINT ( 'NONE',  ( 1.499999999999989120, 3.275000000000020783, 1.214306433183764966E-14 ) ) ;
#145067 = CARTESIAN_POINT ( 'NONE',  ( 4.664136352776428573, -1.432711980460563250, 1.658340198327029613 ) ) ;
#145068 = CARTESIAN_POINT ( 'NONE',  ( -4.623494077460110319, 5.352830164246910272, 1.199719254218462483 ) ) ;
#145069 = CARTESIAN_POINT ( 'NONE',  ( 0.4444767461200390124, 7.387363020590400176, -2.040826832792550505 ) ) ;
#145070 = CARTESIAN_POINT ( 'NONE',  ( -3.421885780383957520, -0.03116325934363972996, -0.1958776937478875768 ) ) ;
#145071 = CARTESIAN_POINT ( 'NONE',  ( -1.001543065824772872E-14, 4.571875000341418804, 1.575800808251672791 ) ) ;
#145072 = CARTESIAN_POINT ( 'NONE',  ( 2.772000617051553206, 1.030904977978854609, 1.627292194166103600 ) ) ;
#145073 = CARTESIAN_POINT ( 'NONE',  ( -1.364683531250000748, 9.359375000341396245, 0.000000000000000000 ) ) ;
#145074 = CARTESIAN_POINT ( 'NONE',  ( -4.039966587192274083, 5.736380323189513852, 1.443375672974064550 ) ) ;
#145075 = CARTESIAN_POINT ( 'NONE',  ( -0.1575499713504755483, -1.374138184231291415, -1.746309953600865716 ) ) ;
#145076 = CARTESIAN_POINT ( 'NONE',  ( -4.800995793014949165, 8.615262501910491366, 0.7216878364870267237 ) ) ;
#145077 = VERTEX_POINT ( 'NONE', #152722 ) ;
#145079 = CARTESIAN_POINT ( 'NONE',  ( 4.271254376947781317, 7.121149023813882373, 1.207541395772090187 ) ) ;
#145078 = CARTESIAN_POINT ( 'NONE',  ( -4.502716413514310290, 6.346531463890372926, -1.443375672974066548 ) ) ;
#145080 = CARTESIAN_POINT ( 'NONE',  ( 5.705283713252285338, 5.550585841749444249, -0.7998128361456211532 ) ) ;
#145081 = DIRECTION ( 'NONE',  ( 0.000000000000000000, 1.000000000000000000, 0.000000000000000000 ) ) ;
#145082 = CARTESIAN_POINT ( 'NONE',  ( -2.335253425310764186, 0.1017894593877472081, -0.4879271257269361395 ) ) ;
#145083 = CARTESIAN_POINT ( 'NONE',  ( 11.48788097203293823, 13.83043054397688287, 3.469500700354829714 ) ) ;
#145084 = CARTESIAN_POINT ( 'NONE',  ( -0.6823417656249969321, 3.530208333674754506, -1.181850606188749264 ) ) ;
#145085 = CARTESIAN_POINT ( 'NONE',  ( 2.612550116648149512, -0.1684838578246611873, 1.732238525843646570 ) ) ;
#145086 = CARTESIAN_POINT ( 'NONE',  ( 0.5550359226569913096, 1.633180182981083028, -1.086726831054436682 ) ) ;
#145087 = CARTESIAN_POINT ( 'NONE',  ( -1.364683531250014514, 0.3010416670080866552, -0.7879004041258359514 ) ) ;
#145088 = VECTOR ( 'NONE', #76770, 1000.000000000000000 ) ;
#145089 = CARTESIAN_POINT ( 'NONE',  ( 6.245025451202089073, -1.828886558906620774, 1.152162773130911644 ) ) ;
#145090 = CARTESIAN_POINT ( 'NONE',  ( -8.513630394377489807, 12.01998699582738972, -1.199719254218446718 ) ) ;
#145091 = CARTESIAN_POINT ( 'NONE',  ( -5.517805330637490790, 9.381263952478319013, 0.7216878364870458196 ) ) ;
#145092 = CARTESIAN_POINT ( 'NONE',  ( 6.174726448494309849, -2.051094451480539149, -0.6828207641706719455 ) ) ;
#145094 = VERTEX_POINT ( 'NONE', #100766 ) ;
#145093 = CARTESIAN_POINT ( 'NONE',  ( -0.2104748580754408904, 1.337026610731705700, -2.356057411969681326 ) ) ;
#145095 = CARTESIAN_POINT ( 'NONE',  ( 0.6823417656249899377, 4.426041667008086655, -1.181850606188754593 ) ) ;
#145096 = CARTESIAN_POINT ( 'NONE',  ( 0.8076147168173102298, -1.862120749842037570, 0.1771838942275505424 ) ) ;
#145097 = CARTESIAN_POINT ( 'NONE',  ( 6.098968314571592053, 0.8511620794300640558, -1.510462927660038090 ) ) ;
#145099 = CARTESIAN_POINT ( 'NONE',  ( 2.859115728684503477, 0.3189004193784421015, -2.168101852914063876 ) ) ;
#145098 = CARTESIAN_POINT ( 'NONE',  ( -1.552391752028397856E-14, -0.04687499965855816686, 1.570758158831750295 ) ) ;
#145100 = CARTESIAN_POINT ( 'NONE',  ( 3.417284581939382448, 2.085149140145211799, 0.9887805580795704374 ) ) ;
#145101 = CARTESIAN_POINT ( 'NONE',  ( 6.468051757712944827, 1.055310785928347928, 1.769903775486596054 ) ) ;
#145102 = CARTESIAN_POINT ( 'NONE',  ( 1.640467198872105348, -1.640604414344963180, 1.038759544029205895 ) ) ;
#145103 = CARTESIAN_POINT ( 'NONE',  ( -6.860062538390436337, 7.105753837651378468, 1.040834085586084257E-14 ) ) ;
#145104 = CARTESIAN_POINT ( 'NONE',  ( -0.03436587256745584490, -7.792803924024958029, -9.554207839743707353 ) ) ;
#145105 = CARTESIAN_POINT ( 'NONE',  ( 4.043311264919998038, 0.1072909356813686182, 2.118029240109862155 ) ) ;
#145106 = CARTESIAN_POINT ( 'NONE',  ( 2.162732623366144136, 1.242727809108796322, 1.587836805404294171 ) ) ;
#145107 = CARTESIAN_POINT ( 'NONE',  ( -6.521108698048791119, 6.710307690586118312, -0.7216878364870267237 ) ) ;
#145108 = CARTESIAN_POINT ( 'NONE',  ( 5.280388062626482970, -1.229865305990836877, 1.832093573602276759 ) ) ;
#145109 = CARTESIAN_POINT ( 'NONE',  ( -3.285556943749998737, -0.5177083328553757635, 1.896917185911908499 ) ) ;
#145110 = CARTESIAN_POINT ( 'NONE',  ( -2.986852260795243463, -3.064349949800098560, 1.744271399710988879 ) ) ;
#145111 = CARTESIAN_POINT ( 'NONE',  ( 0.000000000000000000, 9.799999999999982947, 0.000000000000000000 ) ) ;
#145112 = CARTESIAN_POINT ( 'NONE',  ( -5.915100157312088491, 10.12297696016459092, -0.7998128361456362523 ) ) ;
#145114 = LINE ( 'NONE', #147226, #23287 ) ;
#145113 = CARTESIAN_POINT ( 'NONE',  ( -5.151759543144467379, 7.884679950488731492, 1.249873765817657079 ) ) ;
#145115 = CARTESIAN_POINT ( 'NONE',  ( -10.33392256004288079, 4.765625372279607141, 5.445010993851796322 ) ) ;
#145116 = ORIENTED_EDGE ( 'NONE', *, *, #118204, .F. ) ;
#145117 = CARTESIAN_POINT ( 'NONE',  ( 4.680574674004650326, -1.998471466470305602, -0.5028169189831372954 ) ) ;
#145118 = CARTESIAN_POINT ( 'NONE',  ( 1.360316468749992236, 2.765625000341414896, -4.683753385137379155E-14 ) ) ;
#145119 = LINE ( 'NONE', #47606, #123872 ) ;
#145120 = CARTESIAN_POINT ( 'NONE',  ( -6.227272627378437342, 6.159572908229946187, -0.7998128361456291469 ) ) ;
#145121 = CARTESIAN_POINT ( 'NONE',  ( -2.844178363816758814, 6.540234867753325076, -0.7998128361456481317 ) ) ;
#145122 = CARTESIAN_POINT ( 'NONE',  ( 3.176430186773027575, 0.9099569689122315452, 1.803159259486881938 ) ) ;
#145123 = CARTESIAN_POINT ( 'NONE',  ( 1.499999999999987121, 1.295833333333353377, -0.8660254037844253849 ) ) ;
#145125 = CARTESIAN_POINT ( 'NONE',  ( 8.514157279702022407, 10.95626946445095307, -1.443375672974063439 ) ) ;
#145124 = CARTESIAN_POINT ( 'NONE',  ( -3.332271893908731464, 7.109677319527304640, -0.7998128361456481317 ) ) ;
#145126 = CARTESIAN_POINT ( 'NONE',  ( 6.388916700537700777, 8.476822122092563916, 1.599625672291281386 ) ) ;
#145127 = CARTESIAN_POINT ( 'NONE',  ( 3.239188564323669528, -1.818332144261879613, 0.9699876223461401104 ) ) ;
#145128 = CARTESIAN_POINT ( 'NONE',  ( 3.305314717767214638, 1.277042846462652204, -1.560500556308255460 ) ) ;
#145129 = ORIENTED_EDGE ( 'NONE', *, *, #153640, .T. ) ;
#145130 = CARTESIAN_POINT ( 'NONE',  ( 11.89942855770814312, 12.30000000000000071, 0.6999999999999992895 ) ) ;
#145131 = CARTESIAN_POINT ( 'NONE',  ( 3.832150974156964818, 7.622593236491780999, 1.040834085586084257E-14 ) ) ;
#145132 = AXIS2_PLACEMENT_3D ( 'NONE', #99715, #13125, #111777 ) ;
#145134 = ORIENTED_EDGE ( 'NONE', *, *, #126255, .F. ) ;
#145133 = CARTESIAN_POINT ( 'NONE',  ( -0.4396101492293769120, 7.376551424357159270, -2.043156636846727991 ) ) ;
#145135 = CARTESIAN_POINT ( 'NONE',  ( 3.374374892241317703, -0.3960410224921434574, 1.976653181598592601 ) ) ;
#145136 = CARTESIAN_POINT ( 'NONE',  ( 0.9723034553027898319, -0.04304006056080753040, -1.840805954149108858 ) ) ;
#145137 = CARTESIAN_POINT ( 'NONE',  ( 0.4171991508139940574, 1.586773611656131289, -1.675818712001175381 ) ) ;
#145138 = CARTESIAN_POINT ( 'NONE',  ( 4.712340909201580885, 7.655425606447271214, -1.199719254218452047 ) ) ;
#145139 = CARTESIAN_POINT ( 'NONE',  ( 2.706508253401081809, -0.8245430293080566742, -1.998349536214229616 ) ) ;
#145140 = CARTESIAN_POINT ( 'NONE',  ( -4.446711195602264688, 4.290177271065136466, -0.7216878364870207285 ) ) ;
#145141 = CARTESIAN_POINT ( 'NONE',  ( 5.120359440597627376, 2.086519121862129289, 0.3590335527714014763 ) ) ;
#145142 = CARTESIAN_POINT ( 'NONE',  ( 2.530986164375541581, 2.254368048762548593, -0.4469772407268405301 ) ) ;
#145143 = CARTESIAN_POINT ( 'NONE',  ( 3.039951802757216548, 2.724153688964676689, -2.451370731312840778 ) ) ;
#145144 = CARTESIAN_POINT ( 'NONE',  ( 0.7779422811538607707, -1.042605501850740080, 1.552959968518424771 ) ) ;
#145145 = CARTESIAN_POINT ( 'NONE',  ( 5.330923369760363961, 0.1444485787395009269, 1.966219458991929514 ) ) ;
#145147 = CARTESIAN_POINT ( 'NONE',  ( 8.229436053370667636, 11.58446391469906267, 1.082531754730558626 ) ) ;
#145146 = CARTESIAN_POINT ( 'NONE',  ( -0.6823417656250212460, 2.801041667008084879, 1.181850606188767472 ) ) ;
#145149 = CARTESIAN_POINT ( 'NONE',  ( 6.516252164726425100, -0.9909202252585481707, -1.858390699035996407 ) ) ;
#145148 = CARTESIAN_POINT ( 'NONE',  ( -7.386494761346872551, 7.511998731193139989, -0.7998128361456291469 ) ) ;
#145150 = CARTESIAN_POINT ( 'NONE',  ( 5.969205681473694902, 1.824102622056431811, 0.9793482939001868504 ) ) ;
#145151 = CARTESIAN_POINT ( 'NONE',  ( 6.993308306550549247, 7.053281200597435685, 1.040834085586084257E-14 ) ) ;
#145152 = CARTESIAN_POINT ( 'NONE',  ( -7.237355071596549116, 7.338002426484427687, 1.040834085586084257E-14 ) ) ;
#145153 = CARTESIAN_POINT ( 'NONE',  ( 6.639320575229263888, 1.250520135805782251, 2.217830841512329787 ) ) ;
#145154 = CARTESIAN_POINT ( 'NONE',  ( 5.278184311449350297, -1.095828550124495981, 1.638662057970756925 ) ) ;
#145155 = CARTESIAN_POINT ( 'NONE',  ( 6.310808155552376952, -0.5427901682961560059, -1.945386456709609524 ) ) ;
#145156 = CARTESIAN_POINT ( 'NONE',  ( 1.499999999999987121, 0.3270833340161527492, -0.8660254037844323793 ) ) ;
#145157 = CARTESIAN_POINT ( 'NONE',  ( 4.793776464392771608, 1.707650450486393190, 1.552408976560351483 ) ) ;
#145158 = ADVANCED_FACE ( 'NONE', ( #166848 ), #201443, .F. ) ;
#145159 = CARTESIAN_POINT ( 'NONE',  ( 2.272402725641348820, -0.9685827254542198617, -1.820965734949228310 ) ) ;
#145160 = CARTESIAN_POINT ( 'NONE',  ( 7.809133291791403586, 8.213003049952529722, -0.7216878364870257245 ) ) ;
#145161 = CARTESIAN_POINT ( 'NONE',  ( 6.364626766972446781, 6.390095747748157251, 0.7998128361456352531 ) ) ;
#145162 = CARTESIAN_POINT ( 'NONE',  ( 3.237364818613055473, 6.998952398349030268, -1.734723475976807094E-15 ) ) ;
#145163 = CARTESIAN_POINT ( 'NONE',  ( -1.364683531250000748, 1.821875000341421913, 0.000000000000000000 ) ) ;
#145164 = CARTESIAN_POINT ( 'NONE',  ( 2.891631901464575272, 6.595597328342462262, 0.000000000000000000 ) ) ;
#145165 = CARTESIAN_POINT ( 'NONE',  ( 5.626270559546814098, 7.587068290936515247, 1.443375672974062551 ) ) ;
#145166 = CARTESIAN_POINT ( 'NONE',  ( 4.633362100890871638, 0.004430012494727622249, -2.171350061612055349 ) ) ;
#145167 = CARTESIAN_POINT ( 'NONE',  ( -3.314994193297896796, 6.393354490853021765, -0.7784788408506218005 ) ) ;
#145169 = CARTESIAN_POINT ( 'NONE',  ( 3.649809678215182096, 0.6660801477775115664, 1.716721118343276453 ) ) ;
#145168 = CARTESIAN_POINT ( 'NONE',  ( -3.470524135418300737, 6.032400010421219427, -1.082531754730549967 ) ) ;
#145171 = CARTESIAN_POINT ( 'NONE',  ( 6.620655732516651071, 1.309889148221474509, 1.844503626996786938 ) ) ;
#145170 = CARTESIAN_POINT ( 'NONE',  ( -0.6823417656250212460, 5.301041667008086655, 1.181850606188767472 ) ) ;
#145172 = CARTESIAN_POINT ( 'NONE',  ( 5.478137895480934105, -2.137967713159651506, -0.4810252310911074525 ) ) ;
#145173 = DIRECTION ( 'NONE',  ( 0.000000000000000000, 1.000000000000000000, 0.000000000000000000 ) ) ;
#145174 = CARTESIAN_POINT ( 'NONE',  ( 5.963815663052111304, 2.230244011310183794, -0.3799797021378086836 ) ) ;
#145175 = ORIENTED_EDGE ( 'NONE', *, *, #105176, .F. ) ;
#145176 = CARTESIAN_POINT ( 'NONE',  ( -4.244195945626527688, 7.512047922924973697, -1.038054094898384294 ) ) ;
#145177 = CARTESIAN_POINT ( 'NONE',  ( 5.323208952783781811, 7.729862296028469970, 1.309151360253474339 ) ) ;
#145178 = AXIS2_PLACEMENT_3D ( 'NONE', #196813, #96146, #30056 ) ;
#145179 = CARTESIAN_POINT ( 'NONE',  ( -5.058600711230246461, 7.955432358860325515, 1.082531754730549967 ) ) ;
#145180 = CARTESIAN_POINT ( 'NONE',  ( -6.773846765307993678, -7.473374494058229622, -6.773846765307958151 ) ) ;
#145181 = CARTESIAN_POINT ( 'NONE',  ( 0.6898892245524823608, -1.755727311204742680, -0.2225690630779184609 ) ) ;
#145182 = CARTESIAN_POINT ( 'NONE',  ( 5.567046518764520613, -1.585636444731153061, 1.240160563295252372 ) ) ;
#145183 = CARTESIAN_POINT ( 'NONE',  ( 6.470265622219697477, 8.571729197388226140, -1.599625672291262513 ) ) ;
#145184 = CARTESIAN_POINT ( 'NONE',  ( 4.682709062318923365, -2.042047207266047604, -0.5143438382350475901 ) ) ;
#145185 = CARTESIAN_POINT ( 'NONE',  ( 1.968237613432867184, -1.879027187823999245, -0.3716057669084034676 ) ) ;
#145186 = CARTESIAN_POINT ( 'NONE',  ( 4.467575310902914154, 5.170924936596891008, 1.199719254218464037 ) ) ;
#145187 = CARTESIAN_POINT ( 'NONE',  ( 2.646873730718673379, -0.3338169989568114948, -1.940879108454116375 ) ) ;
#145188 = CARTESIAN_POINT ( 'NONE',  ( 5.730724961554885866, 1.353511160402442570, -1.499384403026276180 ) ) ;
#145189 = CARTESIAN_POINT ( 'NONE',  ( 1.692057038649401601, -1.861345348035767344, -0.1864469194169729449 ) ) ;
#145190 = CARTESIAN_POINT ( 'NONE',  ( 2.330453122711079850, -1.209328770571056921, 1.544706564130463811 ) ) ;
#145193 = ORIENTED_EDGE ( 'NONE', *, *, #26563, .F. ) ;
#145192 = CARTESIAN_POINT ( 'NONE',  ( 1.107505169401588274, 1.450017293480215352, 1.247013401884336403 ) ) ;
#145191 = CARTESIAN_POINT ( 'NONE',  ( 4.846200500028392533, 1.720618765505038006, 0.1221847348328516936 ) ) ;
#145195 = CARTESIAN_POINT ( 'NONE',  ( 4.175548123328908900, 7.815297210618305179, -0.7216878364870197293 ) ) ;
#145194 = CARTESIAN_POINT ( 'NONE',  ( 1.084930333755677045, -2.153824616689365978, -0.4803136671489223741 ) ) ;
#145196 = CARTESIAN_POINT ( 'NONE',  ( -1.364683531249997417, 2.571875000341422357, 1.214306433183764966E-14 ) ) ;
#145198 = ADVANCED_FACE ( 'NONE', ( #184143 ), #102908, .T. ) ;
#145197 = CARTESIAN_POINT ( 'NONE',  ( 7.079328764629950754, 11.41096732537697633, 0.7998128361456462443 ) ) ;
#145199 = CYLINDRICAL_SURFACE ( 'NONE', #136682, 0.08000000000000004330 ) ;
#145200 = CARTESIAN_POINT ( 'NONE',  ( 0.5972946010069523082, 6.677937103010220810, -3.537249470680236652 ) ) ;
#145201 = CARTESIAN_POINT ( 'NONE',  ( -5.607791805026555387, 5.591516722556655772, -0.3863011750756854545 ) ) ;
#145202 = CARTESIAN_POINT ( 'NONE',  ( 6.895378825052528526, -1.852007112603266670, 0.9253362530580526712 ) ) ;
#145203 = CARTESIAN_POINT ( 'NONE',  ( 1.152881054890652957, -0.5012615762394446728, -2.008655542368184221 ) ) ;
#145204 = CARTESIAN_POINT ( 'NONE',  ( -0.7500000000000006661, 1.858333333333357595, -1.299038105676652011 ) ) ;
#145205 = CARTESIAN_POINT ( 'NONE',  ( 6.148786358997489820, 7.132337826040578754, -1.199719254218446718 ) ) ;
#145206 = CARTESIAN_POINT ( 'NONE',  ( -6.632963465583701534, 8.761543347979550589, -1.599625672291263179 ) ) ;
#145207 = CARTESIAN_POINT ( 'NONE',  ( 6.391743074199808916, 6.421731439513382433, -0.7998128361456481317 ) ) ;
#145208 = CARTESIAN_POINT ( 'NONE',  ( 5.303433364654348559, 1.869980213031800398, -0.9998494819224086338 ) ) ;
#145209 = CARTESIAN_POINT ( 'NONE',  ( 4.329849954717849947, 6.144853928627882489, 1.599625672291262513 ) ) ;
#145210 = CARTESIAN_POINT ( 'NONE',  ( -0.6823417656250212460, 2.051041667008083991, 1.181850606188767472 ) ) ;
#145211 = CARTESIAN_POINT ( 'NONE',  ( 1.499999999999989120, 4.004166666666685970, 0.8660254037844524744 ) ) ;
#145213 = CARTESIAN_POINT ( 'NONE',  ( 4.871457266011829823, 4.577788319968905562, -0.7998128361456221525 ) ) ;
#145212 = CARTESIAN_POINT ( 'NONE',  ( 6.566857081534598350, 1.454584517406570132, -1.316677807353151097 ) ) ;
#145214 = CARTESIAN_POINT ( 'NONE',  ( 4.604842190751081255, 0.8645911521153251122, -1.821463593394745395 ) ) ;
#145215 = CARTESIAN_POINT ( 'NONE',  ( 4.118306542938309889, 1.879866726353071060, 0.3679503660072875881 ) ) ;
#145216 = SURFACE_STYLE_FILL_AREA ( #94318 ) ;
#145217 = CARTESIAN_POINT ( 'NONE',  ( 1.804482060849887270, 1.621174160030929068, -1.474864209862189579 ) ) ;
#145218 = CARTESIAN_POINT ( 'NONE',  ( -1.826099658463393061, 3.981846818257626541, 0.3999999999999835354 ) ) ;
#145219 = CARTESIAN_POINT ( 'NONE',  ( -1.500000000000015099, 0.1604166673494879791, -0.8660254037844383745 ) ) ;
#145220 = CARTESIAN_POINT ( 'NONE',  ( 4.834244255588106221, -1.080646305101562232, -1.698427166264226518 ) ) ;
#145221 = CARTESIAN_POINT ( 'NONE',  ( -7.854251061018346469, 8.057714414143200443, -0.7998128361456291469 ) ) ;
#145223 = CARTESIAN_POINT ( 'NONE',  ( 6.046512527486515687, -1.496967179435993778, 1.497493072882298382 ) ) ;
#145222 = CARTESIAN_POINT ( 'NONE',  ( -4.636525346193588248, 4.511627113421689650, 0.7216878364870317197 ) ) ;
#145224 = SURFACE_STYLE_USAGE ( .BOTH. , #161449 ) ;
#145226 = CARTESIAN_POINT ( 'NONE',  ( -5.935437387732586778, 10.14670372898850381, -0.7998128361456362523 ) ) ;
#145225 = CARTESIAN_POINT ( 'NONE',  ( 4.001575260567552306, -2.085028717228009310, 0.1556281442064103848 ) ) ;
#145228 = ORIENTED_EDGE ( 'NONE', *, *, #146528, .F. ) ;
#145227 = CARTESIAN_POINT ( 'NONE',  ( 2.098289149679245735, -0.4564329974444079618, -1.663208130003128948 ) ) ;
#145229 = CARTESIAN_POINT ( 'NONE',  ( 5.730757696090862829, 1.422813033107739988, -1.572628729999878905 ) ) ;
#145230 = CARTESIAN_POINT ( 'NONE',  ( 6.582647274634798151, 7.638508894284114170, 1.199719254218462483 ) ) ;
#145231 = FACE_OUTER_BOUND ( 'NONE', #25471, .T. ) ;
#145232 = DIRECTION ( 'NONE',  ( 0.000000000000000000, 0.000000000000000000, 1.000000000000000000 ) ) ;
#145233 = CARTESIAN_POINT ( 'NONE',  ( 7.494959990256193194, 7.638541498254023843, -0.7998128361456281477 ) ) ;
#145234 = EDGE_LOOP ( 'NONE', ( #72412, #181143, #98050, #198912 ) ) ;
#145235 = LINE ( 'NONE', #25035, #116920 ) ;
#145236 = ORIENTED_EDGE ( 'NONE', *, *, #108943, .T. ) ;
#145238 = CARTESIAN_POINT ( 'NONE',  ( 1.400706157114139261, -0.2655193030335687987, -1.791778796870816759 ) ) ;
#145237 = CARTESIAN_POINT ( 'NONE',  ( 6.391743074199808916, 6.421731439513382433, -0.7998128361456481317 ) ) ;
#145239 = CARTESIAN_POINT ( 'NONE',  ( -7.881367368245678406, 8.089350105908421185, 0.7998128361456602331 ) ) ;
#145240 = ORIENTED_EDGE ( 'NONE', *, *, #103885, .T. ) ;
#145241 = CARTESIAN_POINT ( 'NONE',  ( 2.679707916995359263, 6.278076336469897711, -0.7998128361456291469 ) ) ;
#145242 = VERTEX_POINT ( 'NONE', #165782 ) ;
#145243 = CARTESIAN_POINT ( 'NONE',  ( 6.886615681098613884, 6.999082814228660077, 0.000000000000000000 ) ) ;
#145244 = CARTESIAN_POINT ( 'NONE',  ( 3.053145041208281452, -1.596494782498259157, 0.8559496646718143253 ) ) ;
#145245 = CARTESIAN_POINT ( 'NONE',  ( 6.539320575229256249, 2.979067782826943844, 2.350490835693248126 ) ) ;
#145246 = CARTESIAN_POINT ( 'NONE',  ( -10.95700306400769897, -7.901429653175727097, 0.3289054322349619919 ) ) ;
#145247 = CARTESIAN_POINT ( 'NONE',  ( 4.244147651705390878, 7.284590634535035747, 0.9143829328417275581 ) ) ;
#145248 = ORIENTED_EDGE ( 'NONE', *, *, #1373, .F. ) ;
#145249 =( GEOMETRIC_REPRESENTATION_CONTEXT ( 3 ) GLOBAL_UNCERTAINTY_ASSIGNED_CONTEXT ( ( #33457 ) ) GLOBAL_UNIT_ASSIGNED_CONTEXT ( ( #151033, #52451, #1532 ) ) REPRESENTATION_CONTEXT ( 'NONE', 'WORKASPACE' ) );
#145250 = CARTESIAN_POINT ( 'NONE',  ( 3.472968545230222581, 1.681562272349636622, 0.7977436208898255332 ) ) ;
#145251 = CARTESIAN_POINT ( 'NONE',  ( 2.108866759644252298, 0.002224897612410503371, 1.915793139840407333 ) ) ;
#145252 = CARTESIAN_POINT ( 'NONE',  ( 0.2526013166088726392, -1.469656019175567208, 1.082793315970068004 ) ) ;
#145253 = CARTESIAN_POINT ( 'NONE',  ( 1.500095892183267887, 4.450208832515674118, 0.08036760724049675508 ) ) ;
#145254 = CARTESIAN_POINT ( 'NONE',  ( -2.324088772396477673E-16, -1.093749999044084653, -3.475000000000000089 ) ) ;
#145255 = CARTESIAN_POINT ( 'NONE',  ( 4.661274270878652537, 8.290979908523663511, 0.5017903844357074483 ) ) ;
#145256 = CYLINDRICAL_SURFACE ( 'NONE', #116117, 0.07999999999999998779 ) ;
#145257 = CARTESIAN_POINT ( 'NONE',  ( -2.765500147507697459, 5.209872024525476597, 1.082531754730560403 ) ) ;
#145258 = CARTESIAN_POINT ( 'NONE',  ( 8.948018195339340508, 9.541702104091804415, -0.7216878364870197293 ) ) ;
#145259 = CARTESIAN_POINT ( 'NONE',  ( 5.102387438446081447, 1.963913563476852309, 0.1487572088093111478 ) ) ;
#145260 = CARTESIAN_POINT ( 'NONE',  ( -4.334856428067329404, 6.080418470877079429, -1.599625672291256295 ) ) ;
#145261 = CARTESIAN_POINT ( 'NONE',  ( 0.7442207691023922100, 0.6088243375477386810, 2.000016368695969327 ) ) ;
#145262 = DIRECTION ( 'NONE',  ( 0.000000000000000000, 0.000000000000000000, 1.000000000000000000 ) ) ;
#145263 = CARTESIAN_POINT ( 'NONE',  ( 5.666998703487860389, -1.741597003894586937, -0.8236021136211798543 ) ) ;
#145264 = CARTESIAN_POINT ( 'NONE',  ( -5.859094939400033120, 9.987361195942037639, -0.7998128361456231517 ) ) ;
#145265 = CARTESIAN_POINT ( 'NONE',  ( 0.7447965706881399806, -1.568309060004613231, 0.9341869532639992535 ) ) ;
#145266 = CARTESIAN_POINT ( 'NONE',  ( 2.034064749695370100, -1.442962035976073309, -1.669870808145665020 ) ) ;
#145267 = EDGE_CURVE ( 'NONE', #115982, #157333, #167909, .T. ) ;
#145268 = CARTESIAN_POINT ( 'NONE',  ( -6.282293365727707801, 6.900897561460068275, 0.7630008232915044264 ) ) ;
#145269 = CARTESIAN_POINT ( 'NONE',  ( -0.05268457437105152075, -1.747710896673961622, 0.7768168958157274373 ) ) ;
#145270 = ORIENTED_EDGE ( 'NONE', *, *, #154049, .F. ) ;
#145271 = ORIENTED_EDGE ( 'NONE', *, *, #213625, .T. ) ;
#145272 = CARTESIAN_POINT ( 'NONE',  ( 0.3089591345776849241, -1.584006439100977603, 1.170298647042963935 ) ) ;
#145273 = CARTESIAN_POINT ( 'NONE',  ( 1.347104335016526599, 0.5619601930287048130, -1.858996895088180556 ) ) ;
#145274 = ORIENTED_EDGE ( 'NONE', *, *, #80361, .F. ) ;
#145275 = CARTESIAN_POINT ( 'NONE',  ( 0.2806244687772480040, -1.977743564115455932, 0.3905345501400147024 ) ) ;
#145277 = CARTESIAN_POINT ( 'NONE',  ( 4.996841193152741667, 0.3155067605547862142, 1.833815385591957448 ) ) ;
#145276 = CARTESIAN_POINT ( 'NONE',  ( -6.629010762438975135, 6.698543742459062145, -0.7998128361456362523 ) ) ;
#145278 = CARTESIAN_POINT ( 'NONE',  ( 4.538947565524982686, 8.517465603079630299, 0.000000000000000000 ) ) ;
#145279 = CARTESIAN_POINT ( 'NONE',  ( -2.550000000000000266, 1.000000000000000888, -1.849324200890690717 ) ) ;
#145280 = DIRECTION ( 'NONE',  ( 0.000000000000000000, 0.000000000000000000, -1.000000000000000000 ) ) ;
#145281 = CARTESIAN_POINT ( 'NONE',  ( -5.928993247877788697, 5.811580298812519807, 0.7998128361456341429 ) ) ;
#145282 = CARTESIAN_POINT ( 'NONE',  ( -7.262327558775498737, 8.501745569106741840, 1.199719254218452047 ) ) ;
#145283 = CARTESIAN_POINT ( 'NONE',  ( 1.400213348495438437, -0.7931047570679079506, -2.043190674350242819 ) ) ;
#145284 = CARTESIAN_POINT ( 'NONE',  ( 2.385871846325007706, 5.727341554113725586, -0.7216878364870267237 ) ) ;
#145285 = ORIENTED_EDGE ( 'NONE', *, *, #58887, .F. ) ;
#145286 = CARTESIAN_POINT ( 'NONE',  ( 6.230854113932139171, 9.427024345299638952, 1.199719254218452047 ) ) ;
#145287 = CARTESIAN_POINT ( 'NONE',  ( -11.33772463945037146, 12.69999999999998153, 3.679999999999999272 ) ) ;
#145289 = EDGE_CURVE ( 'NONE', #99453, #159480, #151217, .T. ) ;
#145288 = CARTESIAN_POINT ( 'NONE',  ( 2.156629195875509719, -1.411784796728832392, 1.157573153174975111 ) ) ;
#145290 = CARTESIAN_POINT ( 'NONE',  ( 0.4702634422464547770, 7.494255424139249833, 4.464191613398297953 ) ) ;
#145291 = CARTESIAN_POINT ( 'NONE',  ( -3.632695093457760649, 6.325562478087638496, -1.199719254218452047 ) ) ;
#145292 = CARTESIAN_POINT ( 'NONE',  ( -0.3989295472767397932, 3.108275709649451102, -2.025156007033537708 ) ) ;
#145293 = CARTESIAN_POINT ( 'NONE',  ( 6.609000000000034625, 7.052688111495289291, 2.598153854230552895 ) ) ;
#145294 = CARTESIAN_POINT ( 'NONE',  ( 10.38962578677386084, 11.01565159419135043, 0.000000000000000000 ) ) ;
#145295 = CARTESIAN_POINT ( 'NONE',  ( 1.277817996239123177, 1.146848889641904234, 1.547804080865310850 ) ) ;
#145296 = CARTESIAN_POINT ( 'NONE',  ( 6.016451032921247055, 0.7918200671565789328, 1.795022358689959185 ) ) ;
#145297 = CARTESIAN_POINT ( 'NONE',  ( -6.530223543276495235, 10.77034456713125188, -0.7998128361456291469 ) ) ;
#145298 = CARTESIAN_POINT ( 'NONE',  ( 5.473741331615251227, 7.409117525016355010, -1.599625672291262513 ) ) ;
#145299 = CARTESIAN_POINT ( 'NONE',  ( 5.425378541715013547, -1.389685604419872655, -1.694579525865948844 ) ) ;
#145300 = CARTESIAN_POINT ( 'NONE',  ( 1.500000000000039524, 7.000000000000000000, -10.99818166789401097 ) ) ;
#145301 = CARTESIAN_POINT ( 'NONE',  ( 3.784089331405198209, -1.229265877060268242, -1.665672133652921660 ) ) ;
#145303 = CARTESIAN_POINT ( 'NONE',  ( 1.364683531249986537, 0.6760416670080884316, 0.7879004041258500513 ) ) ;
#145302 = FACE_OUTER_BOUND ( 'NONE', #26218, .T. ) ;
#145304 = EDGE_LOOP ( 'NONE', ( #55275, #195175, #6259, #177939, #44043 ) ) ;
#145305 = VERTEX_POINT ( 'NONE', #53085 ) ;
#145306 = CARTESIAN_POINT ( 'NONE',  ( 4.043764476089898530, -1.703284420474758143, 1.543771250003633355 ) ) ;
#145308 = ORIENTED_EDGE ( 'NONE', *, *, #150358, .T. ) ;
#145307 = CARTESIAN_POINT ( 'NONE',  ( 6.616015773788773480, 10.66250946948817813, -0.7216878364870267237 ) ) ;
#145310 = CARTESIAN_POINT ( 'NONE',  ( 1.001543065824772753E-15, -0.3718749995220430038, 3.793834371823811669 ) ) ;
#145309 = CARTESIAN_POINT ( 'NONE',  ( 4.882344714696929877, 8.710169577206153591, -0.7216878364870458196 ) ) ;
#145312 = EDGE_CURVE ( 'NONE', #44672, #161612, #116769, .T. ) ;
#145311 = CARTESIAN_POINT ( 'NONE',  ( -7.730132016634532199, -5.756136661604536187, -7.730132016634490455 ) ) ;
#145313 = B_SPLINE_CURVE_WITH_KNOTS ( 'NONE', 3,
 ( #3875, #123105, #89450, #69948 ),
 .UNSPECIFIED., .F., .F.,
 ( 4, 4 ),
 ( 0.0001647631253658502772, 0.001106915643567259362 ),
 .UNSPECIFIED. ) ;
#145314 = CARTESIAN_POINT ( 'NONE',  ( -7.075376061485238566, 9.347967719856493218, 1.599625672291269396 ) ) ;
#145315 = CARTESIAN_POINT ( 'NONE',  ( 3.890518024738118807, 1.639914603359222456, -1.039847546996591765 ) ) ;
#145316 = CARTESIAN_POINT ( 'NONE',  ( -11.18654035131441127, 1.000000000000000888, 4.041720556560751021 ) ) ;
#145317 = ADVANCED_FACE ( 'NONE', ( #149529 ), #84521, .T. ) ;
#145318 = ORIENTED_EDGE ( 'NONE', *, *, #178819, .F. ) ;
#145319 = CARTESIAN_POINT ( 'NONE',  ( 5.220932206144772714, 1.444093599275039885, -1.253800916539760113 ) ) ;
#145320 = FACE_OUTER_BOUND ( 'NONE', #5253, .T. ) ;
#145321 = CARTESIAN_POINT ( 'NONE',  ( 6.545920775329808983, 0.6544052999908689383, -1.596017746584824426 ) ) ;
#145322 = CARTESIAN_POINT ( 'NONE',  ( 4.874232570624013050, -2.001857581374043349, -0.2420344392276354561 ) ) ;
#145323 = CARTESIAN_POINT ( 'NONE',  ( -0.1532706334859310904, -0.8918953437966909981, -3.289477106180646704 ) ) ;
#145324 = CARTESIAN_POINT ( 'NONE',  ( 1.911028901235469313, 1.633884665098099598, -1.483674895440662667 ) ) ;
#145326 = CARTESIAN_POINT ( 'NONE',  ( -4.828112100242291760, 6.726159765073026264, -1.443375672974066548 ) ) ;
#145325 = CARTESIAN_POINT ( 'NONE',  ( 11.07790593930098311, 13.79999999999999893, 0.6999999999999992895 ) ) ;
#145328 = CARTESIAN_POINT ( 'NONE',  ( 0.3207183204587023551, -0.09351970983179427876, 1.767511165302604326 ) ) ;
#145327 = CARTESIAN_POINT ( 'NONE',  ( 1.904351452098542063, 1.548259960728815665, -1.405051437006714643 ) ) ;
#145329 = CARTESIAN_POINT ( 'NONE',  ( 5.906875006520014182, -1.122496024291631755, -1.674889250513518446 ) ) ;
#145331 = CARTESIAN_POINT ( 'NONE',  ( 2.976851957573245944, -0.1693691376928093406, -2.286062073229557345 ) ) ;
#145330 = CARTESIAN_POINT ( 'NONE',  ( 4.199993725183334803, 8.122019456014369254, -0.7998128361456362523 ) ) ;
#145332 = CARTESIAN_POINT ( 'NONE',  ( 0.6205767395346533100, -1.653899685646512019, 0.5418069113267124370 ) ) ;
#145333 = AXIS2_PLACEMENT_3D ( 'NONE', #181613, #48457, #707 ) ;
#145334 = CARTESIAN_POINT ( 'NONE',  ( 2.981521246686049231, 6.451858035227898469, -0.1755584056236529911 ) ) ;
#145335 = CARTESIAN_POINT ( 'NONE',  ( 0.7899210882133401723, -1.648783996043493350, 0.5366646198887611297 ) ) ;
#145336 = CARTESIAN_POINT ( 'NONE',  ( -2.353626204688216217E-14, 0.1093750003414345612, -1.570758158831782270 ) ) ;
#145337 = CARTESIAN_POINT ( 'NONE',  ( -11.35573736746270335, 12.48729585586721491, 3.554362808847973731 ) ) ;
#145338 = CARTESIAN_POINT ( 'NONE',  ( 1.592468369012179918, 1.070935286220242366, -1.888628467986789738 ) ) ;
#145339 = CARTESIAN_POINT ( 'NONE',  ( 2.800017839408690090, -0.9981255096969069429, -1.752139039461996006 ) ) ;
#145340 = CARTESIAN_POINT ( 'NONE',  ( 3.718750000000002220, -0.7852924748297895885, 1.895863743164163617 ) ) ;
#145341 = CARTESIAN_POINT ( 'NONE',  ( -1.201851678989727383E-14, 0.9937500006828198229, 1.732050807568877637 ) ) ;
#145342 = CARTESIAN_POINT ( 'NONE',  ( 6.094356125077982078, -1.917462007409322267, -0.1864201481798656301 ) ) ;
#145343 = CARTESIAN_POINT ( 'NONE',  ( 1.364683531250000303, 13.25520833367472839, -0.7879004041258355073 ) ) ;
#145344 = CARTESIAN_POINT ( 'NONE',  ( 3.973042321754824524, -1.644474126697339944, 1.493583396047935219 ) ) ;
#145345 = ORIENTED_EDGE ( 'NONE', *, *, #145827, .T. ) ;
#145346 = DIRECTION ( 'NONE',  ( 0.000000000000000000, 0.000000000000000000, 1.000000000000000000 ) ) ;
#145347 = DIRECTION ( 'NONE',  ( -1.000000000000000000, 5.421010862427522170E-16, 0.000000000000000000 ) ) ;
#145348 = CARTESIAN_POINT ( 'NONE',  ( 8.402302512167096893, 10.82577223566020841, -1.599625672291268286 ) ) ;
#145349 = CARTESIAN_POINT ( 'NONE',  ( 6.170369307550816806, 9.252495721234380355, 1.082531754730549967 ) ) ;
#145350 = CARTESIAN_POINT ( 'NONE',  ( -1.364683531250000748, -1.240624999658580752, 0.000000000000000000 ) ) ;
#145351 = CARTESIAN_POINT ( 'NONE',  ( 5.811982450300033243, 1.162468279597946630, -1.295502344845029574 ) ) ;
#145352 = ADVANCED_FACE ( 'NONE', ( #172188 ), #140781, .T. ) ;
#145353 = CARTESIAN_POINT ( 'NONE',  ( 3.666413850373055450, -0.7928392042928497085, -1.794698522912529182 ) ) ;
#145355 = CARTESIAN_POINT ( 'NONE',  ( -4.595850885352567694, 8.305650432979225783, 1.040834085586084257E-14 ) ) ;
#145354 = CARTESIAN_POINT ( 'NONE',  ( 2.523789150438203510, 6.096171108819874007, 0.7998128361456462443 ) ) ;
#145356 = AXIS2_PLACEMENT_3D ( 'NONE', #138948, #189802, #92347 ) ;
#145357 = CARTESIAN_POINT ( 'NONE',  ( -1.466385952843404006, 4.235368455307408908, 0.3259651399136407890 ) ) ;
#145358 = CARTESIAN_POINT ( 'NONE',  ( 4.130342294306089457, 1.214786636354926452, -1.908452007788311366 ) ) ;
#145359 = CARTESIAN_POINT ( 'NONE',  ( 2.154800422482431532, -0.5477745769525663722, -1.988566864369076592 ) ) ;
#145360 = CARTESIAN_POINT ( 'NONE',  ( -6.775324078527193983, 8.927630729746953264, -1.599625672291263179 ) ) ;
#145361 =( BOUNDED_CURVE ( )  B_SPLINE_CURVE ( 3, ( #207829, #123496, #172157, #56270 ),
 .UNSPECIFIED., .F., .T. ) 
 B_SPLINE_CURVE_WITH_KNOTS ( ( 4, 4 ),
 ( 4.712388980384695003, 5.276666415325903969 ),
 .UNSPECIFIED. ) 
 CURVE ( )  GEOMETRIC_REPRESENTATION_ITEM ( )  RATIONAL_B_SPLINE_CURVE ( ( 1.000000000000000000, 0.9736414627471347005, 0.9736414627471347005, 1.000000000000000000 ) ) 
 REPRESENTATION_ITEM ( '' )  );
#145362 = CARTESIAN_POINT ( 'NONE',  ( 2.448426410784361185, 2.261989705503023806, 0.05584468559862928311 ) ) ;
#145363 = ORIENTED_EDGE ( 'NONE', *, *, #63620, .T. ) ;
#145364 = CARTESIAN_POINT ( 'NONE',  ( -0.7500000000000006661, 1.639583334016154970, -1.299038105676652011 ) ) ;
#145365 = CARTESIAN_POINT ( 'NONE',  ( 4.006994748872731549, 1.602975652146242380, 0.9638501484771769823 ) ) ;
#145366 = CARTESIAN_POINT ( 'NONE',  ( 2.812812116114179251, 0.9611239539163253243, -1.443176275507858319 ) ) ;
#145367 = CARTESIAN_POINT ( 'NONE',  ( 6.198795224570643470, 1.821041368708445907, 1.219022265761634971 ) ) ;
#145368 = CARTESIAN_POINT ( 'NONE',  ( 0.2357703454196959370, -2.016519153289020760, 0.8967723332334791575 ) ) ;
#145369 = CARTESIAN_POINT ( 'NONE',  ( 4.522454563201145028, 1.332364063043836033, -1.702191164408660251 ) ) ;
#145370 = CARTESIAN_POINT ( 'NONE',  ( 4.804598357785225815, 1.690330731384475094, 0.9558792251623483560 ) ) ;
#145371 = CARTESIAN_POINT ( 'NONE',  ( -2.426546306721660606, 5.774795091243142053, 0.7216878364870317197 ) ) ;
#145373 = UNCERTAINTY_MEASURE_WITH_UNIT (LENGTH_MEASURE( 1.000000000000000082E-05 ), #180815, 'distance_accuracy_value', 'NONE');
#145372 = CARTESIAN_POINT ( 'NONE',  ( -2.580963302752292243, -0.4788041664876945269, 0.000000000000000000 ) ) ;
#145374 = CARTESIAN_POINT ( 'NONE',  ( 4.047743032765107607, 7.529339606631276105, 0.4638284745723305624 ) ) ;
#145375 = CARTESIAN_POINT ( 'NONE',  ( 0.003376046620571365731, -7.161464053357560644, 9.586610838029431036 ) ) ;
#145376 = CARTESIAN_POINT ( 'NONE',  ( 0.2631197012187462270, -3.232243495192088645, 3.285556943749978753 ) ) ;
#145377 = CARTESIAN_POINT ( 'NONE',  ( -1.360316468749998675, 2.411458333674740828, 0.7853790794158941324 ) ) ;
#145378 = CARTESIAN_POINT ( 'NONE',  ( 6.170546107226446253, 1.392543322632183722, 1.458558933167881211 ) ) ;
#145379 = CARTESIAN_POINT ( 'NONE',  ( -10.32861409551237486, 10.94447128771960287, 1.040834085586084257E-14 ) ) ;
#145380 = CARTESIAN_POINT ( 'NONE',  ( 8.392660782059197189, 9.750191319612612872, 1.199719254218462483 ) ) ;
#145381 = CARTESIAN_POINT ( 'NONE',  ( 2.905190055078214595, 6.611415174225076186, 0.7998128361456271485 ) ) ;
#145382 = CARTESIAN_POINT ( 'NONE',  ( 2.754317325142870754, 0.6151756178996542479, 1.719052816137212503 ) ) ;
#145383 = CARTESIAN_POINT ( 'NONE',  ( -7.055228938194283650, -8.176568542494891290, 6.396834479292372144 ) ) ;
#145384 = EDGE_LOOP ( 'NONE', ( #180875, #137630, #3325, #196086 ) ) ;
#145385 = CARTESIAN_POINT ( 'NONE',  ( -3.458738584817664385, 7.049295759013638474, 0.7216878364870338292 ) ) ;
#145386 = CARTESIAN_POINT ( 'NONE',  ( 3.285556943750000070, -3.871874999522042504, 0.000000000000000000 ) ) ;
#145387 = CARTESIAN_POINT ( 'NONE',  ( -6.645467848992654858, 10.90479625713344625, 0.7998128361456481317 ) ) ;
#145388 = CARTESIAN_POINT ( 'NONE',  ( 1.125267019654611733, 1.783345095244772249, 0.9482059100444378830 ) ) ;
#145389 = CARTESIAN_POINT ( 'NONE',  ( 0.8738735914427527840, 0.4098651554323496926, -2.080331290949386513 ) ) ;
#145390 = ORIENTED_EDGE ( 'NONE', *, *, #91149, .T. ) ;
#145391 = CARTESIAN_POINT ( 'NONE',  ( -5.906512197408906317, 6.919960980845699439, -1.199719254218453823 ) ) ;
#145392 = CARTESIAN_POINT ( 'NONE',  ( 2.008444763995967275, 0.5780311502073384178, 1.769000597778628947 ) ) ;
#145393 = CARTESIAN_POINT ( 'NONE',  ( 4.891794496432329886, 4.601515088792824670, -0.7998128361456211532 ) ) ;
#145394 = CARTESIAN_POINT ( 'NONE',  ( 6.631718597260928050, -1.344210725561691300, -1.562263648894322898 ) ) ;
#145395 = CARTESIAN_POINT ( 'NONE',  ( 6.135388727473008785, 0.6351960432287793168, 1.913804721665197883 ) ) ;
#145396 = ORIENTED_EDGE ( 'NONE', *, *, #56811, .T. ) ;
#145397 = CARTESIAN_POINT ( 'NONE',  ( -6.091691091241777656, 6.001394449403842479, 0.7998128361456341429 ) ) ;
#145398 = CARTESIAN_POINT ( 'NONE',  ( -9.541187415715041809, 12.15447128979948310, -1.599625672291263179 ) ) ;
#145399 = CARTESIAN_POINT ( 'NONE',  ( 3.615676881913011176, -1.798418494116042821, 0.3134422064149794407 ) ) ;
#145401 = CARTESIAN_POINT ( 'NONE',  ( -2.324088772396477673E-16, -2.887500000000000178, -3.475000000000000089 ) ) ;
#145400 = CARTESIAN_POINT ( 'NONE',  ( -5.167592825464113915, 6.057888380243431570, 1.199719254218452935 ) ) ;
#145402 = CARTESIAN_POINT ( 'NONE',  ( 6.344829475870412239, 6.940264737885684987, 0.8615092103797560297 ) ) ;
#145403 = CARTESIAN_POINT ( 'NONE',  ( 5.852888695852590750, -0.9090035733541059759, 1.799648235488074732 ) ) ;
#145404 = CARTESIAN_POINT ( 'NONE',  ( 5.296754776809613041, 1.507285696749562476, 1.057021923447129197 ) ) ;
#145405 = CARTESIAN_POINT ( 'NONE',  ( 0.07680821025393863577, 5.725641208404781857, -2.404836704152548688 ) ) ;
#145406 = CARTESIAN_POINT ( 'NONE',  ( 3.440313875665978127, 1.038139129215289946, -2.061066213440334582 ) ) ;
#145407 = CARTESIAN_POINT ( 'NONE',  ( 6.866278450678116485, 6.975356045404744521, 0.000000000000000000 ) ) ;
#145408 = CARTESIAN_POINT ( 'NONE',  ( 6.345025448074324892, -1.829860219143174982, 1.150409744987097804 ) ) ;
#145409 = CARTESIAN_POINT ( 'NONE',  ( 6.226218857173709154, 8.287007971501239467, 1.599625672291281386 ) ) ;
#145410 = CARTESIAN_POINT ( 'NONE',  ( 1.593202639421680278, -0.6524502387153191529, 1.829324111618094717 ) ) ;
#145411 = VERTEX_POINT ( 'NONE', #58428 ) ;
#145412 = CARTESIAN_POINT ( 'NONE',  ( 4.464446571738351466, 1.842799458866357210, 1.373389552433499139 ) ) ;
#145413 = LINE ( 'NONE', #195187, #23793 ) ;
#145414 = CARTESIAN_POINT ( 'NONE',  ( -3.142457743317409680, 6.888227477170756785, 0.7998128361456352531 ) ) ;
#145415 = CARTESIAN_POINT ( 'NONE',  ( 4.592568387165754551, -0.4099775813008778025, -1.825014511474598589 ) ) ;
#145416 = ORIENTED_EDGE ( 'NONE', *, *, #143956, .F. ) ;
#145419 = CARTESIAN_POINT ( 'NONE',  ( -4.664887371553763096, 7.600063145858131364, -1.199719254218453823 ) ) ;
#145418 = CARTESIAN_POINT ( 'NONE',  ( -0.7500000000000006661, 0.3895833340161539149, -1.299038105676652011 ) ) ;
#145417 = CARTESIAN_POINT ( 'NONE',  ( 2.777492966359981441, 0.2764497561681695803, -1.892163382976944419 ) ) ;
#145420 = CARTESIAN_POINT ( 'NONE',  ( 4.055453297694236348, -1.834216022232620702, -1.226887332174103173 ) ) ;
#145421 = CARTESIAN_POINT ( 'NONE',  ( 6.883263157960364254, 6.036844454314826081, 2.541088405340941492 ) ) ;
#145422 = CARTESIAN_POINT ( 'NONE',  ( 2.530568227245037605, 6.104080031761181857, 0.000000000000000000 ) ) ;
#145423 = CARTESIAN_POINT ( 'NONE',  ( 6.333067150914808430, 8.481940657524365434, 1.443375672974063439 ) ) ;
#145424 = CARTESIAN_POINT ( 'NONE',  ( -3.755772246185468788, 4.340488027759846545, -1.199719254218452047 ) ) ;
#145425 = CARTESIAN_POINT ( 'NONE',  ( -4.597623488365601752, 8.377994813152914944, 0.7216878364870267237 ) ) ;
#145426 = CARTESIAN_POINT ( 'NONE',  ( 1.792193567899300177, -1.961476155570774926, -0.1973719964898524026 ) ) ;
#145427 = CARTESIAN_POINT ( 'NONE',  ( 1.536587678696316184, 1.135727589777148605, -2.008695742776007709 ) ) ;
#145428 = CARTESIAN_POINT ( 'NONE',  ( 2.137090596337941406, -0.09316805448006218460, -1.959763546484971197 ) ) ;
#145429 = CARTESIAN_POINT ( 'NONE',  ( 11.35573736746281526, 11.11270414413281848, 3.554362808847904009 ) ) ;
#145430 = CARTESIAN_POINT ( 'NONE',  ( 5.858276910504900847, -2.062741130177087268, -0.005609060510954055022 ) ) ;
#145431 = CARTESIAN_POINT ( 'NONE',  ( 5.178851490740205676, 6.104710163027444736, 1.082531754730558626 ) ) ;
#145432 = CARTESIAN_POINT ( 'NONE',  ( 4.193214648376505593, 8.114110533073061404, 0.000000000000000000 ) ) ;
#145433 = ORIENTED_EDGE ( 'NONE', *, *, #74793, .F. ) ;
#145434 = CARTESIAN_POINT ( 'NONE',  ( -0.6823417656250212460, 5.613541667008087543, 1.181850606188767472 ) ) ;
#145435 = CARTESIAN_POINT ( 'NONE',  ( -0.9311234436981480345, -1.471869630441517751, -3.475000000000001421 ) ) ;
#145436 = CARTESIAN_POINT ( 'NONE',  ( 10.18233705906309972, 11.83814697611718714, 1.199719254218450271 ) ) ;
#145437 = CARTESIAN_POINT ( 'NONE',  ( 0.5499837882529658994, 1.607816289776839991, 1.459057700483844311 ) ) ;
#145438 = CARTESIAN_POINT ( 'NONE',  ( -0.7500000000000179856, 12.29166666666666607, 1.299038105676658228 ) ) ;
#145439 = CARTESIAN_POINT ( 'NONE',  ( 6.445605026751811018, -8.233137084989715859, 6.979380938965673131 ) ) ;
#145440 = CARTESIAN_POINT ( 'NONE',  ( 3.511198596259283544, 6.271927390929313617, 2.420000000000010587 ) ) ;
#145441 = CARTESIAN_POINT ( 'NONE',  ( 2.161206213664386144, 0.3243885794495802721, -1.842051381961368639 ) ) ;
#145442 = CARTESIAN_POINT ( 'NONE',  ( 6.608665842073913943, 1.606649649811153990, -1.446306907624186344 ) ) ;
#145443 = ADVANCED_FACE ( 'NONE', ( #21615 ), #204646, .T. ) ;
#145445 = CARTESIAN_POINT ( 'NONE',  ( 6.727182134110202050, 7.629137130509070275, 2.410944104600750038 ) ) ;
#145444 = CARTESIAN_POINT ( 'NONE',  ( -0.02244404828157658613, 0.6916080914694566761, -2.270927585766496559 ) ) ;
#145446 = CARTESIAN_POINT ( 'NONE',  ( -0.6823417656250246877, -0.1989583329919109023, 1.181850606188755259 ) ) ;
#145447 = CARTESIAN_POINT ( 'NONE',  ( 2.350135150926917493, 0.8998847150011924922, -1.687291145760522859 ) ) ;
#145448 =( BOUNDED_CURVE ( )  B_SPLINE_CURVE ( 2, ( #40410, #25198, #92381, #120655, #104336, #137909, #158415, #58777, #26262 ),
 .UNSPECIFIED., .F., .T. ) 
 B_SPLINE_CURVE_WITH_KNOTS ( ( 3, 2, 2, 2, 3 ),
 ( 0.5446428571428572063, 0.5476190476190476719, 0.5535714285714286031, 0.5595238095238095344, 0.5625000000000000000 ),
 .UNSPECIFIED. ) 
 CURVE ( )  GEOMETRIC_REPRESENTATION_ITEM ( )  RATIONAL_B_SPLINE_CURVE ( ( 0.9330127018922194093, 0.9330127018922206306, 1.000000000000000000, 0.8660254037844387076, 1.000000000000000000, 0.8660254037844387076, 1.000000000000000000, 0.9330127018922194093, 0.9330127018922194093 ) ) 
 REPRESENTATION_ITEM ( '' )  );
#145449 = CARTESIAN_POINT ( 'NONE',  ( 3.783871084116468886, -0.8724064270978303393, 1.539809854060821603 ) ) ;
#145450 = CARTESIAN_POINT ( 'NONE',  ( 2.174333686202088334, 0.8191313854410250395, 1.728107290330855639 ) ) ;
#145451 = CARTESIAN_POINT ( 'NONE',  ( -5.742041750587549842, 6.657802449562273850, 1.199719254218450271 ) ) ;
#145453 = CARTESIAN_POINT ( 'NONE',  ( 5.343340938886254499, 0.3690371538600076273, -1.879538113519742204 ) ) ;
#145452 =( LENGTH_UNIT ( ) NAMED_UNIT ( * ) SI_UNIT ( .MILLI., .METRE. ) );
#145454 = CARTESIAN_POINT ( 'NONE',  ( 6.637161372131059167, -0.09511470475139816028, -1.967365288627285214 ) ) ;
#145455 = CARTESIAN_POINT ( 'NONE',  ( 0.7499999999999920064, 4.983333333333353821, 1.299038105676669330 ) ) ;
#145457 = EDGE_CURVE ( 'NONE', #212473, #186645, #174710, .T. ) ;
#145456 = CARTESIAN_POINT ( 'NONE',  ( 2.373420902723611725, -1.847293605357634982, -1.041186957106011723 ) ) ;
#145458 =( NAMED_UNIT ( * ) SI_UNIT ( $, .STERADIAN. ) SOLID_ANGLE_UNIT ( ) );
#145459 = CARTESIAN_POINT ( 'NONE',  ( 4.768341783539651324, -1.221614081569386334, 1.416756073533788518 ) ) ;
#145461 = ORIENTED_EDGE ( 'NONE', *, *, #57003, .F. ) ;
#145460 = CARTESIAN_POINT ( 'NONE',  ( 2.174178736149934732, -1.123764393468742684, 1.438770255985911684 ) ) ;
#145463 = CARTESIAN_POINT ( 'NONE',  ( 4.826264338009964128, 8.099924789650724932, 0.8724150771263041726 ) ) ;
#145462 = CARTESIAN_POINT ( 'NONE',  ( 4.143358556170802842, -1.920740624720223666, 1.086653567583625746 ) ) ;
#145464 = CARTESIAN_POINT ( 'NONE',  ( 0.6823417656249917140, 5.655208333674749177, 1.181850606188765695 ) ) ;
#145465 = CARTESIAN_POINT ( 'NONE',  ( 1.381380011782725958, -0.05272402391268657396, 2.062171479924046036 ) ) ;
#145466 = CARTESIAN_POINT ( 'NONE',  ( 4.788000803920411386, 8.737751371215816576, 1.040834085586084257E-14 ) ) ;
#145467 = CARTESIAN_POINT ( 'NONE',  ( -7.343712760096452463, 11.71941532008788833, -0.7998128361456291469 ) ) ;
#145468 = DIRECTION ( 'NONE',  ( 0.000000000000000000, 0.000000000000000000, -1.000000000000000000 ) ) ;
#145469 = CARTESIAN_POINT ( 'NONE',  ( 8.218213668177886788, 12.73966637951625813, 0.7998128361456462443 ) ) ;
#145470 = CARTESIAN_POINT ( 'NONE',  ( 1.466385952843407559, 3.464631544692571286, 0.3259651399136304639 ) ) ;
#145471 = CARTESIAN_POINT ( 'NONE',  ( 0.000000000000000000, 5.868705557303649734, -4.125226524755057689 ) ) ;
#145472 = CARTESIAN_POINT ( 'NONE',  ( 7.503511670520385479, 7.718794801887437274, 0.7998128361456281477 ) ) ;
#145473 = ORIENTED_EDGE ( 'NONE', *, *, #153202, .T. ) ;
#145474 = CARTESIAN_POINT ( 'NONE',  ( 3.877443546529443452, -0.1552652338182025915, 2.064615508632794860 ) ) ;
#145475 = CARTESIAN_POINT ( 'NONE',  ( 1.499999999999990896, 5.525000000000022560, 1.214306433183764966E-14 ) ) ;
#145476 = CARTESIAN_POINT ( 'NONE',  ( 2.108864864398530159, 1.603267699958549342, -1.450045708023157687 ) ) ;
#145477 = CARTESIAN_POINT ( 'NONE',  ( -6.190206388764837975, 6.963036634120459922, -0.8879648754220506035 ) ) ;
#145478 = CARTESIAN_POINT ( 'NONE',  ( 3.194014839594649491, 1.283080201803546538, 1.559715919771433867 ) ) ;
#145479 = CARTESIAN_POINT ( 'NONE',  ( 6.620655732516679493, 3.689697857139722981, 2.587825964709880910 ) ) ;
#145480 = ORIENTED_EDGE ( 'NONE', *, *, #157268, .T. ) ;
#145482 = CARTESIAN_POINT ( 'NONE',  ( 7.348156068926750883, 8.635565504245116486, -1.082531754730537976 ) ) ;
#145481 = CARTESIAN_POINT ( 'NONE',  ( 1.737499999999999378, -1.166666666666666519, -3.009438278150925683 ) ) ;
#145483 = CARTESIAN_POINT ( 'NONE',  ( -3.472296738431328134, 7.065113604896248845, 0.000000000000000000 ) ) ;
#145484 = CARTESIAN_POINT ( 'NONE',  ( 1.481658059775035952, -0.6748446255696785023, 1.900416712880992343 ) ) ;
#145485 = CARTESIAN_POINT ( 'NONE',  ( 6.339412547452306868, 0.8406370108028878851, -2.024118718474729128 ) ) ;
#145486 = B_SPLINE_CURVE_WITH_KNOTS ( 'NONE', 3,
 ( #102076, #83679, #118387, #134610, #184376, #133547, #20797, #35995 ),
 .UNSPECIFIED., .F., .F.,
 ( 4, 2, 2, 4 ),
 ( 0.000000000000000000, 0.0002034531274099183142, 0.0004069062548198371706, 0.0008138125096396707633 ),
 .UNSPECIFIED. ) ;
#145487 = CARTESIAN_POINT ( 'NONE',  ( 1.499999999999989120, 5.077083334016151639, -0.8660254037844323793 ) ) ;
#145488 = CARTESIAN_POINT ( 'NONE',  ( 4.939673314881130040, -1.814047719456039154, 0.6055163330952323397 ) ) ;
#145489 = CARTESIAN_POINT ( 'NONE',  ( -2.591579918506545344, 6.175260338232929413, 1.040834085586084257E-14 ) ) ;
#145490 = CARTESIAN_POINT ( 'NONE',  ( 5.734735788456138295, 8.673980272298743799, -1.082531754730537976 ) ) ;
#145492 = CARTESIAN_POINT ( 'NONE',  ( 2.460564738353550496, -1.930424690641812768, -0.5826366834433827080 ) ) ;
#145491 = CARTESIAN_POINT ( 'NONE',  ( -7.632877294369372123, 11.84884791016554573, 0.7216878364870458196 ) ) ;
#145493 = CARTESIAN_POINT ( 'NONE',  ( -8.012344526598182026E-15, 13.85937500034139447, -1.575800808251669460 ) ) ;
#145494 = CARTESIAN_POINT ( 'NONE',  ( -5.178288325776719603, 5.006034233019745372, 0.000000000000000000 ) ) ;
#145495 = CARTESIAN_POINT ( 'NONE',  ( 5.385687109042746279, 1.161108558237003985, 1.275598767315838211 ) ) ;
#145496 = CARTESIAN_POINT ( 'NONE',  ( -0.1394461523060988861, 1.283499747810852520, -2.524650647122913316 ) ) ;
#145497 = CARTESIAN_POINT ( 'NONE',  ( 10.07334494527360569, 10.85458331234846696, 0.000000000000000000 ) ) ;
#145498 = DIRECTION ( 'NONE',  ( 1.000000000000000000, -0.000000000000000000, 1.224646799147353207E-16 ) ) ;
#145499 = CARTESIAN_POINT ( 'NONE',  ( 4.891794496432329886, 4.601515088792824670, -0.7998128361456211532 ) ) ;
#145500 = LINE ( 'NONE', #142281, #171830 ) ;
#145501 = CARTESIAN_POINT ( 'NONE',  ( 0.9540663221972445207, -0.7486024665571254788, 1.930331157511067097 ) ) ;
#145502 = VERTEX_POINT ( 'NONE', #153796 ) ;
#145503 = CARTESIAN_POINT ( 'NONE',  ( 4.635318128526639825, -0.08385371298775616544, 1.809651570580686819 ) ) ;
#145504 = CARTESIAN_POINT ( 'NONE',  ( 5.662465432362883355, 6.635239754958710989, 1.199719254218451159 ) ) ;
#145505 = CARTESIAN_POINT ( 'NONE',  ( 6.855650617048432593, -7.357813805523310435, -6.855650617048458351 ) ) ;
#145506 = CARTESIAN_POINT ( 'NONE',  ( 6.340474544234134591, 1.036764729950395258, -1.485249760763515114 ) ) ;
#145507 = CARTESIAN_POINT ( 'NONE',  ( 5.736508391913541338, 6.825586224388162648, -1.082531754730548412 ) ) ;
#145508 = CARTESIAN_POINT ( 'NONE',  ( 10.72402378181932114, 9.913041843844986545, 5.394155308403613347 ) ) ;
#145509 = CARTESIAN_POINT ( 'NONE',  ( 3.433693710695666201, 0.9853049363134911420, -1.957518807868402044 ) ) ;
#145510 = ORIENTED_EDGE ( 'NONE', *, *, #209784, .F. ) ;
#145512 = CARTESIAN_POINT ( 'NONE',  ( 8.239604668803105270, 10.63595808506888396, -1.599625672291268286 ) ) ;
#145511 = CARTESIAN_POINT ( 'NONE',  ( 0.1683002474503410839, -0.8351952195557797998, -1.773497582445908938 ) ) ;
#145513 = CARTESIAN_POINT ( 'NONE',  ( 4.394081885627950435, -0.8225995951327015332, -1.730150695830068308 ) ) ;
#145514 = CARTESIAN_POINT ( 'NONE',  ( -1.499999999999995781, 8.627523663848663205, 2.580000000000011173 ) ) ;
#145515 = CARTESIAN_POINT ( 'NONE',  ( 0.6823417656249882723, 0.1760416670080894308, -1.181850606188749264 ) ) ;
#145517 = ORIENTED_EDGE ( 'NONE', *, *, #79248, .T. ) ;
#145516 = CARTESIAN_POINT ( 'NONE',  ( 4.351804120306567825, 8.020929207092235558, 1.040834085586084257E-14 ) ) ;
#145518 = CARTESIAN_POINT ( 'NONE',  ( -8.676855123066022912, 10.18571440074093282, -1.082531754730543971 ) ) ;
#145519 = CARTESIAN_POINT ( 'NONE',  ( 1.499129196564862987, 1.767075381950654611, -1.244890797856931686 ) ) ;
#145520 = CARTESIAN_POINT ( 'NONE',  ( -5.334207092333882017, 5.187939460669764635, 0.7998128361456281477 ) ) ;
#145521 = CARTESIAN_POINT ( 'NONE',  ( 4.797606254389322089, 6.690569611577942943, 1.599625672291268286 ) ) ;
#145522 = CARTESIAN_POINT ( 'NONE',  ( 2.485134345765506847, 1.670108983700506977, -0.7376146046164517855 ) ) ;
#145523 = CARTESIAN_POINT ( 'NONE',  ( -3.795392936821753604, 6.515376628678959392, -1.199719254218452047 ) ) ;
#145524 = CARTESIAN_POINT ( 'NONE',  ( 4.330939430599492823, 0.08983702179986637060, 1.823481399301420947 ) ) ;
#145525 = ADVANCED_FACE ( 'NONE', ( #154866 ), #57361, .T. ) ;
#145526 = CARTESIAN_POINT ( 'NONE',  ( 9.268416190114901809, 13.02345702987866893, 8.984174778941602213 ) ) ;
#145527 = CARTESIAN_POINT ( 'NONE',  ( 2.724755696555291262, 1.382288352666941389, -1.321784923088549446 ) ) ;
#145528 = ORIENTED_EDGE ( 'NONE', *, *, #148738, .F. ) ;
#145529 = CARTESIAN_POINT ( 'NONE',  ( 3.596117507753269660, 0.8876951776618343670, -1.758253228584506944 ) ) ;
#145530 = ORIENTED_EDGE ( 'NONE', *, *, #131165, .F. ) ;
#145531 = CARTESIAN_POINT ( 'NONE',  ( 6.181195893160847277, 1.342424930544680928, 1.403604608442722057 ) ) ;
#145532 = VERTEX_POINT ( 'NONE', #122456 ) ;
#145533 = CARTESIAN_POINT ( 'NONE',  ( -6.505933609711270549, 8.683618192786854095, -1.599625672291271394 ) ) ;
#145535 = CARTESIAN_POINT ( 'NONE',  ( 5.554972086574996304, 0.4156608669513594534, 2.079290889414136423 ) ) ;
#145534 = CARTESIAN_POINT ( 'NONE',  ( 6.801350335910821165, 7.963938809097990124, 1.199719254218452047 ) ) ;
#145536 = CARTESIAN_POINT ( 'NONE',  ( 4.921594424112039512, 4.706558014410965107, -0.4536484767114294936 ) ) ;
#145537 = CARTESIAN_POINT ( 'NONE',  ( 2.895058368816882499, -0.1428820475998151818, -1.907012587803847303 ) ) ;
#145538 = CARTESIAN_POINT ( 'NONE',  ( 4.834557559160812978, 6.939504195329335268, -1.414529171088283688 ) ) ;
#145539 = CARTESIAN_POINT ( 'NONE',  ( -15.75000000000000000, 13.79999999999999893, -3.200000000000001510 ) ) ;
#145540 = ORIENTED_EDGE ( 'NONE', *, *, #159892, .T. ) ;
#145541 = CARTESIAN_POINT ( 'NONE',  ( 4.146814880933355596, 5.931313009212638931, 1.599625672291261402 ) ) ;
#145542 = CIRCLE ( 'NONE', #79773, 0.08000000000000040412 ) ;
#145543 = CARTESIAN_POINT ( 'NONE',  ( 5.197907085625908863, 1.353584514550598472, 1.490229472901122065 ) ) ;
#145544 = FACE_BOUND ( 'NONE', #75808, .T. ) ;
#145545 = CARTESIAN_POINT ( 'NONE',  ( 6.340460056601358474, 1.806591233369018834, 0.2625940548972791611 ) ) ;
#145546 = CARTESIAN_POINT ( 'NONE',  ( 1.170471352854907776, -0.9292243337341490328, -1.850172451097586990 ) ) ;
#145547 = CARTESIAN_POINT ( 'NONE',  ( -8.866669273657352690, 9.446795028796142191, 0.7216878364870438212 ) ) ;
#145548 = CARTESIAN_POINT ( 'NONE',  ( -6.429665931644899857, 6.880618766637560668, 0.7446329532827021813 ) ) ;
#145549 = CARTESIAN_POINT ( 'NONE',  ( -0.3817069231124953776, 3.999999999999980904, -1.007084182327226296 ) ) ;
#145550 = DIRECTION ( 'NONE',  ( 1.000000000000000000, -0.000000000000000000, -0.000000000000000000 ) ) ;
#145551 = CARTESIAN_POINT ( 'NONE',  ( 6.205881626753210867, 8.263281202677319470, 1.599625672291281386 ) ) ;
#145552 = DIRECTION ( 'NONE',  ( 0.000000000000000000, 1.000000000000000000, 0.000000000000000000 ) ) ;
#145553 = CARTESIAN_POINT ( 'NONE',  ( -0.6823417656250003738, 10.96354166700806765, 1.181850606188754593 ) ) ;
#145554 = CARTESIAN_POINT ( 'NONE',  ( -3.653032323878261600, 6.349289246911547835, -1.199719254218452047 ) ) ;
#145556 = CARTESIAN_POINT ( 'NONE',  ( -6.474900878978163021, 9.711745571186627402, -1.199719254218452047 ) ) ;
#145555 = CARTESIAN_POINT ( 'NONE',  ( -11.94980361058168938, 10.90000000000000036, -1.100000000000000311 ) ) ;
#145557 = B_SPLINE_CURVE_WITH_KNOTS ( 'NONE', 3,
 ( #169628, #139284, #58013, #174990, #205314, #92679 ),
 .UNSPECIFIED., .F., .F.,
 ( 4, 2, 4 ),
 ( 0.001251957608719239451, 0.001565178843344208238, 0.001878400077969176810 ),
 .UNSPECIFIED. ) ;
#145558 = CARTESIAN_POINT ( 'NONE',  ( -5.901876940650454095, 5.779944607047298177, -0.7998128361456291469 ) ) ;
#145559 = CARTESIAN_POINT ( 'NONE',  ( 1.815371668717490339, -1.773540675419151169, -1.067758146248848128 ) ) ;
#145560 = CARTESIAN_POINT ( 'NONE',  ( 2.741944773236061117, 2.106750310803459758, -0.2105854985169057503 ) ) ;
#145561 = CARTESIAN_POINT ( 'NONE',  ( 6.564118927310645724, 10.80988918183778225, -0.7998128361456291469 ) ) ;
#145562 = CARTESIAN_POINT ( 'NONE',  ( 0.3788956605885618889, 3.049042541176487209, 0.4283520265745445199 ) ) ;
#145563 = CARTESIAN_POINT ( 'NONE',  ( 1.059349595761612584, 1.606854154984382443, 1.138435182648824373 ) ) ;
#145564 = CARTESIAN_POINT ( 'NONE',  ( 4.064005108223194718, 7.741596126659699983, 0.5534810405699239766 ) ) ;
#145565 = CARTESIAN_POINT ( 'NONE',  ( 4.148431816101584957, 6.823292304551739740, -1.082531754730548412 ) ) ;
#145567 = DIRECTION ( 'NONE',  ( 1.000000000000000000, 0.000000000000000000, -3.491481338843133355E-15 ) ) ;
#145566 = CARTESIAN_POINT ( 'NONE',  ( -3.475000000000000533, -3.529166666666667229, -2.006292185433948827 ) ) ;
#145568 = CARTESIAN_POINT ( 'NONE',  ( 2.642860430951101680, -1.905069302404806875, 1.274549645703947132 ) ) ;
#145570 = ADVANCED_FACE ( 'NONE', ( #43265 ), #154766, .T. ) ;
#145569 = CARTESIAN_POINT ( 'NONE',  ( 0.3283667639546791195, 1.746078182827022429, 0.5332771064449209897 ) ) ;
#145571 = CARTESIAN_POINT ( 'NONE',  ( 2.144650067465687648, 1.855875215511919363, 0.4610605321611755958 ) ) ;
#145572 = CARTESIAN_POINT ( 'NONE',  ( 6.099189001301251523, 8.209082816308541197, 1.599625672291268286 ) ) ;
#145573 = CARTESIAN_POINT ( 'NONE',  ( 5.938108092661121162, 9.871617174839238729, 1.040834085586084257E-14 ) ) ;
#145574 = CARTESIAN_POINT ( 'NONE',  ( 1.283448800676566970, 0.1440664973490720091, -2.008080635846798856 ) ) ;
#145575 = CARTESIAN_POINT ( 'NONE',  ( 2.377722661024490147, -1.904092233959910896, 0.4717398701708991893 ) ) ;
#145576 = CARTESIAN_POINT ( 'NONE',  ( -8.622095623286845978, 12.14652976288826913, 1.199719254218462483 ) ) ;
#145577 = CARTESIAN_POINT ( 'NONE',  ( -6.877010230629689858, 9.046264573866535486, 1.599625672291283607 ) ) ;
#145579 = EDGE_CURVE ( 'NONE', #60914, #64456, #6448, .T. ) ;
#145578 = CARTESIAN_POINT ( 'NONE',  ( -11.81838370251299075, 7.795688761918559528, -1.817169319662425009 ) ) ;
#145581 = CARTESIAN_POINT ( 'NONE',  ( 3.660817930519409291, -1.560716028760079421, -0.8345783561882027524 ) ) ;
#145580 = CARTESIAN_POINT ( 'NONE',  ( 4.664062431145298504, -1.365975323770602268, 1.582769587995744853 ) ) ;
#145582 = CARTESIAN_POINT ( 'NONE',  ( -9.898321827459227507, 16.00000000000624212, 7.924999999990193444 ) ) ;
#145584 = CARTESIAN_POINT ( 'NONE',  ( 6.439416457043729558, 0.8834936782941483768, -2.115358923741214259 ) ) ;
#145583 = CARTESIAN_POINT ( 'NONE',  ( 1.569538198872422630, 8.730447571941267526, -2.495330465741606218 ) ) ;
#145585 = CARTESIAN_POINT ( 'NONE',  ( 4.611116368171574109, -1.705915267380184286, 0.3434222965797654181 ) ) ;
#145586 = CARTESIAN_POINT ( 'NONE',  ( 9.901532256681887745, 10.44620914241737530, 0.000000000000000000 ) ) ;
#145587 = CARTESIAN_POINT ( 'NONE',  ( 1.499999999999987121, 4.045833333333359150, -0.8660254037844323793 ) ) ;
#145588 = CARTESIAN_POINT ( 'NONE',  ( 4.024493581903946016, 1.720846971656955438, -0.2109413284564972679 ) ) ;
#145589 = STYLED_ITEM ( 'NONE', ( #72280 ), #184056 ) ;
#145590 = CARTESIAN_POINT ( 'NONE',  ( 4.141221389272289777, -0.2091070545618961274, -2.161069556037761519 ) ) ;
#145591 = CARTESIAN_POINT ( 'NONE',  ( 2.849184837166184536, 6.475799410002530898, 0.7998128361456362523 ) ) ;
#145592 = CARTESIAN_POINT ( 'NONE',  ( 5.928922775424462444, -1.700964743930567513, 1.082835439959836776 ) ) ;
#145593 = CARTESIAN_POINT ( 'NONE',  ( 5.968750000000003553, 0.7852924748296689073, -1.895863743164208026 ) ) ;
#145594 = CARTESIAN_POINT ( 'NONE',  ( 0.7499999999999902300, 5.097916667349482012, -1.299038105676658228 ) ) ;
#145595 = CARTESIAN_POINT ( 'NONE',  ( 3.135679483595578798, -1.292546426170533058, -1.428565414989799054 ) ) ;
#145596 = CARTESIAN_POINT ( 'NONE',  ( 1.500000000000001332, 9.906250000682799595, 0.000000000000000000 ) ) ;
#145597 = CARTESIAN_POINT ( 'NONE',  ( 0.5576789645300848086, -1.902086909048054331, 1.147088156025797057 ) ) ;
#145598 = VERTEX_POINT ( 'NONE', #92019 ) ;
#145600 = AXIS2_PLACEMENT_3D ( 'NONE', #12716, #160057, #126576 ) ;
#145599 = CARTESIAN_POINT ( 'NONE',  ( 6.883263157960418432, 2.078485899884211285, 2.154856264959764012 ) ) ;
#145601 = CARTESIAN_POINT ( 'NONE',  ( 0.7499999999999885647, 3.566666666666690411, -1.299038105676658228 ) ) ;
#145602 = CARTESIAN_POINT ( 'NONE',  ( 6.498435699651741615, 6.475929825882159818, -0.7998128361456281477 ) ) ;
#145603 = CARTESIAN_POINT ( 'NONE',  ( 1.823182589357236205, 1.643363032943769397, -1.494666050352111863 ) ) ;
#145604 = CARTESIAN_POINT ( 'NONE',  ( 10.45358220256315285, 1.000000000000000888, -5.892590188894412329 ) ) ;
#145605 = CARTESIAN_POINT ( 'NONE',  ( 8.609064354997688184, 9.146255957026539818, 1.040834085586084257E-14 ) ) ;
#145606 = CARTESIAN_POINT ( 'NONE',  ( -1.115562610750309283E-14, 10.09375000068279782, 1.500000000000001554 ) ) ;
#145607 = EDGE_CURVE ( 'NONE', #112521, #188607, #59485, .T. ) ;
#145608 = CARTESIAN_POINT ( 'NONE',  ( 3.444653546323793947, 6.176457016423196222, 1.199719254218451159 ) ) ;
#145610 = CARTESIAN_POINT ( 'NONE',  ( 5.143062936040889710, -0.2492579690161021710, -2.047486851065055458 ) ) ;
#145609 = DIRECTION ( 'NONE',  ( 1.000000000000000000, 0.000000000000000000, 0.000000000000000000 ) ) ;
#145611 = DIRECTION ( 'NONE',  ( -0.6507913734559641616, -0.7592566023653004592, 0.000000000000000000 ) ) ;
#145612 = CARTESIAN_POINT ( 'NONE',  ( -2.767835915484202047, 6.380892334706859792, -0.7998128361456281477 ) ) ;
#145613 = DIRECTION ( 'NONE',  ( 1.000000000000000000, 0.000000000000000000, 0.000000000000000000 ) ) ;
#145614 = CARTESIAN_POINT ( 'NONE',  ( -1.402160292154681736E-14, 0.9468750003414176941, -1.575800808251659024 ) ) ;
#145615 = CARTESIAN_POINT ( 'NONE',  ( 6.819622122755134797, -1.814287395386984691, 0.4549875680220638596 ) ) ;
#145616 = CARTESIAN_POINT ( 'NONE',  ( 5.625553438129872852, 0.3468616029342861951, 1.698903693450015684 ) ) ;
#145617 = CARTESIAN_POINT ( 'NONE',  ( 5.583501753226309816, -0.7750115735715494836, 1.558442325393385897 ) ) ;
#145618 = CARTESIAN_POINT ( 'NONE',  ( 5.183294799126148433, 4.941598775268944976, 1.040834085586084257E-14 ) ) ;
#145619 = CARTESIAN_POINT ( 'NONE',  ( 3.070184882724129594, -1.363667385223182871, 1.842535374393680980 ) ) ;
#145620 = CARTESIAN_POINT ( 'NONE',  ( -0.6823417656250246877, -1.198958332991911790, 1.181850606188755259 ) ) ;
#145621 = B_SPLINE_CURVE_WITH_KNOTS ( 'NONE', 3,
 ( #75014, #186618, #157345, #124912 ),
 .UNSPECIFIED., .F., .F.,
 ( 4, 4 ),
 ( 1.810030818090551184E-16, 0.0003120095058623759956 ),
 .UNSPECIFIED. ) ;
#145622 = CARTESIAN_POINT ( 'NONE',  ( 1.218424693763892730, -0.04700249260505655335, 1.840701667592301138 ) ) ;
#145623 = LINE ( 'NONE', #144554, #84693 ) ;
#145624 = CARTESIAN_POINT ( 'NONE',  ( -10.71870444596734195, 5.124999999999999112, -5.395310463726811001 ) ) ;
#145625 = CARTESIAN_POINT ( 'NONE',  ( 2.432394421669949569, 1.770131964307398498, 0.4459858026567494194 ) ) ;
#145626 = CARTESIAN_POINT ( 'NONE',  ( 1.605704095283020605, -2.174604996184846595, 0.2706701637196773369 ) ) ;
#145627 = CARTESIAN_POINT ( 'NONE',  ( 7.652507619935904337, 14.87749650460459705, -8.827801418404110478 ) ) ;
#145628 = CARTESIAN_POINT ( 'NONE',  ( 4.278421442896533478, -1.214510211351152336, 1.720268157014235078 ) ) ;
#145629 = CARTESIAN_POINT ( 'NONE',  ( -6.028571859570855729, 10.18508426947466816, 0.000000000000000000 ) ) ;
#145630 = CARTESIAN_POINT ( 'NONE',  ( 7.649194982119887243, 14.87821958379617016, 8.830808698579634353 ) ) ;
#145631 =( BOUNDED_SURFACE ( )  B_SPLINE_SURFACE ( 1, 2, ( 
 ( #181248, #199619, #331, #114202, #33935, #180200, #149839, #66404, #1409, #32875, #80558, #197496, #98952, #31822, #165003, #196447, #211604, #113129, #81619, #16598, #161827, #166074, #15535, #198548, #212671, #95770, #50196, #100009, #64312, #30759, #116315, #182306, #130457, #48090, #132549, #117389, #147703, #213722, #162887, #183385, #14469, #131492, #67469, #82679, #187647, #135721, #34991, #167150, #202814, #22996, #171406, #39274, #19808, #52327, #203882, #137862, #151969, #3542, #71746, #138930, #53386, #69613, #134675, #122763, #204950, #2471, #89113, #37132, #105369, #201745, #101062, #18737, #54463, #155168, #6751, #56599, #136786, #119522, #72827, #84821, #150909, #186584, #120607, #68548, #200678, #118457, #184443, #36061, #154098, #102142, #168209, #85894, #185509, #103214, #4601, #38212, #104285, #169274, #20860, #86959, #170332, #153027, #70676, #21917, #88026, #5667, #55526, #121681, #194845, #108610, #95244, #12878, #25148, #107544, #161292, #213210, #91249, #64839, #90181, #190842, #78954, #24076, #163428, #13942, #172489, #146128, #40360, #156244, #106463, #140007, #177543, #212141, #47561, #29154, #188722, #7821, #30223, #73914, #42503, #189785, #206030, #57665, #123823, #145076, #41435, #157309, #173578, #211079, #113671, #62702, #179675, #147185, #128863, #15005, #96307, #207099, #129936, #58727, #31295, #162363, #97370, #46478, #8899, #112602, #178613, #124878, #80025, #74980, #141088, #63777, #195924, #81096, #196976, #201226, #133086, #19285, #33411, #130985, #85367, #17140, #99490, #32353, #132026, #199084, #4087, #181778, #180728, #165547, #51816, #151449, #48615, #36606, #168750, #98418, #164483, #149299, #116856, #50730, #200162, #135211, #84296, #114730, #3021, #198036, #34475, #182857, #16069, #100547, #880, #49666, #214247, #69089, #20353, #83217, #66946, #166620, #52867, #119002, #18212, #102692, #150381, #65878, #1952, #68013, #148245, #134154, #117934, #183928, #184980, #86438, #152503, #35540, #82153, #115789, #101617, #167684, #189271, #72297, #136269, #190325, #37689 ),
 ( #123307, #206579, #155713, #55011, #171962, #89660, #88588, #7296, #170884, #120078, #103766, #56078, #23553, #202289, #140567, #138404, #173040, #187129, #70158, #24623, #74462, #121160, #87514, #90730, #156793, #38758, #104839, #107016, #174122, #154645, #22477, #169817, #157861, #25695, #21404, #58208, #204423, #8379, #6227, #53941, #186054, #73374, #124367, #41984, #91803, #139479, #122235, #108093, #153579, #5148, #205509, #57140, #71225, #137340, #203359, #188194, #39830, #40910, #105938, #125422, #191388, #27841, #209770, #143775, #78712, #13710, #177301, #97134, #178374, #10510, #127573, #77653, #9454, #61410, #93938, #76584, #92868, #96068, #47318, #176239, #126493, #193541, #29983, #162121, #110231, #129699, #159979, #158914, #11581, #45183, #26766, #192456, #44110, #111297, #63543, #79783, #113431, #144840, #195681, #75526, #210846, #28915, #128634, #95000, #141637, #179438, #43054, #12642, #207646, #142695, #62472, #145896, #161046, #194600, #46244, #112361, #31058, #109167, #211906, #175180, #59266, #208705, #60332, #65635, #64606, #32108, #67756, #132836, #198840, #116607, #182600, #196740, #80862, #84041, #34224, #33167, #98193, #130746, #131783, #146952, #14771, #181539, #133907, #151194, #35282, #66689, #148002, #150129, #214013, #164241, #48380, #99249, #163187, #114493, #180489, #167436, #199913, #1702, #50486, #212967, #197787, #165297, #16892, #100296, #51560, #166363, #15829, #81915, #49424, #115544, #82973, #149046, #622, #17954, #117685, #183677, #101358, #19028, #36348, #85108, #2765, #68836, #134956, #200964, #52611, #118740, #184724, #38501, #120896, #138148, #139210, #55812, #103502, #20094, #202021, #168495, #136008, #203101, #87248, #54746, #4888, #3824, #169562, #104579, #190076, #153313, #152251, #70966, #23291, #56882, #102426, #8124, #140305, #69897, #53681, #186869, #88323, #22210, #171692, #106755, #121967, #86182, #123057, #21144, #5965, #170624, #119812, #154387, #72035, #137076, #185792, #189011, #206323, #204157, #187933, #39563, #40654, #172783, #105665, #74210, #89401 ) ),
 .UNSPECIFIED., .F., .F., .T. ) 
 B_SPLINE_SURFACE_WITH_KNOTS ( ( 2, 2 ),
 ( 3, 2, 2, 2, 2, 2, 2, 2, 2, 2, 2, 2, 2, 2, 2, 2, 2, 2, 2, 2, 2, 2, 2, 2, 2, 2, 2, 2, 2, 2, 2, 2, 2, 2, 2, 2, 2, 2, 2, 2, 2, 2, 2, 2, 2, 2, 2, 2, 2, 2, 2, 2, 2, 2, 2, 2, 2, 2, 2, 2, 2, 2, 2, 2, 2, 2, 2, 2, 2, 2, 2, 2, 2, 2, 2, 2, 2, 2, 2, 2, 2, 2, 2, 2, 2, 2, 2, 2, 2, 2, 2, 2, 2, 2, 2, 2, 2, 2, 2, 2, 2, 2, 2, 2, 2, 2, 2, 2, 2, 2, 2, 2, 2, 2, 2, 2, 2, 2, 2, 2, 3 ),
 ( 0.000000000000000000, 1.000000000000000000 ),
 ( 0.000000000000000000, 0.008333333333333333218, 0.01666666666666666644, 0.02500000000000000139, 0.03333333333333333287, 0.04166666666666666435, 0.05000000000000000278, 0.05833333333333333426, 0.06666666666666666574, 0.07499999999999999722, 0.08333333333333332871, 0.09166666666666666019, 0.1000000000000000056, 0.1083333333333333370, 0.1166666666666666685, 0.1250000000000000000, 0.1333333333333333315, 0.1416666666666666630, 0.1499999999999999944, 0.1583333333333333259, 0.1666666666666666574, 0.1749999999999999889, 0.1833333333333333204, 0.1916666666666666796, 0.2000000000000000111, 0.2083333333333333426, 0.2166666666666666741, 0.2250000000000000056, 0.2333333333333333370, 0.2416666666666666685, 0.2500000000000000000, 0.2583333333333333592, 0.2666666666666666630, 0.2750000000000000222, 0.2833333333333333259, 0.2916666666666666852, 0.2999999999999999889, 0.3083333333333333481, 0.3166666666666666519, 0.3250000000000000111, 0.3333333333333333148, 0.3416666666666666741, 0.3499999999999999778, 0.3583333333333333370, 0.3666666666666666408, 0.3750000000000000000, 0.3833333333333333592, 0.3916666666666666630, 0.4000000000000000222, 0.4083333333333333259, 0.4166666666666666852, 0.4249999999999999889, 0.4333333333333333481, 0.4416666666666666519, 0.4500000000000000111, 0.4583333333333333148, 0.4666666666666666741, 0.4749999999999999778, 0.4833333333333333370, 0.4916666666666666408, 0.5000000000000000000, 0.5083333333333333037, 0.5166666666666667185, 0.5250000000000000222, 0.5333333333333333259, 0.5416666666666666297, 0.5500000000000000444, 0.5583333333333333481, 0.5666666666666666519, 0.5749999999999999556, 0.5833333333333333703, 0.5916666666666666741, 0.5999999999999999778, 0.6083333333333332815, 0.6166666666666666963, 0.6250000000000000000, 0.6333333333333333037, 0.6416666666666667185, 0.6500000000000000222, 0.6583333333333333259, 0.6666666666666666297, 0.6750000000000000444, 0.6833333333333333481, 0.6916666666666666519, 0.6999999999999999556, 0.7083333333333333703, 0.7166666666666666741, 0.7249999999999999778, 0.7333333333333332815, 0.7416666666666666963, 0.7500000000000000000, 0.7583333333333333037, 0.7666666666666667185, 0.7750000000000000222, 0.7833333333333333259, 0.7916666666666666297, 0.8000000000000000444, 0.8083333333333333481, 0.8166666666666666519, 0.8249999999999999556, 0.8333333333333333703, 0.8416666666666666741, 0.8499999999999999778, 0.8583333333333332815, 0.8666666666666666963, 0.8750000000000000000, 0.8833333333333333037, 0.8916666666666667185, 0.9000000000000000222, 0.9083333333333333259, 0.9166666666666666297, 0.9250000000000000444, 0.9333333333333333481, 0.9416666666666666519, 0.9499999999999999556, 0.9583333333333333703, 0.9666666666666666741, 0.9749999999999999778, 0.9833333333333332815, 0.9916666666666666963, 1.000000000000000000 ),
 .UNSPECIFIED. ) 
 GEOMETRIC_REPRESENTATION_ITEM ( )  RATIONAL_B_SPLINE_SURFACE ( (
 ( 1.000000000000000000, 0.8660254037844387076, 1.000000000000000000, 0.8660254037844387076, 1.000000000000000000, 0.8660254037844387076, 1.000000000000000000, 0.8660254037844387076, 1.000000000000000000, 0.8660254037844387076, 1.000000000000000000, 0.8660254037844387076, 1.000000000000000000, 0.8660254037844387076, 1.000000000000000000, 0.8660254037844387076, 1.000000000000000000, 0.8660254037844387076, 1.000000000000000000, 0.8660254037844387076, 1.000000000000000000, 0.8660254037844387076, 1.000000000000000000, 0.8660254037844387076, 1.000000000000000000, 0.8660254037844387076, 1.000000000000000000, 0.8660254037844387076, 1.000000000000000000, 0.8660254037844387076, 1.000000000000000000, 0.8660254037844387076, 1.000000000000000000, 0.8660254037844387076, 1.000000000000000000, 0.8660254037844387076, 1.000000000000000000, 0.8660254037844387076, 1.000000000000000000, 0.8660254037844387076, 1.000000000000000000, 0.8660254037844387076, 1.000000000000000000, 0.8660254037844387076, 1.000000000000000000, 0.8660254037844387076, 1.000000000000000000, 0.8660254037844387076, 1.000000000000000000, 0.8660254037844387076, 1.000000000000000000, 0.8660254037844387076, 1.000000000000000000, 0.8660254037844387076, 1.000000000000000000, 0.8660254037844387076, 1.000000000000000000, 0.8660254037844387076, 1.000000000000000000, 0.8660254037844387076, 1.000000000000000000, 0.8660254037844387076, 1.000000000000000000, 0.8660254037844387076, 1.000000000000000000, 0.8660254037844387076, 1.000000000000000000, 0.8660254037844387076, 1.000000000000000000, 0.8660254037844387076, 1.000000000000000000, 0.8660254037844387076, 1.000000000000000000, 0.8660254037844387076, 1.000000000000000000, 0.8660254037844387076, 1.000000000000000000, 0.8660254037844387076, 1.000000000000000000, 0.8660254037844387076, 1.000000000000000000, 0.8660254037844387076, 1.000000000000000000, 0.8660254037844387076, 1.000000000000000000, 0.8660254037844387076, 1.000000000000000000, 0.8660254037844387076, 1.000000000000000000, 0.8660254037844387076, 1.000000000000000000, 0.8660254037844387076, 1.000000000000000000, 0.8660254037844387076, 1.000000000000000000, 0.8660254037844387076, 1.000000000000000000, 0.8660254037844387076, 1.000000000000000000, 0.8660254037844387076, 1.000000000000000000, 0.8660254037844387076, 1.000000000000000000, 0.8660254037844387076, 1.000000000000000000, 0.8660254037844387076, 1.000000000000000000, 0.8660254037844387076, 1.000000000000000000, 0.8660254037844387076, 1.000000000000000000, 0.8660254037844387076, 1.000000000000000000, 0.8660254037844387076, 1.000000000000000000, 0.8660254037844387076, 1.000000000000000000, 0.8660254037844387076, 1.000000000000000000, 0.8660254037844387076, 1.000000000000000000, 0.8660254037844387076, 1.000000000000000000, 0.8660254037844387076, 1.000000000000000000, 0.8660254037844387076, 1.000000000000000000, 0.8660254037844387076, 1.000000000000000000, 0.8660254037844387076, 1.000000000000000000, 0.8660254037844387076, 1.000000000000000000, 0.8660254037844387076, 1.000000000000000000, 0.8660254037844387076, 1.000000000000000000, 0.8660254037844387076, 1.000000000000000000, 0.8660254037844387076, 1.000000000000000000, 0.8660254037844387076, 1.000000000000000000, 0.8660254037844387076, 1.000000000000000000, 0.8660254037844387076, 1.000000000000000000, 0.8660254037844387076, 1.000000000000000000, 0.8660254037844387076, 1.000000000000000000, 0.8660254037844387076, 1.000000000000000000, 0.8660254037844387076, 1.000000000000000000, 0.8660254037844387076, 1.000000000000000000, 0.8660254037844387076, 1.000000000000000000, 0.8660254037844387076, 1.000000000000000000, 0.8660254037844387076, 1.000000000000000000, 0.8660254037844387076, 1.000000000000000000, 0.8660254037844387076, 1.000000000000000000, 0.8660254037844387076, 1.000000000000000000, 0.8660254037844387076, 1.000000000000000000, 0.8660254037844387076, 1.000000000000000000, 0.8660254037844387076, 1.000000000000000000, 0.8660254037844387076, 1.000000000000000000, 0.8660254037844387076, 1.000000000000000000, 0.8660254037844387076, 1.000000000000000000, 0.8660254037844387076, 1.000000000000000000, 0.8660254037844387076, 1.000000000000000000, 0.8660254037844387076, 1.000000000000000000, 0.8660254037844387076, 1.000000000000000000, 0.8660254037844387076, 1.000000000000000000, 0.8660254037844387076, 1.000000000000000000, 0.8660254037844387076, 1.000000000000000000, 0.8660254037844387076, 1.000000000000000000, 0.8660254037844387076, 1.000000000000000000, 0.8660254037844387076, 1.000000000000000000, 0.8660254037844387076, 1.000000000000000000, 0.8660254037844387076, 1.000000000000000000, 0.8660254037844387076, 1.000000000000000000, 0.8660254037844387076, 1.000000000000000000, 0.8660254037844387076, 1.000000000000000000, 0.8660254037844387076, 1.000000000000000000, 0.8660254037844387076, 1.000000000000000000, 0.8660254037844387076, 1.000000000000000000, 0.8660254037844387076, 1.000000000000000000, 0.8660254037844387076, 1.000000000000000000, 0.8660254037844387076, 1.000000000000000000, 0.8660254037844387076, 1.000000000000000000, 0.8660254037844387076, 1.000000000000000000, 0.8660254037844387076, 1.000000000000000000, 0.8660254037844387076, 1.000000000000000000, 0.8660254037844387076, 1.000000000000000000, 0.8660254037844387076, 1.000000000000000000, 0.8660254037844387076, 1.000000000000000000, 0.8660254037844387076, 1.000000000000000000, 0.8660254037844387076, 1.000000000000000000),
 ( 1.000000000000000000, 0.8660254037844387076, 1.000000000000000000, 0.8660254037844387076, 1.000000000000000000, 0.8660254037844387076, 1.000000000000000000, 0.8660254037844387076, 1.000000000000000000, 0.8660254037844387076, 1.000000000000000000, 0.8660254037844387076, 1.000000000000000000, 0.8660254037844387076, 1.000000000000000000, 0.8660254037844387076, 1.000000000000000000, 0.8660254037844387076, 1.000000000000000000, 0.8660254037844387076, 1.000000000000000000, 0.8660254037844387076, 1.000000000000000000, 0.8660254037844387076, 1.000000000000000000, 0.8660254037844387076, 1.000000000000000000, 0.8660254037844387076, 1.000000000000000000, 0.8660254037844387076, 1.000000000000000000, 0.8660254037844387076, 1.000000000000000000, 0.8660254037844387076, 1.000000000000000000, 0.8660254037844387076, 1.000000000000000000, 0.8660254037844387076, 1.000000000000000000, 0.8660254037844387076, 1.000000000000000000, 0.8660254037844387076, 1.000000000000000000, 0.8660254037844387076, 1.000000000000000000, 0.8660254037844387076, 1.000000000000000000, 0.8660254037844387076, 1.000000000000000000, 0.8660254037844387076, 1.000000000000000000, 0.8660254037844387076, 1.000000000000000000, 0.8660254037844387076, 1.000000000000000000, 0.8660254037844387076, 1.000000000000000000, 0.8660254037844387076, 1.000000000000000000, 0.8660254037844387076, 1.000000000000000000, 0.8660254037844387076, 1.000000000000000000, 0.8660254037844387076, 1.000000000000000000, 0.8660254037844387076, 1.000000000000000000, 0.8660254037844387076, 1.000000000000000000, 0.8660254037844387076, 1.000000000000000000, 0.8660254037844387076, 1.000000000000000000, 0.8660254037844387076, 1.000000000000000000, 0.8660254037844387076, 1.000000000000000000, 0.8660254037844387076, 1.000000000000000000, 0.8660254037844387076, 1.000000000000000000, 0.8660254037844387076, 1.000000000000000000, 0.8660254037844387076, 1.000000000000000000, 0.8660254037844387076, 1.000000000000000000, 0.8660254037844387076, 1.000000000000000000, 0.8660254037844387076, 1.000000000000000000, 0.8660254037844387076, 1.000000000000000000, 0.8660254037844387076, 1.000000000000000000, 0.8660254037844387076, 1.000000000000000000, 0.8660254037844387076, 1.000000000000000000, 0.8660254037844387076, 1.000000000000000000, 0.8660254037844387076, 1.000000000000000000, 0.8660254037844387076, 1.000000000000000000, 0.8660254037844387076, 1.000000000000000000, 0.8660254037844387076, 1.000000000000000000, 0.8660254037844387076, 1.000000000000000000, 0.8660254037844387076, 1.000000000000000000, 0.8660254037844387076, 1.000000000000000000, 0.8660254037844387076, 1.000000000000000000, 0.8660254037844387076, 1.000000000000000000, 0.8660254037844387076, 1.000000000000000000, 0.8660254037844387076, 1.000000000000000000, 0.8660254037844387076, 1.000000000000000000, 0.8660254037844387076, 1.000000000000000000, 0.8660254037844387076, 1.000000000000000000, 0.8660254037844387076, 1.000000000000000000, 0.8660254037844387076, 1.000000000000000000, 0.8660254037844387076, 1.000000000000000000, 0.8660254037844387076, 1.000000000000000000, 0.8660254037844387076, 1.000000000000000000, 0.8660254037844387076, 1.000000000000000000, 0.8660254037844387076, 1.000000000000000000, 0.8660254037844387076, 1.000000000000000000, 0.8660254037844387076, 1.000000000000000000, 0.8660254037844387076, 1.000000000000000000, 0.8660254037844387076, 1.000000000000000000, 0.8660254037844387076, 1.000000000000000000, 0.8660254037844387076, 1.000000000000000000, 0.8660254037844387076, 1.000000000000000000, 0.8660254037844387076, 1.000000000000000000, 0.8660254037844387076, 1.000000000000000000, 0.8660254037844387076, 1.000000000000000000, 0.8660254037844387076, 1.000000000000000000, 0.8660254037844387076, 1.000000000000000000, 0.8660254037844387076, 1.000000000000000000, 0.8660254037844387076, 1.000000000000000000, 0.8660254037844387076, 1.000000000000000000, 0.8660254037844387076, 1.000000000000000000, 0.8660254037844387076, 1.000000000000000000, 0.8660254037844387076, 1.000000000000000000, 0.8660254037844387076, 1.000000000000000000, 0.8660254037844387076, 1.000000000000000000, 0.8660254037844387076, 1.000000000000000000, 0.8660254037844387076, 1.000000000000000000, 0.8660254037844387076, 1.000000000000000000, 0.8660254037844387076, 1.000000000000000000, 0.8660254037844387076, 1.000000000000000000, 0.8660254037844387076, 1.000000000000000000, 0.8660254037844387076, 1.000000000000000000, 0.8660254037844387076, 1.000000000000000000, 0.8660254037844387076, 1.000000000000000000, 0.8660254037844387076, 1.000000000000000000, 0.8660254037844387076, 1.000000000000000000, 0.8660254037844387076, 1.000000000000000000, 0.8660254037844387076, 1.000000000000000000, 0.8660254037844387076, 1.000000000000000000, 0.8660254037844387076, 1.000000000000000000, 0.8660254037844387076, 1.000000000000000000, 0.8660254037844387076, 1.000000000000000000, 0.8660254037844387076, 1.000000000000000000, 0.8660254037844387076, 1.000000000000000000, 0.8660254037844387076, 1.000000000000000000, 0.8660254037844387076, 1.000000000000000000, 0.8660254037844387076, 1.000000000000000000, 0.8660254037844387076, 1.000000000000000000, 0.8660254037844387076, 1.000000000000000000, 0.8660254037844387076, 1.000000000000000000, 0.8660254037844387076, 1.000000000000000000, 0.8660254037844387076, 1.000000000000000000, 0.8660254037844387076, 1.000000000000000000, 0.8660254037844387076, 1.000000000000000000) ) ) 
 REPRESENTATION_ITEM ( '' )  SURFACE ( )  );
#145632 = CARTESIAN_POINT ( 'NONE',  ( 1.029834584532058672, 1.995790600324919506, -0.5504719462680053299 ) ) ;
#145633 = CARTESIAN_POINT ( 'NONE',  ( 5.250031796989762967, 7.148123067953287446, 1.599625672291267398 ) ) ;
#145634 = CARTESIAN_POINT ( 'NONE',  ( 1.360316468749979801, -0.9322916663252904801, -0.7853790794159041244 ) ) ;
#145635 = CARTESIAN_POINT ( 'NONE',  ( 4.055424778641623540, -1.844328037693225397, 1.046277804987456372 ) ) ;
#145636 = CONTEXT_DEPENDENT_SHAPE_REPRESENTATION ( #85148, #9019 ) ;
#145637 = CARTESIAN_POINT ( 'NONE',  ( 6.129513044595952032, -1.717388127611047421, 0.6198453807191862674 ) ) ;
#145638 = ORIENTED_EDGE ( 'NONE', *, *, #115408, .T. ) ;
#145639 = CARTESIAN_POINT ( 'NONE',  ( -5.712781623311813384, 7.758274208654143855, -1.599625672291271394 ) ) ;
#145640 = CARTESIAN_POINT ( 'NONE',  ( 9.073431116043567002, 11.60875560684942265, -1.599625672291262513 ) ) ;
#145641 = CARTESIAN_POINT ( 'NONE',  ( 7.146556367734776316, 7.510272981878305387, 0.7216878364870267237 ) ) ;
#145642 = CARTESIAN_POINT ( 'NONE',  ( 3.475000000000000533, -2.260416665710749839, 2.006292185433948827 ) ) ;
#145643 = CARTESIAN_POINT ( 'NONE',  ( -6.227272627378437342, 6.159572908229946187, -0.7998128361456291469 ) ) ;
#145644 = CARTESIAN_POINT ( 'NONE',  ( 6.539320575229233157, 0.001224430076711413356, 2.103502572931112091 ) ) ;
#145645 = CARTESIAN_POINT ( 'NONE',  ( 1.325372091284286569, -0.05194335737490791277, 2.105495032795675847 ) ) ;
#145646 = CARTESIAN_POINT ( 'NONE',  ( -5.655686355556086120, 6.627330832017406692, 1.199719254218452935 ) ) ;
#145647 = CARTESIAN_POINT ( 'NONE',  ( 9.348510611822643313, 10.86534945433664134, 1.199719254218453823 ) ) ;
#145648 = CARTESIAN_POINT ( 'NONE',  ( 5.365987026107917224, -1.852166562183876986, 0.1801111341232768115 ) ) ;
#145649 = CARTESIAN_POINT ( 'NONE',  ( 6.753933077901968396, 11.03133902419432566, 0.7998128361456462443 ) ) ;
#145650 = CARTESIAN_POINT ( 'NONE',  ( 4.887048565581556758, 4.918228951918932168, -0.7329281915080710919 ) ) ;
#145651 = CARTESIAN_POINT ( 'NONE',  ( -3.902768115887413014, 5.646591783325653147, -1.599625672291283607 ) ) ;
#145652 = CARTESIAN_POINT ( 'NONE',  ( -9.978437869977959451, 10.74385839117019614, -0.7216878364870267237 ) ) ;
#145654 = CARTESIAN_POINT ( 'NONE',  ( 2.066782613880484565, 1.455849762852476248, -1.315278764014264912 ) ) ;
#145653 = CARTESIAN_POINT ( 'NONE',  ( -8.193204901359996128, 8.453160561208463264, 1.040834085586084257E-14 ) ) ;
#145655 = CARTESIAN_POINT ( 'NONE',  ( 0.5851287433712646369, -0.2658872486876809327, -2.145209338178376335 ) ) ;
#145657 = CARTESIAN_POINT ( 'NONE',  ( -6.087928554039494067, 6.027116558704463500, 0.4103310871990673014 ) ) ;
#145656 = CARTESIAN_POINT ( 'NONE',  ( -6.934069218746458318, 7.054445274817795486, -0.7998128361456362523 ) ) ;
#145658 = CARTESIAN_POINT ( 'NONE',  ( -1.364683531250014514, 0.7385416670080887647, -0.7879004041258289570 ) ) ;
#145659 = CARTESIAN_POINT ( 'NONE',  ( 3.145509197426650694, -0.1243275703598344523, -1.729419848027229367 ) ) ;
#145660 = CARTESIAN_POINT ( 'NONE',  ( 2.501564275351343181, -0.6656319730054968131, -1.608207657179961947 ) ) ;
#145661 = CARTESIAN_POINT ( 'NONE',  ( 6.805829924380105034, 9.923590097543378619, 1.082531754730558626 ) ) ;
#145662 = CARTESIAN_POINT ( 'NONE',  ( -10.44369227015510404, 5.112964020592957404, 5.232143560358708534 ) ) ;
#145663 = CARTESIAN_POINT ( 'NONE',  ( 2.249358885376837591, -1.653154358101496246, -1.230164295365917537 ) ) ;
#145664 = CARTESIAN_POINT ( 'NONE',  ( 0.7024996975148189993, -1.423740904080775138, -1.427721366232127753 ) ) ;
#145665 = CARTESIAN_POINT ( 'NONE',  ( 6.925078400183553029, 2.042159606913606762, 2.349846261904017464 ) ) ;
#145666 = CARTESIAN_POINT ( 'NONE',  ( -4.146814880933400005, 5.931313009212638931, 1.599625672291270506 ) ) ;
#145667 = COLOUR_RGB ( '', 0.40784314, 0.44705882, 0.49803922) ;
#145668 = CARTESIAN_POINT ( 'NONE',  ( 1.006637970050362929, 1.494420418981519338, -1.285951363188575058 ) ) ;
#145670 = CARTESIAN_POINT ( 'NONE',  ( -4.936577329151611515, 7.813071746435248599, 1.082531754730549967 ) ) ;
#145669 = CARTESIAN_POINT ( 'NONE',  ( 6.152599605923961157, 1.892562589925715466, 0.2737767527046449101 ) ) ;
#145671 = CARTESIAN_POINT ( 'NONE',  ( -7.255021596644144921, 7.636815748939187465, 0.7216878364870317197 ) ) ;
#145672 = CARTESIAN_POINT ( 'NONE',  ( 4.895902867866261055, 4.884510565364971413, -0.7216878364870458196 ) ) ;
#145673 = CARTESIAN_POINT ( 'NONE',  ( -5.772739544368596043, 9.956889578397179363, -0.7998128361456362523 ) ) ;
#145674 = CARTESIAN_POINT ( 'NONE',  ( 0.7154971248738207779, 1.652399868344236245, 1.161036454668294304 ) ) ;
#145675 = CARTESIAN_POINT ( 'NONE',  ( 3.334942598837264960, 6.834590765378040444, 1.214306433183764966E-14 ) ) ;
#145676 = CARTESIAN_POINT ( 'NONE',  ( 4.278580467222413475, -1.332036844872594994, 1.884138376372360479 ) ) ;
#145677 = CARTESIAN_POINT ( 'NONE',  ( 5.564887814092526419, 1.486691789297951871, -1.280227714881218892 ) ) ;
#145678 = CARTESIAN_POINT ( 'NONE',  ( 1.832786370036399326, -1.861117592713131819, -0.6203919267877275878 ) ) ;
#145679 = CARTESIAN_POINT ( 'NONE',  ( 8.992082194361556091, 11.51384853155376220, 1.599625672291279388 ) ) ;
#145680 = CARTESIAN_POINT ( 'NONE',  ( -0.06968618116158857567, -1.560424145883563929, -1.276814929289785239 ) ) ;
#145681 = ORIENTED_EDGE ( 'NONE', *, *, #7153, .T. ) ;
#145682 = CARTESIAN_POINT ( 'NONE',  ( 1.552129107922173068, 1.093532845977844170, 1.812997832068358850 ) ) ;
#145684 = CARTESIAN_POINT ( 'NONE',  ( -7.857113714319432063, 9.125386407249497012, 1.199719254218462483 ) ) ;
#145683 = CARTESIAN_POINT ( 'NONE',  ( -3.110706179331648169, 5.716575411607132118, 1.199719254218462483 ) ) ;
#145685 = CARTESIAN_POINT ( 'NONE',  ( 1.218424693763892730, -0.04700249260505655335, 1.840701667592301138 ) ) ;
#145686 = ORIENTED_EDGE ( 'NONE', *, *, #146979, .T. ) ;
#145687 = CARTESIAN_POINT ( 'NONE',  ( 4.012681996134721096, 0.7761599038508348869, 2.027777647250021076 ) ) ;
#145688 = CARTESIAN_POINT ( 'NONE',  ( 11.46766370916821742, 8.380394332300772575, 3.382753340440862289 ) ) ;
#145689 = CARTESIAN_POINT ( 'NONE',  ( 2.232824136269210502, 1.381628265877183903, -1.608862310199298928 ) ) ;
#145690 = CARTESIAN_POINT ( 'NONE',  ( 0.7499999999999920064, 5.014583334016150751, 1.299038105676669330 ) ) ;
#145691 = CARTESIAN_POINT ( 'NONE',  ( 8.239604668803105270, 10.63595808506888396, -1.599625672291268286 ) ) ;
#145692 = CARTESIAN_POINT ( 'NONE',  ( -0.6125000000000105915, 0.5416666666666625218, 1.060881119635880721 ) ) ;
#145693 = CARTESIAN_POINT ( 'NONE',  ( 3.145831276397454079, 0.7450406991881215468, -1.921561753228885783 ) ) ;
#145694 = CIRCLE ( 'NONE', #169754, 11.92000000000000171 ) ;
#145696 = CARTESIAN_POINT ( 'NONE',  ( 0.6086344939593493208, -0.2706599535906920040, 1.821105742621460744 ) ) ;
#145695 = CARTESIAN_POINT ( 'NONE',  ( -8.097244055859620815, 10.46987070330147063, -1.599625672291263179 ) ) ;
#145697 = CARTESIAN_POINT ( 'NONE',  ( 0.6823417656249917140, 3.342708333674754506, 1.181850606188765695 ) ) ;
#145698 = CARTESIAN_POINT ( 'NONE',  ( 1.424678450204434510, 3.957108020605633047, 0.4927150456334776774 ) ) ;
#145699 = CARTESIAN_POINT ( 'NONE',  ( 0.1533209562146371774, -1.769702838771534559, 1.318327933512997152 ) ) ;
#145700 = CARTESIAN_POINT ( 'NONE',  ( 2.601149388587006950, 1.818552668380982951, -1.345706882341807242 ) ) ;
#145701 = CARTESIAN_POINT ( 'NONE',  ( -7.836249599018719536, 12.08611559892311504, 0.7216878364870478180 ) ) ;
#145702 = CARTESIAN_POINT ( 'NONE',  ( 2.654344044762357413, 1.798353594787518217, 0.2176890031466270636 ) ) ;
#145703 = B_SPLINE_CURVE_WITH_KNOTS ( 'NONE', 3,
 ( #180634, #179580, #96214, #182758 ),
 .UNSPECIFIED., .F., .F.,
 ( 4, 4 ),
 ( 0.000000000000000000, 0.0004065497138311910700 ),
 .UNSPECIFIED. ) ;
#145704 = CARTESIAN_POINT ( 'NONE',  ( 2.448326871961825191, -1.317826014703428639, 1.390694818219958107 ) ) ;
#145705 = CARTESIAN_POINT ( 'NONE',  ( 3.402844027952243167, 0.5003511028610057032, 2.008882729757965890 ) ) ;
#145706 = CARTESIAN_POINT ( 'NONE',  ( -1.402160292154681736E-14, 1.759375000341421469, -1.575800808251659024 ) ) ;
#145707 = EDGE_CURVE ( 'NONE', #96482, #122450, #42198, .T. ) ;
#145708 = CARTESIAN_POINT ( 'NONE',  ( 2.008605748815388559, 1.462198227207864853, -1.322556311574287768 ) ) ;
#145709 = CARTESIAN_POINT ( 'NONE',  ( 6.111935756226617222, -1.911612718183410387, 0.2385651428990897549 ) ) ;
#145710 = CARTESIAN_POINT ( 'NONE',  ( 3.186256133050053840, -1.842714570631575510, -0.3211874441736498054 ) ) ;
#145712 = CARTESIAN_POINT ( 'NONE',  ( 4.722521264130603136, 8.336029038342307018, -0.7037175076533495055 ) ) ;
#145711 = CARTESIAN_POINT ( 'NONE',  ( 1.348709242277994269, 2.305235852375675076, 0.1091458774659745806 ) ) ;
#145713 = CARTESIAN_POINT ( 'NONE',  ( 2.699463648093935575, -1.376791127151571592, -1.252357159445316670 ) ) ;
#145714 = CARTESIAN_POINT ( 'NONE',  ( -1.364683531249997417, 3.509375000341423245, 1.214306433183764966E-14 ) ) ;
#145715 = CARTESIAN_POINT ( 'NONE',  ( 5.371554553765571782, -0.3061699256626281840, 2.039728424269163121 ) ) ;
#145716 = CARTESIAN_POINT ( 'NONE',  ( -4.062639585589296942, 7.891496616496157301, 0.7998128361456341429 ) ) ;
#145717 = CARTESIAN_POINT ( 'NONE',  ( 7.786460292950004636, 7.978625184730144149, 1.040834085586084257E-14 ) ) ;
#145718 = CARTESIAN_POINT ( 'NONE',  ( -1.422919657202418087, 3.798112692695652104, 0.5004438751493026638 ) ) ;
#145719 = CARTESIAN_POINT ( 'NONE',  ( 5.842829903504588529, 0.4074447676574670107, 2.065989314711280667 ) ) ;
#145720 = CARTESIAN_POINT ( 'NONE',  ( 0.6823417656249899377, 3.155208333674754062, 1.181850606188765695 ) ) ;
#145721 = CARTESIAN_POINT ( 'NONE',  ( 5.554052124568396920, 2.159397089200214559, -0.09991998142631912383 ) ) ;
#145722 = CARTESIAN_POINT ( 'NONE',  ( 6.287761640583830136, 1.932026593981367002, -0.5884565063561957299 ) ) ;
#145723 = CARTESIAN_POINT ( 'NONE',  ( -1.364683531250014514, -0.7614583329919104582, -0.7879004041258359514 ) ) ;
#145724 = CARTESIAN_POINT ( 'NONE',  ( -4.880572111239580124, 7.677455982212699759, 1.082531754730560403 ) ) ;
#145727 = CARTESIAN_POINT ( 'NONE',  ( 4.039966587192257208, 6.696749537490852333, 1.082531754730558626 ) ) ;
#145726 = CARTESIAN_POINT ( 'NONE',  ( 3.285556943750000070, -0.2843749995220419269, 0.000000000000000000 ) ) ;
#145725 = CARTESIAN_POINT ( 'NONE',  ( 6.658989722967328717, 7.797851427330578566, 1.199719254218452935 ) ) ;
#145728 = CARTESIAN_POINT ( 'NONE',  ( -5.061990249855848667, 6.999017606288844284, -1.599625672291271394 ) ) ;
#145729 = CARTESIAN_POINT ( 'NONE',  ( 4.645720405014278853, 1.993893748393640086, -0.3006458143828410479 ) ) ;
#145730 = CARTESIAN_POINT ( 'NONE',  ( -7.178152263431422320, 10.46192917639026554, 1.199719254218453823 ) ) ;
#145732 = CARTESIAN_POINT ( 'NONE',  ( -5.926322542504860458, 9.928143709648733051, -0.7216878364870338292 ) ) ;
#145731 = CARTESIAN_POINT ( 'NONE',  ( -8.514157279702017078, 12.87700789305364069, -0.7216878364870267237 ) ) ;
#145733 = CARTESIAN_POINT ( 'NONE',  ( -0.6823417656249969321, 5.467708333674756283, -1.181850606188749264 ) ) ;
#145735 = CARTESIAN_POINT ( 'NONE',  ( 1.364683531249997417, 9.234375000341396245, 2.602085213965210642E-15 ) ) ;
#145734 = CARTESIAN_POINT ( 'NONE',  ( 5.647404790089923132, -1.701416311724871067, -1.333359258283283166 ) ) ;
#145736 = DIRECTION ( 'NONE',  ( 0.000000000000000000, -1.000000000000000000, 0.000000000000000000 ) ) ;
#145737 = CARTESIAN_POINT ( 'NONE',  ( -11.38917015317169579, 6.531398568769805735, 3.785358204000274007 ) ) ;
#145739 = CARTESIAN_POINT ( 'NONE',  ( 5.642203898613793456, 0.8197873783117490820, 1.842442240159094080 ) ) ;
#145738 = CARTESIAN_POINT ( 'NONE',  ( -5.029711800545518585, 8.811821500704338561, 0.7216878364870458196 ) ) ;
#145740 = CARTESIAN_POINT ( 'NONE',  ( -1.364683531250014514, -0.9489583329919112353, -0.7879004041258359514 ) ) ;
#145741 = CARTESIAN_POINT ( 'NONE',  ( 1.365380774817010368, 1.699871498885496379, -0.2916373863959387802 ) ) ;
#145742 = CARTESIAN_POINT ( 'NONE',  ( 6.086684617892325733, 6.065829907154645539, -0.7998128361456481317 ) ) ;
#145744 = CARTESIAN_POINT ( 'NONE',  ( 5.508355548902068577, 9.648441583686274470, 0.7998128361456331437 ) ) ;
#145743 = CARTESIAN_POINT ( 'NONE',  ( 7.673551755654734130, 9.015193805427763607, -1.082531754730537976 ) ) ;
#145745 = CARTESIAN_POINT ( 'NONE',  ( -11.55921752046871553, 8.211226526406720794, -3.233205798298055544 ) ) ;
#145746 = CARTESIAN_POINT ( 'NONE',  ( 6.837182164354378422, -1.670574593475544489, 0.8415915117672703172 ) ) ;
#145747 = CARTESIAN_POINT ( 'NONE',  ( 1.348292448571129842, 0.9904378492491233699, -1.752504823097464692 ) ) ;
#145748 = DIRECTION ( 'NONE',  ( -0.6483454320283800199, 0.000000000000000000, 0.7613463080411787542 ) ) ;
#145749 = CARTESIAN_POINT ( 'NONE',  ( 2.995379075007987613, 1.893430763284314811, -1.133229021217339483 ) ) ;
#145750 = CARTESIAN_POINT ( 'NONE',  ( 5.172805277531332457, 1.502137693623846193, -1.567733665727601089 ) ) ;
#145751 = EDGE_LOOP ( 'NONE', ( #147853, #110473 ) ) ;
#145752 = CARTESIAN_POINT ( 'NONE',  ( 0.7499999999999867883, -0.1833333333333131421, -1.299038105676652899 ) ) ;
#145754 = CARTESIAN_POINT ( 'NONE',  ( 7.727784369665023689, 11.95957283134381477, 1.040834085586084257E-14 ) ) ;
#145753 = AXIS2_PLACEMENT_3D ( 'NONE', #170483, #167299, #3686 ) ;
#145756 = CARTESIAN_POINT ( 'NONE',  ( 1.862907868837269998, -0.1017702599966328891, -2.013986063733465226 ) ) ;
#145755 = CARTESIAN_POINT ( 'NONE',  ( 3.510498622083501719, -2.118129049236017192, -0.1023006277712720374 ) ) ;
#145758 = EDGE_LOOP ( 'NONE', ( #10911, #89041 ) ) ;
#145757 = CARTESIAN_POINT ( 'NONE',  ( 2.460951123861610412, -1.504080979915609628, 1.009397298678058164 ) ) ;
#145759 = CARTESIAN_POINT ( 'NONE',  ( 6.886615681098613884, 6.999082814228660077, 0.000000000000000000 ) ) ;
#145760 = CARTESIAN_POINT ( 'NONE',  ( 4.774442650306744085, 8.721933525333202653, -0.7998128361456281477 ) ) ;
#145762 = CARTESIAN_POINT ( 'NONE',  ( 1.165091096179095675, 1.768693976065521589, -0.7364918582971339278 ) ) ;
#145761 = CARTESIAN_POINT ( 'NONE',  ( -3.567766978690493307, 7.314145241780881435, 1.040834085586084257E-14 ) ) ;
#145763 = CARTESIAN_POINT ( 'NONE',  ( 0.3870735955438693310, 1.000000000000000888, -11.88799243440807274 ) ) ;
#145764 = CARTESIAN_POINT ( 'NONE',  ( -4.856601257608931022, 5.009828881649966092, -0.8247166059246564540 ) ) ;
#145765 = CARTESIAN_POINT ( 'NONE',  ( 4.148431815657221300, 7.783661518334664464, 1.040834085586084257E-14 ) ) ;
#145766 = CARTESIAN_POINT ( 'NONE',  ( -1.402160292154681736E-14, 0.009375000341421267647, -1.575800808251665908 ) ) ;
#145767 = DIRECTION ( 'NONE',  ( -0.000000000000000000, 1.000000000000000000, 0.000000000000000000 ) ) ;
#145768 = CARTESIAN_POINT ( 'NONE',  ( -10.29471871147821282, 10.90492667301307605, -0.7998128361456291469 ) ) ;
#145769 = ORIENTED_EDGE ( 'NONE', *, *, #55665, .F. ) ;
#145770 = CARTESIAN_POINT ( 'NONE',  ( 5.067319851952804655, 0.2155487944876262052, -2.150937003660175151 ) ) ;
#145771 = CARTESIAN_POINT ( 'NONE',  ( -5.478903473698260029, 6.525047153136981137, -1.082531754730549967 ) ) ;
#145772 = CARTESIAN_POINT ( 'NONE',  ( 5.560252395380206991, 7.580323442733986283, 1.443375672974065660 ) ) ;
#145773 = CARTESIAN_POINT ( 'NONE',  ( 2.742561299210785286, 1.174483946500170184, -1.765453564165630596 ) ) ;
#145775 = CARTESIAN_POINT ( 'NONE',  ( -12.65289843835643069, 8.694282390621570045, -1.237672713095353982 ) ) ;
#145774 = CARTESIAN_POINT ( 'NONE',  ( -4.826181173005540614, 4.880474388334561375, 0.4619849944318583645 ) ) ;
#145776 = CARTESIAN_POINT ( 'NONE',  ( 2.934795777137487516, 0.2378783870938088740, 1.956871125110821952 ) ) ;
#145777 = ORIENTED_EDGE ( 'NONE', *, *, #136243, .F. ) ;
#145778 = CARTESIAN_POINT ( 'NONE',  ( 0.9243811426856913815, 1.018911950503737174, 1.802186752163869699 ) ) ;
#145779 = CARTESIAN_POINT ( 'NONE',  ( 2.536971540620248433, -1.439279119694805820, -1.303886525222669901 ) ) ;
#145780 = ORIENTED_EDGE ( 'NONE', *, *, #186980, .F. ) ;
#145781 = CARTESIAN_POINT ( 'NONE',  ( -10.99943592164172834, -9.999999999999994671, 0.1113975120798846308 ) ) ;
#145783 = LINE ( 'NONE', #211786, #40766 ) ;
#145782 = CARTESIAN_POINT ( 'NONE',  ( -6.075462232699549325, 9.141770800574526845, 1.082531754730549967 ) ) ;
#145785 = CARTESIAN_POINT ( 'NONE',  ( 6.226218857173709154, 8.287007971501239467, 1.599625672291281386 ) ) ;
#145784 = CARTESIAN_POINT ( 'NONE',  ( 2.853556533831374420, 2.080516846217596250, -0.2054353837145187767 ) ) ;
#145786 = CARTESIAN_POINT ( 'NONE',  ( 8.174640274396848483, 8.501778173076651512, 0.7998128361456291469 ) ) ;
#145788 = ORIENTED_EDGE ( 'NONE', *, *, #169120, .T. ) ;
#145787 = CARTESIAN_POINT ( 'NONE',  ( 6.516268831907007453, -1.911747763583053317, 0.05203757306279645223 ) ) ;
#145789 = CARTESIAN_POINT ( 'NONE',  ( 3.879664727460280904, 2.078262106501146622, -0.7427522710690689367 ) ) ;
#145790 = CARTESIAN_POINT ( 'NONE',  ( 2.942613154609276194, 2.189964478704994555, 0.2713889102748042736 ) ) ;
#145791 = CARTESIAN_POINT ( 'NONE',  ( -0.2619794211619215218, -6.848541063415908070, -10.99716886186657661 ) ) ;
#145792 = CARTESIAN_POINT ( 'NONE',  ( 2.279812546382542493, 1.875032136476075584, -0.3747091278499328770 ) ) ;
#145793 = CARTESIAN_POINT ( 'NONE',  ( 10.57266086055835075, 11.22919251360659310, 0.000000000000000000 ) ) ;
#145794 = CARTESIAN_POINT ( 'NONE',  ( 4.562978833902987752, 1.602482145440896399, -1.310924660355553106 ) ) ;
#145796 = CARTESIAN_POINT ( 'NONE',  ( 2.659225025413253007, -1.880336703546074073, -1.066323988048665017 ) ) ;
#145795 = CARTESIAN_POINT ( 'NONE',  ( 3.022498986271242138, 2.800000000000017586, 2.500000000000000444 ) ) ;
#145797 = CARTESIAN_POINT ( 'NONE',  ( 4.634432875810733599, 0.3748786239917039631, 2.159109584303263940 ) ) ;
#145798 = CARTESIAN_POINT ( 'NONE',  ( -5.876342332316932371, 6.610971932319779754, 0.8968535711802629873 ) ) ;
#145799 = CARTESIAN_POINT ( 'NONE',  ( -0.08369048095984887858, 7.010987279218348078, 1.999726996211184549 ) ) ;
#145800 = CARTESIAN_POINT ( 'NONE',  ( 5.520104819419390907, 6.469152373191302985, 1.199719254218452935 ) ) ;
#145801 = CARTESIAN_POINT ( 'NONE',  ( -3.285556943750000514, -3.026041666188709733, -1.896917185911906722 ) ) ;
#145802 = CARTESIAN_POINT ( 'NONE',  ( -5.978219388983010418, 5.939287140093762574, -0.7998128361456362523 ) ) ;
#145803 = CARTESIAN_POINT ( 'NONE',  ( 0.07093568767341934533, -0.9480374005119349690, 1.779628194860154222 ) ) ;
#145804 = CIRCLE ( 'NONE', #135412, 0.8300000000000008482 ) ;
#145805 = CARTESIAN_POINT ( 'NONE',  ( -9.327646496521992958, 9.984601788804893019, -0.7216878364870267237 ) ) ;
#145806 = CARTESIAN_POINT ( 'NONE',  ( 4.786024367859083029, -1.269482053145968514, -1.635305934682528717 ) ) ;
#145807 = CARTESIAN_POINT ( 'NONE',  ( 2.772000617051553206, 1.030904977978854609, 1.627292194166103600 ) ) ;
#145808 = CARTESIAN_POINT ( 'NONE',  ( 5.905892042933183816, -1.176582040423958642, -1.760015123184681007 ) ) ;
#145809 = CARTESIAN_POINT ( 'NONE',  ( 5.996784015946103885, 5.890669528225568996, 1.040834085586084257E-14 ) ) ;
#145810 = CARTESIAN_POINT ( 'NONE',  ( 0.000000000000000000, -5.166862915010159263, 0.000000000000000000 ) ) ;
#145811 = CARTESIAN_POINT ( 'NONE',  ( 4.188306824812327633, 1.057184280071225890, -1.661461291525099693 ) ) ;
#145812 = CARTESIAN_POINT ( 'NONE',  ( 6.386719491623852996, 1.997645938776301477, -1.124140632904375936 ) ) ;
#145814 = ADVANCED_FACE ( 'NONE', ( #170029 ), #72526, .T. ) ;
#145813 = CARTESIAN_POINT ( 'NONE',  ( 3.615676881913011176, -1.798418494116042821, 0.3134422064149794407 ) ) ;
#145815 = PRODUCT_DEFINITION_SHAPE ( 'NONE', 'NONE',  #51771 ) ;
#145816 = CARTESIAN_POINT ( 'NONE',  ( 7.526184669361807522, 7.953172667109813077, 0.000000000000000000 ) ) ;
#145817 = CARTESIAN_POINT ( 'NONE',  ( 5.463572716182829581, 6.436884926043849653, 1.082531754730560403 ) ) ;
#145818 = CARTESIAN_POINT ( 'NONE',  ( -5.745623237141265882, 9.925253886631958622, 0.7998128361456291469 ) ) ;
#145819 = CARTESIAN_POINT ( 'NONE',  ( 6.717138760927786834, 6.801359740696030443, -0.7998128361456481317 ) ) ;
#145820 = ORIENTED_EDGE ( 'NONE', *, *, #121881, .F. ) ;
#145822 = CARTESIAN_POINT ( 'NONE',  ( 4.869394097828703138, -1.702981969582622046, -1.073415598185305964 ) ) ;
#145821 = CARTESIAN_POINT ( 'NONE',  ( 1.048114208743459619, -1.451426956872736262, 1.132798186660122441 ) ) ;
#145823 = CARTESIAN_POINT ( 'NONE',  ( 6.522148393938469901, -2.055459957301557949, 1.029436805849759828 ) ) ;
#145824 = CARTESIAN_POINT ( 'NONE',  ( 5.787936641206399280, -1.241742415844361291, -1.518776266119965745 ) ) ;
#145825 = CARTESIAN_POINT ( 'NONE',  ( -5.045605722580076780, 9.038290442985410067, -0.7998128361456231517 ) ) ;
#145826 = CARTESIAN_POINT ( 'NONE',  ( -3.425406365747000859, 7.148057860013469877, 1.040834085586084257E-14 ) ) ;
#145827 = EDGE_CURVE ( 'NONE', #203624, #78850, #107243, .T. ) ;
#145828 = CARTESIAN_POINT ( 'NONE',  ( -5.255720823952942489, 6.160704378480398979, -1.199719254218453823 ) ) ;
#145830 = CARTESIAN_POINT ( 'NONE',  ( 0.3033014811697418711, -0.5033704626738467747, 1.801585485020948951 ) ) ;
#145829 = CARTESIAN_POINT ( 'NONE',  ( 2.032869862874300271, -1.866249813966861515, 0.9426962998228316515 ) ) ;
#145831 = CARTESIAN_POINT ( 'NONE',  ( -0.3866901564497978727, 3.102326550341739875, 2.027579305719746205 ) ) ;
#145832 = CARTESIAN_POINT ( 'NONE',  ( -1.364683531250005188, 3.311721076625156357, -0.3840134687763438470 ) ) ;
#145833 = CARTESIAN_POINT ( 'NONE',  ( 0.7315135518511396429, 1.714293348657709881, 0.2994600772705089953 ) ) ;
#145834 = AXIS2_PLACEMENT_3D ( 'NONE', #213719, #131490, #143465 ) ;
#145835 = CARTESIAN_POINT ( 'NONE',  ( 7.311924916471702396, 7.425000578838787391, -0.7998128361456281477 ) ) ;
#145837 = CARTESIAN_POINT ( 'NONE',  ( 2.672702088255949078E-15, 1.625000000682787160, 1.224999999999980549 ) ) ;
#145836 = CARTESIAN_POINT ( 'NONE',  ( 0.000000000000000000, 13.49999999999999822, 0.000000000000000000 ) ) ;
#145838 = CARTESIAN_POINT ( 'NONE',  ( 1.541173760317329666, -1.247365581009220126, -1.191596266039594010 ) ) ;
#145839 = CARTESIAN_POINT ( 'NONE',  ( 1.804482060849887270, 1.621174160030929068, -1.474864209862189579 ) ) ;
#145840 = CARTESIAN_POINT ( 'NONE',  ( 4.002700589841681200, -0.6913439845411989415, -2.095861086919461602 ) ) ;
#145841 = CARTESIAN_POINT ( 'NONE',  ( -10.89408488338165348, 4.581043481790748828, -4.512313115195546231 ) ) ;
#145842 = CARTESIAN_POINT ( 'NONE',  ( 1.885821443427546207, -2.045346407173433967, 0.7285060392495151804 ) ) ;
#145843 = CARTESIAN_POINT ( 'NONE',  ( 0.08226035653636187828, -1.769965142718381124, -0.4472663993063328847 ) ) ;
#145844 = CARTESIAN_POINT ( 'NONE',  ( 2.764987222883477980, -0.1607348756041589999, -2.111328481229361564 ) ) ;
#145845 = CARTESIAN_POINT ( 'NONE',  ( 4.975479186090857375, 5.867442474269873642, 1.082531754730560403 ) ) ;
#145846 = ORIENTED_EDGE ( 'NONE', *, *, #118406, .T. ) ;
#145848 = CARTESIAN_POINT ( 'NONE',  ( -1.402160292154681736E-14, -0.6156249996585817508, 1.575800808251672791 ) ) ;
#145847 = CARTESIAN_POINT ( 'NONE',  ( 2.859215333236740264, 0.3337469566037793989, -2.267824818490314254 ) ) ;
#145849 = CARTESIAN_POINT ( 'NONE',  ( 6.017121246366603060, 5.914396297049491658, 1.040834085586084257E-14 ) ) ;
#145850 = AXIS2_PLACEMENT_3D ( 'NONE', #25837, #126631, #209907 ) ;
#145851 = CARTESIAN_POINT ( 'NONE',  ( 6.322901860479969827, 1.648133277211549563, -1.489392227938668434 ) ) ;
#145852 = CARTESIAN_POINT ( 'NONE',  ( -6.344852701515500293, 9.385783337534627790, 1.082531754730548412 ) ) ;
#145853 = CARTESIAN_POINT ( 'NONE',  ( 6.005898861173831094, 6.109229547565340646, 1.040834085586084257E-14 ) ) ;
#145854 = CARTESIAN_POINT ( 'NONE',  ( -7.497295758232724872, 9.769931022736756177, -1.443375672974058777 ) ) ;
#145855 = ADVANCED_FACE ( 'NONE', ( #9665 ), #173264, .T. ) ;
#145856 = CARTESIAN_POINT ( 'NONE',  ( 4.529832720741620022, 7.338536369956936589, -1.082531754730548412 ) ) ;
#145857 = ORIENTED_EDGE ( 'NONE', *, *, #95954, .F. ) ;
#145858 = CARTESIAN_POINT ( 'NONE',  ( 3.533827422916273164, -1.646839391163470223, 1.163268690995450383 ) ) ;
#145860 = CARTESIAN_POINT ( 'NONE',  ( 2.237243932873288710, -0.09700783546583501005, -2.060382906607181930 ) ) ;
#145859 = CARTESIAN_POINT ( 'NONE',  ( 5.276094334012385367, 9.307193822989793475, 1.040834085586084257E-14 ) ) ;
#145861 = CARTESIAN_POINT ( 'NONE',  ( -11.84668729035137069, 13.50518580017410386, 1.399999999999998357 ) ) ;
#145862 = CARTESIAN_POINT ( 'NONE',  ( 3.879041346841291649, 7.539648981374564407, 1.040834085586084257E-14 ) ) ;
#145863 = CARTESIAN_POINT ( 'NONE',  ( -7.317172109022185289, -6.705807696133232021, -7.317172109022152426 ) ) ;
#145864 = CARTESIAN_POINT ( 'NONE',  ( -1.364683531250010295, 5.030208333674757171, 0.7879004041258379498 ) ) ;
#145865 = CARTESIAN_POINT ( 'NONE',  ( 4.857479518068650748, 2.167902099161696849, -0.3196092617779102696 ) ) ;
#145866 = CARTESIAN_POINT ( 'NONE',  ( 2.233046271152541618, 2.016033844848092560, 0.04667593304989729741 ) ) ;
#145867 = CARTESIAN_POINT ( 'NONE',  ( 2.138008341990283778, 0.4048980806483238326, 1.796005048712509655 ) ) ;
#145868 = CARTESIAN_POINT ( 'NONE',  ( 6.774270308322468459, 11.05506579301824743, 0.7998128361456462443 ) ) ;
#145869 = CARTESIAN_POINT ( 'NONE',  ( 5.403274641334286699, 1.493489847867332854, 1.049580640413529276 ) ) ;
#145870 = CARTESIAN_POINT ( 'NONE',  ( 5.678361341766085424, 1.528739221709461082, 1.314999087022615587 ) ) ;
#145871 = CARTESIAN_POINT ( 'NONE',  ( -6.665805079413154921, 10.92852302595736447, 0.7998128361456481317 ) ) ;
#145873 = CARTESIAN_POINT ( 'NONE',  ( -7.117104292530948229, 7.267986194233038155, -0.7998128361456362523 ) ) ;
#145872 = CARTESIAN_POINT ( 'NONE',  ( 5.383742603502962965, 1.515107113446222398, 1.680479692888930288 ) ) ;
#145874 = CARTESIAN_POINT ( 'NONE',  ( 0.7507728315698600774, 0.6134373412659529512, 2.014746520763583959 ) ) ;
#145875 = CARTESIAN_POINT ( 'NONE',  ( -6.129167961829681488, 9.308390501180058507, -1.199719254218452047 ) ) ;
#145876 = CARTESIAN_POINT ( 'NONE',  ( 10.38962578677386084, 11.01565159419135043, 0.000000000000000000 ) ) ;
#145877 = CARTESIAN_POINT ( 'NONE',  ( 0.6801582343749883464, 2.588541667008101399, -1.178068619123865846 ) ) ;
#145878 = DIRECTION ( 'NONE',  ( -0.6727051628309129727, -0.4815274654731236947, -0.5617820430519868680 ) ) ;
#145879 = CARTESIAN_POINT ( 'NONE',  ( -6.367525699912501835, 10.58053041653993098, -0.7998128361456291469 ) ) ;
#145880 = CARTESIAN_POINT ( 'NONE',  ( -5.111060722671894929, 5.065251719313053513, 0.000000000000000000 ) ) ;
#145881 = CARTESIAN_POINT ( 'NONE',  ( 4.895902867866261055, 4.884510565364971413, -0.7216878364870458196 ) ) ;
#145882 = CARTESIAN_POINT ( 'NONE',  ( 5.000138648025401977, 6.582195279309941860, -1.237349059142704988 ) ) ;
#145883 = CARTESIAN_POINT ( 'NONE',  ( -9.666600336863641729, 10.38004793587015584, 1.040834085586084257E-14 ) ) ;
#145884 = CARTESIAN_POINT ( 'NONE',  ( 2.320824347369263574, -0.8547976213506520704, -2.050556073580122707 ) ) ;
#145885 = CARTESIAN_POINT ( 'NONE',  ( 4.408728476930470165E-16, -0.5000000000000004441, -3.599999999999999201 ) ) ;
#145886 = CARTESIAN_POINT ( 'NONE',  ( -4.749098946536820520, 8.762642214260091933, 0.7998128361456281477 ) ) ;
#145887 = CARTESIAN_POINT ( 'NONE',  ( 7.447506452608354088, 7.583179037664891098, 0.7998128361456341429 ) ) ;
#145888 = CARTESIAN_POINT ( 'NONE',  ( 3.789464544343919883, -1.813617537123424661, 0.7486148740368094856 ) ) ;
#145889 = CARTESIAN_POINT ( 'NONE',  ( 6.972971076130050072, 7.029554431773520129, 1.040834085586084257E-14 ) ) ;
#145890 = CARTESIAN_POINT ( 'NONE',  ( -4.034408581249735448, 7.597519823075112200, 0.2926387080343200164 ) ) ;
#145891 = CARTESIAN_POINT ( 'NONE',  ( 2.523789150438203510, 6.096171108819874007, 0.7998128361456462443 ) ) ;
#145892 = CARTESIAN_POINT ( 'NONE',  ( -4.001064729808656573, 7.682009594836471500, 1.214306433183764966E-14 ) ) ;
#145893 = CARTESIAN_POINT ( 'NONE',  ( -5.395781948558855845, 9.238903340053241209, 0.7216878364870458196 ) ) ;
#145894 = AXIS2_PLACEMENT_3D ( 'NONE', #19322, #34512, #35573 ) ;
#145895 = CARTESIAN_POINT ( 'NONE',  ( 2.637105894733019262, 1.998242115483703341, 0.7103459930332192140 ) ) ;
#145896 = CARTESIAN_POINT ( 'NONE',  ( -5.367048706163331850, 7.354919138647580290, -1.599625672291271394 ) ) ;
#145897 = CARTESIAN_POINT ( 'NONE',  ( 4.856408821558930278, 0.8241108818672329139, 1.998647875481096126 ) ) ;
#145898 = CARTESIAN_POINT ( 'NONE',  ( 2.647807870277216757, 0.6224553824519338807, 1.732961026760751366 ) ) ;
#145899 = TOROIDAL_SURFACE ( 'NONE', #52466, 11.92000000000000171, 0.08000000000000000167 ) ;
#145900 = CARTESIAN_POINT ( 'NONE',  ( -4.964471428385745178, 6.642511170548884181, 1.245120630419704888 ) ) ;
#145901 = CARTESIAN_POINT ( 'NONE',  ( -1.402160292154681736E-14, 0.7593750003414168059, -1.575800808251659024 ) ) ;
#145902 = CARTESIAN_POINT ( 'NONE',  ( 6.105355155539634815, -1.726289741429184899, 0.2200517785161565654 ) ) ;
#145903 = CARTESIAN_POINT ( 'NONE',  ( 11.10517813317444791, 1.720726420432414194, -4.015189785735423733 ) ) ;
#145904 = CARTESIAN_POINT ( 'NONE',  ( 3.375617060122621194, 6.882044303544283537, 1.040834085586084257E-14 ) ) ;
#145905 = DIRECTION ( 'NONE',  ( -0.000000000000000000, -1.000000000000000000, -0.000000000000000000 ) ) ;
#145906 = CARTESIAN_POINT ( 'NONE',  ( 2.711983997553393699, -2.138339778157403615, 0.3160903847422363300 ) ) ;
#145907 = CARTESIAN_POINT ( 'NONE',  ( 4.182970119252515495, -1.034007530860373336, -1.730600854597413640 ) ) ;
#145908 = CARTESIAN_POINT ( 'NONE',  ( -8.744645890690007306, 12.18554205823825498, 1.082531754730558626 ) ) ;
#145909 = CARTESIAN_POINT ( 'NONE',  ( 2.026462046419864826, 1.244889377058140845, -1.767065586814352773 ) ) ;
#145910 = CARTESIAN_POINT ( 'NONE',  ( 3.075414692445295195, 1.873101151500027317, -0.6148835396118810248 ) ) ;
#145911 = CARTESIAN_POINT ( 'NONE',  ( 6.509000000000039421, 2.968845098214093703, 2.453284407971462411 ) ) ;
#145912 = CARTESIAN_POINT ( 'NONE',  ( 4.687022505062548916, 1.441580155910677785, 1.301524815871560214 ) ) ;
#145915 = ORIENTED_EDGE ( 'NONE', *, *, #43786, .T. ) ;
#145914 = SURFACE_STYLE_FILL_AREA ( #77672 ) ;
#145913 = CARTESIAN_POINT ( 'NONE',  ( -8.690413276235355866, 10.20153224610512943, 1.082531754730558626 ) ) ;
#145916 = CARTESIAN_POINT ( 'NONE',  ( -6.420668264523499147, 9.648474187656182366, 1.199719254218452935 ) ) ;
#145917 = CARTESIAN_POINT ( 'NONE',  ( 5.246079093845007257, 5.085123462432798114, 0.7998128361456352531 ) ) ;
#145919 = ORIENTED_EDGE ( 'NONE', *, *, #27402, .F. ) ;
#145918 = CARTESIAN_POINT ( 'NONE',  ( -3.871735385154307263, 6.674719161725423788, -1.199719254218450271 ) ) ;
#145920 = CARTESIAN_POINT ( 'NONE',  ( -8.690413276235355866, 10.20153224610512943, 1.082531754730558626 ) ) ;
#145921 = CARTESIAN_POINT ( 'NONE',  ( 1.325528760500709780, -0.05309137938146882979, 2.206304558879538025 ) ) ;
#145922 = CARTESIAN_POINT ( 'NONE',  ( 1.642778471875001811, -2.092708332855373943, 2.845375778867859751 ) ) ;
#145923 = CARTESIAN_POINT ( 'NONE',  ( 4.733228419949464971, 0.004064956161661801778, -1.961936380062332397 ) ) ;
#145924 = CARTESIAN_POINT ( 'NONE',  ( 1.364683531249990311, 5.426041667008086655, 0.7879004041258500513 ) ) ;
#145925 = CARTESIAN_POINT ( 'NONE',  ( 0.7499999999999920064, 4.264583334016150751, 1.299038105676669330 ) ) ;
#145926 = CARTESIAN_POINT ( 'NONE',  ( 4.825890400613210396, 6.946991693042408045, -1.413043630229819048 ) ) ;
#145927 = DIRECTION ( 'NONE',  ( 0.000000000000000000, 0.000000000000000000, 1.000000000000000000 ) ) ;
#145928 = CARTESIAN_POINT ( 'NONE',  ( 4.154132678086497776, -1.362845063541193946, 1.238102162693654362 ) ) ;
#145929 = VERTEX_POINT ( 'NONE', #8596 ) ;
#145930 = CARTESIAN_POINT ( 'NONE',  ( -1.552391752028397856E-14, 2.750000000682808921, -1.414508159514587415 ) ) ;
#145931 = CARTESIAN_POINT ( 'NONE',  ( -8.993135964566285168, 9.386413468282476913, -0.7998128361456291469 ) ) ;
#145932 = LINE ( 'NONE', #129736, #10142 ) ;
#145933 = CARTESIAN_POINT ( 'NONE',  ( 6.135037582782754129, 1.979230198018981701, 0.7618025574447004900 ) ) ;
#145934 = CARTESIAN_POINT ( 'NONE',  ( 11.82996952080117836, 6.822421697701821053, -1.712177087675395226 ) ) ;
#145935 = CARTESIAN_POINT ( 'NONE',  ( 5.286789834324991055, 8.255339675766103724, -1.199719254218452935 ) ) ;
#145936 = CARTESIAN_POINT ( 'NONE',  ( 6.854767756753092023, -1.595935894175725123, 1.303543064889536751 ) ) ;
#145939 = CARTESIAN_POINT ( 'NONE',  ( 4.194743914777058436, 1.481411246205705412, 1.093257649623424754 ) ) ;
#145938 = CARTESIAN_POINT ( 'NONE',  ( 1.416206177014844192, 0.7498276349873562729, 1.703500622989342572 ) ) ;
#145937 = FACE_OUTER_BOUND ( 'NONE', #161747, .T. ) ;
#145940 = CARTESIAN_POINT ( 'NONE',  ( 8.620286740190458374, 8.951422706510690830, 1.040834085586084257E-14 ) ) ;
#145941 = SURFACE_STYLE_USAGE ( .BOTH. , #80907 ) ;
#145942 = CARTESIAN_POINT ( 'NONE',  ( -6.607619761813764647, 8.802252036906432764, 1.599625672291269396 ) ) ;
#145943 = LINE ( 'NONE', #147000, #56233 ) ;
#145944 = CARTESIAN_POINT ( 'NONE',  ( 2.825073394047578734, 2.078234123670623212, 0.7428476018367863309 ) ) ;
#145945 = CARTESIAN_POINT ( 'NONE',  ( 6.046200420459929781, 2.259369630126391471, 0.1200006983746708389 ) ) ;
#145946 = CARTESIAN_POINT ( 'NONE',  ( -7.049876689426121779, 7.327203680526343632, -0.7216878364870278340 ) ) ;
#145947 = CARTESIAN_POINT ( 'NONE',  ( 6.398695480837623961, -1.778505541023298386, -0.3437013697835926140 ) ) ;
#145948 = CARTESIAN_POINT ( 'NONE',  ( 4.944510238519550072, -1.383032091829504928, 1.325833103116050626 ) ) ;
#145949 = CARTESIAN_POINT ( 'NONE',  ( 3.894033820048787398, 8.999999999999998224, 0.7749999999999996891 ) ) ;
#145950 = EDGE_CURVE ( 'NONE', #128668, #180412, #175390, .T. ) ;
#145951 = CARTESIAN_POINT ( 'NONE',  ( 6.121928861531041655, -1.040746078065577063, -1.554202398018275755 ) ) ;
#145952 = CARTESIAN_POINT ( 'NONE',  ( 6.338329682780378782, -0.9945775373912761896, 1.572806762946916903 ) ) ;
#145953 = CARTESIAN_POINT ( 'NONE',  ( -5.871133375163540613, 5.952003147219978807, -0.6782502278256223871 ) ) ;
#145954 = CARTESIAN_POINT ( 'NONE',  ( 6.016413156365523207, 1.185731173915012038, -1.314077388775713784 ) ) ;
#145955 = CARTESIAN_POINT ( 'NONE',  ( 1.710173085450257924, 1.157096902994741772, -1.651345047625000007 ) ) ;
#145957 = CARTESIAN_POINT ( 'NONE',  ( 3.246800538002168945, 0.5120957664956159450, 2.042728137747833461 ) ) ;
#145956 = CARTESIAN_POINT ( 'NONE',  ( -8.479735010343349089, 11.98044238112085758, 1.199719254218453823 ) ) ;
#145958 = CARTESIAN_POINT ( 'NONE',  ( 7.747594715205354809, 11.12627870345989756, -1.199719254218446718 ) ) ;
#145960 = CARTESIAN_POINT ( 'NONE',  ( -9.612894607289142357, 11.17379744904754801, -1.199719254218441611 ) ) ;
#145959 = CARTESIAN_POINT ( 'NONE',  ( 0.7499999999999867883, 0.06666666666668707997, -1.299038105676652899 ) ) ;
#145961 = FACE_OUTER_BOUND ( 'NONE', #144714, .T. ) ;
#145962 = CARTESIAN_POINT ( 'NONE',  ( 3.533467377359212680, -0.1442520194480846618, 2.014668725452229303 ) ) ;
#145963 = CARTESIAN_POINT ( 'NONE',  ( -1.201851678989727383E-14, 3.571875000341422357, 1.575800808251672791 ) ) ;
#145964 = CARTESIAN_POINT ( 'NONE',  ( 10.05978679165993483, 11.79913468076720306, 1.082531754730548412 ) ) ;
#145965 = CARTESIAN_POINT ( 'NONE',  ( 3.778741785029844369, -2.082091666206013159, -0.5805316298483630399 ) ) ;
#145966 = CARTESIAN_POINT ( 'NONE',  ( 1.436838838544733044, 7.449283400311756509, -4.203727439823553347 ) ) ;
#145967 = CARTESIAN_POINT ( 'NONE',  ( 6.668631453075247073, 8.873432343378178544, -1.599625672291281386 ) ) ;
#145968 = CARTESIAN_POINT ( 'NONE',  ( 9.422553571373278203, 11.05569592376608945, -1.082531754730543083 ) ) ;
#145970 = CARTESIAN_POINT ( 'NONE',  ( 7.894472390712621745, 15.33652541417121640, -9.039190989196168147 ) ) ;
#145969 = CARTESIAN_POINT ( 'NONE',  ( 0.8542542287434266024, -0.7813174834335520069, 2.025881038206469587 ) ) ;
#145971 = CARTESIAN_POINT ( 'NONE',  ( -6.887178846062123938, 8.097758744236356776, -1.082531754730544860 ) ) ;
#145972 = CARTESIAN_POINT ( 'NONE',  ( 0.6823417656249899377, 0.8427083336747520637, 1.181850606188755259 ) ) ;
#145973 = CARTESIAN_POINT ( 'NONE',  ( 2.068174269828721101, -1.345378145056834063, 1.729934933326432445 ) ) ;
#145974 = CARTESIAN_POINT ( 'NONE',  ( 0.5029403714634882450, 7.727853499551113003, 1.993913793680534452 ) ) ;
#145975 = CARTESIAN_POINT ( 'NONE',  ( 2.940562510593609513, 2.245292490812002661, 0.2782218841625680450 ) ) ;
#145976 = CARTESIAN_POINT ( 'NONE',  ( -6.496328159242330536, 10.73079995242472862, 0.000000000000000000 ) ) ;
#145977 = CARTESIAN_POINT ( 'NONE',  ( -4.297571505407598025, 5.076550180139354218, 1.082531754730558626 ) ) ;
#145978 = CARTESIAN_POINT ( 'NONE',  ( -1.201851678989727383E-14, 3.384375000341421469, 1.575800808251672791 ) ) ;
#145979 = CARTESIAN_POINT ( 'NONE',  ( 4.798147134389644464, 8.131168186839138556, 0.8272934513729796047 ) ) ;
#145980 = STYLED_ITEM ( 'NONE', ( #199356 ), #173474 ) ;
#145981 = CARTESIAN_POINT ( 'NONE',  ( 0.7500000000000006661, 10.58333333333333393, 1.299038105676657340 ) ) ;
#145982 = CARTESIAN_POINT ( 'NONE',  ( 6.211043768836170820, 9.299949259400630552, 1.082531754730549967 ) ) ;
#145983 = CARTESIAN_POINT ( 'NONE',  ( 3.637761035129345455, 0.7980134727624802471, -1.579695959945091044 ) ) ;
#145984 = CARTESIAN_POINT ( 'NONE',  ( 8.452618703115982512, 11.94880668935564216, 1.199719254218450271 ) ) ;
#145985 = CARTESIAN_POINT ( 'NONE',  ( 6.106501571484221458, -0.7887142981495840477, -2.061199855587454444 ) ) ;
#145987 = ADVANCED_FACE ( 'NONE', ( #77865 ), #60549, .T. ) ;
#145986 = CARTESIAN_POINT ( 'NONE',  ( -0.6823417656250039265, 9.567708333674735499, -1.181850606188755259 ) ) ;
#145988 = CARTESIAN_POINT ( 'NONE',  ( -6.283277845290492714, 6.295188672452495915, -0.7998128361456362523 ) ) ;
#145989 = CARTESIAN_POINT ( 'NONE',  ( 5.730092268227672037, 2.014234620932173758, 0.09611943034040781875 ) ) ;
#145990 = EDGE_LOOP ( 'NONE', ( #29491, #147733, #58396, #27318 ) ) ;
#145991 = CARTESIAN_POINT ( 'NONE',  ( 3.608139902456270143, -0.7572706533398064765, -1.710698989992056829 ) ) ;
#145992 = CARTESIAN_POINT ( 'NONE',  ( 3.080986915251407776, 1.947773190787219555, 0.7018234266842755531 ) ) ;
#145993 = CARTESIAN_POINT ( 'NONE',  ( -6.061904078641520144, 10.08632216847484031, 0.7216878364870267237 ) ) ;
#145994 = CARTESIAN_POINT ( 'NONE',  ( -1.734723475976807094E-14, 4.000000000000003553, -1.734723475976807094E-14 ) ) ;
#145995 = CYLINDRICAL_SURFACE ( 'NONE', #82416, 1.250000000000000000 ) ;
#145996 =( LENGTH_UNIT ( ) NAMED_UNIT ( * ) SI_UNIT ( .MILLI., .METRE. ) );
#145997 = ADVANCED_FACE ( 'NONE', ( #30191 ), #47537, .F. ) ;
#145998 = CARTESIAN_POINT ( 'NONE',  ( -1.364683531250012516, 3.801041667008087099, -0.7879004041258300672 ) ) ;
#145999 = B_SPLINE_CURVE_WITH_KNOTS ( 'NONE', 3,
 ( #114241, #79532, #64354, #211646, #28654, #145650, #131530, #160787, #197533, #11315 ),
 .UNSPECIFIED., .F., .F.,
 ( 4, 3, 3, 4 ),
 ( 1.849923431806924672E-17, 3.125162491452015815E-05, 6.527199249539997140E-05, 9.931020432975908203E-05 ),
 .UNSPECIFIED. ) ;
#146000 = CARTESIAN_POINT ( 'NONE',  ( 2.769914238037580745, -1.940913097850523128, 0.2850433363836765155 ) ) ;
#146001 = CARTESIAN_POINT ( 'NONE',  ( 1.493517298738750609, 1.942243344100362590, 0.5404107738020345053 ) ) ;
#146002 = CARTESIAN_POINT ( 'NONE',  ( -3.962726036944197894, 7.845207153068690431, -0.7998128361456481317 ) ) ;
#146003 = CARTESIAN_POINT ( 'NONE',  ( 8.934986926605834157, 10.38290515491702770, -1.199719254218446718 ) ) ;
#146004 = CARTESIAN_POINT ( 'NONE',  ( 6.907508285686359883, -0.4377196890756588910, 1.929438547640258017 ) ) ;
#146005 = CARTESIAN_POINT ( 'NONE',  ( 0.6823417656249899377, 3.676041667008085767, -1.181850606188754593 ) ) ;
#146006 = CARTESIAN_POINT ( 'NONE',  ( 1.898691433116481031, -1.975183796067316866, -0.3886032139628642912 ) ) ;
#146008 = CARTESIAN_POINT ( 'NONE',  ( 2.214611691679416072, 2.054518390865597954, 0.5110800211125585690 ) ) ;
#146007 = CARTESIAN_POINT ( 'NONE',  ( -6.643132081016132062, 8.773406732650713025, 1.443375672974078761 ) ) ;
#146009 = FACE_OUTER_BOUND ( 'NONE', #184671, .T. ) ;
#146010 = CARTESIAN_POINT ( 'NONE',  ( 4.193848433072798088, -1.425472641756184489, -1.501718461524886195 ) ) ;
#146011 = CARTESIAN_POINT ( 'NONE',  ( 4.492547798081839794, 6.334668079219206049, 1.599625672291262513 ) ) ;
#146013 = CARTESIAN_POINT ( 'NONE',  ( 4.403700966340357681, 4.032072637018845107, -0.7998128361456211532 ) ) ;
#146012 = CARTESIAN_POINT ( 'NONE',  ( 5.859345120547017949, 2.059885262428410968, -0.3562953063034664525 ) ) ;
#146015 = VERTEX_POINT ( 'NONE', #82126 ) ;
#146014 = CARTESIAN_POINT ( 'NONE',  ( 4.471595891589618788, 1.770651423122941548, -0.4439726157009425411 ) ) ;
#146016 = CARTESIAN_POINT ( 'NONE',  ( 10.07778825365955733, 10.65184113889131012, -0.7998128361456281477 ) ) ;
#146017 = CARTESIAN_POINT ( 'NONE',  ( 1.579999999999990523, 8.674529973577531194, -2.499999999999995115 ) ) ;
#146018 = CARTESIAN_POINT ( 'NONE',  ( 9.897453898556438645, 12.56651866558563313, 7.888353118025118071 ) ) ;
#146019 = CARTESIAN_POINT ( 'NONE',  ( 6.545939543708723107, 0.8506627741289953804, -2.036432556493542823 ) ) ;
#146021 =( BOUNDED_SURFACE ( )  B_SPLINE_SURFACE ( 3, 3, ( 
 ( #139826, #206920, #205855, #141971, #91072, #72654, #87855, #57487, #123648, #8724, #189610, #173387, #74806, #124703, #41256, #190662, #42322, #174458, #125767, #26034, #207983, #105190, #5495, #92146, #21746, #158200, #9790, #75864, #59611, #191729, #71576, #137684, #104109, #170158, #31389, #94275, #28180, #147274, #46580, #44451, #112699, #43385, #209037, #143042, #47658, #146226, #113769, #110568, #11920, #80121, #15107, #194944, #212243, #30325, #60673, #96409, #161396, #179772, #29254, #126836, #97464, #163520, #12980, #128964, #62803, #45518, #145172, #14035, #176570, #111634, #131081, #109506, #63877, #64931, #160316, #130031, #178709, #196022, #81196, #77993, #177645, #175513, #27103, #213306, #93210, #144115, #159242, #162459, #10842, #76916, #192793, #210109, #61749, #127916, #193869, #95346, #79055, #211177, #68106, #214338, #197070, #50824, #67041, #198127, #201310, #115885, #34565, #181870, #65968, #36694, #135296, #49759, #167776, #17231, #100636, #116951, #151537, #152587, #86522, #33506, #98515, #132117, #16162, #166713, #99579, #3105, #18303, #52950, #119088, #48707, #4174, #69176, #185068, #148338, #182950, #32446, #20440, #84389, #199178, #150476, #85452, #2036, #70243, #184012, #165643, #180819, #83306, #149393, #118023, #133178, #51901, #200249, #102779, #134242, #35626, #101704, #975, #114821, #19372, #164577, #168836, #82247, #139567, #54028, #188281, #123392, #71312, #137424, #9539, #120165, #186141, #189356, #40996, #124452, #187216, #121246, #25780, #205594, #203443, #57231, #136358, #87597, #21487, #140651, #24711, #206664, #55097, #104928, #173130, #108181, #73466, #90813, #107107, #153668, #156877, #39922, #58296, #122324, #5236, #190411, #42067, #106030, #7386, #155803, #138491, #23645, #8464, #38845, #202378, #37776, #103850, #74551, #174207, #91892, #170970, #22569, #157948, #169898, #88675, #154734, #6317, #72391, #204512, #56161, #172052, #89753, #76669, #44194, #112441, #47400, #12720, #30063, #62549, #26849, #128712, #193619, #211985, #61490, #92953, #63626, #79864, #45260, #161132, #95084, #77738, #177383, #46325, #208789, #143859, #163266, #141725, #178454, #97214, #142784, #96152, #144916, #13790, #129780, #195761, #162203, #145973, #78793, #60420, #127655, #210923, #176321, #194683, #159000, #75614, #209852, #160060, #126580, #113512, #192541, #111380, #110314, #10593, #179521, #31139, #27927, #207733, #94021, #28997, #59356, #125513, #191475, #43143, #11664, #109256, #175264, #48461, #66775, #214088, #183762, #50567, #19116, #167519, #14848, #36442, #130827, #180567, #118826, #81996, #18043, #133992, #49503, #114575, #85195, #117771, #196819, #15913, #199998, #35371, #131864, #148083, #32189, #711, #16973, #83054, #101446, #151280, #80938, #150216, #184812, #197871, #65716, #115623, #181618, #164323, #132916, #2851, #98265, #99331, #68920, #198921, #84130, #135041, #165380, #116689, #1788, #33247, #102516, #51648, #52695, #149130, #182688, #67845, #147030, #34306, #201054, #100381, #166453, #213052, #64681, #86266, #188022, #39651, #205333, #21233, #87338, #40735, #204249, #37515, #55901, #168579, #119905, #53772, #139304, #23381, #56971, #103591, #4975, #171785, #106841, #122058, #89491, #105760, #185880, #155546, #22299, #123145, #104666, #169648, #189102, #172872, #88411, #138235 ),
 ( #7125, #73198, #24443, #20179, #152337, #3915, #69984, #136096, #71053, #202112, #153406, #137169, #203193, #154479, #54839, #120990, #186957, #38589, #170714, #6057, #72128, #132560, #16610, #201755, #85905, #342, #118468, #182317, #199630, #67483, #102154, #103225, #37143, #198560, #49151, #165015, #181260, #51276, #50208, #168220, #183397, #151979, #35002, #147716, #149851, #1420, #3553, #98964, #133628, #197508, #185519, #117400, #101074, #167161, #36072, #18748, #169284, #134686, #116326, #131504, #66415, #33946, #68559, #17673, #2483, #84833, #150922, #200689, #52340, #184454, #19820, #100021, #69623, #20870, #213734, #135733, #65358, #148773, #53396, #119534, #115268, #32887, #82691, #166085, #83759, #106473, #88037, #72837, #172500, #187658, #24086, #104295, #86969, #155178, #171418, #154109, #91261, #5678, #138941, #71756, #170343, #141099, #25159, #137872, #57676, #121691, #204961, #6762, #41447, #42514, #190853, #203892, #202824, #21928, #120617, #56609, #55537, #107555, #122773, #157320, #188733, #153038, #89124, #40371, #8911, #38222, #90191, #136799, #124889, #156254, #7833, #73924, #189796, #140017, #108620, #206042, #39285, #70686, #105379, #23006, #123834, #173589, #74991, #207110, #58737, #174648, #4612, #54473, #186595, #204552, #145225, #158254, #174513, #143097, #45570, #124757, #109563, #111686, #209090, #125822, #175567, #177693, #142021, #193923, #92204, #208036, #191783, #9843, #108489, #58603, #210161, #78045, #43439, #25022, #157181, #192846, #11971, #61802, #46630, #59663, #10895, #60725, #126888, #27158, #190717, #211230, #79107, #93263, #42379, #144169, #159296, #29304, #62855, #127971, #75918, #8776, #76970, #44505, #160369, #110622, #94327, #28234, #95398, #176623, #161450, #13030, #129020, #194996, #91122, #74859, #26089, #140962, #112753, #206972, #16214, #165694, #113823, #179822, #51953, #96464, #162513, #17283, #83359, #166765, #15159, #163576, #68162, #181925, #31441, #33556, #178765, #130081, #63926, #183000, #67091, #34617, #97520, #147327, #1026, #150527, #115936, #133226, #149444, #196076, #199231, #82298, #100687, #164630, #47708, #18360, #84438, #148391, #49809, #198176, #180872, #66021, #50878, #81247, #32494, #30378, #14085, #117001, #200301, #213355, #2088, #99628, #134294, #80176, #146281, #212294, #64976, #131131, #197120, #214392, #48759, #114871, #98568, #132170, #118075, #186191, #202426, #119137, #122374, #36744, #169948, #102830, #201361, #172101, #56210, #185119, #88725, #152639, #21536, #37824, #72437, #73516, #7435, #168885, #19424, #135347, #151590, #87646, #20489, #138538, #153716, #188331, #5284, #184062, #120217, #103902, #39971, #69229, #71362, #167825, #155848, #137478, #203492, #55145, #6368, #121291, #187267, #205641, #35680, #204562, #139618, #86575, #154783, #38893, #106078, #23694, #89804, #101758, #85503, #104979, #4224, #171019, #22616, #70294, #3157, #53002, #136410, #54081, #141766, #58341, #61532, #190456, #109296, #42115, #140699, #111420, #209894, #124497, #27969, #91934, #175305, #191518, #11706, #12760, #161174, #108227, #173179, #74595, #90861, #26892, #174252, #77780, #92996, #127698, #159040, #57280, #59401, #125557, #193658, #8514, #43183, #107154, #95125, #10633, #76709, #142825, #160103, #208832, #78834, #44237, #25824, #41045, #157994 ),
 ( #123441, #189403, #9583, #24759, #60462, #156925, #126619, #110358, #206713, #75659, #144955, #207774, #192582, #176362, #94063, #45301, #143901, #177424, #29042, #214130, #212023, #65758, #210961, #162243, #96192, #754, #99372, #66820, #63666, #179557, #33288, #182734, #148129, #165424, #197913, #13829, #49541, #114616, #132963, #196859, #79904, #198966, #50610, #180607, #82035, #15952, #213091, #98303, #181661, #129820, #146012, #34353, #116735, #97251, #195802, #115667, #31178, #17022, #32232, #83098, #46363, #163305, #47439, #131905, #64721, #164368, #149178, #113554, #112483, #14886, #30102, #130863, #100426, #178492, #166497, #62588, #18088, #128751, #80981, #84176, #147070, #194724, #48497, #187008, #5030, #53823, #23430, #51696, #152386, #185928, #86314, #103644, #121041, #3964, #117818, #200045, #21284, #87390, #70032, #37564, #134037, #204299, #202165, #55955, #201102, #38639, #104718, #72176, #168626, #19166, #20229, #136148, #122108, #153457, #151328, #183808, #85240, #35418, #101496, #39702, #2896, #71105, #54887, #184862, #167566, #88467, #170766, #68969, #135088, #22355, #154527, #52742, #118876, #36489, #119953, #169696, #137223, #6106, #138284, #150265, #203243, #105811, #102566, #188073, #171837, #1833, #67892, #207530, #110110, #189152, #174004, #176121, #59149, #190206, #25575, #27721, #206459, #43992, #156668, #58086, #41866, #74344, #172922, #123191, #60213, #142573, #107975, #89541, #7177, #42931, #76464, #126374, #111176, #124248, #75409, #125307, #191265, #91686, #26647, #90609, #73248, #24498, #205385, #40791, #193421, #8260, #92748, #208580, #157739, #106896, #93815, #192333, #57024, #140448, #159856, #11459, #9336, #141522, #109041, #175060, #158792, #10389, #77532, #143653, #155592, #209648, #45065, #61289, #127450, #177178, #139355, #178255, #146834, #49315, #128516, #113315, #115432, #212853, #129577, #179321, #181423, #145784, #197671, #95951, #211787, #195564, #13595, #112244, #62355, #213900, #81801, #47200, #28794, #160930, #196624, #15716, #65523, #53303, #63425, #14652, #64490, #130632, #30942, #194484, #506, #82858, #97017, #46127, #147884, #163071, #33053, #48263, #99131, #78597, #80746, #29868, #180372, #114377, #31996, #98077, #79669, #144717, #164132, #162006, #131668, #165180, #210729, #16774, #94878, #135633, #12524, #148934, #69526, #201654, #119435, #41348, #7733, #40263, #89023, #58639, #86870, #187559, #6664, #121587, #138838, #156152, #39186, #152936, #20774, #56509, #122670, #105275, #72740, #169182, #25060, #22907, #91162, #21829, #73819, #139913, #107457, #203789, #54377, #55435, #171312, #157218, #188632, #186493, #4513, #120515, #70586, #136701, #74892, #38124, #106374, #90088, #5577, #202725, #123734, #205944, #104197, #170244, #57575, #189695, #87937, #154011, #71657, #155076, #204854, #172398, #173483, #8816, #185422, #23986, #141000, #137771, #207008, #37040, #103124, #59696, #28270, #145261, #9877, #209128, #211268, #94362, #10930, #60766, #62892, #27192, #79145, #191815, #93298, #77006, #109598, #208070, #158287, #95437, #177730, #143133, #124792, #42416, #78081, #111722, #161488, #146313, #159334, #110656, #160404, #12007, #126926, #75953, #96500, #178801, #192883, #142056, #29342, #44540, #129061, #144205, #195034, #174550, #176657, #125858, #61837, #210201, #128004 ),
 ( #46668, #193958, #43480, #45605, #13066, #112789, #30416, #175603, #190753, #162550, #14121, #80213, #212327, #108521, #26126, #92237, #147363, #118110, #2122, #131166, #34652, #98606, #115972, #198210, #18393, #19458, #167860, #48793, #179857, #81286, #97556, #181962, #114910, #84470, #99662, #68197, #65013, #32531, #100722, #35715, #1064, #150561, #50913, #15195, #117041, #33590, #200334, #49845, #213389, #51985, #134329, #165731, #149481, #83399, #66059, #17319, #166801, #197156, #132202, #151623, #130122, #184095, #85533, #180908, #101791, #133262, #63966, #196110, #47748, #113863, #31481, #67129, #164667, #199270, #183036, #16250, #163614, #82335, #148427, #38386, #87672, #4255, #7467, #136442, #55176, #202458, #86606, #57308, #155878, #70325, #188359, #37856, #121321, #137505, #172129, #173209, #107184, #54113, #119167, #20522, #36777, #187297, #120247, #23724, #38923, #73546, #105006, #3189, #5312, #71394, #139649, #168918, #203522, #53032, #41076, #171046, #22645, #88754, #106108, #154811, #24789, #204590, #186224, #201395, #103935, #169978, #138569, #153744, #72469, #6396, #89830, #56242, #122401, #39999, #205670, #123472, #69260, #135376, #21566, #185152, #189434, #102861, #90892, #152672, #91964, #158023, #30135, #74625, #140730, #209926, #143931, #144987, #207802, #141798, #46395, #160135, #9611, #11735, #156951, #108258, #42143, #161206, #45333, #12792, #159069, #78866, #174279, #10665, #206742, #194758, #126649, #76737, #142857, #111453, #192615, #112511, #61565, #59431, #58373, #75688, #125588, #77810, #26919, #127731, #193689, #177457, #93028, #44268, #29071, #208860, #110389, #8543, #124527, #191548, #190485, #95155, #25854, #60491, #210992, #43213, #109329, #175338, #176394, #27999, #62619, #128780, #178524, #94096, #81013, #200078, #99403, #97285, #165456, #96223, #47474, #195834, #100456, #198997, #166531, #163340, #64756, #132996, #67924, #33322, #50643, #83131, #113587, #149210, #214162, #18121, #82069, #179589, #84209, #150297, #65787, #181692, #115700, #98334, #197948, #66852, #14919, #164400, #183840, #162274, #116770, #117848, #147101, #182767, #17051, #34384, #1863, #134069, #51727, #13861, #785, #213125, #148160, #79938, #196891, #146043, #31211, #212056, #15983, #180642, #130898, #63697, #48529, #131937, #114649, #32267, #129851, #49575, #102606, #6137, #70068, #87424, #169728, #204329, #205419, #139386, #20265, #151362, #52775, #69004, #153491, #86349, #55988, #71136, #39737, #137254, #35451, #37597, #5061, #152420, #122139, #203273, #105842, #54920, #101530, #103680, #21317, #171869, #201137, #121071, #85276, #73282, #187039, #38671, #104750, #138314, #170799, #57056, #22388, #3999, #19198, #168660, #136181, #88498, #119988, #154560, #72207, #188107, #185965, #23465, #89575, #155624, #7209, #167599, #2932, #36519, #135121, #123221, #118913, #184894, #202199, #53855, #190239, #62383, #106931, #172955, #27755, #176155, #177212, #25607, #174035, #78627, #192365, #41897, #44024, #189185, #140479, #74377, #193456, #77567, #45100, #108008, #157770, #11495, #160962, #126405, #143689, #93850, #206491, #159888, #92782, #111209, #175092, #58121, #28825, #94913, #158827, #60248, #208615, #191300, #76495, #209681, #91719, #42968, #40822, #24534, #61325, #210763, #9369, #127485, #110142, #12552, #144751 ),
 ( #109076, #59180, #75440, #90642, #141552, #26680, #207559, #124280, #156702, #8293, #125337, #10423, #142606, #180405, #48294, #82888, #83950, #17867, #113347, #29897, #145812, #162035, #178289, #179352, #13626, #196654, #50399, #95983, #197703, #128547, #150041, #194513, #146867, #49345, #79699, #46161, #198752, #165213, #115464, #32024, #1612, #211819, #130665, #164161, #64519, #81831, #99160, #114406, #63456, #129610, #213930, #65552, #98109, #15746, #112274, #182510, #147914, #34140, #30974, #16803, #148964, #116519, #212888, #195595, #131697, #181455, #100209, #33085, #47230, #97049, #163102, #14682, #80779, #536, #66603, #132749, #166276, #102340, #101268, #5876, #170536, #183585, #68751, #38411, #22121, #184643, #134873, #18939, #53594, #69813, #135919, #88233, #204073, #67671, #203018, #171607, #167352, #121879, #187850, #200880, #2679, #185707, #154302, #85024, #152169, #71950, #37341, #168412, #3738, #138060, #36262, #55725, #52525, #20009, #86093, #118659, #151113, #201938, #104493, #120808, #119728, #133815, #199829, #21060, #54660, #39476, #89316, #103415, #169475, #87157, #153228, #4798, #70878, #105575, #23201, #136991, #186785, #155363, #51470, #117594, #35193, #93596, #56797, #41642, #106670, #158576, #75189, #125091, #26424, #206236, #25357, #142358, #122966, #139127, #77316, #43779, #76249, #191049, #94663, #188925, #9113, #42714, #157518, #174847, #192115, #141301, #40563, #172694, #92536, #10175, #207310, #108822, #205154, #61070, #58933, #127229, #57863, #109892, #175905, #143429, #91457, #90378, #208368, #59999, #193198, #126152, #8031, #24272, #156447, #74121, #140217, #110952, #124025, #27496, #159640, #107756, #189991, #11237, #209425, #173782, #44846, #176959, #28575, #6948, #73028, #112029, #146617, #162851, #14429, #181207, #82639, #160706, #81583, #50153, #194265, #293, #66363, #79452, #95734, #64275, #32835, #45911, #30719, #98912, #130420, #46975, #96802, #164964, #63201, #115217, #13377, #129365, #113091, #145568, #29649, #178031, #131455, #213683, #179097, #12300, #78380, #114165, #147666, #197456, #182266, #195343, #212634, #196407, #48052, #80519, #161786, #132510, #198508, #180158, #211567, #65306, #31784, #16556, #97856, #148723, #210508, #163919, #15495, #49097, #116276, #33891, #144501, #62143, #128303, #84780, #133572, #168168, #21877, #1367, #169229, #99969, #203837, #166034, #184400, #101019, #104243, #18698, #151925, #150867, #183343, #154058, #38170, #167111, #70634, #134634, #3499, #19766, #54422, #55483, #121636, #2429, #67429, #117346, #199578, #69569, #68506, #120564, #135679, #170289, #201703, #17619, #102098, #85848, #87983, #51222, #53347, #149793, #137818, #119481, #185468, #37089, #202772, #103168, #187605, #86917, #200638, #83704, #52286, #118415, #20820, #36020, #152985, #4559, #186541, #136745, #5624, #71705, #34947, #141046, #105324, #171361, #40315, #155127, #42458, #22955, #91205, #26169, #188680, #106421, #129888, #89069, #6709, #92287, #158331, #30170, #90134, #24031, #146081, #108567, #172444, #174594, #39232, #204904, #138886, #46432, #142104, #112550, #156201, #7777, #75999, #13896, #190799, #208117, #9925, #56558, #59745, #157266, #178561, #25103, #122718, #96259, #162311, #8857, #124832, #58684, #41391, #207053, #125905, #73868, #107502, #72785, #139963 ),
 ( #205986, #74936, #194795, #57622, #79978, #123779, #189739, #173530, #212093, #63729, #50683, #99442, #69041, #97324, #197986, #17091, #131978, #149253, #166574, #49614, #163380, #31248, #66896, #133036, #115739, #83169, #179627, #35491, #33360, #101569, #32304, #18161, #150335, #117886, #214199, #64792, #65829, #181729, #167636, #199035, #196929, #14954, #130936, #81052, #147136, #85318, #48567, #116808, #100498, #16020, #213162, #134106, #84249, #114687, #180679, #1903, #67962, #98371, #164434, #82106, #165498, #826, #182808, #200115, #183879, #195872, #34425, #151401, #148199, #19238, #2973, #51766, #47511, #113623, #155663, #20304, #5099, #7246, #38711, #21356, #71175, #73323, #37637, #89612, #202239, #103715, #87462, #120026, #4037, #168700, #105885, #188148, #153530, #135158, #52815, #88538, #122182, #171910, #156741, #169766, #121113, #104791, #170837, #137293, #86389, #106968, #189223, #203311, #152457, #39779, #54961, #139425, #22428, #205460, #184932, #187078, #70106, #72247, #154600, #6179, #138355, #186002, #36556, #204372, #136219, #56029, #57093, #102644, #23507, #201177, #24573, #118953, #123258, #40863, #53891, #172992, #90680, #8331, #27789, #45133, #142644, #41933, #124317, #159927, #11530, #208652, #110179, #58159, #128582, #126441, #194548, #125372, #111243, #28860, #210795, #92817, #157807, #158861, #60283, #46192, #77600, #75476, #190276, #9405, #108046, #25643, #178325, #141588, #143723, #193491, #109114, #174071, #12587, #177248, #91754, #207595, #94947, #160995, #191335, #59214, #43001, #192404, #76531, #44059, #78660, #62418, #74416, #209716, #29933, #175128, #112310, #96017, #26715, #10458, #176189, #144788, #93887, #61361, #162070, #127520, #140515, #206527, #34168, #130696, #182542, #80809, #196688, #180437, #212919, #97082, #47265, #198782, #66634, #114437, #13659, #145847, #181486, #567, #50431, #35225, #48327, #213961, #131728, #197733, #32054, #113380, #199858, #67701, #98142, #179387, #132779, #164191, #100240, #49374, #166308, #63490, #15777, #31007, #165243, #81863, #115491, #33115, #64553, #129646, #147947, #163134, #65581, #150071, #195631, #82919, #79731, #117627, #211854, #99192, #148992, #14718, #146899, #83983, #116550, #17897, #16837, #101301, #1643, #133848, #51501, #183618, #203047, #167381, #118688, #52556, #138090, #22149, #204103, #102370, #3766, #170567, #39507, #54688, #88264, #186814, #184672, #38442, #21087, #55755, #103445, #36294, #121911, #187880, #87190, #137020, #70910, #119757, #153255, #104522, #20039, #185736, #18971, #151141, #154332, #85055, #86126, #5907, #71980, #105606, #171637, #23234, #2708, #68782, #134901, #69841, #120839, #200907, #168440, #152199, #4830, #135952, #201967, #53625, #37369, #169505, #65232, #198432, #131382, #15418, #200559, #84701, #213605, #117264, #181134, #50078, #66284, #100940, #102021, #35942, #197378, #47974, #163839, #180081, #116199, #49019, #167027, #182186, #150788, #33814, #146543, #148647, #213, #2351, #97779, #132431, #196330, #184317, #99893, #165954, #17538, #34866, #83627, #168090, #133493, #115138, #130341, #32754, #98836, #67348, #16480, #1290, #149710, #18622, #82561, #199496, #51140, #183262, #68427, #212561, #64200, #147587, #114090, #134556, #31704, #52206, #118332, #81508, #164886, #19689, #3424, #69491, #138800 ),
 ( #171279, #186454, #22871, #103089, #85767, #153976, #170210, #86835, #90054, #4478, #137737, #70549, #169147, #139875, #23950, #152900, #56471, #120482, #203757, #5543, #40227, #41311, #189659, #136668, #201619, #20740, #119399, #55400, #202693, #106338, #121554, #156114, #187525, #151848, #87903, #71624, #7696, #37007, #39156, #135598, #123698, #105239, #88987, #155040, #188596, #6626, #107418, #72705, #54343, #53268, #38091, #104162, #204820, #21795, #122633, #172360, #73779, #205906, #57541, #173443, #185388, #144241, #93333, #191852, #208107, #176690, #79184, #158322, #143169, #145299, #28303, #159369, #209164, #211304, #175641, #13105, #125893, #27227, #10968, #43514, #142092, #92275, #29378, #111758, #77042, #58673, #190787, #12042, #45641, #95473, #80251, #60803, #44577, #94398, #160436, #126961, #9914, #30451, #112823, #192921, #75989, #177762, #110691, #62929, #78113, #129098, #108554, #210235, #59735, #61872, #128037, #193991, #161521, #109635, #174585, #195069, #46708, #178837, #96536, #26161, #162583, #14157, #146350, #124822, #42450, #32564, #187069, #213423, #113899, #4027, #130154, #52807, #202231, #147397, #65046, #88529, #196144, #47785, #53883, #131202, #114944, #167628, #197191, #81320, #31516, #185993, #120017, #98641, #212362, #179893, #168691, #37627, #103707, #22419, #19229, #201167, #118945, #184924, #180944, #97591, #38702, #54949, #85307, #163650, #169758, #151393, #21346, #36548, #87455, #15230, #2963, #48829, #152449, #69034, #102634, #20295, #135151, #86381, #70097, #136212, #153522, #137283, #5091, #71166, #64004, #104781, #203302, #121102, #170828, #56018, #72237, #10449, #191326, #9395, #58150, #27780, #122172, #156732, #190268, #90669, #108036, #125362, #8322, #188138, #204362, #25634, #91746, #74407, #41925, #138345, #208643, #206518, #60275, #205450, #42992, #109105, #76522, #172984, #23497, #24563, #140507, #126432, #157799, #155654, #39769, #89603, #105874, #171899, #44050, #7236, #75467, #59206, #189212, #73313, #92809, #175120, #139416, #57084, #26706, #158852, #123249, #40852, #106959, #124308, #174062, #141579, #142633, #192395, #154590, #110170, #6169, #207586, #176180, #209707, #11522, #164184, #130689, #163126, #211843, #181477, #61351, #96007, #129636, #29924, #47257, #64545, #162061, #127511, #143715, #179377, #30998, #13650, #195622, #77591, #147937, #145839, #213953, #144779, #196679, #48318, #15770, #112299, #177238, #178315, #79722, #65574, #97073, #94939, #193481, #28851, #45125, #111235, #197725, #160987, #14708, #212912, #128574, #12579, #32046, #114430, #78651, #210787, #180429, #98134, #62410, #194538, #46185, #63481, #113371, #80802, #81855, #131721, #93878, #146892, #49365, #115484, #159916, #67693, #166298, #182532, #151133, #53615, #132770, #117615, #119748, #2700, #133839, #20028, #100230, #153245, #86117, #17889, #150062, #199850, #83974, #116542, #66623, #3757, #152188, #51492, #33107, #165234, #200899, #69832, #135940, #54678, #183607, #18961, #68773, #134892, #1634, #198773, #4818, #87179, #35216, #50422, #201958, #101291, #185726, #52546, #37359, #82911, #167373, #34160, #184663, #85045, #118678, #36282, #102360, #148984, #168432, #103434, #169495, #21077, #559, #70899, #99183, #137010, #203037, #120827, #16827, #6966, #105594, #121900, #90396, #207332, #71968 ) ),
 .UNSPECIFIED., .T., .F., .F. ) 
 B_SPLINE_SURFACE_WITH_KNOTS ( ( 4, 3, 4 ),
 ( 4, 1, 1, 1, 1, 1, 1, 1, 1, 1, 1, 1, 1, 1, 1, 1, 1, 1, 1, 1, 1, 1, 1, 1, 1, 1, 1, 1, 1, 1, 1, 1, 1, 1, 1, 1, 1, 1, 1, 1, 1, 1, 1, 1, 1, 1, 1, 1, 1, 1, 1, 1, 1, 1, 1, 1, 1, 1, 1, 1, 1, 1, 1, 1, 1, 1, 1, 1, 1, 1, 1, 1, 1, 1, 1, 1, 1, 1, 1, 1, 1, 1, 1, 1, 1, 1, 1, 1, 1, 1, 1, 1, 1, 1, 1, 1, 1, 1, 1, 1, 1, 1, 1, 1, 1, 1, 1, 1, 1, 1, 1, 1, 1, 1, 1, 1, 1, 1, 1, 1, 1, 1, 1, 1, 1, 1, 1, 1, 1, 1, 1, 1, 1, 1, 1, 1, 1, 1, 1, 1, 1, 1, 1, 1, 1, 1, 1, 1, 1, 1, 1, 1, 1, 1, 1, 1, 1, 1, 1, 1, 1, 1, 1, 1, 1, 1, 1, 1, 1, 1, 1, 1, 1, 1, 1, 1, 1, 1, 1, 1, 1, 1, 1, 1, 1, 1, 1, 1, 1, 1, 1, 1, 1, 1, 1, 1, 1, 1, 1, 1, 1, 1, 1, 1, 1, 1, 1, 1, 1, 1, 1, 1, 1, 1, 1, 1, 1, 1, 1, 1, 1, 1, 1, 1, 1, 1, 1, 1, 1, 1, 1, 1, 1, 1, 1, 1, 1, 1, 1, 1, 1, 1, 1, 1, 1, 1, 1, 1, 1, 1, 1, 1, 1, 1, 1, 1, 1, 1, 1, 1, 1, 1, 1, 1, 1, 1, 1, 1, 1, 1, 1, 1, 1, 1, 1, 1, 1, 1, 1, 1, 1, 1, 1, 1, 1, 1, 1, 1, 1, 1, 1, 1, 1, 1, 1, 1, 1, 1, 1, 1, 1, 1, 1, 1, 1, 1, 1, 1, 1, 1, 1, 1, 1, 1, 1, 1, 1, 1, 1, 1, 1, 1, 1, 1, 1, 1, 1, 1, 1, 1, 1, 1, 1, 1, 1, 1, 1, 1, 1, 1, 1, 1, 1, 1, 1, 1, 1, 1, 1, 1, 1, 1, 1, 1, 1, 1, 1, 1, 1, 1, 1, 1, 1, 1, 1, 1, 1, 1, 1, 1, 1, 1, 1, 1, 1, 1, 1, 1, 1, 1, 1, 1, 1, 1, 4 ),
 ( 0.000000000000000000, 0.5000000000000000000, 1.000000000000000000 ),
 ( 0.000000000000000000, 0.002599888508634240914, 0.005208754120092145765, 0.007813069968323356138, 0.01041690100177071650, 0.01302019566086259385, 0.01562517182793091500, 0.01822893254318404960, 0.02083328139698771564, 0.02343764900838959594, 0.02604139750447371365, 0.02864615928571910553, 0.03124958462592061434, 0.03385442086835698666, 0.03645794792899405279, 0.03906256697173399878, 0.04166661757251870907, 0.04427067912273281725, 0.04687528696281444140, 0.04947881815967773017, 0.05208365228821221909, 0.05468707701066444909, 0.05729184299815447134, 0.05989557646906591704, 0.06249996333325048142, 0.06510433798480201595, 0.06770807906337909798, 0.07031283757201339801, 0.07291626355048291819, 0.07552109983967189577, 0.07812462590386089201, 0.08072924387304455940, 0.08333329402460390445, 0.08593735478041557296, 0.08854196204427712547, 0.09114549249794960672, 0.09375032597506528786, 0.09635375006294695510, 0.09895851527076646170, 0.1015622481948881828, 0.1041666342325376776, 0.1067710083972730206, 0.1093747487337090180, 0.1119795066911244419, 0.1145829320296284648, 0.1171877676425944481, 0.1197912931610935483, 0.1223959103579086161, 0.1249999600491941698, 0.1276040200539713398, 0.1302086268569593308, 0.1328121566649932417, 0.1354169895755736042, 0.1380204131161003600, 0.1406251776355303407, 0.1432289101024236955, 0.1458332954032181272, 0.1484376691708411133, 0.1510414088543486633, 0.1536461663508109643, 0.1562495911381983071, 0.1588544261652600487, 0.1614579512270202244, 0.1640625677415503691, 0.1666666170620310916, 0.1692706764052687440, 0.1718752828374313091, 0.1744788120887783289, 0.1770836445231302458, 0.1796870676051354199, 0.1822918315264069888, 0.1848955636252137269, 0.1874999482789682093, 0.1901043217392619777, 0.1927080608589964439, 0.1953128179847096746, 0.1979162423098047296, 0.2005210768412587219, 0.2031246015352002054, 0.2057292174574958665, 0.2083332664966131842, 0.2109373252677763377, 0.2135419314191336626, 0.2161454602027163274, 0.2187502922511180836, 0.2213537149634070833, 0.2239584783767220588, 0.2265622101965570623, 0.2291665942930569411, 0.2317709675357785548, 0.2343747061808670040, 0.2369794630260087243, 0.2395828869776091552, 0.2421877211037245237, 0.2447912455187418734, 0.2473958609388257068, 0.2499999097859964270, 0.2526039680745227334, 0.2552085740350705789, 0.2578121024397855843, 0.2604169341924902348, 0.2630203566238439872, 0.2656251196193780695, 0.2682288512493328225, 0.2708332348783377697, 0.2734376079932215875, 0.2760413462527663842, 0.2786461029074911444, 0.2812495265743710227, 0.2838543603853929120, 0.2864578846103582599, 0.2890624996182282747, 0.2916665483628478883, 0.2942706062581511572, 0.2968752121178640513, 0.2994787402325856385, 0.3020835717798243114, 0.3046869940190023440, 0.3072917566869088346, 0.3098954882160545599, 0.3124998714673014044, 0.3151042445440625506, 0.3177079825071445485, 0.3203127390615869707, 0.3229161625325003282, 0.3255209961186533163, 0.3281245202424198926, 0.3307291349280532256, 0.3333331836594992104, 0.3359372412509727956, 0.3385418470998076690, 0.3411453750133909280, 0.3437502064453764050, 0.3463536285811206206, 0.3489583910115333087, 0.3515621225289245477, 0.3541665054921307454, 0.3567708786204680238, 0.3593746163761498691, 0.3619793729204284771, 0.3645827962841124981, 0.3671876297356038710, 0.3697911538470093351, 0.3723957683003653041, 0.3749998171080005105, 0.3776038744850206963, 0.3802084804129200468, 0.3828120082142042468, 0.3854168396211344327, 0.3880202617421720235, 0.3906250240252089334, 0.3932287556198868494, 0.3958331383847540352, 0.3984375116543538153, 0.4010412492916836102, 0.4036460059159037717, 0.4062494292610819846, 0.4088542626681055392, 0.4114577868559751161, 0.4140624011669984950, 0.4166664501401745602, 0.4192705073921035863, 0.4218751134889988097, 0.4244786412668108966, 0.4270834727388717056, 0.4296868949339185950, 0.4322916571596854274, 0.4348953889206810253, 0.4374997715768980666, 0.4401041450774376140, 0.4427078826854516369, 0.4453126394797092824, 0.4479160628950952239, 0.4505208963478340434, 0.4531244207009840763, 0.4557290349596088697, 0.4583330841876695483, 0.4609371414038593850, 0.4635417477596745495, 0.4661452756028321986, 0.4687501072302013849, 0.4713535295879656695, 0.4739582918465587991, 0.4765620238628961447, 0.4791664065001429718, 0.4817707803212932793, 0.4843745179890200370, 0.4869792750434049911, 0.4895826986177053142, 0.4921875322063354874, 0.4947910568135764908, 0.4973956711097291539, 0.4999997206820134821, 0.5026037779518089943, 0.5052083846564635605, 0.5078119126537786743, 0.5104167445266291070, 0.5130201671358142201, 0.5156249295173244152, 0.5182286618780244103, 0.5208330445859747915, 0.5234374188174044651, 0.5260411566338674128, 0.5286459140384663913, 0.5312493378603841965, 0.5338541716750782040, 0.5364576966252184720, 0.5390623110488209635, 0.5416663610546670338, 0.5442704184674093115, 0.5468750256108222407, 0.5494785538511040013, 0.5520833860596070508, 0.5546868090089153158, 0.5572915716034309019, 0.5598953043975141153, 0.5624996872658396541, 0.5651040619972180767, 0.5677078000514395040, 0.5703125578963399445, 0.5729159820545779436, 0.5755208161855079885, 0.5781243415673570363, 0.5807289562083304268, 0.5833330067370782190, 0.5859370643821081304, 0.5885416720542003821, 0.5911452006262593040, 0.5937500332605881725, 0.5963534566387238556, 0.5989582195363342132, 0.6015619528528246551, 0.6041663359711972880, 0.6067707112921981727, 0.6093744496732020899, 0.6119792080484952601, 0.6145826326317597177, 0.6171874671691013337, 0.6197909930714722293, 0.6223956080197403651, 0.6249996591607356322, 0.6276037171273963766, 0.6302083254180952387, 0.6328118544107458332, 0.6354166875610788301, 0.6380201114567515264, 0.6406248747475506988, 0.6432286086754787080, 0.6458329921335752566, 0.6484373681338796436, 0.6510411069306952792, 0.6536458659264798854, 0.6562492910234830612, 0.6588541260574176661, 0.6614576525691320263, 0.6640622679146246377, 0.6666663197572214594, 0.6692703781348633418, 0.6718749871341050950, 0.6744785166361690898, 0.6770833503926931840, 0.6796867748946214816, 0.6822915386687108397, 0.6848952732971168578, 0.6874996571846213600, 0.6901040339539210589, 0.6927077732555863010, 0.6953125329619718187, 0.6979159586614360755, 0.7005207942821553013, 0.7031243214920454010, 0.7057289373247008779, 0.7083329899582661016, 0.7109370488362486418, 0.7135416586339821121, 0.7161451887342924483, 0.7187500231872065992, 0.7213534483841206324, 0.7239582127316128712, 0.7265619481495508847, 0.7291663325561579256, 0.7317707101841592898, 0.7343744500797240171, 0.7369792105868335774, 0.7395826369774940456, 0.7421874732752028470, 0.7447910012721150608, 0.7473956176818850050, 0.7499996711958007989, 0.7526037306634962842, 0.7552083413496862851, 0.7578118721370898925, 0.7604167073766084917, 0.7630201333572542710, 0.7656248983682768516, 0.7682286346648167230, 0.7708330196802359868, 0.7734373982566630223, 0.7760411388351919904, 0.7786459002331664880, 0.7812493274037752844, 0.7838541644686951582, 0.7864576933414935134, 0.7890623104183455139, 0.7916663649020125870, 0.7942704250488100692, 0.7968750367134410650, 0.7994785682768023038, 0.8020834043931583945, 0.8046868312463003603, 0.8072915970109983963, 0.8098953342752303053, 0.8124997199891885735, 0.8151040996037859365, 0.8177078409543626636, 0.8203126033333638656, 0.8229160313726919806, 0.8255208692950642968, 0.8281243991326340259, 0.8307290169665545454, 0.8333330725093962554, 0.8359371334247044372, 0.8385417461577832077, 0.8411452785859873105, 0.8437501156694361404, 0.8463535434838604932, 0.8489583100924004144, 0.8515620484134380774, 0.8541664349156833369, 0.8567708156582201084, 0.8593745578699503174, 0.8619793213201638604, 0.8645827503170061545, 0.8671875891870957087, 0.8697911200783463581, 0.8723957387593448409, 0.8749997954508100806, 0.8776038572240605351, 0.8802084711156200614, 0.8828120044975765746, 0.8854168426383988155, 0.8880202715029178462, 0.8906250390454908406, 0.8932287785124739532, 0.8958331658927787267, 0.8984375478530519654, 0.9010412910150662480, 0.9036460556267057465, 0.9062494856698833923, 0.9088543255779816255, 0.9114578576118502751, 0.9140624772299625889, 0.9166665351595286726, 0.9192705978801787303, 0.9218752130202838568, 0.9244787474449313036, 0.9270835867334279445, 0.9296870167368762594, 0.9322917853037333558, 0.9348955260058576799, 0.9374999143539141100, 0.9401042976215825409, 0.9427080418234272674, 0.9453128076877782560, 0.9479162388645026027, 0.9505210798953250828, 0.9531246131693177359, 0.9557292338404025367, 0.9583332930514818493, 0.9609373567081632705, 0.9635419734050364449, 0.9661455093234165847, 0.9687503490003109841, 0.9713537788664922124, 0.9739585512809396661, 0.9765622998769101226, 0.9791666815729623830, 0.9817710277688282972, 0.9843747994658795797, 0.9869797739623470401, 0.9895830763955310028, 0.9921869177308453303, 0.9947912343601759133, 0.9974001139318913189, 1.000000000000000000 ),
 .UNSPECIFIED. ) 
 GEOMETRIC_REPRESENTATION_ITEM ( )  RATIONAL_B_SPLINE_SURFACE ( (
 ( 1.000000000000000222, 1.000000000000000222, 1.000000000000000222, 1.000000000000000000, 1.000000000000000000, 1.000000000000000444, 1.000000000000000000, 0.9999999999999997780, 1.000000000000000444, 0.9999999999999997780, 0.9999999999999997780, 1.000000000000000222, 0.9999999999999997780, 0.9999999999999997780, 1.000000000000000444, 0.9999999999999997780, 1.000000000000000222, 1.000000000000000222, 0.9999999999999996669, 1.000000000000000222, 0.9999999999999996669, 1.000000000000000444, 0.9999999999999994449, 1.000000000000000444, 0.9999999999999996669, 1.000000000000000222, 1.000000000000000000, 0.9999999999999997780, 1.000000000000000222, 0.9999999999999997780, 1.000000000000000000, 0.9999999999999997780, 1.000000000000000000, 1.000000000000000222, 0.9999999999999996669, 1.000000000000000000, 0.9999999999999997780, 1.000000000000000000, 1.000000000000000444, 0.9999999999999996669, 1.000000000000000222, 1.000000000000000000, 1.000000000000000222, 1.000000000000000222, 0.9999999999999997780, 0.9999999999999997780, 1.000000000000000222, 0.9999999999999997780, 1.000000000000000222, 0.9999999999999997780, 0.9999999999999997780, 0.9999999999999997780, 1.000000000000000444, 1.000000000000000000, 0.9999999999999997780, 1.000000000000000222, 1.000000000000000000, 1.000000000000000000, 0.9999999999999997780, 1.000000000000000222, 1.000000000000000000, 1.000000000000000000, 1.000000000000000222, 1.000000000000000000, 1.000000000000000000, 1.000000000000000000, 1.000000000000000222, 1.000000000000000000, 0.9999999999999997780, 1.000000000000000444, 1.000000000000000000, 0.9999999999999997780, 1.000000000000000000, 1.000000000000000222, 0.9999999999999997780, 1.000000000000000222, 0.9999999999999996669, 1.000000000000000222, 1.000000000000000000, 1.000000000000000000, 1.000000000000000000, 1.000000000000000222, 0.9999999999999997780, 1.000000000000000000, 1.000000000000000222, 0.9999999999999997780, 1.000000000000000000, 1.000000000000000000, 0.9999999999999996669, 1.000000000000000000, 1.000000000000000000, 1.000000000000000222, 1.000000000000000000, 0.9999999999999997780, 1.000000000000000222, 0.9999999999999996669, 1.000000000000000222, 0.9999999999999997780, 1.000000000000000000, 1.000000000000000000, 1.000000000000000222, 0.9999999999999996669, 1.000000000000000444, 1.000000000000000000, 0.9999999999999997780, 1.000000000000000000, 1.000000000000000000, 1.000000000000000222, 0.9999999999999997780, 1.000000000000000000, 1.000000000000000222, 1.000000000000000444, 1.000000000000000000, 1.000000000000000000, 1.000000000000000444, 1.000000000000000000, 0.9999999999999997780, 1.000000000000000222, 1.000000000000000000, 1.000000000000000000, 1.000000000000000000, 1.000000000000000000, 1.000000000000000000, 1.000000000000000000, 0.9999999999999996669, 1.000000000000000222, 0.9999999999999997780, 1.000000000000000222, 1.000000000000000000, 0.9999999999999997780, 1.000000000000000222, 0.9999999999999997780, 0.9999999999999997780, 0.9999999999999997780, 1.000000000000000000, 1.000000000000000000, 0.9999999999999996669, 1.000000000000000444, 1.000000000000000222, 1.000000000000000000, 1.000000000000000000, 1.000000000000000222, 1.000000000000000222, 1.000000000000000000, 1.000000000000000222, 0.9999999999999996669, 1.000000000000000444, 0.9999999999999997780, 0.9999999999999997780, 1.000000000000000444, 1.000000000000000000, 1.000000000000000222, 0.9999999999999997780, 1.000000000000000222, 1.000000000000000000, 1.000000000000000222, 1.000000000000000000, 1.000000000000000000, 0.9999999999999996669, 1.000000000000000444, 1.000000000000000000, 1.000000000000000222, 0.9999999999999997780, 1.000000000000000000, 1.000000000000000000, 1.000000000000000000, 1.000000000000000000, 0.9999999999999997780, 1.000000000000000000, 1.000000000000000000, 1.000000000000000000, 1.000000000000000222, 1.000000000000000222, 0.9999999999999997780, 1.000000000000000000, 1.000000000000000000, 0.9999999999999997780, 1.000000000000000000, 1.000000000000000000, 1.000000000000000000, 1.000000000000000000, 1.000000000000000444, 0.9999999999999997780, 1.000000000000000222, 0.9999999999999997780, 1.000000000000000000, 1.000000000000000222, 0.9999999999999997780, 1.000000000000000222, 1.000000000000000000, 1.000000000000000000, 1.000000000000000000, 1.000000000000000000, 0.9999999999999997780, 1.000000000000000000, 1.000000000000000000, 1.000000000000000000, 1.000000000000000000, 1.000000000000000000, 1.000000000000000222, 1.000000000000000000, 1.000000000000000222, 0.9999999999999997780, 1.000000000000000222, 0.9999999999999997780, 1.000000000000000222, 1.000000000000000000, 0.9999999999999997780, 1.000000000000000222, 0.9999999999999996669, 1.000000000000000444, 1.000000000000000000, 0.9999999999999996669, 1.000000000000000222, 1.000000000000000000, 1.000000000000000222, 0.9999999999999997780, 1.000000000000000444, 1.000000000000000000, 1.000000000000000000, 0.9999999999999997780, 1.000000000000000222, 1.000000000000000000, 1.000000000000000000, 1.000000000000000000, 1.000000000000000222, 0.9999999999999997780, 1.000000000000000222, 1.000000000000000000, 0.9999999999999997780, 1.000000000000000000, 0.9999999999999997780, 1.000000000000000222, 0.9999999999999996669, 1.000000000000000000, 1.000000000000000000, 1.000000000000000000, 1.000000000000000444, 1.000000000000000222, 1.000000000000000000, 1.000000000000000000, 0.9999999999999997780, 0.9999999999999997780, 1.000000000000000444, 0.9999999999999996669, 1.000000000000000444, 0.9999999999999997780, 0.9999999999999997780, 1.000000000000000222, 0.9999999999999997780, 0.9999999999999996669, 1.000000000000000444, 0.9999999999999997780, 1.000000000000000222, 1.000000000000000222, 1.000000000000000000, 0.9999999999999997780, 1.000000000000000222, 1.000000000000000000, 1.000000000000000222, 1.000000000000000000, 1.000000000000000000, 0.9999999999999997780, 0.9999999999999997780, 1.000000000000000444, 0.9999999999999997780, 0.9999999999999997780, 1.000000000000000222, 0.9999999999999994449, 1.000000000000000222, 0.9999999999999997780, 1.000000000000000000, 0.9999999999999997780, 1.000000000000000000, 1.000000000000000000, 1.000000000000000000, 1.000000000000000000, 1.000000000000000000, 1.000000000000000000, 1.000000000000000000, 1.000000000000000222, 1.000000000000000000, 1.000000000000000000, 1.000000000000000000, 1.000000000000000000, 1.000000000000000000, 1.000000000000000000, 1.000000000000000000, 1.000000000000000222, 1.000000000000000000, 1.000000000000000222, 0.9999999999999997780, 1.000000000000000000, 1.000000000000000444, 1.000000000000000000, 1.000000000000000000, 1.000000000000000000, 1.000000000000000222, 0.9999999999999997780, 1.000000000000000444, 0.9999999999999997780, 1.000000000000000222, 1.000000000000000000, 1.000000000000000000, 1.000000000000000000, 1.000000000000000222, 0.9999999999999994449, 1.000000000000000222, 1.000000000000000000, 1.000000000000000000, 1.000000000000000000, 0.9999999999999997780, 0.9999999999999997780, 1.000000000000000444, 0.9999999999999996669, 1.000000000000000222, 0.9999999999999997780, 1.000000000000000444, 0.9999999999999997780, 1.000000000000000222, 1.000000000000000222, 0.9999999999999996669, 1.000000000000000222, 1.000000000000000000, 1.000000000000000444, 1.000000000000000000, 1.000000000000000000, 1.000000000000000222, 1.000000000000000000, 1.000000000000000000, 0.9999999999999997780, 0.9999999999999997780, 1.000000000000000000, 0.9999999999999997780, 1.000000000000000222, 1.000000000000000222, 1.000000000000000000, 1.000000000000000222, 1.000000000000000222, 1.000000000000000000, 0.9999999999999997780, 0.9999999999999997780, 1.000000000000000222, 0.9999999999999997780, 1.000000000000000222, 1.000000000000000000, 1.000000000000000000, 1.000000000000000000, 0.9999999999999996669, 1.000000000000000222, 0.9999999999999997780, 1.000000000000000000, 0.9999999999999997780, 1.000000000000000222, 0.9999999999999997780, 1.000000000000000444, 0.9999999999999996669, 1.000000000000000222, 1.000000000000000222, 1.000000000000000000, 1.000000000000000000, 0.9999999999999997780, 1.000000000000000222, 0.9999999999999997780, 1.000000000000000222, 0.9999999999999997780, 0.9999999999999997780, 1.000000000000000000, 1.000000000000000000, 1.000000000000000222, 1.000000000000000000, 1.000000000000000444, 0.9999999999999997780, 1.000000000000000222, 0.9999999999999997780, 0.9999999999999997780, 1.000000000000000222, 1.000000000000000000, 0.9999999999999997780, 1.000000000000000000, 1.000000000000000000, 1.000000000000000000, 0.9999999999999997780, 1.000000000000000444, 0.9999999999999997780, 1.000000000000000000, 1.000000000000000000),
 ( 0.3333333333333334259, 0.3333333333333334259, 0.3333333333333333703, 0.3333333333333334259, 0.3333333333333334259, 0.3333333333333334259, 0.3333333333333334259, 0.3333333333333332593, 0.3333333333333335369, 0.3333333333333332593, 0.3333333333333333703, 0.3333333333333334259, 0.3333333333333333703, 0.3333333333333332593, 0.3333333333333334814, 0.3333333333333332593, 0.3333333333333334259, 0.3333333333333334259, 0.3333333333333332593, 0.3333333333333335369, 0.3333333333333332038, 0.3333333333333335369, 0.3333333333333331483, 0.3333333333333334814, 0.3333333333333333148, 0.3333333333333333703, 0.3333333333333333703, 0.3333333333333333148, 0.3333333333333333703, 0.3333333333333333148, 0.3333333333333333703, 0.3333333333333333703, 0.3333333333333333703, 0.3333333333333333703, 0.3333333333333333703, 0.3333333333333333703, 0.3333333333333333148, 0.3333333333333333148, 0.3333333333333334259, 0.3333333333333332593, 0.3333333333333334259, 0.3333333333333333148, 0.3333333333333334259, 0.3333333333333333703, 0.3333333333333333148, 0.3333333333333334259, 0.3333333333333333703, 0.3333333333333333703, 0.3333333333333334259, 0.3333333333333333148, 0.3333333333333333703, 0.3333333333333332593, 0.3333333333333335369, 0.3333333333333333703, 0.3333333333333333148, 0.3333333333333334259, 0.3333333333333333703, 0.3333333333333333703, 0.3333333333333333148, 0.3333333333333333703, 0.3333333333333333703, 0.3333333333333334259, 0.3333333333333334259, 0.3333333333333334259, 0.3333333333333333703, 0.3333333333333333703, 0.3333333333333334259, 0.3333333333333333148, 0.3333333333333333703, 0.3333333333333334259, 0.3333333333333334259, 0.3333333333333332593, 0.3333333333333333703, 0.3333333333333334259, 0.3333333333333333703, 0.3333333333333334259, 0.3333333333333333148, 0.3333333333333334814, 0.3333333333333333148, 0.3333333333333332593, 0.3333333333333334259, 0.3333333333333333703, 0.3333333333333333148, 0.3333333333333333703, 0.3333333333333334259, 0.3333333333333334259, 0.3333333333333333148, 0.3333333333333333703, 0.3333333333333332593, 0.3333333333333333703, 0.3333333333333333703, 0.3333333333333333703, 0.3333333333333333703, 0.3333333333333333148, 0.3333333333333333703, 0.3333333333333333148, 0.3333333333333334259, 0.3333333333333333703, 0.3333333333333334259, 0.3333333333333333148, 0.3333333333333333703, 0.3333333333333333148, 0.3333333333333334259, 0.3333333333333333703, 0.3333333333333333703, 0.3333333333333333703, 0.3333333333333333703, 0.3333333333333333703, 0.3333333333333332593, 0.3333333333333333703, 0.3333333333333333703, 0.3333333333333335369, 0.3333333333333334259, 0.3333333333333333148, 0.3333333333333335369, 0.3333333333333333148, 0.3333333333333333703, 0.3333333333333333703, 0.3333333333333334259, 0.3333333333333333148, 0.3333333333333333703, 0.3333333333333334259, 0.3333333333333334259, 0.3333333333333333703, 0.3333333333333332593, 0.3333333333333334259, 0.3333333333333333703, 0.3333333333333334814, 0.3333333333333333148, 0.3333333333333333703, 0.3333333333333334259, 0.3333333333333333703, 0.3333333333333333148, 0.3333333333333333703, 0.3333333333333333148, 0.3333333333333334259, 0.3333333333333332593, 0.3333333333333334814, 0.3333333333333333703, 0.3333333333333334259, 0.3333333333333333703, 0.3333333333333333703, 0.3333333333333334259, 0.3333333333333333703, 0.3333333333333333703, 0.3333333333333333148, 0.3333333333333335924, 0.3333333333333333148, 0.3333333333333333703, 0.3333333333333334259, 0.3333333333333333148, 0.3333333333333334259, 0.3333333333333333148, 0.3333333333333334259, 0.3333333333333333703, 0.3333333333333334259, 0.3333333333333333703, 0.3333333333333333703, 0.3333333333333333703, 0.3333333333333334259, 0.3333333333333333703, 0.3333333333333334814, 0.3333333333333333148, 0.3333333333333334814, 0.3333333333333333148, 0.3333333333333333703, 0.3333333333333333148, 0.3333333333333333703, 0.3333333333333333703, 0.3333333333333333703, 0.3333333333333333703, 0.3333333333333333703, 0.3333333333333334259, 0.3333333333333333148, 0.3333333333333334259, 0.3333333333333333703, 0.3333333333333333703, 0.3333333333333333703, 0.3333333333333333703, 0.3333333333333333148, 0.3333333333333333703, 0.3333333333333334259, 0.3333333333333333148, 0.3333333333333334259, 0.3333333333333333148, 0.3333333333333333703, 0.3333333333333333703, 0.3333333333333333148, 0.3333333333333333703, 0.3333333333333334259, 0.3333333333333333148, 0.3333333333333334259, 0.3333333333333333703, 0.3333333333333332593, 0.3333333333333334814, 0.3333333333333332593, 0.3333333333333334259, 0.3333333333333333148, 0.3333333333333333703, 0.3333333333333334814, 0.3333333333333333703, 0.3333333333333333703, 0.3333333333333332593, 0.3333333333333334814, 0.3333333333333333148, 0.3333333333333333703, 0.3333333333333334259, 0.3333333333333333148, 0.3333333333333334259, 0.3333333333333333148, 0.3333333333333333703, 0.3333333333333333703, 0.3333333333333332593, 0.3333333333333333703, 0.3333333333333333703, 0.3333333333333334259, 0.3333333333333333148, 0.3333333333333334814, 0.3333333333333333703, 0.3333333333333334259, 0.3333333333333333148, 0.3333333333333334259, 0.3333333333333333703, 0.3333333333333333703, 0.3333333333333333703, 0.3333333333333333703, 0.3333333333333333148, 0.3333333333333334814, 0.3333333333333333703, 0.3333333333333333703, 0.3333333333333333148, 0.3333333333333334259, 0.3333333333333333703, 0.3333333333333332593, 0.3333333333333333703, 0.3333333333333333703, 0.3333333333333333703, 0.3333333333333334259, 0.3333333333333334259, 0.3333333333333333703, 0.3333333333333333703, 0.3333333333333333703, 0.3333333333333333703, 0.3333333333333334259, 0.3333333333333332593, 0.3333333333333335369, 0.3333333333333332038, 0.3333333333333333148, 0.3333333333333333703, 0.3333333333333333148, 0.3333333333333333148, 0.3333333333333334259, 0.3333333333333333703, 0.3333333333333333703, 0.3333333333333333703, 0.3333333333333334259, 0.3333333333333333148, 0.3333333333333334814, 0.3333333333333333703, 0.3333333333333334259, 0.3333333333333333703, 0.3333333333333333703, 0.3333333333333332593, 0.3333333333333333148, 0.3333333333333334814, 0.3333333333333333148, 0.3333333333333332593, 0.3333333333333334259, 0.3333333333333332038, 0.3333333333333334259, 0.3333333333333333148, 0.3333333333333333148, 0.3333333333333334259, 0.3333333333333333703, 0.3333333333333333703, 0.3333333333333333703, 0.3333333333333333703, 0.3333333333333334259, 0.3333333333333333148, 0.3333333333333333148, 0.3333333333333334259, 0.3333333333333333148, 0.3333333333333334259, 0.3333333333333333148, 0.3333333333333333703, 0.3333333333333334259, 0.3333333333333333148, 0.3333333333333334814, 0.3333333333333333148, 0.3333333333333334259, 0.3333333333333334259, 0.3333333333333333148, 0.3333333333333333148, 0.3333333333333335369, 0.3333333333333333148, 0.3333333333333333148, 0.3333333333333333703, 0.3333333333333335369, 0.3333333333333332593, 0.3333333333333335369, 0.3333333333333333148, 0.3333333333333333148, 0.3333333333333334259, 0.3333333333333333148, 0.3333333333333334259, 0.3333333333333333703, 0.3333333333333332593, 0.3333333333333333703, 0.3333333333333333148, 0.3333333333333334259, 0.3333333333333333148, 0.3333333333333334259, 0.3333333333333332593, 0.3333333333333335369, 0.3333333333333332038, 0.3333333333333334259, 0.3333333333333332593, 0.3333333333333335369, 0.3333333333333333148, 0.3333333333333334259, 0.3333333333333334259, 0.3333333333333333148, 0.3333333333333333148, 0.3333333333333334259, 0.3333333333333334814, 0.3333333333333333148, 0.3333333333333333148, 0.3333333333333334259, 0.3333333333333333703, 0.3333333333333334259, 0.3333333333333333148, 0.3333333333333333148, 0.3333333333333333703, 0.3333333333333333703, 0.3333333333333334814, 0.3333333333333333148, 0.3333333333333334259, 0.3333333333333333703, 0.3333333333333334259, 0.3333333333333334259, 0.3333333333333333148, 0.3333333333333333703, 0.3333333333333334259, 0.3333333333333333148, 0.3333333333333334814, 0.3333333333333333703, 0.3333333333333333148, 0.3333333333333333703, 0.3333333333333333148, 0.3333333333333334259, 0.3333333333333333148, 0.3333333333333333703, 0.3333333333333332593, 0.3333333333333334814, 0.3333333333333333703, 0.3333333333333334814, 0.3333333333333333148, 0.3333333333333334259, 0.3333333333333334814, 0.3333333333333333148, 0.3333333333333334259, 0.3333333333333332593, 0.3333333333333334259, 0.3333333333333333703, 0.3333333333333333703, 0.3333333333333333148, 0.3333333333333333148, 0.3333333333333334259, 0.3333333333333333148, 0.3333333333333334814, 0.3333333333333333148, 0.3333333333333335924, 0.3333333333333333148, 0.3333333333333334259, 0.3333333333333333148, 0.3333333333333333703, 0.3333333333333333703, 0.3333333333333334814, 0.3333333333333332593, 0.3333333333333333703, 0.3333333333333333703, 0.3333333333333334259, 0.3333333333333333148, 0.3333333333333334259, 0.3333333333333333703, 0.3333333333333333703, 0.3333333333333333703),
 ( 0.3333333333333334259, 0.3333333333333334259, 0.3333333333333333703, 0.3333333333333334259, 0.3333333333333334259, 0.3333333333333334259, 0.3333333333333334259, 0.3333333333333332593, 0.3333333333333335369, 0.3333333333333332593, 0.3333333333333333703, 0.3333333333333334259, 0.3333333333333333703, 0.3333333333333332593, 0.3333333333333334814, 0.3333333333333332593, 0.3333333333333334259, 0.3333333333333334259, 0.3333333333333332593, 0.3333333333333335369, 0.3333333333333332038, 0.3333333333333335369, 0.3333333333333331483, 0.3333333333333334814, 0.3333333333333333148, 0.3333333333333333703, 0.3333333333333333703, 0.3333333333333333148, 0.3333333333333333703, 0.3333333333333333148, 0.3333333333333333703, 0.3333333333333333703, 0.3333333333333333703, 0.3333333333333333703, 0.3333333333333333703, 0.3333333333333333703, 0.3333333333333333148, 0.3333333333333333148, 0.3333333333333334259, 0.3333333333333332593, 0.3333333333333334259, 0.3333333333333333148, 0.3333333333333334259, 0.3333333333333333703, 0.3333333333333333148, 0.3333333333333334259, 0.3333333333333333703, 0.3333333333333333703, 0.3333333333333334259, 0.3333333333333333148, 0.3333333333333333703, 0.3333333333333332593, 0.3333333333333335369, 0.3333333333333333703, 0.3333333333333333148, 0.3333333333333334259, 0.3333333333333333703, 0.3333333333333333703, 0.3333333333333333148, 0.3333333333333333703, 0.3333333333333333703, 0.3333333333333334259, 0.3333333333333334259, 0.3333333333333334259, 0.3333333333333333703, 0.3333333333333333703, 0.3333333333333334259, 0.3333333333333333148, 0.3333333333333333703, 0.3333333333333334259, 0.3333333333333334259, 0.3333333333333332593, 0.3333333333333333703, 0.3333333333333334259, 0.3333333333333333703, 0.3333333333333334259, 0.3333333333333333148, 0.3333333333333334814, 0.3333333333333333148, 0.3333333333333332593, 0.3333333333333334259, 0.3333333333333333703, 0.3333333333333333148, 0.3333333333333333703, 0.3333333333333334259, 0.3333333333333334259, 0.3333333333333333148, 0.3333333333333333703, 0.3333333333333332593, 0.3333333333333333703, 0.3333333333333333703, 0.3333333333333333703, 0.3333333333333333703, 0.3333333333333333148, 0.3333333333333333703, 0.3333333333333333148, 0.3333333333333334259, 0.3333333333333333703, 0.3333333333333334259, 0.3333333333333333148, 0.3333333333333333703, 0.3333333333333333148, 0.3333333333333334259, 0.3333333333333333703, 0.3333333333333333703, 0.3333333333333333703, 0.3333333333333333703, 0.3333333333333333703, 0.3333333333333332593, 0.3333333333333333703, 0.3333333333333333703, 0.3333333333333335369, 0.3333333333333334259, 0.3333333333333333148, 0.3333333333333335369, 0.3333333333333333148, 0.3333333333333333703, 0.3333333333333333703, 0.3333333333333334259, 0.3333333333333333148, 0.3333333333333333703, 0.3333333333333334259, 0.3333333333333334259, 0.3333333333333333703, 0.3333333333333332593, 0.3333333333333334259, 0.3333333333333333703, 0.3333333333333334814, 0.3333333333333333148, 0.3333333333333333703, 0.3333333333333334259, 0.3333333333333333703, 0.3333333333333333148, 0.3333333333333333703, 0.3333333333333333148, 0.3333333333333334259, 0.3333333333333332593, 0.3333333333333334814, 0.3333333333333333703, 0.3333333333333334259, 0.3333333333333333703, 0.3333333333333333703, 0.3333333333333334259, 0.3333333333333333703, 0.3333333333333333703, 0.3333333333333333148, 0.3333333333333335924, 0.3333333333333333148, 0.3333333333333333703, 0.3333333333333334259, 0.3333333333333333148, 0.3333333333333334259, 0.3333333333333333148, 0.3333333333333334259, 0.3333333333333333703, 0.3333333333333334259, 0.3333333333333333703, 0.3333333333333333703, 0.3333333333333333703, 0.3333333333333334259, 0.3333333333333333703, 0.3333333333333334814, 0.3333333333333333148, 0.3333333333333334814, 0.3333333333333333148, 0.3333333333333333703, 0.3333333333333333148, 0.3333333333333333703, 0.3333333333333333703, 0.3333333333333333703, 0.3333333333333333703, 0.3333333333333333703, 0.3333333333333334259, 0.3333333333333333148, 0.3333333333333334259, 0.3333333333333333703, 0.3333333333333333703, 0.3333333333333333703, 0.3333333333333333703, 0.3333333333333333148, 0.3333333333333333703, 0.3333333333333334259, 0.3333333333333333148, 0.3333333333333334259, 0.3333333333333333148, 0.3333333333333333703, 0.3333333333333333703, 0.3333333333333333148, 0.3333333333333333703, 0.3333333333333334259, 0.3333333333333333148, 0.3333333333333334259, 0.3333333333333333703, 0.3333333333333332593, 0.3333333333333334814, 0.3333333333333332593, 0.3333333333333334259, 0.3333333333333333148, 0.3333333333333333703, 0.3333333333333334814, 0.3333333333333333703, 0.3333333333333333703, 0.3333333333333332593, 0.3333333333333334814, 0.3333333333333333148, 0.3333333333333333703, 0.3333333333333334259, 0.3333333333333333148, 0.3333333333333334259, 0.3333333333333333148, 0.3333333333333333703, 0.3333333333333333703, 0.3333333333333332593, 0.3333333333333333703, 0.3333333333333333703, 0.3333333333333334259, 0.3333333333333333148, 0.3333333333333334814, 0.3333333333333333703, 0.3333333333333334259, 0.3333333333333333148, 0.3333333333333334259, 0.3333333333333333703, 0.3333333333333333703, 0.3333333333333333703, 0.3333333333333333703, 0.3333333333333333148, 0.3333333333333334814, 0.3333333333333333703, 0.3333333333333333703, 0.3333333333333333148, 0.3333333333333334259, 0.3333333333333333703, 0.3333333333333332593, 0.3333333333333333703, 0.3333333333333333703, 0.3333333333333333703, 0.3333333333333334259, 0.3333333333333334259, 0.3333333333333333703, 0.3333333333333333703, 0.3333333333333333703, 0.3333333333333333703, 0.3333333333333334259, 0.3333333333333332593, 0.3333333333333335369, 0.3333333333333332038, 0.3333333333333333148, 0.3333333333333333703, 0.3333333333333333148, 0.3333333333333333148, 0.3333333333333334259, 0.3333333333333333703, 0.3333333333333333703, 0.3333333333333333703, 0.3333333333333334259, 0.3333333333333333148, 0.3333333333333334814, 0.3333333333333333703, 0.3333333333333334259, 0.3333333333333333703, 0.3333333333333333703, 0.3333333333333332593, 0.3333333333333333148, 0.3333333333333334814, 0.3333333333333333148, 0.3333333333333332593, 0.3333333333333334259, 0.3333333333333332038, 0.3333333333333334259, 0.3333333333333333148, 0.3333333333333333148, 0.3333333333333334259, 0.3333333333333333703, 0.3333333333333333703, 0.3333333333333333703, 0.3333333333333333703, 0.3333333333333334259, 0.3333333333333333148, 0.3333333333333333148, 0.3333333333333334259, 0.3333333333333333148, 0.3333333333333334259, 0.3333333333333333148, 0.3333333333333333703, 0.3333333333333334259, 0.3333333333333333148, 0.3333333333333334814, 0.3333333333333333148, 0.3333333333333334259, 0.3333333333333334259, 0.3333333333333333148, 0.3333333333333333148, 0.3333333333333335369, 0.3333333333333333148, 0.3333333333333333148, 0.3333333333333333703, 0.3333333333333335369, 0.3333333333333332593, 0.3333333333333335369, 0.3333333333333333148, 0.3333333333333333148, 0.3333333333333334259, 0.3333333333333333148, 0.3333333333333334259, 0.3333333333333333703, 0.3333333333333332593, 0.3333333333333333703, 0.3333333333333333148, 0.3333333333333334259, 0.3333333333333333148, 0.3333333333333334259, 0.3333333333333332593, 0.3333333333333335369, 0.3333333333333332038, 0.3333333333333334259, 0.3333333333333332593, 0.3333333333333335369, 0.3333333333333333148, 0.3333333333333334259, 0.3333333333333334259, 0.3333333333333333148, 0.3333333333333333148, 0.3333333333333334259, 0.3333333333333334814, 0.3333333333333333148, 0.3333333333333333148, 0.3333333333333334259, 0.3333333333333333703, 0.3333333333333334259, 0.3333333333333333148, 0.3333333333333333148, 0.3333333333333333703, 0.3333333333333333703, 0.3333333333333334814, 0.3333333333333333148, 0.3333333333333334259, 0.3333333333333333703, 0.3333333333333334259, 0.3333333333333334259, 0.3333333333333333148, 0.3333333333333333703, 0.3333333333333334259, 0.3333333333333333148, 0.3333333333333334814, 0.3333333333333333703, 0.3333333333333333148, 0.3333333333333333703, 0.3333333333333333148, 0.3333333333333334259, 0.3333333333333333148, 0.3333333333333333703, 0.3333333333333332593, 0.3333333333333334814, 0.3333333333333333703, 0.3333333333333334814, 0.3333333333333333148, 0.3333333333333334259, 0.3333333333333334814, 0.3333333333333333148, 0.3333333333333334259, 0.3333333333333332593, 0.3333333333333334259, 0.3333333333333333703, 0.3333333333333333703, 0.3333333333333333148, 0.3333333333333333148, 0.3333333333333334259, 0.3333333333333333148, 0.3333333333333334814, 0.3333333333333333148, 0.3333333333333335924, 0.3333333333333333148, 0.3333333333333334259, 0.3333333333333333148, 0.3333333333333333703, 0.3333333333333333703, 0.3333333333333334814, 0.3333333333333332593, 0.3333333333333333703, 0.3333333333333333703, 0.3333333333333334259, 0.3333333333333333148, 0.3333333333333334259, 0.3333333333333333703, 0.3333333333333333703, 0.3333333333333333703),
 ( 1.000000000000000222, 1.000000000000000222, 1.000000000000000222, 1.000000000000000000, 1.000000000000000000, 1.000000000000000444, 1.000000000000000000, 0.9999999999999997780, 1.000000000000000444, 0.9999999999999997780, 0.9999999999999997780, 1.000000000000000222, 0.9999999999999997780, 0.9999999999999997780, 1.000000000000000444, 0.9999999999999997780, 1.000000000000000222, 1.000000000000000222, 0.9999999999999996669, 1.000000000000000222, 0.9999999999999996669, 1.000000000000000444, 0.9999999999999994449, 1.000000000000000444, 0.9999999999999996669, 1.000000000000000222, 1.000000000000000000, 0.9999999999999997780, 1.000000000000000222, 0.9999999999999997780, 1.000000000000000000, 0.9999999999999997780, 1.000000000000000000, 1.000000000000000222, 0.9999999999999996669, 1.000000000000000000, 0.9999999999999997780, 1.000000000000000000, 1.000000000000000444, 0.9999999999999996669, 1.000000000000000222, 1.000000000000000000, 1.000000000000000222, 1.000000000000000222, 0.9999999999999997780, 0.9999999999999997780, 1.000000000000000222, 0.9999999999999997780, 1.000000000000000222, 0.9999999999999997780, 0.9999999999999997780, 0.9999999999999997780, 1.000000000000000444, 1.000000000000000000, 0.9999999999999997780, 1.000000000000000222, 1.000000000000000000, 1.000000000000000000, 0.9999999999999997780, 1.000000000000000222, 1.000000000000000000, 1.000000000000000000, 1.000000000000000222, 1.000000000000000000, 1.000000000000000000, 1.000000000000000000, 1.000000000000000222, 1.000000000000000000, 0.9999999999999997780, 1.000000000000000444, 1.000000000000000000, 0.9999999999999997780, 1.000000000000000000, 1.000000000000000222, 0.9999999999999997780, 1.000000000000000222, 0.9999999999999996669, 1.000000000000000222, 1.000000000000000000, 1.000000000000000000, 1.000000000000000000, 1.000000000000000222, 0.9999999999999997780, 1.000000000000000000, 1.000000000000000222, 0.9999999999999997780, 1.000000000000000000, 1.000000000000000000, 0.9999999999999996669, 1.000000000000000000, 1.000000000000000000, 1.000000000000000222, 1.000000000000000000, 0.9999999999999997780, 1.000000000000000222, 0.9999999999999996669, 1.000000000000000222, 0.9999999999999997780, 1.000000000000000000, 1.000000000000000000, 1.000000000000000222, 0.9999999999999996669, 1.000000000000000444, 1.000000000000000000, 0.9999999999999997780, 1.000000000000000000, 1.000000000000000000, 1.000000000000000222, 0.9999999999999997780, 1.000000000000000000, 1.000000000000000222, 1.000000000000000444, 1.000000000000000000, 1.000000000000000000, 1.000000000000000444, 1.000000000000000000, 0.9999999999999997780, 1.000000000000000222, 1.000000000000000000, 1.000000000000000000, 1.000000000000000000, 1.000000000000000000, 1.000000000000000000, 1.000000000000000000, 0.9999999999999996669, 1.000000000000000222, 0.9999999999999997780, 1.000000000000000222, 1.000000000000000000, 0.9999999999999997780, 1.000000000000000222, 0.9999999999999997780, 0.9999999999999997780, 0.9999999999999997780, 1.000000000000000000, 1.000000000000000000, 0.9999999999999996669, 1.000000000000000444, 1.000000000000000222, 1.000000000000000000, 1.000000000000000000, 1.000000000000000222, 1.000000000000000222, 1.000000000000000000, 1.000000000000000222, 0.9999999999999996669, 1.000000000000000444, 0.9999999999999997780, 0.9999999999999997780, 1.000000000000000444, 1.000000000000000000, 1.000000000000000222, 0.9999999999999997780, 1.000000000000000222, 1.000000000000000000, 1.000000000000000222, 1.000000000000000000, 1.000000000000000000, 0.9999999999999996669, 1.000000000000000444, 1.000000000000000000, 1.000000000000000222, 0.9999999999999997780, 1.000000000000000000, 1.000000000000000000, 1.000000000000000000, 1.000000000000000000, 0.9999999999999997780, 1.000000000000000000, 1.000000000000000000, 1.000000000000000000, 1.000000000000000222, 1.000000000000000222, 0.9999999999999997780, 1.000000000000000000, 1.000000000000000000, 0.9999999999999997780, 1.000000000000000000, 1.000000000000000000, 1.000000000000000000, 1.000000000000000000, 1.000000000000000444, 0.9999999999999997780, 1.000000000000000222, 0.9999999999999997780, 1.000000000000000000, 1.000000000000000222, 0.9999999999999997780, 1.000000000000000222, 1.000000000000000000, 1.000000000000000000, 1.000000000000000000, 1.000000000000000000, 0.9999999999999997780, 1.000000000000000000, 1.000000000000000000, 1.000000000000000000, 1.000000000000000000, 1.000000000000000000, 1.000000000000000222, 1.000000000000000000, 1.000000000000000222, 0.9999999999999997780, 1.000000000000000222, 0.9999999999999997780, 1.000000000000000222, 1.000000000000000000, 0.9999999999999997780, 1.000000000000000222, 0.9999999999999996669, 1.000000000000000444, 1.000000000000000000, 0.9999999999999996669, 1.000000000000000222, 1.000000000000000000, 1.000000000000000222, 0.9999999999999997780, 1.000000000000000444, 1.000000000000000000, 1.000000000000000000, 0.9999999999999997780, 1.000000000000000222, 1.000000000000000000, 1.000000000000000000, 1.000000000000000000, 1.000000000000000222, 0.9999999999999997780, 1.000000000000000222, 1.000000000000000000, 0.9999999999999997780, 1.000000000000000000, 0.9999999999999997780, 1.000000000000000222, 0.9999999999999996669, 1.000000000000000000, 1.000000000000000000, 1.000000000000000000, 1.000000000000000444, 1.000000000000000222, 1.000000000000000000, 1.000000000000000000, 0.9999999999999997780, 0.9999999999999997780, 1.000000000000000444, 0.9999999999999996669, 1.000000000000000444, 0.9999999999999997780, 0.9999999999999997780, 1.000000000000000222, 0.9999999999999997780, 0.9999999999999996669, 1.000000000000000444, 0.9999999999999997780, 1.000000000000000222, 1.000000000000000222, 1.000000000000000000, 0.9999999999999997780, 1.000000000000000222, 1.000000000000000000, 1.000000000000000222, 1.000000000000000000, 1.000000000000000000, 0.9999999999999997780, 0.9999999999999997780, 1.000000000000000444, 0.9999999999999997780, 0.9999999999999997780, 1.000000000000000222, 0.9999999999999994449, 1.000000000000000222, 0.9999999999999997780, 1.000000000000000000, 0.9999999999999997780, 1.000000000000000000, 1.000000000000000000, 1.000000000000000000, 1.000000000000000000, 1.000000000000000000, 1.000000000000000000, 1.000000000000000000, 1.000000000000000222, 1.000000000000000000, 1.000000000000000000, 1.000000000000000000, 1.000000000000000000, 1.000000000000000000, 1.000000000000000000, 1.000000000000000000, 1.000000000000000222, 1.000000000000000000, 1.000000000000000222, 0.9999999999999997780, 1.000000000000000000, 1.000000000000000444, 1.000000000000000000, 1.000000000000000000, 1.000000000000000000, 1.000000000000000222, 0.9999999999999997780, 1.000000000000000444, 0.9999999999999997780, 1.000000000000000222, 1.000000000000000000, 1.000000000000000000, 1.000000000000000000, 1.000000000000000222, 0.9999999999999994449, 1.000000000000000222, 1.000000000000000000, 1.000000000000000000, 1.000000000000000000, 0.9999999999999997780, 0.9999999999999997780, 1.000000000000000444, 0.9999999999999996669, 1.000000000000000222, 0.9999999999999997780, 1.000000000000000444, 0.9999999999999997780, 1.000000000000000222, 1.000000000000000222, 0.9999999999999996669, 1.000000000000000222, 1.000000000000000000, 1.000000000000000444, 1.000000000000000000, 1.000000000000000000, 1.000000000000000222, 1.000000000000000000, 1.000000000000000000, 0.9999999999999997780, 0.9999999999999997780, 1.000000000000000000, 0.9999999999999997780, 1.000000000000000222, 1.000000000000000222, 1.000000000000000000, 1.000000000000000222, 1.000000000000000222, 1.000000000000000000, 0.9999999999999997780, 0.9999999999999997780, 1.000000000000000222, 0.9999999999999997780, 1.000000000000000222, 1.000000000000000000, 1.000000000000000000, 1.000000000000000000, 0.9999999999999996669, 1.000000000000000222, 0.9999999999999997780, 1.000000000000000000, 0.9999999999999997780, 1.000000000000000222, 0.9999999999999997780, 1.000000000000000444, 0.9999999999999996669, 1.000000000000000222, 1.000000000000000222, 1.000000000000000000, 1.000000000000000000, 0.9999999999999997780, 1.000000000000000222, 0.9999999999999997780, 1.000000000000000222, 0.9999999999999997780, 0.9999999999999997780, 1.000000000000000000, 1.000000000000000000, 1.000000000000000222, 1.000000000000000000, 1.000000000000000444, 0.9999999999999997780, 1.000000000000000222, 0.9999999999999997780, 0.9999999999999997780, 1.000000000000000222, 1.000000000000000000, 0.9999999999999997780, 1.000000000000000000, 1.000000000000000000, 1.000000000000000000, 0.9999999999999997780, 1.000000000000000444, 0.9999999999999997780, 1.000000000000000000, 1.000000000000000000),
 ( 0.3333333333333334259, 0.3333333333333334259, 0.3333333333333333703, 0.3333333333333334259, 0.3333333333333334259, 0.3333333333333334259, 0.3333333333333334259, 0.3333333333333332593, 0.3333333333333335369, 0.3333333333333332593, 0.3333333333333333703, 0.3333333333333334259, 0.3333333333333333703, 0.3333333333333332593, 0.3333333333333334814, 0.3333333333333332593, 0.3333333333333334259, 0.3333333333333334259, 0.3333333333333332593, 0.3333333333333335369, 0.3333333333333332038, 0.3333333333333335369, 0.3333333333333331483, 0.3333333333333334814, 0.3333333333333333148, 0.3333333333333333703, 0.3333333333333333703, 0.3333333333333333148, 0.3333333333333333703, 0.3333333333333333148, 0.3333333333333333703, 0.3333333333333333703, 0.3333333333333333703, 0.3333333333333333703, 0.3333333333333333703, 0.3333333333333333703, 0.3333333333333333148, 0.3333333333333333148, 0.3333333333333334259, 0.3333333333333332593, 0.3333333333333334259, 0.3333333333333333148, 0.3333333333333334259, 0.3333333333333333703, 0.3333333333333333148, 0.3333333333333334259, 0.3333333333333333703, 0.3333333333333333703, 0.3333333333333334259, 0.3333333333333333148, 0.3333333333333333703, 0.3333333333333332593, 0.3333333333333335369, 0.3333333333333333703, 0.3333333333333333148, 0.3333333333333334259, 0.3333333333333333703, 0.3333333333333333703, 0.3333333333333333148, 0.3333333333333333703, 0.3333333333333333703, 0.3333333333333334259, 0.3333333333333334259, 0.3333333333333334259, 0.3333333333333333703, 0.3333333333333333703, 0.3333333333333334259, 0.3333333333333333148, 0.3333333333333333703, 0.3333333333333334259, 0.3333333333333334259, 0.3333333333333332593, 0.3333333333333333703, 0.3333333333333334259, 0.3333333333333333703, 0.3333333333333334259, 0.3333333333333333148, 0.3333333333333334814, 0.3333333333333333148, 0.3333333333333332593, 0.3333333333333334259, 0.3333333333333333703, 0.3333333333333333148, 0.3333333333333333703, 0.3333333333333334259, 0.3333333333333334259, 0.3333333333333333148, 0.3333333333333333703, 0.3333333333333332593, 0.3333333333333333703, 0.3333333333333333703, 0.3333333333333333703, 0.3333333333333333703, 0.3333333333333333148, 0.3333333333333333703, 0.3333333333333333148, 0.3333333333333334259, 0.3333333333333333703, 0.3333333333333334259, 0.3333333333333333148, 0.3333333333333333703, 0.3333333333333333148, 0.3333333333333334259, 0.3333333333333333703, 0.3333333333333333703, 0.3333333333333333703, 0.3333333333333333703, 0.3333333333333333703, 0.3333333333333332593, 0.3333333333333333703, 0.3333333333333333703, 0.3333333333333335369, 0.3333333333333334259, 0.3333333333333333148, 0.3333333333333335369, 0.3333333333333333148, 0.3333333333333333703, 0.3333333333333333703, 0.3333333333333334259, 0.3333333333333333148, 0.3333333333333333703, 0.3333333333333334259, 0.3333333333333334259, 0.3333333333333333703, 0.3333333333333332593, 0.3333333333333334259, 0.3333333333333333703, 0.3333333333333334814, 0.3333333333333333148, 0.3333333333333333703, 0.3333333333333334259, 0.3333333333333333703, 0.3333333333333333148, 0.3333333333333333703, 0.3333333333333333148, 0.3333333333333334259, 0.3333333333333332593, 0.3333333333333334814, 0.3333333333333333703, 0.3333333333333334259, 0.3333333333333333703, 0.3333333333333333703, 0.3333333333333334259, 0.3333333333333333703, 0.3333333333333333703, 0.3333333333333333148, 0.3333333333333335924, 0.3333333333333333148, 0.3333333333333333703, 0.3333333333333334259, 0.3333333333333333148, 0.3333333333333334259, 0.3333333333333333148, 0.3333333333333334259, 0.3333333333333333703, 0.3333333333333334259, 0.3333333333333333703, 0.3333333333333333703, 0.3333333333333333703, 0.3333333333333334259, 0.3333333333333333703, 0.3333333333333334814, 0.3333333333333333148, 0.3333333333333334814, 0.3333333333333333148, 0.3333333333333333703, 0.3333333333333333148, 0.3333333333333333703, 0.3333333333333333703, 0.3333333333333333703, 0.3333333333333333703, 0.3333333333333333703, 0.3333333333333334259, 0.3333333333333333148, 0.3333333333333334259, 0.3333333333333333703, 0.3333333333333333703, 0.3333333333333333703, 0.3333333333333333703, 0.3333333333333333148, 0.3333333333333333703, 0.3333333333333334259, 0.3333333333333333148, 0.3333333333333334259, 0.3333333333333333148, 0.3333333333333333703, 0.3333333333333333703, 0.3333333333333333148, 0.3333333333333333703, 0.3333333333333334259, 0.3333333333333333148, 0.3333333333333334259, 0.3333333333333333703, 0.3333333333333332593, 0.3333333333333334814, 0.3333333333333332593, 0.3333333333333334259, 0.3333333333333333148, 0.3333333333333333703, 0.3333333333333334814, 0.3333333333333333703, 0.3333333333333333703, 0.3333333333333332593, 0.3333333333333334814, 0.3333333333333333148, 0.3333333333333333703, 0.3333333333333334259, 0.3333333333333333148, 0.3333333333333334259, 0.3333333333333333148, 0.3333333333333333703, 0.3333333333333333703, 0.3333333333333332593, 0.3333333333333333703, 0.3333333333333333703, 0.3333333333333334259, 0.3333333333333333148, 0.3333333333333334814, 0.3333333333333333703, 0.3333333333333334259, 0.3333333333333333148, 0.3333333333333334259, 0.3333333333333333703, 0.3333333333333333703, 0.3333333333333333703, 0.3333333333333333703, 0.3333333333333333148, 0.3333333333333334814, 0.3333333333333333703, 0.3333333333333333703, 0.3333333333333333148, 0.3333333333333334259, 0.3333333333333333703, 0.3333333333333332593, 0.3333333333333333703, 0.3333333333333333703, 0.3333333333333333703, 0.3333333333333334259, 0.3333333333333334259, 0.3333333333333333703, 0.3333333333333333703, 0.3333333333333333703, 0.3333333333333333703, 0.3333333333333334259, 0.3333333333333332593, 0.3333333333333335369, 0.3333333333333332038, 0.3333333333333333148, 0.3333333333333333703, 0.3333333333333333148, 0.3333333333333333148, 0.3333333333333334259, 0.3333333333333333703, 0.3333333333333333703, 0.3333333333333333703, 0.3333333333333334259, 0.3333333333333333148, 0.3333333333333334814, 0.3333333333333333703, 0.3333333333333334259, 0.3333333333333333703, 0.3333333333333333703, 0.3333333333333332593, 0.3333333333333333148, 0.3333333333333334814, 0.3333333333333333148, 0.3333333333333332593, 0.3333333333333334259, 0.3333333333333332038, 0.3333333333333334259, 0.3333333333333333148, 0.3333333333333333148, 0.3333333333333334259, 0.3333333333333333703, 0.3333333333333333703, 0.3333333333333333703, 0.3333333333333333703, 0.3333333333333334259, 0.3333333333333333148, 0.3333333333333333148, 0.3333333333333334259, 0.3333333333333333148, 0.3333333333333334259, 0.3333333333333333148, 0.3333333333333333703, 0.3333333333333334259, 0.3333333333333333148, 0.3333333333333334814, 0.3333333333333333148, 0.3333333333333334259, 0.3333333333333334259, 0.3333333333333333148, 0.3333333333333333148, 0.3333333333333335369, 0.3333333333333333148, 0.3333333333333333148, 0.3333333333333333703, 0.3333333333333335369, 0.3333333333333332593, 0.3333333333333335369, 0.3333333333333333148, 0.3333333333333333148, 0.3333333333333334259, 0.3333333333333333148, 0.3333333333333334259, 0.3333333333333333703, 0.3333333333333332593, 0.3333333333333333703, 0.3333333333333333148, 0.3333333333333334259, 0.3333333333333333148, 0.3333333333333334259, 0.3333333333333332593, 0.3333333333333335369, 0.3333333333333332038, 0.3333333333333334259, 0.3333333333333332593, 0.3333333333333335369, 0.3333333333333333148, 0.3333333333333334259, 0.3333333333333334259, 0.3333333333333333148, 0.3333333333333333148, 0.3333333333333334259, 0.3333333333333334814, 0.3333333333333333148, 0.3333333333333333148, 0.3333333333333334259, 0.3333333333333333703, 0.3333333333333334259, 0.3333333333333333148, 0.3333333333333333148, 0.3333333333333333703, 0.3333333333333333703, 0.3333333333333334814, 0.3333333333333333148, 0.3333333333333334259, 0.3333333333333333703, 0.3333333333333334259, 0.3333333333333334259, 0.3333333333333333148, 0.3333333333333333703, 0.3333333333333334259, 0.3333333333333333148, 0.3333333333333334814, 0.3333333333333333703, 0.3333333333333333148, 0.3333333333333333703, 0.3333333333333333148, 0.3333333333333334259, 0.3333333333333333148, 0.3333333333333333703, 0.3333333333333332593, 0.3333333333333334814, 0.3333333333333333703, 0.3333333333333334814, 0.3333333333333333148, 0.3333333333333334259, 0.3333333333333334814, 0.3333333333333333148, 0.3333333333333334259, 0.3333333333333332593, 0.3333333333333334259, 0.3333333333333333703, 0.3333333333333333703, 0.3333333333333333148, 0.3333333333333333148, 0.3333333333333334259, 0.3333333333333333148, 0.3333333333333334814, 0.3333333333333333148, 0.3333333333333335924, 0.3333333333333333148, 0.3333333333333334259, 0.3333333333333333148, 0.3333333333333333703, 0.3333333333333333703, 0.3333333333333334814, 0.3333333333333332593, 0.3333333333333333703, 0.3333333333333333703, 0.3333333333333334259, 0.3333333333333333148, 0.3333333333333334259, 0.3333333333333333703, 0.3333333333333333703, 0.3333333333333333703),
 ( 0.3333333333333334259, 0.3333333333333334259, 0.3333333333333333703, 0.3333333333333334259, 0.3333333333333334259, 0.3333333333333334259, 0.3333333333333334259, 0.3333333333333332593, 0.3333333333333335369, 0.3333333333333332593, 0.3333333333333333703, 0.3333333333333334259, 0.3333333333333333703, 0.3333333333333332593, 0.3333333333333334814, 0.3333333333333332593, 0.3333333333333334259, 0.3333333333333334259, 0.3333333333333332593, 0.3333333333333335369, 0.3333333333333332038, 0.3333333333333335369, 0.3333333333333331483, 0.3333333333333334814, 0.3333333333333333148, 0.3333333333333333703, 0.3333333333333333703, 0.3333333333333333148, 0.3333333333333333703, 0.3333333333333333148, 0.3333333333333333703, 0.3333333333333333703, 0.3333333333333333703, 0.3333333333333333703, 0.3333333333333333703, 0.3333333333333333703, 0.3333333333333333148, 0.3333333333333333148, 0.3333333333333334259, 0.3333333333333332593, 0.3333333333333334259, 0.3333333333333333148, 0.3333333333333334259, 0.3333333333333333703, 0.3333333333333333148, 0.3333333333333334259, 0.3333333333333333703, 0.3333333333333333703, 0.3333333333333334259, 0.3333333333333333148, 0.3333333333333333703, 0.3333333333333332593, 0.3333333333333335369, 0.3333333333333333703, 0.3333333333333333148, 0.3333333333333334259, 0.3333333333333333703, 0.3333333333333333703, 0.3333333333333333148, 0.3333333333333333703, 0.3333333333333333703, 0.3333333333333334259, 0.3333333333333334259, 0.3333333333333334259, 0.3333333333333333703, 0.3333333333333333703, 0.3333333333333334259, 0.3333333333333333148, 0.3333333333333333703, 0.3333333333333334259, 0.3333333333333334259, 0.3333333333333332593, 0.3333333333333333703, 0.3333333333333334259, 0.3333333333333333703, 0.3333333333333334259, 0.3333333333333333148, 0.3333333333333334814, 0.3333333333333333148, 0.3333333333333332593, 0.3333333333333334259, 0.3333333333333333703, 0.3333333333333333148, 0.3333333333333333703, 0.3333333333333334259, 0.3333333333333334259, 0.3333333333333333148, 0.3333333333333333703, 0.3333333333333332593, 0.3333333333333333703, 0.3333333333333333703, 0.3333333333333333703, 0.3333333333333333703, 0.3333333333333333148, 0.3333333333333333703, 0.3333333333333333148, 0.3333333333333334259, 0.3333333333333333703, 0.3333333333333334259, 0.3333333333333333148, 0.3333333333333333703, 0.3333333333333333148, 0.3333333333333334259, 0.3333333333333333703, 0.3333333333333333703, 0.3333333333333333703, 0.3333333333333333703, 0.3333333333333333703, 0.3333333333333332593, 0.3333333333333333703, 0.3333333333333333703, 0.3333333333333335369, 0.3333333333333334259, 0.3333333333333333148, 0.3333333333333335369, 0.3333333333333333148, 0.3333333333333333703, 0.3333333333333333703, 0.3333333333333334259, 0.3333333333333333148, 0.3333333333333333703, 0.3333333333333334259, 0.3333333333333334259, 0.3333333333333333703, 0.3333333333333332593, 0.3333333333333334259, 0.3333333333333333703, 0.3333333333333334814, 0.3333333333333333148, 0.3333333333333333703, 0.3333333333333334259, 0.3333333333333333703, 0.3333333333333333148, 0.3333333333333333703, 0.3333333333333333148, 0.3333333333333334259, 0.3333333333333332593, 0.3333333333333334814, 0.3333333333333333703, 0.3333333333333334259, 0.3333333333333333703, 0.3333333333333333703, 0.3333333333333334259, 0.3333333333333333703, 0.3333333333333333703, 0.3333333333333333148, 0.3333333333333335924, 0.3333333333333333148, 0.3333333333333333703, 0.3333333333333334259, 0.3333333333333333148, 0.3333333333333334259, 0.3333333333333333148, 0.3333333333333334259, 0.3333333333333333703, 0.3333333333333334259, 0.3333333333333333703, 0.3333333333333333703, 0.3333333333333333703, 0.3333333333333334259, 0.3333333333333333703, 0.3333333333333334814, 0.3333333333333333148, 0.3333333333333334814, 0.3333333333333333148, 0.3333333333333333703, 0.3333333333333333148, 0.3333333333333333703, 0.3333333333333333703, 0.3333333333333333703, 0.3333333333333333703, 0.3333333333333333703, 0.3333333333333334259, 0.3333333333333333148, 0.3333333333333334259, 0.3333333333333333703, 0.3333333333333333703, 0.3333333333333333703, 0.3333333333333333703, 0.3333333333333333148, 0.3333333333333333703, 0.3333333333333334259, 0.3333333333333333148, 0.3333333333333334259, 0.3333333333333333148, 0.3333333333333333703, 0.3333333333333333703, 0.3333333333333333148, 0.3333333333333333703, 0.3333333333333334259, 0.3333333333333333148, 0.3333333333333334259, 0.3333333333333333703, 0.3333333333333332593, 0.3333333333333334814, 0.3333333333333332593, 0.3333333333333334259, 0.3333333333333333148, 0.3333333333333333703, 0.3333333333333334814, 0.3333333333333333703, 0.3333333333333333703, 0.3333333333333332593, 0.3333333333333334814, 0.3333333333333333148, 0.3333333333333333703, 0.3333333333333334259, 0.3333333333333333148, 0.3333333333333334259, 0.3333333333333333148, 0.3333333333333333703, 0.3333333333333333703, 0.3333333333333332593, 0.3333333333333333703, 0.3333333333333333703, 0.3333333333333334259, 0.3333333333333333148, 0.3333333333333334814, 0.3333333333333333703, 0.3333333333333334259, 0.3333333333333333148, 0.3333333333333334259, 0.3333333333333333703, 0.3333333333333333703, 0.3333333333333333703, 0.3333333333333333703, 0.3333333333333333148, 0.3333333333333334814, 0.3333333333333333703, 0.3333333333333333703, 0.3333333333333333148, 0.3333333333333334259, 0.3333333333333333703, 0.3333333333333332593, 0.3333333333333333703, 0.3333333333333333703, 0.3333333333333333703, 0.3333333333333334259, 0.3333333333333334259, 0.3333333333333333703, 0.3333333333333333703, 0.3333333333333333703, 0.3333333333333333703, 0.3333333333333334259, 0.3333333333333332593, 0.3333333333333335369, 0.3333333333333332038, 0.3333333333333333148, 0.3333333333333333703, 0.3333333333333333148, 0.3333333333333333148, 0.3333333333333334259, 0.3333333333333333703, 0.3333333333333333703, 0.3333333333333333703, 0.3333333333333334259, 0.3333333333333333148, 0.3333333333333334814, 0.3333333333333333703, 0.3333333333333334259, 0.3333333333333333703, 0.3333333333333333703, 0.3333333333333332593, 0.3333333333333333148, 0.3333333333333334814, 0.3333333333333333148, 0.3333333333333332593, 0.3333333333333334259, 0.3333333333333332038, 0.3333333333333334259, 0.3333333333333333148, 0.3333333333333333148, 0.3333333333333334259, 0.3333333333333333703, 0.3333333333333333703, 0.3333333333333333703, 0.3333333333333333703, 0.3333333333333334259, 0.3333333333333333148, 0.3333333333333333148, 0.3333333333333334259, 0.3333333333333333148, 0.3333333333333334259, 0.3333333333333333148, 0.3333333333333333703, 0.3333333333333334259, 0.3333333333333333148, 0.3333333333333334814, 0.3333333333333333148, 0.3333333333333334259, 0.3333333333333334259, 0.3333333333333333148, 0.3333333333333333148, 0.3333333333333335369, 0.3333333333333333148, 0.3333333333333333148, 0.3333333333333333703, 0.3333333333333335369, 0.3333333333333332593, 0.3333333333333335369, 0.3333333333333333148, 0.3333333333333333148, 0.3333333333333334259, 0.3333333333333333148, 0.3333333333333334259, 0.3333333333333333703, 0.3333333333333332593, 0.3333333333333333703, 0.3333333333333333148, 0.3333333333333334259, 0.3333333333333333148, 0.3333333333333334259, 0.3333333333333332593, 0.3333333333333335369, 0.3333333333333332038, 0.3333333333333334259, 0.3333333333333332593, 0.3333333333333335369, 0.3333333333333333148, 0.3333333333333334259, 0.3333333333333334259, 0.3333333333333333148, 0.3333333333333333148, 0.3333333333333334259, 0.3333333333333334814, 0.3333333333333333148, 0.3333333333333333148, 0.3333333333333334259, 0.3333333333333333703, 0.3333333333333334259, 0.3333333333333333148, 0.3333333333333333148, 0.3333333333333333703, 0.3333333333333333703, 0.3333333333333334814, 0.3333333333333333148, 0.3333333333333334259, 0.3333333333333333703, 0.3333333333333334259, 0.3333333333333334259, 0.3333333333333333148, 0.3333333333333333703, 0.3333333333333334259, 0.3333333333333333148, 0.3333333333333334814, 0.3333333333333333703, 0.3333333333333333148, 0.3333333333333333703, 0.3333333333333333148, 0.3333333333333334259, 0.3333333333333333148, 0.3333333333333333703, 0.3333333333333332593, 0.3333333333333334814, 0.3333333333333333703, 0.3333333333333334814, 0.3333333333333333148, 0.3333333333333334259, 0.3333333333333334814, 0.3333333333333333148, 0.3333333333333334259, 0.3333333333333332593, 0.3333333333333334259, 0.3333333333333333703, 0.3333333333333333703, 0.3333333333333333148, 0.3333333333333333148, 0.3333333333333334259, 0.3333333333333333148, 0.3333333333333334814, 0.3333333333333333148, 0.3333333333333335924, 0.3333333333333333148, 0.3333333333333334259, 0.3333333333333333148, 0.3333333333333333703, 0.3333333333333333703, 0.3333333333333334814, 0.3333333333333332593, 0.3333333333333333703, 0.3333333333333333703, 0.3333333333333334259, 0.3333333333333333148, 0.3333333333333334259, 0.3333333333333333703, 0.3333333333333333703, 0.3333333333333333703),
 ( 1.000000000000000222, 1.000000000000000222, 1.000000000000000222, 1.000000000000000000, 1.000000000000000000, 1.000000000000000444, 1.000000000000000000, 0.9999999999999997780, 1.000000000000000444, 0.9999999999999997780, 0.9999999999999997780, 1.000000000000000222, 0.9999999999999997780, 0.9999999999999997780, 1.000000000000000444, 0.9999999999999997780, 1.000000000000000222, 1.000000000000000222, 0.9999999999999996669, 1.000000000000000222, 0.9999999999999996669, 1.000000000000000444, 0.9999999999999994449, 1.000000000000000444, 0.9999999999999996669, 1.000000000000000222, 1.000000000000000000, 0.9999999999999997780, 1.000000000000000222, 0.9999999999999997780, 1.000000000000000000, 0.9999999999999997780, 1.000000000000000000, 1.000000000000000222, 0.9999999999999996669, 1.000000000000000000, 0.9999999999999997780, 1.000000000000000000, 1.000000000000000444, 0.9999999999999996669, 1.000000000000000222, 1.000000000000000000, 1.000000000000000222, 1.000000000000000222, 0.9999999999999997780, 0.9999999999999997780, 1.000000000000000222, 0.9999999999999997780, 1.000000000000000222, 0.9999999999999997780, 0.9999999999999997780, 0.9999999999999997780, 1.000000000000000444, 1.000000000000000000, 0.9999999999999997780, 1.000000000000000222, 1.000000000000000000, 1.000000000000000000, 0.9999999999999997780, 1.000000000000000222, 1.000000000000000000, 1.000000000000000000, 1.000000000000000222, 1.000000000000000000, 1.000000000000000000, 1.000000000000000000, 1.000000000000000222, 1.000000000000000000, 0.9999999999999997780, 1.000000000000000444, 1.000000000000000000, 0.9999999999999997780, 1.000000000000000000, 1.000000000000000222, 0.9999999999999997780, 1.000000000000000222, 0.9999999999999996669, 1.000000000000000222, 1.000000000000000000, 1.000000000000000000, 1.000000000000000000, 1.000000000000000222, 0.9999999999999997780, 1.000000000000000000, 1.000000000000000222, 0.9999999999999997780, 1.000000000000000000, 1.000000000000000000, 0.9999999999999996669, 1.000000000000000000, 1.000000000000000000, 1.000000000000000222, 1.000000000000000000, 0.9999999999999997780, 1.000000000000000222, 0.9999999999999996669, 1.000000000000000222, 0.9999999999999997780, 1.000000000000000000, 1.000000000000000000, 1.000000000000000222, 0.9999999999999996669, 1.000000000000000444, 1.000000000000000000, 0.9999999999999997780, 1.000000000000000000, 1.000000000000000000, 1.000000000000000222, 0.9999999999999997780, 1.000000000000000000, 1.000000000000000222, 1.000000000000000444, 1.000000000000000000, 1.000000000000000000, 1.000000000000000444, 1.000000000000000000, 0.9999999999999997780, 1.000000000000000222, 1.000000000000000000, 1.000000000000000000, 1.000000000000000000, 1.000000000000000000, 1.000000000000000000, 1.000000000000000000, 0.9999999999999996669, 1.000000000000000222, 0.9999999999999997780, 1.000000000000000222, 1.000000000000000000, 0.9999999999999997780, 1.000000000000000222, 0.9999999999999997780, 0.9999999999999997780, 0.9999999999999997780, 1.000000000000000000, 1.000000000000000000, 0.9999999999999996669, 1.000000000000000444, 1.000000000000000222, 1.000000000000000000, 1.000000000000000000, 1.000000000000000222, 1.000000000000000222, 1.000000000000000000, 1.000000000000000222, 0.9999999999999996669, 1.000000000000000444, 0.9999999999999997780, 0.9999999999999997780, 1.000000000000000444, 1.000000000000000000, 1.000000000000000222, 0.9999999999999997780, 1.000000000000000222, 1.000000000000000000, 1.000000000000000222, 1.000000000000000000, 1.000000000000000000, 0.9999999999999996669, 1.000000000000000444, 1.000000000000000000, 1.000000000000000222, 0.9999999999999997780, 1.000000000000000000, 1.000000000000000000, 1.000000000000000000, 1.000000000000000000, 0.9999999999999997780, 1.000000000000000000, 1.000000000000000000, 1.000000000000000000, 1.000000000000000222, 1.000000000000000222, 0.9999999999999997780, 1.000000000000000000, 1.000000000000000000, 0.9999999999999997780, 1.000000000000000000, 1.000000000000000000, 1.000000000000000000, 1.000000000000000000, 1.000000000000000444, 0.9999999999999997780, 1.000000000000000222, 0.9999999999999997780, 1.000000000000000000, 1.000000000000000222, 0.9999999999999997780, 1.000000000000000222, 1.000000000000000000, 1.000000000000000000, 1.000000000000000000, 1.000000000000000000, 0.9999999999999997780, 1.000000000000000000, 1.000000000000000000, 1.000000000000000000, 1.000000000000000000, 1.000000000000000000, 1.000000000000000222, 1.000000000000000000, 1.000000000000000222, 0.9999999999999997780, 1.000000000000000222, 0.9999999999999997780, 1.000000000000000222, 1.000000000000000000, 0.9999999999999997780, 1.000000000000000222, 0.9999999999999996669, 1.000000000000000444, 1.000000000000000000, 0.9999999999999996669, 1.000000000000000222, 1.000000000000000000, 1.000000000000000222, 0.9999999999999997780, 1.000000000000000444, 1.000000000000000000, 1.000000000000000000, 0.9999999999999997780, 1.000000000000000222, 1.000000000000000000, 1.000000000000000000, 1.000000000000000000, 1.000000000000000222, 0.9999999999999997780, 1.000000000000000222, 1.000000000000000000, 0.9999999999999997780, 1.000000000000000000, 0.9999999999999997780, 1.000000000000000222, 0.9999999999999996669, 1.000000000000000000, 1.000000000000000000, 1.000000000000000000, 1.000000000000000444, 1.000000000000000222, 1.000000000000000000, 1.000000000000000000, 0.9999999999999997780, 0.9999999999999997780, 1.000000000000000444, 0.9999999999999996669, 1.000000000000000444, 0.9999999999999997780, 0.9999999999999997780, 1.000000000000000222, 0.9999999999999997780, 0.9999999999999996669, 1.000000000000000444, 0.9999999999999997780, 1.000000000000000222, 1.000000000000000222, 1.000000000000000000, 0.9999999999999997780, 1.000000000000000222, 1.000000000000000000, 1.000000000000000222, 1.000000000000000000, 1.000000000000000000, 0.9999999999999997780, 0.9999999999999997780, 1.000000000000000444, 0.9999999999999997780, 0.9999999999999997780, 1.000000000000000222, 0.9999999999999994449, 1.000000000000000222, 0.9999999999999997780, 1.000000000000000000, 0.9999999999999997780, 1.000000000000000000, 1.000000000000000000, 1.000000000000000000, 1.000000000000000000, 1.000000000000000000, 1.000000000000000000, 1.000000000000000000, 1.000000000000000222, 1.000000000000000000, 1.000000000000000000, 1.000000000000000000, 1.000000000000000000, 1.000000000000000000, 1.000000000000000000, 1.000000000000000000, 1.000000000000000222, 1.000000000000000000, 1.000000000000000222, 0.9999999999999997780, 1.000000000000000000, 1.000000000000000444, 1.000000000000000000, 1.000000000000000000, 1.000000000000000000, 1.000000000000000222, 0.9999999999999997780, 1.000000000000000444, 0.9999999999999997780, 1.000000000000000222, 1.000000000000000000, 1.000000000000000000, 1.000000000000000000, 1.000000000000000222, 0.9999999999999994449, 1.000000000000000222, 1.000000000000000000, 1.000000000000000000, 1.000000000000000000, 0.9999999999999997780, 0.9999999999999997780, 1.000000000000000444, 0.9999999999999996669, 1.000000000000000222, 0.9999999999999997780, 1.000000000000000444, 0.9999999999999997780, 1.000000000000000222, 1.000000000000000222, 0.9999999999999996669, 1.000000000000000222, 1.000000000000000000, 1.000000000000000444, 1.000000000000000000, 1.000000000000000000, 1.000000000000000222, 1.000000000000000000, 1.000000000000000000, 0.9999999999999997780, 0.9999999999999997780, 1.000000000000000000, 0.9999999999999997780, 1.000000000000000222, 1.000000000000000222, 1.000000000000000000, 1.000000000000000222, 1.000000000000000222, 1.000000000000000000, 0.9999999999999997780, 0.9999999999999997780, 1.000000000000000222, 0.9999999999999997780, 1.000000000000000222, 1.000000000000000000, 1.000000000000000000, 1.000000000000000000, 0.9999999999999996669, 1.000000000000000222, 0.9999999999999997780, 1.000000000000000000, 0.9999999999999997780, 1.000000000000000222, 0.9999999999999997780, 1.000000000000000444, 0.9999999999999996669, 1.000000000000000222, 1.000000000000000222, 1.000000000000000000, 1.000000000000000000, 0.9999999999999997780, 1.000000000000000222, 0.9999999999999997780, 1.000000000000000222, 0.9999999999999997780, 0.9999999999999997780, 1.000000000000000000, 1.000000000000000000, 1.000000000000000222, 1.000000000000000000, 1.000000000000000444, 0.9999999999999997780, 1.000000000000000222, 0.9999999999999997780, 0.9999999999999997780, 1.000000000000000222, 1.000000000000000000, 0.9999999999999997780, 1.000000000000000000, 1.000000000000000000, 1.000000000000000000, 0.9999999999999997780, 1.000000000000000444, 0.9999999999999997780, 1.000000000000000000, 1.000000000000000000) ) ) 
 REPRESENTATION_ITEM ( '' )  SURFACE ( )  );
#146020 = CARTESIAN_POINT ( 'NONE',  ( -1.402160292154681736E-14, 10.73437500034139624, 1.575800808251682339 ) ) ;
#146022 = CARTESIAN_POINT ( 'NONE',  ( 5.479139036522528983, -1.730609802697373079, -0.8137914003483390779 ) ) ;
#146023 = CARTESIAN_POINT ( 'NONE',  ( -9.215791728987058562, 11.77484298861683598, -1.599625672291263179 ) ) ;
#146024 = STYLED_ITEM ( 'NONE', ( #16334 ), #60799 ) ;
#146025 = CARTESIAN_POINT ( 'NONE',  ( 6.714312387265682247, 8.856450423275211037, 1.599625672291281386 ) ) ;
#146026 = MECHANICAL_DESIGN_GEOMETRIC_PRESENTATION_REPRESENTATION (  '', ( #69753 ), #125222 ) ;
#146027 = CARTESIAN_POINT ( 'NONE',  ( 1.360316468749971586, 1.026041667008143143, 0.7853790794158540534 ) ) ;
#146028 = CARTESIAN_POINT ( 'NONE',  ( 3.456965981360264895, 6.016582164020185530, -1.082531754730543971 ) ) ;
#146029 = CARTESIAN_POINT ( 'NONE',  ( 0.5031362391596030381, -1.832460416942282011, 0.1798594046882526221 ) ) ;
#146030 = ORIENTED_EDGE ( 'NONE', *, *, #108972, .F. ) ;
#146031 = PRESENTATION_STYLE_ASSIGNMENT (( #79924 ) ) ;
#146032 = CARTESIAN_POINT ( 'NONE',  ( 4.217926093758465278, -0.9595593063399066036, -1.605508702137818045 ) ) ;
#146033 = CARTESIAN_POINT ( 'NONE',  ( -0.02299388927986567924, 0.7252709198883336983, -1.993311845943528837 ) ) ;
#146034 = CARTESIAN_POINT ( 'NONE',  ( 7.180978637093494044, 8.406838493811077839, -1.199719254218452047 ) ) ;
#146035 = CARTESIAN_POINT ( 'NONE',  ( -5.804269833667989431, 7.239147048582937671, 1.181955602297209751 ) ) ;
#146036 = CARTESIAN_POINT ( 'NONE',  ( -6.236387472606158333, 7.338502141871059870, -1.082531754730544860 ) ) ;
#146037 = CARTESIAN_POINT ( 'NONE',  ( 5.196852952739813070, 4.957416621151553571, -0.7998128361456221525 ) ) ;
#146038 = CARTESIAN_POINT ( 'NONE',  ( 1.446085390411493199, -0.8901679511373729037, 1.756898273940428634 ) ) ;
#146039 = CARTESIAN_POINT ( 'NONE',  ( 2.196888872880573551, 1.802427395782604247, 0.9040921628407010413 ) ) ;
#146040 = CARTESIAN_POINT ( 'NONE',  ( -9.318531651294266638, 9.766041769465124034, -0.7998128361456291469 ) ) ;
#146041 = CARTESIAN_POINT ( 'NONE',  ( 4.908934136599710563, 7.884784371745123366, 1.199719254218451159 ) ) ;
#146042 = CARTESIAN_POINT ( 'NONE',  ( -11.92619526913699879, 10.90000000000000036, -1.328859060402686199 ) ) ;
#146043 = CARTESIAN_POINT ( 'NONE',  ( 2.185716925580234449, -0.9354795820612994417, 1.981881815340847730 ) ) ;
#146044 = CARTESIAN_POINT ( 'NONE',  ( -5.546112223000226216, 5.929839062422638918, -0.8878705470019981894 ) ) ;
#146045 = CARTESIAN_POINT ( 'NONE',  ( -9.755255220232635693, 11.33988483081495957, -1.199719254218441611 ) ) ;
#146046 = FACE_OUTER_BOUND ( 'NONE', #82457, .T. ) ;
#146047 = CARTESIAN_POINT ( 'NONE',  ( 3.687454593236886513, 7.245854758844370913, -0.7216878364869879769 ) ) ;
#146048 = CARTESIAN_POINT ( 'NONE',  ( -10.43233925736708301, 5.066585305077033752, -5.254699789447807134 ) ) ;
#146049 = CARTESIAN_POINT ( 'NONE',  ( 8.072990401933337168, 11.50590700464255356, -1.199719254218446718 ) ) ;
#146050 = CARTESIAN_POINT ( 'NONE',  ( -3.289951133708662212, 7.658661826346112811, -2.499999999999995115 ) ) ;
#146051 = CARTESIAN_POINT ( 'NONE',  ( 4.882344714696929877, 8.710169577206153591, -0.7216878364870458196 ) ) ;
#146052 = ORIENTED_EDGE ( 'NONE', *, *, #209026, .F. ) ;
#146054 = CARTESIAN_POINT ( 'NONE',  ( 1.699859389132576837, 1.389752512480733060, 1.456620396263593520 ) ) ;
#146053 = CARTESIAN_POINT ( 'NONE',  ( 5.108874002337426390, -0.2646564886703614006, 1.822002613180016883 ) ) ;
#146055 = CARTESIAN_POINT ( 'NONE',  ( 3.691010296293754323, -1.365721494773973754, -1.848513781679576251 ) ) ;
#146057 = CARTESIAN_POINT ( 'NONE',  ( 1.674410341579468442, 1.254762736130067502, -1.374450116433557856 ) ) ;
#146056 = CARTESIAN_POINT ( 'NONE',  ( -1.500000000000001110, 10.02083333333333393, 0.8660254037844418162 ) ) ;
#146058 = CARTESIAN_POINT ( 'NONE',  ( 0.000000000000000000, -1.946874999522044014, -3.793834371823813001 ) ) ;
#146059 = CARTESIAN_POINT ( 'NONE',  ( 5.537344615273096515, -0.04053095765194079242, 1.912125305397804009 ) ) ;
#146060 = CARTESIAN_POINT ( 'NONE',  ( -7.971304249830880373, 11.38727316052296601, 1.199719254218453823 ) ) ;
#146061 = EDGE_CURVE ( 'NONE', #60352, #94456, #93087, .T. ) ;
#146062 = CARTESIAN_POINT ( 'NONE',  ( -4.475600106286965918, 8.235634200727838916, 0.7216878364870338292 ) ) ;
#146064 = CARTESIAN_POINT ( 'NONE',  ( 3.836663719693265584, 0.2738035037005565053, 1.850374562403465983 ) ) ;
#146063 = CARTESIAN_POINT ( 'NONE',  ( 4.950766902526997804, -1.767019275552136115, -1.117201988274316049 ) ) ;
#146065 = CARTESIAN_POINT ( 'NONE',  ( 6.141480397310468575, 10.10888486359680982, 1.040834085586084257E-14 ) ) ;
#146066 = CARTESIAN_POINT ( 'NONE',  ( 6.269096963164666469, 1.759884223096353173, -0.5412972069449849544 ) ) ;
#146067 = VECTOR ( 'NONE', #38891, 1000.000000000000000 ) ;
#146068 = CARTESIAN_POINT ( 'NONE',  ( 3.225950485047770933, 5.851027101609320269, 1.199719254218450271 ) ) ;
#146069 = DIRECTION ( 'NONE',  ( 0.000000000000000000, -7.228014483236694583E-17, 1.000000000000000000 ) ) ;
#146070 = CARTESIAN_POINT ( 'NONE',  ( 5.180183349501196410, -0.9537450585986576579, 1.436990496349071833 ) ) ;
#146071 = CARTESIAN_POINT ( 'NONE',  ( -4.577849422908604637, 8.492574760035358494, -0.7998128361456281477 ) ) ;
#146072 = CARTESIAN_POINT ( 'NONE',  ( 0.8263334968928169877, 0.7041814825227004082, -1.584920328518927279 ) ) ;
#146073 = SURFACE_STYLE_USAGE ( .BOTH. , #62648 ) ;
#146074 = CARTESIAN_POINT ( 'NONE',  ( 1.882262909678013463, 3.299172163371834277, 0.4004916885352222677 ) ) ;
#146075 = CARTESIAN_POINT ( 'NONE',  ( 11.04536101718726293, 11.00590937888831000, -1.100000000000000311 ) ) ;
#146076 = DIRECTION ( 'NONE',  ( 0.000000000000000000, 1.000000000000000000, 0.000000000000000000 ) ) ;
#146077 = CARTESIAN_POINT ( 'NONE',  ( 4.381792451580825976, -2.079388800107518698, 0.6243644347086656499 ) ) ;
#146078 = CARTESIAN_POINT ( 'NONE',  ( 3.334410585898534674, 1.781380905032422746, 0.3990451814587444024 ) ) ;
#146079 = CARTESIAN_POINT ( 'NONE',  ( 0.8659734994756922433, -1.952832785578303199, 0.1866259229855101731 ) ) ;
#146080 = CARTESIAN_POINT ( 'NONE',  ( 0.1404439707000069981, 0.8148842331482269996, 1.954324566802398744 ) ) ;
#146082 = CARTESIAN_POINT ( 'NONE',  ( 0.6823417656249917140, 4.405208333674755394, 1.181850606188765695 ) ) ;
#146081 = CARTESIAN_POINT ( 'NONE',  ( 0.5512257746139355152, -1.939593085364198721, -1.221404215731338283 ) ) ;
#146083 = CARTESIAN_POINT ( 'NONE',  ( 5.690973801500785356, 5.856266416811339859, 2.500000000000011102 ) ) ;
#146084 = CARTESIAN_POINT ( 'NONE',  ( 9.511208455186636712, 11.05516360492796935, 1.199719254218453823 ) ) ;
#146085 = CARTESIAN_POINT ( 'NONE',  ( 2.508575005364023003, -2.114979441823850337, -0.1534387461676611220 ) ) ;
#146086 = CARTESIAN_POINT ( 'NONE',  ( -3.145128448690310830, 6.613140923539910787, -0.7216878364870267237 ) ) ;
#146087 = CARTESIAN_POINT ( 'NONE',  ( 5.598048612495534648, 5.756137568112394298, 0.6639549446901950036 ) ) ;
#146088 = CARTESIAN_POINT ( 'NONE',  ( -5.870317324592829067, 5.951051088220814300, -0.7216878364870197293 ) ) ;
#146089 = CIRCLE ( 'NONE', #156914, 2.500000000000000888 ) ;
#146090 = CARTESIAN_POINT ( 'NONE',  ( 0.6552395816744536194, 1.723207459482085202, -1.147090658606984892 ) ) ;
#146092 = CARTESIAN_POINT ( 'NONE',  ( -1.402160292154681736E-14, 13.84375000068279782, 1.732050807568881190 ) ) ;
#146091 = CARTESIAN_POINT ( 'NONE',  ( 6.983263157960360346, 2.057644363497754814, 2.260506123227977948 ) ) ;
#146094 = ORIENTED_EDGE ( 'NONE', *, *, #2148, .T. ) ;
#146093 = CARTESIAN_POINT ( 'NONE',  ( 2.157158246434082827, 0.4899616716134093108, 2.166440146811992040 ) ) ;
#146095 = CARTESIAN_POINT ( 'NONE',  ( 0.1769827672329090662, 1.709356359883105636, 1.537109589704383827 ) ) ;
#146097 = CARTESIAN_POINT ( 'NONE',  ( 5.735237406732953680, -0.04512126716067199617, -2.062225806692425945 ) ) ;
#146096 = CARTESIAN_POINT ( 'NONE',  ( 3.684065054611349144, 5.321161868511784299, -1.599625672291262513 ) ) ;
#146099 = CARTESIAN_POINT ( 'NONE',  ( 3.475000000000000533, -1.924999999999999600, 0.000000000000000000 ) ) ;
#146098 = CARTESIAN_POINT ( 'NONE',  ( 6.039231080244466199, 6.010467446565510130, 0.7998128361456352531 ) ) ;
#146100 = CARTESIAN_POINT ( 'NONE',  ( 4.712340909201580885, 7.655425606447271214, -1.199719254218452047 ) ) ;
#146101 = CARTESIAN_POINT ( 'NONE',  ( -3.285556943750000070, -2.646874999522041971, 0.000000000000000000 ) ) ;
#146102 = CARTESIAN_POINT ( 'NONE',  ( 0.1331565106231363538, 0.2470099659030860484, -1.980838409567912572 ) ) ;
#146103 = CARTESIAN_POINT ( 'NONE',  ( 5.917501325027624048, -1.028386522942719816, -1.527094029191010893 ) ) ;
#146105 = VERTEX_POINT ( 'NONE', #200135 ) ;
#146104 = CARTESIAN_POINT ( 'NONE',  ( 5.087333953625774008, 6.958308917361963886, 1.599625672291267398 ) ) ;
#146106 = CARTESIAN_POINT ( 'NONE',  ( 1.957592155046536941, 1.720466030779904454, -0.1226356519287794405 ) ) ;
#146107 = CARTESIAN_POINT ( 'NONE',  ( 0.6730650033222317363, 1.776164188848127878, -0.9548607967814757291 ) ) ;
#146108 = CARTESIAN_POINT ( 'NONE',  ( 1.364683531249988535, 3.717708333674750953, -0.7879004041258239610 ) ) ;
#146109 = CARTESIAN_POINT ( 'NONE',  ( 2.706632988724329891, -0.8634771713065221288, -2.091333714195188431 ) ) ;
#146110 = CARTESIAN_POINT ( 'NONE',  ( 4.389357127182037743, 1.881541760944308139, -0.9463713395347850277 ) ) ;
#146111 = CARTESIAN_POINT ( 'NONE',  ( -6.563555762791521531, 9.711213252348503744, 1.082531754730549967 ) ) ;
#146112 = CARTESIAN_POINT ( 'NONE',  ( 2.670886861492921316, 0.09125233944726543478, -1.767527270347787116 ) ) ;
#146113 = CARTESIAN_POINT ( 'NONE',  ( 5.666418135507635512, 8.698239360479199433, 1.199719254218462483 ) ) ;
#146115 = CARTESIAN_POINT ( 'NONE',  ( 5.109026413134919231, -0.3384823820529453964, 2.267118282965301379 ) ) ;
#146114 = CARTESIAN_POINT ( 'NONE',  ( 4.489158259456265121, 7.291082831790689056, -1.082531754730548412 ) ) ;
#146116 = CARTESIAN_POINT ( 'NONE',  ( -4.086893239515592136, 6.855460315155083251, 1.199719254218464037 ) ) ;
#146117 = CARTESIAN_POINT ( 'NONE',  ( 1.499999999999989120, 2.254166666666685970, 0.8660254037844524744 ) ) ;
#146118 = CARTESIAN_POINT ( 'NONE',  ( -0.1102773484824119410, -0.006951161900758255283, -2.203378182130751206 ) ) ;
#146119 = CARTESIAN_POINT ( 'NONE',  ( 4.646525747415945595, -1.761044916313101671, 1.304081410864160739 ) ) ;
#146120 = CARTESIAN_POINT ( 'NONE',  ( -4.973143418114339021, 4.696422164088486895, 0.7998128361456341429 ) ) ;
#146121 = CARTESIAN_POINT ( 'NONE',  ( 0.5500358407890573176, 7.827628757559660144, -1.923053904898945232 ) ) ;
#146122 = CARTESIAN_POINT ( 'NONE',  ( 6.621762855810419346, -0.4656160214656123730, 2.076383538966434017 ) ) ;
#146123 = CARTESIAN_POINT ( 'NONE',  ( 0.6823417656249917140, 3.342708333674754506, 1.181850606188765695 ) ) ;
#146124 = CARTESIAN_POINT ( 'NONE',  ( 3.158729500758109765, -1.458545141725621219, 1.258684350631077642 ) ) ;
#146125 = CARTESIAN_POINT ( 'NONE',  ( -8.012344526598182026E-15, 9.546875000341399797, -1.575800808251669460 ) ) ;
#146126 = CARTESIAN_POINT ( 'NONE',  ( -5.422898255786209099, 5.429062174613087599, -0.7216878364870207285 ) ) ;
#146127 = CARTESIAN_POINT ( 'NONE',  ( 5.467072749063267345, -1.670387955228332277, 1.306269166133757986 ) ) ;
#146128 = CARTESIAN_POINT ( 'NONE',  ( -6.455090533882213322, 6.703562842383589349, -0.7216878364870338292 ) ) ;
#146129 = EDGE_LOOP ( 'NONE', ( #58234, #104273, #125787, #151720 ) ) ;
#146131 =( NAMED_UNIT ( * ) SI_UNIT ( $, .STERADIAN. ) SOLID_ANGLE_UNIT ( ) );
#146130 = CARTESIAN_POINT ( 'NONE',  ( -4.123088112331656951, 6.864000993478624579, 1.082531754730549967 ) ) ;
#146132 = CARTESIAN_POINT ( 'NONE',  ( 3.571683402196252910, 6.254382171615883834, 1.199719254218462483 ) ) ;
#146133 = CARTESIAN_POINT ( 'NONE',  ( 6.567912610837368881, -1.126952994821692533, 1.456688911285822119 ) ) ;
#146134 = CARTESIAN_POINT ( 'NONE',  ( 1.500000000000001332, 11.15625000068279427, 0.000000000000000000 ) ) ;
#146135 = CARTESIAN_POINT ( 'NONE',  ( 4.909844308960606085, 4.783825108070185905, -0.2656215318195585540 ) ) ;
#146136 = CARTESIAN_POINT ( 'NONE',  ( 1.364683531249990311, 3.946875000341417028, 1.214306433183764966E-14 ) ) ;
#146137 = CARTESIAN_POINT ( 'NONE',  ( 2.260927701655718103, 1.706565837815830822, -0.3407169315452397984 ) ) ;
#146138 = CARTESIAN_POINT ( 'NONE',  ( 3.375617060122621194, 6.882044303544283537, 1.040834085586084257E-14 ) ) ;
#146139 = CARTESIAN_POINT ( 'NONE',  ( 0.4019237886466816012, 10.95758545099816317, -1.499999999999998668 ) ) ;
#146140 = CARTESIAN_POINT ( 'NONE',  ( 1.364683531249986537, 0.4677083336747514530, -0.7879004041258309554 ) ) ;
#146141 = CARTESIAN_POINT ( 'NONE',  ( -4.262896864317852419, 7.367918308143647010, -0.9672248769079903052 ) ) ;
#146142 = CARTESIAN_POINT ( 'NONE',  ( 6.561405286136595905, 0.3748316153167965403, -2.128808860954830795 ) ) ;
#146143 = CARTESIAN_POINT ( 'NONE',  ( -8.622095623286845978, 12.14652976288826913, 1.199719254218462483 ) ) ;
#146144 = CARTESIAN_POINT ( 'NONE',  ( -6.521108698048783126, 7.670676904887464786, -1.082531754730543083 ) ) ;
#146145 = CARTESIAN_POINT ( 'NONE',  ( 6.104392421991035711, -0.7735064434604683736, -2.018760209060527888 ) ) ;
#146147 = ORIENTED_EDGE ( 'NONE', *, *, #106908, .F. ) ;
#146146 = FACE_OUTER_BOUND ( 'NONE', #158219, .T. ) ;
#146148 = CARTESIAN_POINT ( 'NONE',  ( 1.364683531249988535, 4.405208333674754506, -0.7879004041258300672 ) ) ;
#146149 = CARTESIAN_POINT ( 'NONE',  ( 5.870382883074816149, -1.252475921811508019, 1.522319303672705848 ) ) ;
#146150 = CARTESIAN_POINT ( 'NONE',  ( 5.096919866207451300, 0.8898786499993548427, -1.487894112255260692 ) ) ;
#146152 = CARTESIAN_POINT ( 'NONE',  ( 1.874823134854076923, -0.1115055541827478930, -2.188858692977871279 ) ) ;
#146151 = CARTESIAN_POINT ( 'NONE',  ( 1.360316468749975582, -0.4635416663252802660, -0.7853790794159301036 ) ) ;
#146153 = CARTESIAN_POINT ( 'NONE',  ( 3.030630200643165573, 1.283085264563757599, -1.917795831646688320 ) ) ;
#146154 = CARTESIAN_POINT ( 'NONE',  ( 5.923136198411797615, -0.05496255519776967885, 2.060232511946280098 ) ) ;
#146155 = CARTESIAN_POINT ( 'NONE',  ( 0.9724825242501096145, -0.04715749842807348546, -1.941539141333733953 ) ) ;
#146156 = CARTESIAN_POINT ( 'NONE',  ( -4.717874267431199087, 8.448011045404303587, 1.040834085586084257E-14 ) ) ;
#146157 = CARTESIAN_POINT ( 'NONE',  ( -5.004894982100124068, 5.868074229652107121, 1.199719254218452935 ) ) ;
#146158 = DIRECTION ( 'NONE',  ( -5.551115123125765446E-17, 0.000000000000000000, 1.000000000000000000 ) ) ;
#146159 = CARTESIAN_POINT ( 'NONE',  ( 4.254221937059123881, 0.9039275175388861161, -1.918405034562712830 ) ) ;
#146160 = CARTESIAN_POINT ( 'NONE',  ( -0.3866913795912775842, 3.974415841077572509, 11.53480748357604035 ) ) ;
#146161 = CARTESIAN_POINT ( 'NONE',  ( 2.285779929129946098, 1.617817622347239803, -1.203354541732377658 ) ) ;
#146162 = CARTESIAN_POINT ( 'NONE',  ( -6.249945625775490399, 7.354319987235250267, 1.082531754730549967 ) ) ;
#146163 = CARTESIAN_POINT ( 'NONE',  ( 4.981566806912656631, 2.060606067865732527, -0.7902562557115796471 ) ) ;
#146164 = CARTESIAN_POINT ( 'NONE',  ( 3.879041346841291649, 7.539648981374564407, 1.040834085586084257E-14 ) ) ;
#146165 = FACE_OUTER_BOUND ( 'NONE', #117723, .T. ) ;
#146166 = CARTESIAN_POINT ( 'NONE',  ( 1.677086603292890824E-15, 14.57145996863935800, 11.92238957220009610 ) ) ;
#146167 = CARTESIAN_POINT ( 'NONE',  ( -5.399890319992785237, 9.521898816625391504, 0.7998128361456291469 ) ) ;
#146169 = CARTESIAN_POINT ( 'NONE',  ( 6.825078400183572036, 7.629137130509069387, 2.744348168701661095 ) ) ;
#146168 = CARTESIAN_POINT ( 'NONE',  ( -5.468737822882341781, 7.600800700804905219, 1.347914668206271038 ) ) ;
#146170 = CARTESIAN_POINT ( 'NONE',  ( 10.98549472050129694, 12.34270202721272014, -1.592011381755358723 ) ) ;
#146171 = VERTEX_POINT ( 'NONE', #70126 ) ;
#146172 = CARTESIAN_POINT ( 'NONE',  ( 4.996976137430897857, 1.714615628211055398, -1.143075302399678472 ) ) ;
#146173 = CARTESIAN_POINT ( 'NONE',  ( -1.360316468750010666, 2.869791667008063651, -0.7853790794158961308 ) ) ;
#146174 = CARTESIAN_POINT ( 'NONE',  ( 0.2331563151865486683, 0.005903526429595904942, -1.945944850731482934 ) ) ;
#146175 = CARTESIAN_POINT ( 'NONE',  ( -4.218558352146454915, 8.073401844146177453, 1.040834085586084257E-14 ) ) ;
#146176 = CARTESIAN_POINT ( 'NONE',  ( -4.899292406491858820, 6.809203455697518947, -1.599625672291271394 ) ) ;
#146177 = CARTESIAN_POINT ( 'NONE',  ( 3.422525317731230032, -0.8204878289409988090, -1.845699721510121183 ) ) ;
#146178 = CARTESIAN_POINT ( 'NONE',  ( -1.500000000000015099, 0.8791666666666874130, -0.8660254037844313801 ) ) ;
#146179 = CARTESIAN_POINT ( 'NONE',  ( 3.440018289565364817, 5.036440642624797626, 1.599625672291267398 ) ) ;
#146180 = CARTESIAN_POINT ( 'NONE',  ( 8.145751363712157911, 8.397798100619326078, -0.7998128361456281477 ) ) ;
#146181 = CARTESIAN_POINT ( 'NONE',  ( 2.518495319897054330, 1.347246837915631490, -1.559621528479130825 ) ) ;
#146182 = CARTESIAN_POINT ( 'NONE',  ( 3.129529892704606020, 0.4926417352555876872, 1.955172657653013957 ) ) ;
#146183 = CARTESIAN_POINT ( 'NONE',  ( -6.423886587202998655, 6.778203476158441987, 0.4838116631791135602 ) ) ;
#146184 = CARTESIAN_POINT ( 'NONE',  ( 6.017121246366603060, 5.914396297049491658, 1.040834085586084257E-14 ) ) ;
#146185 = AXIS2_PLACEMENT_3D ( 'NONE', #72022, #139199, #40640 ) ;
#146186 = CARTESIAN_POINT ( 'NONE',  ( -0.3421332810201531127, 7.155223633118590776, -1.971148363701348050 ) ) ;
#146187 = CARTESIAN_POINT ( 'NONE',  ( 0.8140990769837243013, 1.700254657383609036, 0.7068247239481675326 ) ) ;
#146188 = COLOUR_RGB ( '', 0.09019608, 0.27058824, 0.51372549) ;
#146189 = CARTESIAN_POINT ( 'NONE',  ( 6.410767893487317792, 1.638320036227768783, -1.478771730184471389 ) ) ;
#146190 = CARTESIAN_POINT ( 'NONE',  ( 5.387385936583818591, 7.378645907471495846, -1.599625672291283607 ) ) ;
#146191 = CARTESIAN_POINT ( 'NONE',  ( 2.899875653925917174, -0.6810940995312758650, 2.051530325002319799 ) ) ;
#146192 = CARTESIAN_POINT ( 'NONE',  ( -3.416291520963659512, 5.969128626890772615, 1.082531754730560403 ) ) ;
#146193 = CARTESIAN_POINT ( 'NONE',  ( 4.065693644434860587, 1.385821322041587145, 1.600864752689701076 ) ) ;
#146194 = CARTESIAN_POINT ( 'NONE',  ( 2.829810162582825139, -1.586297295151902986, 1.663386555757565555 ) ) ;
#146195 = EDGE_CURVE ( 'NONE', #28319, #41218, #182420, .T. ) ;
#146196 = CARTESIAN_POINT ( 'NONE',  ( -0.04573888721146443515, 3.402170834691579770, -2.080515066271528823 ) ) ;
#146197 = CARTESIAN_POINT ( 'NONE',  ( 1.287742131874554552, -0.8442722623961744777, 1.669378388412197767 ) ) ;
#146198 = CARTESIAN_POINT ( 'NONE',  ( 4.557473252141114983, 0.4328338235230348996, -1.923210603423119780 ) ) ;
#146199 = CARTESIAN_POINT ( 'NONE',  ( 5.050017674172561755, 0.9981218692422781924, 1.752141108012375437 ) ) ;
#146201 = FACE_OUTER_BOUND ( 'NONE', #36093, .T. ) ;
#146200 = CARTESIAN_POINT ( 'NONE',  ( 0.6823417656249899377, 3.926041667008085767, -1.181850606188754593 ) ) ;
#146203 = CARTESIAN_POINT ( 'NONE',  ( 5.918611218600786650, 1.415673333675367296, -1.559471542009479350 ) ) ;
#146202 = CARTESIAN_POINT ( 'NONE',  ( -6.063521013809733518, 8.097193820909906137, 1.599625672291283607 ) ) ;
#146204 = CARTESIAN_POINT ( 'NONE',  ( 5.063152511717405879, 4.908155404373435005, -0.2552525419090029835 ) ) ;
#146205 = CARTESIAN_POINT ( 'NONE',  ( 5.133733721068893807, 9.141106441222381918, 1.040834085586084257E-14 ) ) ;
#146206 = CARTESIAN_POINT ( 'NONE',  ( -5.526920175865215334, 9.599823971818089774, 0.7998128361456481317 ) ) ;
#146207 = CARTESIAN_POINT ( 'NONE',  ( 6.539320575229274013, 2.055156488754609878, 2.310649141506931681 ) ) ;
#146208 = CARTESIAN_POINT ( 'NONE',  ( 4.662937792257120684, -1.760523130880174314, -0.8874255463059472770 ) ) ;
#146209 = CARTESIAN_POINT ( 'NONE',  ( 5.906511930418064438, -2.010445946205151380, -0.1936997237232794822 ) ) ;
#146210 = CARTESIAN_POINT ( 'NONE',  ( 1.499999999999987121, -0.2145833326505137972, 0.8660254037844524744 ) ) ;
#146211 = CARTESIAN_POINT ( 'NONE',  ( 5.075001523147505189, -2.171532227461204556, -0.7813444033149226087 ) ) ;
#146212 = EDGE_CURVE ( 'NONE', #207748, #57355, #25838, .T. ) ;
#146213 = CARTESIAN_POINT ( 'NONE',  ( 2.114201203919101157, 2.057314814202032771, -0.1476098556340669499 ) ) ;
#146214 = CARTESIAN_POINT ( 'NONE',  ( 8.270110514656037637, 8.750809809961280550, 0.7216878364870458196 ) ) ;
#146215 = CARTESIAN_POINT ( 'NONE',  ( 4.342354338126830804, 8.288106837781779035, -0.7998128361456381397 ) ) ;
#146216 = CARTESIAN_POINT ( 'NONE',  ( 4.923546060418115822, 5.773167154356443120, -1.199719254218452047 ) ) ;
#146217 = CARTESIAN_POINT ( 'NONE',  ( 1.364683531249988535, 2.676041667008082214, 0.7879004041258500513 ) ) ;
#146218 = CARTESIAN_POINT ( 'NONE',  ( -0.7616689537640918273, 14.53077577685077415, 12.01010950169515468 ) ) ;
#146219 = CARTESIAN_POINT ( 'NONE',  ( 7.307481607641395094, 8.588111966078864512, -1.082531754730537976 ) ) ;
#146220 = CARTESIAN_POINT ( 'NONE',  ( 4.668535151219040280, -0.9243884330643321601, -1.964686384670484953 ) ) ;
#146221 = CARTESIAN_POINT ( 'NONE',  ( -3.286906687871170352, 6.405221329422087884, -0.7651497088209441300 ) ) ;
#146223 = CARTESIAN_POINT ( 'NONE',  ( 2.419273308677453826, -1.061688697878185206, -1.504126257600538974 ) ) ;
#146222 = CARTESIAN_POINT ( 'NONE',  ( -2.968872451712654126, 6.407508927065978632, 1.040834085586084257E-14 ) ) ;
#146225 = CARTESIAN_POINT ( 'NONE',  ( 6.620655732516659064, 6.039214117936751336, 2.421170424969817603 ) ) ;
#146224 = CARTESIAN_POINT ( 'NONE',  ( -0.6823417656249969321, 5.217708333674756283, -1.181850606188749264 ) ) ;
#146226 = CARTESIAN_POINT ( 'NONE',  ( 5.847271748948593029, 0.6375361197438635941, -2.096799129279611762 ) ) ;
#146227 = CARTESIAN_POINT ( 'NONE',  ( 6.928203230280113090, 14.48195938056039900, 9.797958971139216544 ) ) ;
#146228 = CARTESIAN_POINT ( 'NONE',  ( 6.174757231500850096, -2.146110616029934803, -0.7165941539545512828 ) ) ;
#146229 = CARTESIAN_POINT ( 'NONE',  ( -5.356222800695524811, 6.520424213373273936, -1.360004217313095953 ) ) ;
#146230 = CARTESIAN_POINT ( 'NONE',  ( 4.690754089986846509, 8.373302309308519042, 0.6171781843518510113 ) ) ;
#146231 = CARTESIAN_POINT ( 'NONE',  ( -4.936577328707246082, 8.773440960218172435, 0.000000000000000000 ) ) ;
#146232 = CARTESIAN_POINT ( 'NONE',  ( -7.465774003072983334, -6.268611901546733201, -7.465774003072939813 ) ) ;
#146233 = CARTESIAN_POINT ( 'NONE',  ( 6.714108650864204719, -0.8368934294483711955, -1.559304158387794015 ) ) ;
#146234 = CARTESIAN_POINT ( 'NONE',  ( 4.195951375888273382, 1.316525029674735947, 1.522990447314742424 ) ) ;
#146235 = CARTESIAN_POINT ( 'NONE',  ( 6.063521013809720195, 8.097193820909906137, 1.599625672291281386 ) ) ;
#146236 = CARTESIAN_POINT ( 'NONE',  ( 3.083145409929681335, -0.1532580487927890645, -2.100430568508942830 ) ) ;
#146237 = CARTESIAN_POINT ( 'NONE',  ( 2.196773704658647297, 1.712196953037805613, 0.8591283806286521552 ) ) ;
#146239 = ADVANCED_FACE ( 'NONE', ( #214221 ), #20323, .F. ) ;
#146238 = CARTESIAN_POINT ( 'NONE',  ( 3.551346171775753735, 6.230655402791975384, 1.199719254218462483 ) ) ;
#146240 = CARTESIAN_POINT ( 'NONE',  ( 2.928127725102438461, 1.051234477803453027, 1.665338043752979447 ) ) ;
#146241 = CARTESIAN_POINT ( 'NONE',  ( 1.393192293617943944, 1.414286473764417185, 1.224485199485196629 ) ) ;
#146242 = CARTESIAN_POINT ( 'NONE',  ( 2.154674626568295892, -0.5202524484802829585, -1.891573884155263396 ) ) ;
#146245 = ORIENTED_EDGE ( 'NONE', *, *, #122928, .T. ) ;
#146244 = CARTESIAN_POINT ( 'NONE',  ( 0.8262462788446511830, -0.8622288892402606431, -1.707089296137359158 ) ) ;
#146243 = CARTESIAN_POINT ( 'NONE',  ( 3.703458238649427692, -0.4988927697323896071, 1.651148375757867326 ) ) ;
#146247 = CARTESIAN_POINT ( 'NONE',  ( 4.636525346193557162, 7.392734756325715750, -1.082531754730549078 ) ) ;
#146246 = CARTESIAN_POINT ( 'NONE',  ( 1.313402753022639091, 1.947697196196996217, 1.037691534346518729 ) ) ;
#146248 = CARTESIAN_POINT ( 'NONE',  ( 0.6823417656249899377, 1.405208333674752508, 1.181850606188755259 ) ) ;
#146249 = CARTESIAN_POINT ( 'NONE',  ( 6.702024585102262400, -1.870183347854617262, 0.04844413084104796929 ) ) ;
#146250 = DIRECTION ( 'NONE',  ( 0.000000000000000000, 0.000000000000000000, -1.000000000000000000 ) ) ;
#146251 = CARTESIAN_POINT ( 'NONE',  ( 2.341816809502491381, 5.373577454990479119, -0.7037892630772487612 ) ) ;
#146252 = VECTOR ( 'NONE', #33424, 1000.000000000000000 ) ;
#146253 = VERTEX_POINT ( 'NONE', #166593 ) ;
#146254 = CARTESIAN_POINT ( 'NONE',  ( 6.702015291077846548, 0.7979701500827086624, -1.910492173269620508 ) ) ;
#146255 = CIRCLE ( 'NONE', #139281, 0.08000000000000020983 ) ;
#146256 = CARTESIAN_POINT ( 'NONE',  ( 0.5376586404672692998, 1.932363751568724641, -0.7437053376125392079 ) ) ;
#146257 = CARTESIAN_POINT ( 'NONE',  ( 0.7499999999999885647, 1.316666666666688190, -1.299038105676652899 ) ) ;
#146258 = CARTESIAN_POINT ( 'NONE',  ( 5.276094334012385367, 9.307193822989793475, 1.040834085586084257E-14 ) ) ;
#146259 = CARTESIAN_POINT ( 'NONE',  ( -6.692921386640485082, 10.96015871772258521, -0.7998128361456291469 ) ) ;
#146260 = CARTESIAN_POINT ( 'NONE',  ( 4.420840606507738357, 7.315341919971147355, 1.199719254218451159 ) ) ;
#146262 = ADVANCED_FACE ( 'NONE', ( #98392 ), #65850, .F. ) ;
#146261 = CARTESIAN_POINT ( 'NONE',  ( 5.707716976326653757, 1.605689621071492601, 1.385122894465253607 ) ) ;
#146263 = CARTESIAN_POINT ( 'NONE',  ( 3.061108821635398769, 6.793320401875094561, -0.7998128361456362523 ) ) ;
#146264 = CARTESIAN_POINT ( 'NONE',  ( -1.364683531250012516, 2.030208333674750953, 0.7879004041258379498 ) ) ;
#146265 = EDGE_CURVE ( 'NONE', #175731, #125736, #124334, .T. ) ;
#146266 = CARTESIAN_POINT ( 'NONE',  ( -1.499999999999997780, 2.400000000000020339, 1.214306433183764966E-14 ) ) ;
#146268 = CARTESIAN_POINT ( 'NONE',  ( 4.857899112398166075, 4.561970474086296079, 1.040834085586084257E-14 ) ) ;
#146267 = CARTESIAN_POINT ( 'NONE',  ( 6.637165056451467038, -0.09505199798197358496, -1.959668910398344233 ) ) ;
#146269 = CARTESIAN_POINT ( 'NONE',  ( 4.042342166264912606, 1.899327733865596946, -0.6766104081444987983 ) ) ;
#146270 = CARTESIAN_POINT ( 'NONE',  ( 3.749167220118687638, 0.2288279286139145163, -1.901904479094515210 ) ) ;
#146271 = DIRECTION ( 'NONE',  ( -0.000000000000000000, 1.000000000000000000, -0.000000000000000000 ) ) ;
#146272 = CIRCLE ( 'NONE', #49452, 10.75000000000000000 ) ;
#146273 = CARTESIAN_POINT ( 'NONE',  ( 1.857222401600963302, 0.3706860215506869727, -2.159823580554325329 ) ) ;
#146274 = CARTESIAN_POINT ( 'NONE',  ( 0.1335669894368813060, 0.6916768264315333870, -2.234939561487662818 ) ) ;
#146275 = CARTESIAN_POINT ( 'NONE',  ( -0.7500000000000006661, 0.8895833340161543035, -1.299038105676652011 ) ) ;
#146276 = CARTESIAN_POINT ( 'NONE',  ( 4.728775500204083215, 1.385159600073909258, -1.461172115097974622 ) ) ;
#146277 = CARTESIAN_POINT ( 'NONE',  ( -5.845536785786364931, 9.971543350059432598, 0.000000000000000000 ) ) ;
#146279 = CARTESIAN_POINT ( 'NONE',  ( 5.677400705446850715, 1.603760038662904286, 1.382376383168891998 ) ) ;
#146278 = CARTESIAN_POINT ( 'NONE',  ( -3.280709984826970516, 6.771319382366015383, 0.7216878364870317197 ) ) ;
#146280 = CARTESIAN_POINT ( 'NONE',  ( -1.402160292154681736E-14, 8.984375000341396245, 1.575800808251682339 ) ) ;
#146282 = CARTESIAN_POINT ( 'NONE',  ( -6.420668264523499147, 9.648474187656182366, 1.199719254218452935 ) ) ;
#146281 = CARTESIAN_POINT ( 'NONE',  ( 1.927394988521138774, -1.368145043076029133, -1.581016005797744262 ) ) ;
#146284 = EDGE_LOOP ( 'NONE', ( #75634, #3864 ) ) ;
#146283 = CARTESIAN_POINT ( 'NONE',  ( 0.3402809042804251227, 0.2871511109263942818, 1.700534619074739906 ) ) ;
#146285 = CARTESIAN_POINT ( 'NONE',  ( 5.937581207780954884, 9.014596278131406848, -1.199719254218440723 ) ) ;
#146286 = CARTESIAN_POINT ( 'NONE',  ( -7.834948825496940827, -6.134628647623485698, -7.720982897393570354 ) ) ;
#146287 = CARTESIAN_POINT ( 'NONE',  ( 7.679448064523580975, -6.453073674884648447, 7.727353211424090595 ) ) ;
#146288 = CARTESIAN_POINT ( 'NONE',  ( -0.1738264060025679902, -9.190401220100135049, 9.624818503329224839 ) ) ;
#146290 = CARTESIAN_POINT ( 'NONE',  ( 9.531018800282609504, 10.22186947652563305, 0.7216878364870458196 ) ) ;
#146289 = CARTESIAN_POINT ( 'NONE',  ( 6.120616281565444794, 9.228137197546649517, -1.199719254218440723 ) ) ;
#146291 = ORIENTED_EDGE ( 'NONE', *, *, #144973, .F. ) ;
#146292 = DIRECTION ( 'NONE',  ( -0.9982742078614211811, 0.000000000000000000, 0.05872483221476467591 ) ) ;
#146294 = CARTESIAN_POINT ( 'NONE',  ( 2.156637704053586901, 0.3978940469637832766, 1.767043172555267772 ) ) ;
#146293 = CARTESIAN_POINT ( 'NONE',  ( 6.527324610336440180, 6.579909898339485252, 0.7998128361456331437 ) ) ;
#146295 = CARTESIAN_POINT ( 'NONE',  ( -6.612626235163205024, 8.737816579155630592, -1.599625672291263179 ) ) ;
#146296 = CARTESIAN_POINT ( 'NONE',  ( 5.301401758143367893, 6.143722458377430584, 1.199719254218462483 ) ) ;
#146297 = CARTESIAN_POINT ( 'NONE',  ( 6.412080304620304538, 6.445458208337293549, -0.7998128361456481317 ) ) ;
#146298 = CARTESIAN_POINT ( 'NONE',  ( 6.639320575229249677, 4.701313753536039641, 2.359456658813867236 ) ) ;
#146299 = CARTESIAN_POINT ( 'NONE',  ( 4.318426605249491068, 7.201576024430431211, 1.005918518748824875 ) ) ;
#146300 = CARTESIAN_POINT ( 'NONE',  ( 8.432808358020004391, 12.78210081775797669, 0.7216878364870438212 ) ) ;
#146301 = ORIENTED_EDGE ( 'NONE', *, *, #11886, .F. ) ;
#146302 = CARTESIAN_POINT ( 'NONE',  ( 3.349909636924102596, -0.7564274094383013347, 1.700591413421480125 ) ) ;
#146303 = CARTESIAN_POINT ( 'NONE',  ( 0.08730790862205867198, -0.5103928513382477439, 1.846301284274171728 ) ) ;
#146304 = CARTESIAN_POINT ( 'NONE',  ( 6.792047303494690880, -0.8216981310003536043, 1.740383667632472875 ) ) ;
#146305 = FACE_OUTER_BOUND ( 'NONE', #40682, .T. ) ;
#146306 = CARTESIAN_POINT ( 'NONE',  ( 4.595929827128614420, 8.372548788374160722, -0.07784623617661419470 ) ) ;
#146307 = CARTESIAN_POINT ( 'NONE',  ( -2.168941388506379742, 5.474256019991960542, -0.7216878364870267237 ) ) ;
#146308 = CARTESIAN_POINT ( 'NONE',  ( 8.107412671292035355, 10.48173408797264194, 1.443375672974076540 ) ) ;
#146309 = CARTESIAN_POINT ( 'NONE',  ( 4.205875300247041260, 0.6677108253347485700, -1.852911535531636789 ) ) ;
#146310 = CARTESIAN_POINT ( 'NONE',  ( -3.242371291962510504, 6.934516940598226320, 1.040834085586084257E-14 ) ) ;
#146311 = CARTESIAN_POINT ( 'NONE',  ( -10.87904062401159422, 6.606773729959338759, 4.960639138626822486 ) ) ;
#146312 = PLANE ( 'NONE',  #184219 ) ;
#146313 = CARTESIAN_POINT ( 'NONE',  ( 0.3223637989299525941, 2.001183132641819906, 0.6049928108779398794 ) ) ;
#146314 = CARTESIAN_POINT ( 'NONE',  ( 4.393008644795362905, 7.016788222801661590, 1.284222742053114041 ) ) ;
#146315 = CARTESIAN_POINT ( 'NONE',  ( 5.877940811483009398, 1.147681995895684315, 1.547064007116766060 ) ) ;
#146316 = CARTESIAN_POINT ( 'NONE',  ( -6.531277313481209212, 8.642909503859968368, 1.599625672291283607 ) ) ;
#146317 = CARTESIAN_POINT ( 'NONE',  ( 0.000000000000000000, 1.000000000000000888, -4.500000000000000000 ) ) ;
#146318 = CARTESIAN_POINT ( 'NONE',  ( 1.946200625105892312, 0.8427435547867198062, -2.039832142532324255 ) ) ;
#146319 = CARTESIAN_POINT ( 'NONE',  ( -6.101747606705155924, 7.024000329443246926, 0.9821876679783679842 ) ) ;
#146320 = CARTESIAN_POINT ( 'NONE',  ( 0.3692113334803036606, -1.616751421056546789, -1.021125667832627260 ) ) ;
#146321 = ORIENTED_EDGE ( 'NONE', *, *, #114330, .T. ) ;
#146322 = ORIENTED_EDGE ( 'NONE', *, *, #13102, .T. ) ;
#146323 = CARTESIAN_POINT ( 'NONE',  ( 0.2034765232073352526, -1.520001300341488948, -1.252246736068510335 ) ) ;
#146324 = CARTESIAN_POINT ( 'NONE',  ( 1.628360684195095054, 0.1923838640373880249, 1.932526033267305765 ) ) ;
#146325 = CARTESIAN_POINT ( 'NONE',  ( 0.6321852052597470850, 0.2004073784105386835, -2.006138679842318862 ) ) ;
#146327 = CARTESIAN_POINT ( 'NONE',  ( 5.981279135395962676, -0.04703572473597864706, 1.860536724379359574 ) ) ;
#146326 = CARTESIAN_POINT ( 'NONE',  ( -6.818824913030298696, 6.919993584815607335, 0.7998128361456341429 ) ) ;
#146328 = CARTESIAN_POINT ( 'NONE',  ( 4.227110032410640095, 8.153655147779589996, 0.7998128361456271485 ) ) ;
#146329 = CARTESIAN_POINT ( 'NONE',  ( 3.469446951953614189E-15, 6.120000000000021423, 1.214306433183764966E-14 ) ) ;
#146330 = CARTESIAN_POINT ( 'NONE',  ( 1.440240048128890171, 7.355731858842234239, -4.317885097517412341 ) ) ;
#146331 = CARTESIAN_POINT ( 'NONE',  ( -5.259673527097670664, 8.223703984000886535, -1.199719254218446718 ) ) ;
#146332 = ADVANCED_FACE ( 'NONE', ( #8348 ), #38729, .F. ) ;
#146333 = CARTESIAN_POINT ( 'NONE',  ( -7.099629715411508890, 8.311931418515415615, 1.199719254218452047 ) ) ;
#146334 = CARTESIAN_POINT ( 'NONE',  ( 1.347511689332027807, 0.6317163119916607839, -2.098556723903362009 ) ) ;
#146335 = CARTESIAN_POINT ( 'NONE',  ( 3.714570900464278846, 5.356752022006865843, 1.443375672974062551 ) ) ;
#146336 = EDGE_LOOP ( 'NONE', ( #172661, #9388, #160346, #124628 ) ) ;
#146337 = DIRECTION ( 'NONE',  ( 0.000000000000000000, 0.000000000000000000, 1.000000000000000000 ) ) ;
#146338 = CARTESIAN_POINT ( 'NONE',  ( -9.499668754385632852, -7.246166700194470067, -0.07933194154487524519 ) ) ;
#146339 = CARTESIAN_POINT ( 'NONE',  ( 1.242498012622397674, 0.3540479964400863877, 1.790853789395550955 ) ) ;
#146340 = CARTESIAN_POINT ( 'NONE',  ( -2.598358995313378550, 6.183169261174235487, 0.7998128361456341429 ) ) ;
#146341 = MECHANICAL_DESIGN_GEOMETRIC_PRESENTATION_REPRESENTATION (  '', ( #211995 ), #104889 ) ;
#146342 = CARTESIAN_POINT ( 'NONE',  ( -0.2953305167033711820, 3.289220156445278320, -2.050567765197571113 ) ) ;
#146343 = CARTESIAN_POINT ( 'NONE',  ( 6.609000000000036401, 0.5823242425131782696, 2.053003180352876100 ) ) ;
#146344 = CARTESIAN_POINT ( 'NONE',  ( 8.380911511541880188, 12.92948053010758258, 0.7998128361456462443 ) ) ;
#146345 = COLOUR_RGB ( '', 0.66274510, 0.83137255, 0.94901961) ;
#146346 = CARTESIAN_POINT ( 'NONE',  ( 0.4340449649811276012, 0.9916047912509761142, -1.651568591070247116 ) ) ;
#146347 = CARTESIAN_POINT ( 'NONE',  ( 4.539869136473917877, 1.278287603951251183, 1.488235606430035274 ) ) ;
#146348 = CARTESIAN_POINT ( 'NONE',  ( -6.828502922777144768, 11.11833717654868892, 0.7998128361456481317 ) ) ;
#146349 = CARTESIAN_POINT ( 'NONE',  ( 5.983225862332436584, 5.874851682342960402, 0.7998128361456341429 ) ) ;
#146350 = CARTESIAN_POINT ( 'NONE',  ( 4.493798347139664529, -2.191065130646638437, -0.05333993539427539510 ) ) ;
#146351 = EDGE_CURVE ( 'NONE', #30079, #184155, #112934, .T. ) ;
#146352 = CARTESIAN_POINT ( 'NONE',  ( 6.609000000000034625, 7.052688111495289291, 2.598153854230552895 ) ) ;
#146353 = CARTESIAN_POINT ( 'NONE',  ( 4.012602964903419611, 0.7404812365185129419, 1.933494928807255375 ) ) ;
#146355 = CARTESIAN_POINT ( 'NONE',  ( -1.364683531250014514, 1.801041667008085767, -0.7879004041258289570 ) ) ;
#146354 = DIRECTION ( 'NONE',  ( 0.000000000000000000, 1.000000000000000000, 0.000000000000000000 ) ) ;
#146356 = VERTEX_POINT ( 'NONE', #139443 ) ;
#146357 = CARTESIAN_POINT ( 'NONE',  ( 3.674713919220749414, 1.665813291469726787, 1.584223201981638685 ) ) ;
#146358 = CARTESIAN_POINT ( 'NONE',  ( 7.944714827928050838, 9.331550723079971021, 1.082531754730558626 ) ) ;
#146360 = CARTESIAN_POINT ( 'NONE',  ( -4.989037340148921196, 5.883260320670900434, 1.082531754730560403 ) ) ;
#146359 = CARTESIAN_POINT ( 'NONE',  ( 6.102578539926878598, 7.252668063737060855, -1.082531754730548412 ) ) ;
#146361 = CARTESIAN_POINT ( 'NONE',  ( 6.620655732516652847, 2.468432086671234149, 2.210906647470804565 ) ) ;
#146362 = CARTESIAN_POINT ( 'NONE',  ( -8.100070429521727178, 8.414780020722290033, 0.7998128361456341429 ) ) ;
#146363 = CARTESIAN_POINT ( 'NONE',  ( 3.275267064432846098, 1.232403799581788251, 1.500778006584954749 ) ) ;
#146364 = ORIENTED_EDGE ( 'NONE', *, *, #93138, .T. ) ;
#146365 = ADVANCED_FACE ( 'NONE', ( #169785 ), #170855, .F. ) ;
#146366 = CARTESIAN_POINT ( 'NONE',  ( 5.115449499555525747, 1.566912803841558732, 1.096118974231160781 ) ) ;
#146367 = CARTESIAN_POINT ( 'NONE',  ( 4.664925512212582781, -1.541612441252750543, -0.7736475682248912245 ) ) ;
#146368 = CARTESIAN_POINT ( 'NONE',  ( 4.469935555517978720, -0.9463019959239076240, 1.780667052345537238 ) ) ;
#146369 = CARTESIAN_POINT ( 'NONE',  ( 5.432396523169654934, -1.810675156642663541, -1.416092387804610553 ) ) ;
#146370 = CARTESIAN_POINT ( 'NONE',  ( -0.3058401130151643388, -0.8903248038550014565, -3.276851707331648544 ) ) ;
#146371 = CARTESIAN_POINT ( 'NONE',  ( 0.3291288957359936318, 2.113116833900237967, 0.6364493931270903682 ) ) ;
#146373 = CARTESIAN_POINT ( 'NONE',  ( -3.363831509966360489, 6.938570838353784076, -0.7216878364870458196 ) ) ;
#146372 = CARTESIAN_POINT ( 'NONE',  ( -8.469039510030723861, 13.03229652834454733, 1.040834085586084257E-14 ) ) ;
#146374 = CARTESIAN_POINT ( 'NONE',  ( 6.380137019068807369, -0.9445444496645590826, 1.496399839161892897 ) ) ;
#146375 = CARTESIAN_POINT ( 'NONE',  ( 4.465470312728934132, -1.956561007648183192, -0.4872041746135646889 ) ) ;
#146377 = CARTESIAN_POINT ( 'NONE',  ( 2.150677785613893889, -1.770481577899532644, 1.455972101185269985 ) ) ;
#146376 = CARTESIAN_POINT ( 'NONE',  ( 6.550524494058025837, 7.671308660269694712, -1.199719254218452047 ) ) ;
#146378 = CARTESIAN_POINT ( 'NONE',  ( 1.481926975991064710, -0.2526488567047910361, -1.721760536436983680 ) ) ;
#146379 = AXIS2_PLACEMENT_3D ( 'NONE', #192363, #155623, #209679 ) ;
#146380 = CARTESIAN_POINT ( 'NONE',  ( 11.80251051724185807, 11.29999999999999893, -1.695257889419042874 ) ) ;
#146381 = CARTESIAN_POINT ( 'NONE',  ( 1.053531109644106678, 1.532759392139435128, -0.8104334526845609066 ) ) ;
#146382 = CARTESIAN_POINT ( 'NONE',  ( 1.360316468749965590, 1.067708333674703081, -0.7853790794159082322 ) ) ;
#146383 = CARTESIAN_POINT ( 'NONE',  ( -11.96533679318038068, 13.75246011186986372, -0.9151144679400586845 ) ) ;
#146384 = CARTESIAN_POINT ( 'NONE',  ( 1.434277768017662824, 1.292756205793591517, 1.744237601605197252 ) ) ;
#146385 = CARTESIAN_POINT ( 'NONE',  ( 2.624232735793774030, 2.001858099149746550, 0.2420302859193757539 ) ) ;
#146386 = CARTESIAN_POINT ( 'NONE',  ( -0.7500000000000006661, 1.889583334016155192, -1.299038105676652011 ) ) ;
#146387 = CARTESIAN_POINT ( 'NONE',  ( 0.2527871956496882122, -1.549381263408876830, 1.144551880545265465 ) ) ;
#146388 = CARTESIAN_POINT ( 'NONE',  ( 0.6823417656249969321, 13.52604166700806232, -1.181850606188757036 ) ) ;
#146389 = CARTESIAN_POINT ( 'NONE',  ( 2.180208177693909288, 2.177553952664741388, -0.4384792121874846460 ) ) ;
#146390 = EDGE_LOOP ( 'NONE', ( #87361, #188562, #205275 ) ) ;
#146391 = CARTESIAN_POINT ( 'NONE',  ( 6.773376349083136461, -7.473374494058229622, 6.661184041420955104 ) ) ;
#146392 = FACE_OUTER_BOUND ( 'NONE', #164283, .T. ) ;
#146393 = CARTESIAN_POINT ( 'NONE',  ( 8.535021395002688749, 9.916278701380017324, 1.199719254218462483 ) ) ;
#146394 = SURFACE_STYLE_FILL_AREA ( #118190 ) ;
#146395 = SURFACE_STYLE_USAGE ( .BOTH. , #64052 ) ;
#146396 = CARTESIAN_POINT ( 'NONE',  ( 5.144012499716256848, 0.5123920008897012712, 1.663301317158589754 ) ) ;
#146397 = CARTESIAN_POINT ( 'NONE',  ( 3.262109210011232108, -1.959739898415867154, 0.09363895518171151677 ) ) ;
#146399 = CARTESIAN_POINT ( 'NONE',  ( -6.222829318992474157, 10.20379193889247382, 0.000000000000000000 ) ) ;
#146398 = CARTESIAN_POINT ( 'NONE',  ( 4.359110081993588182, 5.044382169536003602, -1.199719254218452047 ) ) ;
#146400 = EDGE_CURVE ( 'NONE', #90832, #22501, #109530, .T. ) ;
#146401 = CARTESIAN_POINT ( 'NONE',  ( -1.478151113144027251, 4.278273110089232389, 0.2686735943297190454 ) ) ;
#146402 = CARTESIAN_POINT ( 'NONE',  ( 4.183118113821016948, -0.2165105290278953043, -2.252005913828499573 ) ) ;
#146403 = PRESENTATION_LAYER_ASSIGNMENT (  '', '', ( #28720 ) ) ;
#146404 = AXIS2_PLACEMENT_3D ( 'NONE', #68855, #49443, #181558 ) ;
#146405 = CARTESIAN_POINT ( 'NONE',  ( 0.8892172652632176488, 0.1500229334146038762, 2.057259515242230830 ) ) ;
#146406 = CARTESIAN_POINT ( 'NONE',  ( -7.366157530926372488, 7.488271962369228874, -0.7998128361456291469 ) ) ;
#146407 = CARTESIAN_POINT ( 'NONE',  ( 2.149658728627835469, -1.817393572686412107, -1.347411789871997057 ) ) ;
#146408 = EDGE_LOOP ( 'NONE', ( #90662, #19131 ) ) ;
#146409 = CARTESIAN_POINT ( 'NONE',  ( 1.499999999999987121, 1.077083334016148308, -0.8660254037844253849 ) ) ;
#146410 = CARTESIAN_POINT ( 'NONE',  ( 3.462029368274913477, 0.8381641302350505418, 1.672297462726477946 ) ) ;
#146411 = CARTESIAN_POINT ( 'NONE',  ( 1.968989728591052479, -1.700769290752032870, -0.3374826141460812168 ) ) ;
#146412 = CARTESIAN_POINT ( 'NONE',  ( 5.970311429539967740, -2.080533979117826782, -0.6889730390344513955 ) ) ;
#146413 = CARTESIAN_POINT ( 'NONE',  ( 0.09513611692719620150, -0.4880922032983874281, -2.160105283315365998 ) ) ;
#146414 = CARTESIAN_POINT ( 'NONE',  ( 4.206063578812153203, -2.156103337031569200, 0.1562769059922017589 ) ) ;
#146415 = CARTESIAN_POINT ( 'NONE',  ( 4.417874594837376101, 1.193482090904834925, -1.531842204047480616 ) ) ;
#146416 = CARTESIAN_POINT ( 'NONE',  ( -8.967828540435322182, 12.54988483289483980, 1.199719254218462483 ) ) ;
#146418 = ORIENTED_EDGE ( 'NONE', *, *, #192938, .T. ) ;
#146417 = DIRECTION ( 'NONE',  ( 0.000000000000000000, 0.000000000000000000, 1.000000000000000000 ) ) ;
#146419 = CARTESIAN_POINT ( 'NONE',  ( 0.1249994045006353610, -2.052053476427470269, 7.016016019767730053E-15 ) ) ;
#146420 = CARTESIAN_POINT ( 'NONE',  ( 4.062392026992976746, 7.509557588607558287, 0.5198811075141016591 ) ) ;
#146421 = CARTESIAN_POINT ( 'NONE',  ( 0.001123102408843089329, -7.189630408304394926, 9.584291988782279503 ) ) ;
#146423 = CARTESIAN_POINT ( 'NONE',  ( 6.047500043413473136, -1.423963828944514010, 1.427935028000301809 ) ) ;
#146422 = CIRCLE ( 'NONE', #181016, 0.07999999999999979350 ) ;
#146424 = CARTESIAN_POINT ( 'NONE',  ( -3.267151830768959098, 4.834763107362302748, -1.443375672974058777 ) ) ;
#146425 = CARTESIAN_POINT ( 'NONE',  ( 6.825640269476072497, 10.05066518344239412, 1.199719254218460707 ) ) ;
#146426 = CARTESIAN_POINT ( 'NONE',  ( 11.94105721237523277, 12.57259215598211100, 1.187919463087244720 ) ) ;
#146428 = CARTESIAN_POINT ( 'NONE',  ( -6.663994888585887288, -7.154544010627095219, 6.770610912236890044 ) ) ;
#146427 = CARTESIAN_POINT ( 'NONE',  ( 2.824607995650964209, 1.719152210223941823, 0.6149139946348627372 ) ) ;
#146429 = CARTESIAN_POINT ( 'NONE',  ( 11.00592642091246454, 11.11020272436436507, -1.444015479094874710 ) ) ;
#146430 = ORIENTED_EDGE ( 'NONE', *, *, #62981, .T. ) ;
#146431 = CARTESIAN_POINT ( 'NONE',  ( -4.407809337774280856, 7.196175756495025055, 1.082531754730549967 ) ) ;
#146432 = CARTESIAN_POINT ( 'NONE',  ( -1.642778471874998480, -3.638541666188710444, 2.845375778867863303 ) ) ;
#146433 = CARTESIAN_POINT ( 'NONE',  ( -7.160677686311960777, 11.50587440067263678, -0.7998128361456291469 ) ) ;
#146434 = CARTESIAN_POINT ( 'NONE',  ( 0.2112021888033519534, 1.676852382702203714, -1.125601893279993160 ) ) ;
#146435 = CARTESIAN_POINT ( 'NONE',  ( 0.6453774867190856801, 0.1600191834128759094, 2.114519675249281416 ) ) ;
#146436 = EDGE_CURVE ( 'NONE', #19108, #211395, #88557, .T. ) ;
#146437 = CIRCLE ( 'NONE', #98035, 1.000000000000000000 ) ;
#146438 = CARTESIAN_POINT ( 'NONE',  ( -5.367048706163331850, 7.354919138647580290, -1.599625672291271394 ) ) ;
#146439 = CARTESIAN_POINT ( 'NONE',  ( 3.354752944377597856, 6.001296637494123232, -1.199719254218446718 ) ) ;
#146440 = CARTESIAN_POINT ( 'NONE',  ( 0.1456854043008250221, -1.672057201651616642, -1.369741535119282982 ) ) ;
#146441 = CARTESIAN_POINT ( 'NONE',  ( 5.889296118903345700, -0.7283762112263308941, -1.880435897373772258 ) ) ;
#146442 = VERTEX_POINT ( 'NONE', #72265 ) ;
#146443 = VERTEX_POINT ( 'NONE', #9422 ) ;
#146444 = CARTESIAN_POINT ( 'NONE',  ( -8.513630394377489807, 12.01998699582738972, -1.199719254218446718 ) ) ;
#146445 = DIRECTION ( 'NONE',  ( -0.6507913734559641616, -0.7592566023653004592, 0.000000000000000000 ) ) ;
#146447 = ORIENTED_EDGE ( 'NONE', *, *, #108295, .T. ) ;
#146446 = CARTESIAN_POINT ( 'NONE',  ( -6.005335696210345020, 5.970922831858983315, 0.7998128361456281477 ) ) ;
#146448 = CARTESIAN_POINT ( 'NONE',  ( 6.270956187569860063, 6.991113019333711875, 0.9580997929081371822 ) ) ;
#146449 = CARTESIAN_POINT ( 'NONE',  ( 6.749375321999433908, -1.976647572034227140, -0.3960365597561604778 ) ) ;
#146450 = CARTESIAN_POINT ( 'NONE',  ( 4.136529068399773301, -1.600833271991594531, 0.9093273525555561898 ) ) ;
#146451 = CARTESIAN_POINT ( 'NONE',  ( 0.07700591528352926374, 4.093948292925152721, -2.465843965391618209 ) ) ;
#146452 = CARTESIAN_POINT ( 'NONE',  ( 3.616130377633751003, -2.273733826016415716, 0.3936331181264277612 ) ) ;
#146453 = CARTESIAN_POINT ( 'NONE',  ( 5.825163275726873202, 6.825053905550038991, 1.199719254218452047 ) ) ;
#146454 = CARTESIAN_POINT ( 'NONE',  ( 5.729794944320468097, -1.366427417996706417, -1.674954217032841974 ) ) ;
#146455 = CARTESIAN_POINT ( 'NONE',  ( 6.500244582748090139, 9.671036882259738121, 1.199719254218460707 ) ) ;
#146456 = CARTESIAN_POINT ( 'NONE',  ( 1.294366139777222369, 1.586748096885544745, -1.119478687268110173 ) ) ;
#146457 = CARTESIAN_POINT ( 'NONE',  ( -2.950870989268691957, 6.594433254122103349, -0.7998128361456281477 ) ) ;
#146458 = ORIENTED_EDGE ( 'NONE', *, *, #44801, .F. ) ;
#146459 = CARTESIAN_POINT ( 'NONE',  ( 4.815913765717094286, -1.849969270989433534, 1.363755144342413850 ) ) ;
#146460 = DIRECTION ( 'NONE',  ( -1.054711873393901277E-15, 0.8656921114426510133, 0.5005768354468321801 ) ) ;
#146461 = CARTESIAN_POINT ( 'NONE',  ( -5.679940009482361774, 5.591294530676332641, 0.7998128361456281477 ) ) ;
#146462 = CARTESIAN_POINT ( 'NONE',  ( 4.750782166719051069, -1.502237938222051650, 1.114538048626475986 ) ) ;
#146465 = CARTESIAN_POINT ( 'NONE',  ( -4.749098946536820520, 8.762642214260091933, 0.7998128361456281477 ) ) ;
#146464 = CARTESIAN_POINT ( 'NONE',  ( -1.500000000000001332, -0.3187499993171846735, 0.000000000000000000 ) ) ;
#146463 = CARTESIAN_POINT ( 'NONE',  ( 1.388764059443419407, -1.816923020173771830, -0.5969786173363604842 ) ) ;
#146466 = CARTESIAN_POINT ( 'NONE',  ( 3.141465813989018141, -1.946189201368169641, 1.040519825639886431 ) ) ;
#146467 = CARTESIAN_POINT ( 'NONE',  ( 4.729096653068339151, 4.411700938201493116, -0.7998128361456211532 ) ) ;
#146468 = CARTESIAN_POINT ( 'NONE',  ( 5.844973620822830895, 8.872867420051733234, 1.082531754730549967 ) ) ;
#146469 = CARTESIAN_POINT ( 'NONE',  ( -2.272963308585411735, 5.803540959991587478, 0.7998128361456341429 ) ) ;
#146470 = CARTESIAN_POINT ( 'NONE',  ( -5.844973620822877969, 7.912498205750389424, 1.443375672974058777 ) ) ;
#146471 = CARTESIAN_POINT ( 'NONE',  ( 1.247272744223869356, -1.551563771690873006, -1.215972028847669417 ) ) ;
#146472 = CARTESIAN_POINT ( 'NONE',  ( 0.7280630558558630616, -2.190032360377992315, 0.7273814547973026512 ) ) ;
#146474 = ADVANCED_FACE ( 'NONE', ( #171929 ), #122202, .F. ) ;
#146473 = CARTESIAN_POINT ( 'NONE',  ( 3.086327779807009009, 1.092107249913790712, -1.629585102321646328 ) ) ;
#146475 = CARTESIAN_POINT ( 'NONE',  ( 5.172745336439665387, 1.426162745032448109, -1.490257803364034128 ) ) ;
#146476 = CARTESIAN_POINT ( 'NONE',  ( 3.538314903486612817, 7.071858454135611538, 1.040834085586084257E-14 ) ) ;
#146477 = CARTESIAN_POINT ( 'NONE',  ( 5.662465432362883355, 6.635239754958710989, 1.199719254218451159 ) ) ;
#146478 = ORIENTED_EDGE ( 'NONE', *, *, #142755, .T. ) ;
#146479 = CARTESIAN_POINT ( 'NONE',  ( -9.917953063596627317, 11.52969898140628047, -1.199719254218441611 ) ) ;
#146480 = DIRECTION ( 'NONE',  ( -0.6483454320283799088, 0.000000000000000000, 0.7613463080411786432 ) ) ;
#146481 = CARTESIAN_POINT ( 'NONE',  ( 3.348500752450929596, 6.850408611260650815, 0.7216878364870317197 ) ) ;
#146482 = CARTESIAN_POINT ( 'NONE',  ( 0.7433368588017514877, -0.2641965325859591540, -2.154838077344235714 ) ) ;
#146484 = DIRECTION ( 'NONE',  ( -0.6507913734559658270, -0.7592566023652989049, 0.000000000000000000 ) ) ;
#146483 = CARTESIAN_POINT ( 'NONE',  ( -0.04582610853913851590, -10.00039265882532824, -11.00004154231846520 ) ) ;
#146485 = DIRECTION ( 'NONE',  ( 3.330669073875478989E-16, -3.540251991789410786E-16, -1.000000000000000000 ) ) ;
#146486 = DIRECTION ( 'NONE',  ( 0.000000000000000000, 0.000000000000000000, 1.000000000000000000 ) ) ;
#146487 = CARTESIAN_POINT ( 'NONE',  ( 2.653401028632852654, 0.5028369177751991215, -1.801603059227441239 ) ) ;
#146488 = CARTESIAN_POINT ( 'NONE',  ( 6.907524304660562109, -0.4813806915026208055, 2.115094849305596103 ) ) ;
#146489 = CARTESIAN_POINT ( 'NONE',  ( -6.123385318682658784, 6.005027156464323390, -0.2239653954101868127 ) ) ;
#146490 = CARTESIAN_POINT ( 'NONE',  ( 6.727182134110196721, 2.084960209934753284, 2.120171393779949565 ) ) ;
#146491 = CARTESIAN_POINT ( 'NONE',  ( -1.364683531250000748, 0.009375000341420303140, 0.000000000000000000 ) ) ;
#146492 = EDGE_CURVE ( 'NONE', #11760, #188370, #157871, .T. ) ;
#146493 = CARTESIAN_POINT ( 'NONE',  ( 2.719282321824310511, 1.616554633311767297, 1.021241153818429614 ) ) ;
#146494 = CIRCLE ( 'NONE', #53060, 0.07999999999999993228 ) ;
#146495 = CARTESIAN_POINT ( 'NONE',  ( 3.801397759637317186, -0.5140543387622575899, 1.693523888807080047 ) ) ;
#146496 = CARTESIAN_POINT ( 'NONE',  ( 1.857924044808876296, 0.7306008629870773818, -1.767408594711167735 ) ) ;
#146497 = CIRCLE ( 'NONE', #80758, 0.08000000000000020983 ) ;
#146498 = CARTESIAN_POINT ( 'NONE',  ( -5.904739593951539689, 6.847616600153594746, 1.199719254218450271 ) ) ;
#146500 = CARTESIAN_POINT ( 'NONE',  ( 5.765228759176680207, 1.768025090248021902, -0.7378185885129113775 ) ) ;
#146499 = CARTESIAN_POINT ( 'NONE',  ( 0.9110743962804412899, -3.148497594347263284, -3.249005144921567556 ) ) ;
#146501 = CARTESIAN_POINT ( 'NONE',  ( 6.760212172060996672, -1.969150147884619173, 0.04690145372830689663 ) ) ;
#146502 = CARTESIAN_POINT ( 'NONE',  ( 0.7499999999999902300, 4.566666666666691299, -1.299038105676658228 ) ) ;
#146503 = CARTESIAN_POINT ( 'NONE',  ( 2.215225606797793567, 1.700350911433265555, -1.266953333846132512 ) ) ;
#146504 = PLANE ( 'NONE',  #158798 ) ;
#146505 = CARTESIAN_POINT ( 'NONE',  ( 5.559403950928493821, 0.3636877230743483236, -1.834782481876767291 ) ) ;
#146507 = ORIENTED_EDGE ( 'NONE', *, *, #7130, .T. ) ;
#146506 = CARTESIAN_POINT ( 'NONE',  ( 0.3811277156573149583, 1.704729334087114578, -0.6539457117896373406 ) ) ;
#146509 = CARTESIAN_POINT ( 'NONE',  ( -0.7499999999999972244, 4.358333333333352932, -1.299038105676652011 ) ) ;
#146508 = CARTESIAN_POINT ( 'NONE',  ( 4.617920694193921705, -2.164688156338661962, 0.4286357439418769788 ) ) ;
#146510 = CARTESIAN_POINT ( 'NONE',  ( -1.402160292154681736E-14, -1.178124999658576311, 1.575800808251672791 ) ) ;
#146511 = CARTESIAN_POINT ( 'NONE',  ( 1.926308760915905527, 1.058537693354057785, 1.770204612073868145 ) ) ;
#146512 = CARTESIAN_POINT ( 'NONE',  ( 5.113396490648394632, 9.117379672398465473, 1.040834085586084257E-14 ) ) ;
#146513 = CARTESIAN_POINT ( 'NONE',  ( -6.828502922777144768, 11.11833717654868892, 0.7998128361456481317 ) ) ;
#146514 = CARTESIAN_POINT ( 'NONE',  ( 8.028399517586572998, 12.51821653715971472, -0.7998128361456352531 ) ) ;
#146515 = CARTESIAN_POINT ( 'NONE',  ( 11.97929049433705728, 11.37999999999999901, -0.7046979865771821894 ) ) ;
#146516 = AXIS2_PLACEMENT_3D ( 'NONE', #129716, #79802, #162141 ) ;
#146517 = SURFACE_STYLE_FILL_AREA ( #195240 ) ;
#146518 = DIRECTION ( 'NONE',  ( 0.3162277660168373861, -0.9486832980505139901, 0.000000000000000000 ) ) ;
#146519 = ORIENTED_EDGE ( 'NONE', *, *, #152411, .F. ) ;
#146520 = CARTESIAN_POINT ( 'NONE',  ( 4.475093801846619535, 1.891600172242546840, 0.8420093967692193759 ) ) ;
#146521 = CARTESIAN_POINT ( 'NONE',  ( -1.001543065824772872E-14, 5.712500000000021672, 1.732050807568877637 ) ) ;
#146522 = CARTESIAN_POINT ( 'NONE',  ( 1.177287030172860183, -0.05180490295666683592, -2.161124318685260004 ) ) ;
#146523 = CARTESIAN_POINT ( 'NONE',  ( -5.917914848013369422, 7.154962168230770025, -1.123475595150375650 ) ) ;
#146525 = ADVANCED_FACE ( 'NONE', ( #140533 ), #72165, .F. ) ;
#146524 = CARTESIAN_POINT ( 'NONE',  ( 2.139325021376851765, 0.002241307429765720949, 2.019862492052142855 ) ) ;
#146526 = CARTESIAN_POINT ( 'NONE',  ( 3.836594282542955092, 7.419851063034579752, 0.7216878364870705775 ) ) ;
#146527 = VERTEX_POINT ( 'NONE', #99254 ) ;
#146528 = EDGE_CURVE ( 'NONE', #93013, #147554, #26088, .T. ) ;
#146530 = CARTESIAN_POINT ( 'NONE',  ( 6.629573927402440781, 10.67832731537079383, 1.040834085586084257E-14 ) ) ;
#146529 = CARTESIAN_POINT ( 'NONE',  ( -1.737499999999997824, -3.441666666666665986, 3.009438278150925683 ) ) ;
#146531 = CARTESIAN_POINT ( 'NONE',  ( -0.08058606167704472634, -5.741816521215563185, 10.99970480906934078 ) ) ;
#146532 = CARTESIAN_POINT ( 'NONE',  ( -6.071018923869249129, 10.30488218781460574, 0.7998128361456291469 ) ) ;
#146533 = CARTESIAN_POINT ( 'NONE',  ( 0.5324358445358172709, 0.5899921999869184308, 1.928256190492839028 ) ) ;
#146534 = CARTESIAN_POINT ( 'NONE',  ( 5.372676843235411503, -0.05303982195071360595, -2.191091664329389399 ) ) ;
#146535 = CARTESIAN_POINT ( 'NONE',  ( -1.500000000000011324, 4.952083334016150751, 0.8660254037844403729 ) ) ;
#146536 = CARTESIAN_POINT ( 'NONE',  ( 5.203337695038355193, 1.683698669361912259, -0.9069238330124268499 ) ) ;
#146537 = CARTESIAN_POINT ( 'NONE',  ( -3.093231602212184850, 6.760520635889515795, -0.7998128361456281477 ) ) ;
#146538 = CARTESIAN_POINT ( 'NONE',  ( 5.124618875841165710, 8.922546421882614709, 1.040834085586084257E-14 ) ) ;
#146540 = CARTESIAN_POINT ( 'NONE',  ( 2.689077551358230789, 1.704951624378052033, 1.076298511635757738 ) ) ;
#146539 = CARTESIAN_POINT ( 'NONE',  ( -9.775065565328612038, 10.50659070241261794, -0.7216878364870267237 ) ) ;
#146541 = B_SPLINE_CURVE_WITH_KNOTS ( 'NONE', 3,
 ( #112545, #179621, #29104, #160167 ),
 .UNSPECIFIED., .F., .F.,
 ( 4, 4 ),
 ( 9.058118219994478620E-18, 0.0001726908832626409531 ),
 .UNSPECIFIED. ) ;
#146542 = CARTESIAN_POINT ( 'NONE',  ( -0.6823417656250003738, 12.96354166700806942, 1.181850606188754593 ) ) ;
#146544 = CARTESIAN_POINT ( 'NONE',  ( -5.015590482412729756, 4.816220082428420923, 0.000000000000000000 ) ) ;
#146543 = CARTESIAN_POINT ( 'NONE',  ( 0.5918695612782381987, -0.8180161699140885423, 2.141640516796620375 ) ) ;
#146545 = CARTESIAN_POINT ( 'NONE',  ( 5.315364200056264643, -0.2495996188201006494, 1.706489999720143480 ) ) ;
#146546 = DIRECTION ( 'NONE',  ( 6.314299915563594049E-62, 8.546850786086437571E-32, 1.000000000000000000 ) ) ;
#146547 = CARTESIAN_POINT ( 'NONE',  ( 3.174580523894166006, 6.855427711185178019, 0.7998128361456341429 ) ) ;
#146548 = FACE_OUTER_BOUND ( 'NONE', #74362, .T. ) ;
#146549 = DIRECTION ( 'NONE',  ( 0.000000000000000000, 0.000000000000000000, 1.000000000000000000 ) ) ;
#146550 = LINE ( 'NONE', #197387, #6285 ) ;
#146551 = ORIENTED_EDGE ( 'NONE', *, *, #83136, .T. ) ;
#146552 = CARTESIAN_POINT ( 'NONE',  ( 5.619718922174004483, -0.4339147374951453084, 1.758609293272636487 ) ) ;
#146553 = CARTESIAN_POINT ( 'NONE',  ( 4.529305835417093640, 7.441884687032027657, -1.199719254218450271 ) ) ;
#146554 = CARTESIAN_POINT ( 'NONE',  ( -9.579665964948885559, 7.849261790823902629, -0.07999999999998980149 ) ) ;
#146555 = CARTESIAN_POINT ( 'NONE',  ( 5.637325938770506362, -0.03788160184842354061, 1.811251791611239170 ) ) ;
#146556 = CARTESIAN_POINT ( 'NONE',  ( 6.333067150914808430, 8.481940657524365434, 1.443375672974063439 ) ) ;
#146557 = CARTESIAN_POINT ( 'NONE',  ( -11.87828357749949149, 9.796897472595777145, -1.708055325888893972 ) ) ;
#146558 = CARTESIAN_POINT ( 'NONE',  ( 3.380998015235132215, 1.981133383611884735, -0.9370748116589098231 ) ) ;
#146559 = ORIENTED_EDGE ( 'NONE', *, *, #48267, .F. ) ;
#146561 = CARTESIAN_POINT ( 'NONE',  ( 8.215351014876830504, 11.67199438640995801, -1.199719254218446718 ) ) ;
#146560 = CARTESIAN_POINT ( 'NONE',  ( 0.9769180011504545735, 1.811320799089161993, 0.7541596914439269161 ) ) ;
#146562 = AXIS2_PLACEMENT_3D ( 'NONE', #12179, #211440, #96673 ) ;
#146563 = CARTESIAN_POINT ( 'NONE',  ( 4.112823271221511590, 0.09766498815510017695, 1.913256991299339793 ) ) ;
#146564 = PRESENTATION_LAYER_ASSIGNMENT (  '', '', ( #91194 ) ) ;
#146565 = DIRECTION ( 'NONE',  ( 0.000000000000000000, 0.000000000000000000, 1.000000000000000000 ) ) ;
#146566 = CARTESIAN_POINT ( 'NONE',  ( -1.364683531250014514, -0.5114583329919092369, -0.7879004041258359514 ) ) ;
#146567 = CIRCLE ( 'NONE', #208814, 10.99999999999719513 ) ;
#146568 = CARTESIAN_POINT ( 'NONE',  ( 5.558479791922850133, 6.547609847740540445, -1.082531754730542195 ) ) ;
#146569 = CARTESIAN_POINT ( 'NONE',  ( -7.700668062882065179, 10.96756792579566664, -1.082531754730543971 ) ) ;
#146570 = CARTESIAN_POINT ( 'NONE',  ( 1.710078970767275885, -2.145365142986368934, 0.2646356489638818088 ) ) ;
#146571 = CARTESIAN_POINT ( 'NONE',  ( -4.599959256786493533, 8.588645909551377855, 0.000000000000000000 ) ) ;
#146572 = CARTESIAN_POINT ( 'NONE',  ( 3.705121118284530279, 7.544668081299086282, -1.734723475976807094E-15 ) ) ;
#146573 = CARTESIAN_POINT ( 'NONE',  ( 1.887459117809231701, 1.256508940344562397, 1.324596713471258402 ) ) ;
#146574 = CARTESIAN_POINT ( 'NONE',  ( -4.627410500965859264, 4.293067094081919777, 0.7998128361456341429 ) ) ;
#146575 = CARTESIAN_POINT ( 'NONE',  ( 3.733261478165556646, -1.687024869733319221, 0.6981082995600741414 ) ) ;
#146576 = AXIS2_PLACEMENT_3D ( 'NONE', #146554, #213618, #129302 ) ;
#146577 = CARTESIAN_POINT ( 'NONE',  ( 9.635860615942547724, 11.95819851461962813, 8.658877209414601595 ) ) ;
#146578 = CARTESIAN_POINT ( 'NONE',  ( 2.496234081663367022, -0.9796988711565941532, 1.642222327643327873 ) ) ;
#146579 = EDGE_LOOP ( 'NONE', ( #140965, #184116, #566, #126676, #23771 ) ) ;
#146580 = CARTESIAN_POINT ( 'NONE',  ( 3.297268302959563524, -1.738273807845453600, 0.9259864402798111405 ) ) ;
#146581 = ORIENTED_EDGE ( 'NONE', *, *, #102005, .T. ) ;
#146582 = CARTESIAN_POINT ( 'NONE',  ( 4.599131018191075171, -0.5143685224620330176, 1.872658368587260647 ) ) ;
#146583 = VERTEX_POINT ( 'NONE', #100303 ) ;
#146584 = CARTESIAN_POINT ( 'NONE',  ( -6.774234028683526532, 7.932303117332766718, 1.199719254218452047 ) ) ;
#146586 = CARTESIAN_POINT ( 'NONE',  ( 5.765915565743810589, 0.6138260544302427402, -2.029845472315944921 ) ) ;
#146585 = CARTESIAN_POINT ( 'NONE',  ( 4.993145711582793744, 9.047363440147082159, -0.7998128361456481317 ) ) ;
#146587 = CARTESIAN_POINT ( 'NONE',  ( 0.000000000000000000, -4.517653975874099892, 0.000000000000000000 ) ) ;
#146588 = CARTESIAN_POINT ( 'NONE',  ( 5.531458889030211878, 6.400359360821498811, -1.228567739025695493 ) ) ;
#146589 = CARTESIAN_POINT ( 'NONE',  ( -9.484513307599961252, -6.630981389236807466, 0.1588444833727626904 ) ) ;
#146590 = CARTESIAN_POINT ( 'NONE',  ( 5.174371902270911150, 6.065797303184739420, 1.199719254218452047 ) ) ;
#146591 = CARTESIAN_POINT ( 'NONE',  ( 4.424480750451430744, -0.8629065238535367222, -1.818916818396177026 ) ) ;
#146592 = CARTESIAN_POINT ( 'NONE',  ( -0.1435606456237618622, 2.537783136032443654, 1.995875440081346097 ) ) ;
#146593 = CARTESIAN_POINT ( 'NONE',  ( 5.057177669875371429, -1.544152220135000420, -0.9737345633797565014 ) ) ;
#146594 = CARTESIAN_POINT ( 'NONE',  ( 1.223191768902037957, -1.870915810643185795, -0.8869332102946840823 ) ) ;
#146595 = CARTESIAN_POINT ( 'NONE',  ( -8.080296364064746939, 9.489729181906076505, 1.082531754730558626 ) ) ;
#146596 = CARTESIAN_POINT ( 'NONE',  ( -6.584207447892295839, 6.778236197985048506, 0.3223495580488393575 ) ) ;
#146597 = CARTESIAN_POINT ( 'NONE',  ( 1.177073619093308432, 2.881928502340592058, -0.7749999999999910294 ) ) ;
#146598 = CARTESIAN_POINT ( 'NONE',  ( 5.348468966913380029, 0.5439794105128460400, 1.789823788735760646 ) ) ;
#146599 = CARTESIAN_POINT ( 'NONE',  ( 7.311924916471702396, 7.425000578838787391, -0.7998128361456281477 ) ) ;
#146600 = CARTESIAN_POINT ( 'NONE',  ( 2.891631901464575272, 6.595597328342462262, 0.000000000000000000 ) ) ;
#146601 = CARTESIAN_POINT ( 'NONE',  ( -0.6823417656250003738, 10.46354166700806587, 1.181850606188754593 ) ) ;
#146602 = CARTESIAN_POINT ( 'NONE',  ( -6.735703387890906946, 6.752742128827836865, -0.7998128361456291469 ) ) ;
#146604 = CARTESIAN_POINT ( 'NONE',  ( -6.933015448541747006, 9.181880338089085214, 1.599625672291269396 ) ) ;
#146603 = CARTESIAN_POINT ( 'NONE',  ( -11.89942855770813956, 11.29999999999999893, -0.7000000000000009548 ) ) ;
#146605 = CARTESIAN_POINT ( 'NONE',  ( -5.555090253297260361, 7.504024600312024340, 1.599625672291269396 ) ) ;
#146606 = CARTESIAN_POINT ( 'NONE',  ( 1.727480438796034745, 0.1563249218069600044, -2.064440809470533544 ) ) ;
#146607 =( BOUNDED_SURFACE ( )  B_SPLINE_SURFACE ( 3, 3, ( 
 ( #136447, #188364, #40004, #20528, #106113, #54118, #155883, #3194, #186229, #169983 ),
 ( #152677, #119172, #4260, #102866, #25858, #9615, #76741, #45338, #42148, #8549 ),
 ( #110394, #111457, #109334, #75692, #140735, #127737, #142862, #207807, #94101, #141803 ),
 ( #43217, #59436, #58376, #158027, #159074, #30139, #125593, #178528, #176399, #175344 ),
 ( #206747, #191553, #126654, #124532, #128783, #26924, #28004, #93033, #174284, #193694 ),
 ( #160140, #12797, #10670, #208865, #143936, #108262, #209931, #91970, #60495, #192620 ),
 ( #44273, #177461, #78870, #11739, #77814, #61569, #29076, #95160, #161210, #144992 ) ),
 .UNSPECIFIED., .T., .F., .T. ) 
 B_SPLINE_SURFACE_WITH_KNOTS ( ( 4, 3, 4 ),
 ( 4, 1, 1, 1, 1, 1, 1, 4 ),
 ( 0.000000000000000000, 0.5000000000000000000, 1.000000000000000000 ),
 ( 0.000000000000000000, 0.09599525230796020214, 0.1893027314675523320, 0.2592390727089966540, 0.3619855251144610819, 0.5211967264240887632, 0.7336899926499302893, 1.000000000000000000 ),
 .UNSPECIFIED. ) 
 GEOMETRIC_REPRESENTATION_ITEM ( )  RATIONAL_B_SPLINE_SURFACE ( (
 ( 1.000000000000000222, 1.000000000000000222, 0.9999999999999997780, 1.000000000000000444, 1.000000000000000222, 1.000000000000000222, 1.000000000000000222, 1.000000000000000222, 1.000000000000000222, 1.000000000000000222),
 ( 0.3333333333333334259, 0.3333333333333334259, 0.3333333333333333148, 0.3333333333333335369, 0.3333333333333334259, 0.3333333333333333703, 0.3333333333333334259, 0.3333333333333333703, 0.3333333333333334259, 0.3333333333333334259),
 ( 0.3333333333333334259, 0.3333333333333334259, 0.3333333333333333148, 0.3333333333333335369, 0.3333333333333334259, 0.3333333333333333703, 0.3333333333333334259, 0.3333333333333333703, 0.3333333333333334259, 0.3333333333333334259),
 ( 1.000000000000000222, 1.000000000000000222, 0.9999999999999997780, 1.000000000000000444, 1.000000000000000222, 1.000000000000000222, 1.000000000000000222, 1.000000000000000222, 1.000000000000000222, 1.000000000000000222),
 ( 0.3333333333333334259, 0.3333333333333334259, 0.3333333333333333148, 0.3333333333333335369, 0.3333333333333334259, 0.3333333333333333703, 0.3333333333333334259, 0.3333333333333333703, 0.3333333333333334259, 0.3333333333333334259),
 ( 0.3333333333333334259, 0.3333333333333334259, 0.3333333333333333148, 0.3333333333333335369, 0.3333333333333334259, 0.3333333333333333703, 0.3333333333333334259, 0.3333333333333333703, 0.3333333333333334259, 0.3333333333333334259),
 ( 1.000000000000000222, 1.000000000000000222, 0.9999999999999997780, 1.000000000000000444, 1.000000000000000222, 1.000000000000000222, 1.000000000000000222, 1.000000000000000222, 1.000000000000000222, 1.000000000000000222) ) ) 
 REPRESENTATION_ITEM ( '' )  SURFACE ( )  );
#146608 = CARTESIAN_POINT ( 'NONE',  ( 2.091562808734966250, -0.4604446976123123814, 2.066416142659666111 ) ) ;
#146609 = CARTESIAN_POINT ( 'NONE',  ( 8.055515824813896941, 12.54985222892493368, 0.7998128361456462443 ) ) ;
#146610 = DIRECTION ( 'NONE',  ( 0.000000000000000000, -1.000000000000000000, 0.000000000000000000 ) ) ;
#146611 = CARTESIAN_POINT ( 'NONE',  ( 0.7956772557287052905, -1.388798143503049420, -1.396678344884971112 ) ) ;
#146612 = CARTESIAN_POINT ( 'NONE',  ( 4.526804827544169463, 7.221866427374837194, 1.292974732014543271 ) ) ;
#146613 = CARTESIAN_POINT ( 'NONE',  ( 4.365362273920244007, 6.116008624372160973, 1.443375672974062551 ) ) ;
#146615 = DIRECTION ( 'NONE',  ( -5.578564026256490882E-16, -1.000000000000000000, -9.066213480720158442E-32 ) ) ;
#146614 = DIRECTION ( 'NONE',  ( 1.276756478318932585E-15, -1.000000000000000000, 1.665334536937738262E-16 ) ) ;
#146616 = B_SPLINE_CURVE_WITH_KNOTS ( 'NONE', 3,
 ( #121583, #136695, #17566, #149739, #135627, #119429, #1316, #67378, #133519, #86865, #199525, #51169, #202721, #152929, #186487, #168118 ),
 .UNSPECIFIED., .F., .F.,
 ( 4, 3, 3, 3, 3, 4 ),
 ( 0.000000000000000000, 4.416163517950592750E-06, 1.117787330550273205E-05, 1.792356377820730995E-05, 2.465171878522349184E-05, 3.136847552909858286E-05 ),
 .UNSPECIFIED. ) ;
#146617 = CARTESIAN_POINT ( 'NONE',  ( 3.117397163603967680, -2.209095822378583929, 0.6116082133489489925 ) ) ;
#146618 = CARTESIAN_POINT ( 'NONE',  ( 0.9964003531478006215, -0.4411313887022934033, -1.771462291394958255 ) ) ;
#146619 = CARTESIAN_POINT ( 'NONE',  ( 2.636851627972558454, 1.802111047976437508, 0.6404684511054498097 ) ) ;
#146620 = ORIENTED_EDGE ( 'NONE', *, *, #134985, .F. ) ;
#146621 = CARTESIAN_POINT ( 'NONE',  ( 7.171900071504736296, 9.390302721554109056, -1.443375672974058777 ) ) ;
#146622 = CARTESIAN_POINT ( 'NONE',  ( 1.230727935554910557, 1.348888731755660153, -1.494678444409401896 ) ) ;
#146623 = CARTESIAN_POINT ( 'NONE',  ( 1.112071775475082402, 1.959765382314464732, -0.09068415226199526280 ) ) ;
#146624 = CARTESIAN_POINT ( 'NONE',  ( -7.947050595904583403, 12.42330946186405249, 0.7998128361456481317 ) ) ;
#146625 = CARTESIAN_POINT ( 'NONE',  ( -6.204827856548512877, 10.39071626594860476, -0.7998128361456291469 ) ) ;
#146626 = DIRECTION ( 'NONE',  ( 0.000000000000000000, 1.000000000000000000, 0.000000000000000000 ) ) ;
#146628 = CARTESIAN_POINT ( 'NONE',  ( 2.131405713275540847, -1.153620894759581184, -1.342296593837268848 ) ) ;
#146627 = CARTESIAN_POINT ( 'NONE',  ( 3.750014218873336969, 0.7526759941024010470, 1.950626372838085265 ) ) ;
#146629 = CARTESIAN_POINT ( 'NONE',  ( -8.752560967064900055, 13.99999998466135231, 9.356054886190362296 ) ) ;
#146631 = CARTESIAN_POINT ( 'NONE',  ( 5.384854118993849248, 2.023671607873143152, -1.076698936902406922 ) ) ;
#146630 = CARTESIAN_POINT ( 'NONE',  ( 1.534012367094065077, 8.737164261768352702, -2.508166476568407965 ) ) ;
#146632 = CARTESIAN_POINT ( 'NONE',  ( 4.312277775531628166, 1.592579213294993634, 0.7021690120074929320 ) ) ;
#146633 = ADVANCED_FACE ( 'NONE', ( #166369 ), #52618, .T. ) ;
#146634 = CARTESIAN_POINT ( 'NONE',  ( 7.889955328148847258, 11.29236608522730911, -1.199719254218446718 ) ) ;
#146635 = CARTESIAN_POINT ( 'NONE',  ( -0.1104750535120251204, 2.866086309876151539, -2.591737134608104842 ) ) ;
#146636 = CARTESIAN_POINT ( 'NONE',  ( 4.868316058674494684, -0.4618845756635507893, 1.671066720262862182 ) ) ;
#146637 = CIRCLE ( 'NONE', #91290, 2.250000000000000444 ) ;
#146638 = CARTESIAN_POINT ( 'NONE',  ( 4.809118753965334392, -1.746635306876740401, 1.289517135737711540 ) ) ;
#146639 = CARTESIAN_POINT ( 'NONE',  ( 2.984766373302843778, 6.633977868828633717, -0.7998128361456291469 ) ) ;
#146640 = CARTESIAN_POINT ( 'NONE',  ( 5.384000029850495750, -2.016708404008683786, 0.004832792792668073358 ) ) ;
#146641 = CARTESIAN_POINT ( 'NONE',  ( 1.468750000000000888, 0.7852924748299092705, -1.895863743164120097 ) ) ;
#146642 = CARTESIAN_POINT ( 'NONE',  ( -0.7499999999999972244, 4.889583334016150751, -1.299038105676652899 ) ) ;
#146643 = CARTESIAN_POINT ( 'NONE',  ( 3.698194863803183630, -1.924136204678703832, -0.09579085892482024078 ) ) ;
#146644 = CARTESIAN_POINT ( 'NONE',  ( -1.500000000000015099, 9.510416667349463893, -0.8660254037844309360 ) ) ;
#146645 = CARTESIAN_POINT ( 'NONE',  ( 0.3643397115577310941, 0.6907578271265965020, -2.111251545739430302 ) ) ;
#146646 = ORIENTED_EDGE ( 'NONE', *, *, #163416, .T. ) ;
#146647 = CARTESIAN_POINT ( 'NONE',  ( 6.983263157960366563, 2.446371134953594151, 2.328889586965996905 ) ) ;
#146648 = CARTESIAN_POINT ( 'NONE',  ( -0.7499999999999972244, 3.608333333333359150, -1.299038105676652011 ) ) ;
#146649 = CARTESIAN_POINT ( 'NONE',  ( 6.959412922516382771, 7.013736585890911535, 0.7998128361456341429 ) ) ;
#146650 = ADVANCED_FACE ( 'NONE', ( #67762, #133913 ), #81382, .T. ) ;
#146651 = CARTESIAN_POINT ( 'NONE',  ( 1.717743135698499124, 1.849103211704594463, 1.230578002476825583 ) ) ;
#146652 = DIRECTION ( 'NONE',  ( 1.000000000000000000, 0.000000000000000000, 0.000000000000000000 ) ) ;
#146653 = CARTESIAN_POINT ( 'NONE',  ( 6.290620087060792009, 10.28288116830553101, -0.7216878364870267237 ) ) ;
#146654 = EDGE_CURVE ( 'NONE', #22347, #7256, #132304, .T. ) ;
#146655 = CARTESIAN_POINT ( 'NONE',  ( 0.2607081404540609326, 7.167562920730477849, 2.095805658632963642 ) ) ;
#146656 = CARTESIAN_POINT ( 'NONE',  ( 4.686278372178935392, 5.496354851410763409, 1.199719254218452047 ) ) ;
#146657 = CARTESIAN_POINT ( 'NONE',  ( -0.01695367945527340853, -2.016028864686558730, -0.04667425414178058563 ) ) ;
#146659 = CARTESIAN_POINT ( 'NONE',  ( 5.441865409415975741, 1.382631645094612338, 1.530856317113358678 ) ) ;
#146658 = CARTESIAN_POINT ( 'NONE',  ( -0.4408745273427117084, 3.070687961115757592, -0.4190752896376583325 ) ) ;
#146660 = DIRECTION ( 'NONE',  ( -0.000000000000000000, 1.000000000000000000, -0.000000000000000000 ) ) ;
#146661 = CARTESIAN_POINT ( 'NONE',  ( -4.928552533767591726, 5.708731696605642725, 1.199719254218462483 ) ) ;
#146662 = CARTESIAN_POINT ( 'NONE',  ( 1.499999999999990896, 4.806250000682819490, 1.214306433183764966E-14 ) ) ;
#146663 = CARTESIAN_POINT ( 'NONE',  ( -1.364683531250000748, 0.2593750003414205252, 0.000000000000000000 ) ) ;
#146664 = CARTESIAN_POINT ( 'NONE',  ( 0.6492013947936903229, 0.5632195774387914744, -1.677790250104938874 ) ) ;
#146665 = CARTESIAN_POINT ( 'NONE',  ( 5.379468213355050210, -0.4295577260071090087, -1.679954900457746980 ) ) ;
#146666 = CARTESIAN_POINT ( 'NONE',  ( 4.880260771415650289, -0.2196809260722985546, -1.726461634439285797 ) ) ;
#146667 = CARTESIAN_POINT ( 'NONE',  ( 4.304877467538922531, 4.981110786005563007, 1.199719254218464037 ) ) ;
#146668 = CARTESIAN_POINT ( 'NONE',  ( 2.982263410219893274, -2.258884913406122408, -0.3895283529634691599 ) ) ;
#146669 = CARTESIAN_POINT ( 'NONE',  ( -1.364683531249997417, 5.071875000341417916, 1.214306433183764966E-14 ) ) ;
#146670 = CARTESIAN_POINT ( 'NONE',  ( 1.429379046243149931, 0.9088080074306194023, -1.601118750654044964 ) ) ;
#146671 = CARTESIAN_POINT ( 'NONE',  ( 4.425744359874354217, 7.314857078510163646, 1.252187566917076778 ) ) ;
#146672 = FILL_AREA_STYLE_COLOUR ( '', #200715 ) ;
#146673 = CARTESIAN_POINT ( 'NONE',  ( 1.992912282819898850, 1.589903476415389871, -0.8970392876451321884 ) ) ;
#146674 = CARTESIAN_POINT ( 'NONE',  ( 2.918592439375994552, -1.356299846568160827, -1.492255409411530120 ) ) ;
#146675 = CARTESIAN_POINT ( 'NONE',  ( 1.254151665356119549, 0.8908215700371600043, 2.002402562943622844 ) ) ;
#146676 = CARTESIAN_POINT ( 'NONE',  ( 8.790672116344218523, 15.72076966503868789, -9.208843758835506321 ) ) ;
#146677 = CARTESIAN_POINT ( 'NONE',  ( 3.926872384942071914, 1.999011803875171189, 0.6627620907858290389 ) ) ;
#146678 = CARTESIAN_POINT ( 'NONE',  ( -6.191269702934848240, 10.37489842006599616, 0.000000000000000000 ) ) ;
#146679 = CARTESIAN_POINT ( 'NONE',  ( 8.779893817263781486, 13.51977368570809013, 7.713389242581872196 ) ) ;
#146680 = CARTESIAN_POINT ( 'NONE',  ( 1.258353326579707776, -2.070544811992577561, -0.001879966208345739808 ) ) ;
#146681 = CARTESIAN_POINT ( 'NONE',  ( 4.761938266897790761, 6.578680616179308771, 1.599625672291267398 ) ) ;
#146682 = CARTESIAN_POINT ( 'NONE',  ( -1.360316468750042862, -0.8489583329918899413, -0.7853790794159322131 ) ) ;
#146683 = CARTESIAN_POINT ( 'NONE',  ( 3.897227946829431300, -0.2092540311423168320, -2.110150122182581356 ) ) ;
#146684 = CARTESIAN_POINT ( 'NONE',  ( 0.2582596107527914131, 0.7359740259155130859, 1.780569212123730871 ) ) ;
#146685 = ORIENTED_EDGE ( 'NONE', *, *, #209914, .F. ) ;
#146686 = CARTESIAN_POINT ( 'NONE',  ( -6.493429226302317225, 6.540365283632955773, 0.7998128361456341429 ) ) ;
#146687 = CARTESIAN_POINT ( 'NONE',  ( 9.911173986789782120, 11.52179005846497972, -1.199719254218440723 ) ) ;
#146688 = CARTESIAN_POINT ( 'NONE',  ( 5.356880090730850696, 9.263794182579101033, 0.7216878364870317197 ) ) ;
#146689 = CARTESIAN_POINT ( 'NONE',  ( 1.737499999999999378, -3.222916665710749751, -3.009438278150925683 ) ) ;
#146690 = CARTESIAN_POINT ( 'NONE',  ( -5.742041750587549842, 6.657802449562273850, 1.199719254218450271 ) ) ;
#146691 = CARTESIAN_POINT ( 'NONE',  ( 2.742449504557340489, 1.118516972803576870, -1.681586373676981827 ) ) ;
#146692 = CARTESIAN_POINT ( 'NONE',  ( 1.589043446250279601, -0.3083810453359912551, -2.083120927691509916 ) ) ;
#146693 = CARTESIAN_POINT ( 'NONE',  ( -4.782994330570982555, 8.802186828966616972, 0.000000000000000000 ) ) ;
#146694 = CARTESIAN_POINT ( 'NONE',  ( 10.05067194643221207, 10.62020544712608938, 0.7998128361456462443 ) ) ;
#146695 = CARTESIAN_POINT ( 'NONE',  ( 5.559367761144698328, 1.520187721101939671, 1.073055572604255214 ) ) ;
#146696 = CARTESIAN_POINT ( 'NONE',  ( 9.237182729612253951, 9.671134694169463586, 0.7998128361456462443 ) ) ;
#146697 = CARTESIAN_POINT ( 'NONE',  ( 0.4214947629262710826, 3.038568440852366770, 0.4183962726258849685 ) ) ;
#146698 = CARTESIAN_POINT ( 'NONE',  ( -3.962726036944197894, 7.845207153068690431, -0.7998128361456481317 ) ) ;
#146699 = CARTESIAN_POINT ( 'NONE',  ( -8.514157279702017078, 12.87700789305364069, -0.7216878364870267237 ) ) ;
#146700 =( BOUNDED_CURVE ( )  B_SPLINE_CURVE ( 3, ( #72746, #171317, #93304, #155081 ),
 .UNSPECIFIED., .F., .T. ) 
 B_SPLINE_CURVE_WITH_KNOTS ( ( 4, 4 ),
 ( 4.082329036708564729, 4.712388980384689674 ),
 .UNSPECIFIED. ) 
 CURVE ( )  GEOMETRIC_REPRESENTATION_ITEM ( )  RATIONAL_B_SPLINE_CURVE ( ( 1.000000000000000000, 0.9671913951452629776, 0.9671913951452629776, 1.000000000000000000 ) ) 
 REPRESENTATION_ITEM ( '' )  );
#146701 = CARTESIAN_POINT ( 'NONE',  ( -8.044065211609668253, 8.279164256499745633, 0.7998128361456602331 ) ) ;
#146702 = CARTESIAN_POINT ( 'NONE',  ( 6.789916310432966284, -0.8843476597930698402, 1.859958747594625317 ) ) ;
#146704 = CARTESIAN_POINT ( 'NONE',  ( -4.055257346293188014, 7.741894102302186553, 0.6119906029944787162 ) ) ;
#146703 = CARTESIAN_POINT ( 'NONE',  ( -4.827585214917754719, 7.789877296449459365, -1.199719254218453823 ) ) ;
#146705 = CARTESIAN_POINT ( 'NONE',  ( -1.364683531250000748, 0.2593750003414205252, 0.000000000000000000 ) ) ;
#146706 = CARTESIAN_POINT ( 'NONE',  ( 2.530263549637286502, 1.701127810229096982, -0.3340974653274173534 ) ) ;
#146707 = CARTESIAN_POINT ( 'NONE',  ( 1.534671620441448558, -1.258764033546970529, -1.202027791382529909 ) ) ;
#146709 = CARTESIAN_POINT ( 'NONE',  ( 6.968527767744098433, 9.153035033833367251, 1.443375672974076540 ) ) ;
#146708 = CARTESIAN_POINT ( 'NONE',  ( 6.481126831302748137, -0.1059855822947413234, -2.305399816445557359 ) ) ;
#146710 = CARTESIAN_POINT ( 'NONE',  ( -12.00295043402534212, 5.507662538472692049, -4.496421502479775789 ) ) ;
#146711 = CARTESIAN_POINT ( 'NONE',  ( 2.811851269462920744, -2.038842655386669644, 0.2989082417928933810 ) ) ;
#146712 = CARTESIAN_POINT ( 'NONE',  ( 1.388045824401448414, -0.05229234656609069859, 2.015604296821980057 ) ) ;
#146713 = CARTESIAN_POINT ( 'NONE',  ( 6.825078400183577365, 2.023440267519378999, 2.448151054272352578 ) ) ;
#146715 = COLOUR_RGB ( '', 0.40784314, 0.44705882, 0.49803922) ;
#146714 = CARTESIAN_POINT ( 'NONE',  ( -5.581116510680924847, 6.540332679663050541, -1.199719254218453823 ) ) ;
#146716 = CARTESIAN_POINT ( 'NONE',  ( 0.7429697149608678330, -1.692012040804885098, 1.011587418319284781 ) ) ;
#146717 = CIRCLE ( 'NONE', #22166, 2.750000000000000444 ) ;
#146719 = CARTESIAN_POINT ( 'NONE',  ( -5.885648082108231982, 7.959951743916638733, 1.443375672974058777 ) ) ;
#146718 = CARTESIAN_POINT ( 'NONE',  ( 5.009976098083095408, -0.6827417919906975108, 1.786564173047608062 ) ) ;
#146720 = CARTESIAN_POINT ( 'NONE',  ( -5.099275172071237705, 8.963255110809500437, 0.000000000000000000 ) ) ;
#146721 = CARTESIAN_POINT ( 'NONE',  ( 5.851225812749518695, 8.984124660586543243, -1.199719254218452047 ) ) ;
#146722 = CARTESIAN_POINT ( 'NONE',  ( -5.745623237141265882, 9.925253886631958622, 0.7998128361456291469 ) ) ;
#146723 = CARTESIAN_POINT ( 'NONE',  ( 0.8912779446055114629, -0.05177971647825175411, -2.019189627193836323 ) ) ;
#146724 = DIRECTION ( 'NONE',  ( -0.000000000000000000, 1.000000000000000000, -0.000000000000000000 ) ) ;
#146725 = CARTESIAN_POINT ( 'NONE',  ( 4.928937574911031128, 2.206605557787114869, 0.6751633795739877542 ) ) ;
#146727 = EDGE_CURVE ( 'NONE', #170765, #180412, #57187, .T. ) ;
#146726 = CARTESIAN_POINT ( 'NONE',  ( 6.092239754786219486, 0.9682357284593717806, -1.706234036142616928 ) ) ;
#146728 = CARTESIAN_POINT ( 'NONE',  ( 1.621847549879053885, 1.933622029546874010, -0.3300716771732490895 ) ) ;
#146729 = CARTESIAN_POINT ( 'NONE',  ( -4.963467767100621764, 4.685133904572482244, 0.2290337979854002448 ) ) ;
#146730 = CARTESIAN_POINT ( 'NONE',  ( -9.386185638472888115, 14.48154095986880918, 7.476657895028183454 ) ) ;
#146731 = EDGE_LOOP ( 'NONE', ( #185900, #208039, #175866, #89894, #184465, #100920, #77275, #48167, #75048, #6914, #177441, #144688 ) ) ;
#146732 = CARTESIAN_POINT ( 'NONE',  ( 1.042374724401398334, 0.8638241406289723923, 1.933313940807819487 ) ) ;
#146734 = CARTESIAN_POINT ( 'NONE',  ( -7.263417608619167076, 9.497073181520933716, -1.599625672291263179 ) ) ;
#146733 = CARTESIAN_POINT ( 'NONE',  ( -5.461236948206312114, 5.265864615862458464, 0.7998128361456341429 ) ) ;
#146735 = CARTESIAN_POINT ( 'NONE',  ( 1.095364067855080448, -1.841320589428995236, -0.001981933617903330457 ) ) ;
#146736 = EDGE_LOOP ( 'NONE', ( #83566, #47981, #153580, #55960, #35921 ) ) ;
#146737 = CARTESIAN_POINT ( 'NONE',  ( 4.065408448962204879, 1.859168595270783042, 1.121007083124803572 ) ) ;
#146738 = CARTESIAN_POINT ( 'NONE',  ( 11.51992191991745251, 8.397398980953870051, -3.382552691539911116 ) ) ;
#146739 = CARTESIAN_POINT ( 'NONE',  ( 1.933984528066152953, -2.055706711753771287, 0.5200354980386610038 ) ) ;
#146740 = CARTESIAN_POINT ( 'NONE',  ( -1.500000000000013101, 2.660416667349483788, -0.8660254037844313801 ) ) ;
#146741 = CARTESIAN_POINT ( 'NONE',  ( 7.079328764629950754, 11.41096732537697633, 0.7998128361456462443 ) ) ;
#146742 = CARTESIAN_POINT ( 'NONE',  ( 3.356764223755447141, -1.562743594079138321, 1.343508228479517230 ) ) ;
#146744 = CARTESIAN_POINT ( 'NONE',  ( 0.1164230846485321547, -0.09151219166612066525, 1.839079034809627755 ) ) ;
#146743 = CARTESIAN_POINT ( 'NONE',  ( -8.178592977541617515, 10.56477777859713463, 1.599625672291295375 ) ) ;
#146745 = CARTESIAN_POINT ( 'NONE',  ( -0.6823417656250003738, 2.967708333674754062, -1.181850606188749264 ) ) ;
#146746 = CARTESIAN_POINT ( 'NONE',  ( -10.87339879486171590, 5.131770238416462959, 5.487091846871368084 ) ) ;
#146747 = EDGE_CURVE ( 'NONE', #109653, #1642, #70433, .T. ) ;
#146748 = CARTESIAN_POINT ( 'NONE',  ( 1.317902950743182089, 4.161287538672367781, -0.3966175983076890010 ) ) ;
#146749 = CARTESIAN_POINT ( 'NONE',  ( 0.1357705729100426029, -2.015811560716780360, 0.8986578214904348272 ) ) ;
#146750 = CARTESIAN_POINT ( 'NONE',  ( 1.476233607035297490, 1.347422320225545089, 1.817282701917295240 ) ) ;
#146751 = CARTESIAN_POINT ( 'NONE',  ( -8.351459436338023679, 12.68719374246231624, -0.7216878364870267237 ) ) ;
#146752 = CARTESIAN_POINT ( 'NONE',  ( 2.548825626188336635, 0.2254045845835982720, 1.797452833117135329 ) ) ;
#146753 = CARTESIAN_POINT ( 'NONE',  ( 1.604551054648394537, 1.788909703809701712, 0.6859268596576766353 ) ) ;
#146754 = CARTESIAN_POINT ( 'NONE',  ( 2.928250347896840022, 1.105370970781336837, 1.750397071514836478 ) ) ;
#146755 = CARTESIAN_POINT ( 'NONE',  ( 1.364683531249986537, 0.9260416670080896528, 0.7879004041258500513 ) ) ;
#146756 = CARTESIAN_POINT ( 'NONE',  ( 1.200003858469798956, -1.971640592295399896, -0.002163809803111190443 ) ) ;
#146757 = CARTESIAN_POINT ( 'NONE',  ( 6.551400848983751857, -1.549099897634421685, -1.145107510758677893 ) ) ;
#146758 = CARTESIAN_POINT ( 'NONE',  ( 3.203821283898714345, -1.868584281295191607, 0.09040415888627445495 ) ) ;
#146760 = CARTESIAN_POINT ( 'NONE',  ( 5.819104682239041537, 7.212836251160942957, -1.171789181936284896 ) ) ;
#146759 = CARTESIAN_POINT ( 'NONE',  ( 1.717812883538033297, -0.2792282863031622653, 2.290681961221084695 ) ) ;
#146761 = CARTESIAN_POINT ( 'NONE',  ( 2.752234738034575301, -1.855867026150724186, -0.1399345609422244507 ) ) ;
#146762 = CARTESIAN_POINT ( 'NONE',  ( -1.364683531250012516, 2.780208333674754506, 0.7879004041258379498 ) ) ;
#146763 = CARTESIAN_POINT ( 'NONE',  ( 5.248506731170051509, -2.046683549694120252, -0.2560125357965719606 ) ) ;
#146764 = CARTESIAN_POINT ( 'NONE',  ( -4.564291269294938225, 8.476756914152748124, 1.040834085586084257E-14 ) ) ;
#146765 = CARTESIAN_POINT ( 'NONE',  ( 10.98546401119367566, 13.75740562920347188, 1.592223900679732518 ) ) ;
#146767 = CARTESIAN_POINT ( 'NONE',  ( 6.422895033429510292, 1.963595603779586973, 0.7616278367365038049 ) ) ;
#146766 = VECTOR ( 'NONE', #47578, 1000.000000000000000 ) ;
#146768 = CARTESIAN_POINT ( 'NONE',  ( 1.364683531249990311, 2.696875000341415696, 1.214306433183764966E-14 ) ) ;
#146769 = CARTESIAN_POINT ( 'NONE',  ( 6.186834690482100108, -0.3103498281695793448, -2.139073744226393181 ) ) ;
#146770 = CARTESIAN_POINT ( 'NONE',  ( 0.4152503475762688856, -0.9843521281015167324, -1.555853522519357934 ) ) ;
#146772 = ADVANCED_FACE ( 'NONE', ( #173319 ), #151275, .T. ) ;
#146771 = CARTESIAN_POINT ( 'NONE',  ( 5.707677564275420501, 1.530686452870811065, 1.317726828763097435 ) ) ;
#146773 = CARTESIAN_POINT ( 'NONE',  ( -15.75000000000000000, 13.39999999999998259, 1.399999999999998579 ) ) ;
#146774 = CARTESIAN_POINT ( 'NONE',  ( -5.477130870240893401, 6.452702772444876445, 1.082531754730548412 ) ) ;
#146775 = ADVANCED_FACE ( 'NONE', ( #157066 ), #122514, .F. ) ;
#146778 = CARTESIAN_POINT ( 'NONE',  ( 5.666945020832181434, 5.713783400500082266, 0.7216878364870317197 ) ) ;
#146777 = CARTESIAN_POINT ( 'NONE',  ( -1.642778471874998480, -1.801041666188708090, 2.845375778867863303 ) ) ;
#146776 = CARTESIAN_POINT ( 'NONE',  ( 7.038618024149998043, 8.240751112043669835, -1.199719254218452047 ) ) ;
#146779 = CARTESIAN_POINT ( 'NONE',  ( -4.281342646865346602, 8.216926531310035031, 0.7998128361456352531 ) ) ;
#146780 = CARTESIAN_POINT ( 'NONE',  ( 3.555875268649951959, 1.124244472066991518, 1.673854899288424347 ) ) ;
#146781 = CARTESIAN_POINT ( 'NONE',  ( -6.842061076390810292, 11.13415502243129218, 0.000000000000000000 ) ) ;
#146783 =( NAMED_UNIT ( * ) PLANE_ANGLE_UNIT ( ) SI_UNIT ( $, .RADIAN. ) );
#146782 = CARTESIAN_POINT ( 'NONE',  ( -4.464712657601869417, 4.103252943490596216, 0.7998128361456341429 ) ) ;
#146784 = CARTESIAN_POINT ( 'NONE',  ( 1.364683531249988535, 5.405208333674750953, -0.7879004041258300672 ) ) ;
#146786 = CARTESIAN_POINT ( 'NONE',  ( 0.6823417656249969321, 9.026041667008065872, -1.181850606188757036 ) ) ;
#146785 = CARTESIAN_POINT ( 'NONE',  ( 6.139563164240942506, -1.562336469324271837, -1.494251390645913613 ) ) ;
#146787 = CARTESIAN_POINT ( 'NONE',  ( 10.33323920393387674, 4.021557182957052667, -5.965898435992177617 ) ) ;
#146788 = CARTESIAN_POINT ( 'NONE',  ( -11.37863701345828993, 6.568914681733530436, 3.817141491415757759 ) ) ;
#146790 = CARTESIAN_POINT ( 'NONE',  ( 5.923453886551514280, -1.462456689723025782, -1.388475849216065372 ) ) ;
#146789 = CARTESIAN_POINT ( 'NONE',  ( -6.846504384776774366, 7.089935991768773427, -0.7216878364870267237 ) ) ;
#146791 = CARTESIAN_POINT ( 'NONE',  ( 1.364683531249986981, -1.053124999658580752, 0.000000000000000000 ) ) ;
#146792 = CARTESIAN_POINT ( 'NONE',  ( 1.681838029686154146, -0.9247999101687879309, 1.455793735983588633 ) ) ;
#146793 = CARTESIAN_POINT ( 'NONE',  ( 3.888156192069020634, 7.758209000714329839, 1.040834085586084257E-14 ) ) ;
#146795 = CARTESIAN_POINT ( 'NONE',  ( 5.830888582329017744, 8.960397891762626799, -1.199719254218452047 ) ) ;
#146794 = CARTESIAN_POINT ( 'NONE',  ( 5.965224400332808763, 9.903252867122883885, -0.7216878364870267237 ) ) ;
#146796 = CARTESIAN_POINT ( 'NONE',  ( -11.99998407866956107, 9.073076179820285248, -0.6191218322778160310 ) ) ;
#146797 = CARTESIAN_POINT ( 'NONE',  ( 0.2273421782777407807, -1.081390543313685226, -1.401283913643845969 ) ) ;
#146798 = CARTESIAN_POINT ( 'NONE',  ( 0.2936080233231981862, 1.877589464902774674, -0.7265071302150533095 ) ) ;
#146799 = CARTESIAN_POINT ( 'NONE',  ( -0.3788956605886382167, 3.049042541176487209, -0.4283520265746191269 ) ) ;
#146800 = CARTESIAN_POINT ( 'NONE',  ( 2.766872162265196611, -1.522532973755141850, 1.597636210702752635 ) ) ;
#146801 = CARTESIAN_POINT ( 'NONE',  ( 5.471592230178073279, -0.3258623020658823477, 2.146390899824067056 ) ) ;
#146802 = ORIENTED_EDGE ( 'NONE', *, *, #177186, .T. ) ;
#146803 = CARTESIAN_POINT ( 'NONE',  ( 3.074666975249065626, 6.809138247757705820, 0.000000000000000000 ) ) ;
#146805 = CARTESIAN_POINT ( 'NONE',  ( 1.564077599769473803, -1.076297475396456704, 1.704952281334138675 ) ) ;
#146804 = CARTESIAN_POINT ( 'NONE',  ( 2.965608807194367813, -1.734805745614193873, -1.219131234129526398 ) ) ;
#146807 = ORIENTED_EDGE ( 'NONE', *, *, #168859, .T. ) ;
#146806 = CARTESIAN_POINT ( 'NONE',  ( 2.074188967152798657, 0.7772732722058082189, 1.636524323399509928 ) ) ;
#146808 = CARTESIAN_POINT ( 'NONE',  ( 5.631432701629774051, 7.663367133358481631, 1.599625672291269396 ) ) ;
#146809 = CARTESIAN_POINT ( 'NONE',  ( 6.745345117998789775, 7.828323044875442172, 1.199719254218462483 ) ) ;
#146810 = CLOSED_SHELL ( 'NONE', ( #158998, #121837, #56893, #5413, #97096, #59390, #74522, #17633, #42237, #195134, #65822, #36430, #87466, #79941, #165584, #37195, #86509, #149431, #173956, #201706, #196298, #48143, #25207, #174913, #27242, #85507, #43465, #178025, #159434, #37096, #94400, #117578, #144182, #119978, #56751, #81437, #160339, #202122, #179324, #197936, #22111, #19570, #189681, #33195, #100399, #110329, #159239, #86557, #66162, #182098, #156957, #75064, #210702, #128008, #203108, #57138, #90115, #43581, #206144, #56506, #108668, #142814, #194303, #125431, #194681, #203429, #172604, #196809, #86101, #15528, #74846, #44250, #158480, #122337, #62018, #90432, #123144, #54222, #71794, #76442, #144934, #76659, #74075, #84066, #20749, #40352, #52077, #196198, #192908, #184803, #210893, #90686, #180697, #51670, #160866, #137121, #127673, #16500, #208816, #150135, #178601, #200866, #15402, #113616, #134474, #208955, #58775, #202344, #151998, #18732, #8764, #152763, #80978, #102849, #82199, #92642, #108806, #135685, #153018, #11779, #127235, #206650, #135663, #109787, #155903, #86819, #162261, #203635, #38249, #143567, #3210, #23203, #57915, #199601, #191707, #141003, #155116, #166198, #145198, #40762, #35450, #138164, #121014, #198057, #1659, #180030, #115127, #96258, #99603, #108118, #106561, #105238, #191153, #101058, #39511, #163169, #151627, #78029, #64949, #96395, #117192, #100389, #25256, #200993, #16231, #133529, #66977, #110808, #174907, #115639, #26585, #59158, #58379, #181907, #69647, #198572, #97080, #57415, #129065, #147458, #109652, #165521, #30087, #104698, #211495, #203821, #59775, #195939, #110287, #21707, #85334, #105000, #120104, #133198, #11, #167897, #1172, #176145, #50966, #199778, #1267, #8363, #96339, #60535, #115223, #134212, #88291, #201696, #30024, #49813, #134495, #192810, #62527, #27069, #48204, #77243, #97602, #39071, #97204, #92629, #4429, #105685, #5782, #195534, #93703, #172492, #80396, #28318, #178501, #76793, #8950, #80971, #91529, #200496, #52970, #192497, #110989 ) ) ;
#146812 = CARTESIAN_POINT ( 'NONE',  ( 0.9014164429375628451, -1.868237418080781254, 0.4230343950424199084 ) ) ;
#146811 = CARTESIAN_POINT ( 'NONE',  ( -4.334856428067329404, 6.080418470877079429, -1.599625672291256295 ) ) ;
#146813 = CARTESIAN_POINT ( 'NONE',  ( -2.642331537210447667, 0.3998488639457564719, -0.1525862845480549512 ) ) ;
#146814 = CARTESIAN_POINT ( 'NONE',  ( 9.612263720970512182, -6.681311647492914396, -0.1963700886235927867 ) ) ;
#146815 = CARTESIAN_POINT ( 'NONE',  ( 5.300874872818830852, 7.207439989753867238, 1.443375672974062551 ) ) ;
#146816 = CARTESIAN_POINT ( 'NONE',  ( -1.364683531250000748, -0.1781249996585798634, 0.000000000000000000 ) ) ;
#146817 = CARTESIAN_POINT ( 'NONE',  ( 4.858757509019037357, 5.629766575900002401, 2.420000000000000373 ) ) ;
#146818 = CARTESIAN_POINT ( 'NONE',  ( -10.30827686509187835, 10.92074451889568643, 1.040834085586084257E-14 ) ) ;
#146819 = CARTESIAN_POINT ( 'NONE',  ( 4.750933126423753095, -1.738186171353903742, 1.284983810367075208 ) ) ;
#146820 = CARTESIAN_POINT ( 'NONE',  ( -4.828112100242283766, 7.686528979374367410, -1.082531754730549967 ) ) ;
#146821 = CARTESIAN_POINT ( 'NONE',  ( 5.234856708652233515, 6.240325927249993576, 1.082531754730549078 ) ) ;
#146822 = CARTESIAN_POINT ( 'NONE',  ( 1.758217466200185042, 0.8068918862002281145, -1.961288232260410380 ) ) ;
#146823 = CARTESIAN_POINT ( 'NONE',  ( 10.91962425643199985, -9.919999999999998153, -0.09058751758333170867 ) ) ;
#146824 = CARTESIAN_POINT ( 'NONE',  ( 3.462146415373760444, 0.8834382129937996542, 1.762370924576799114 ) ) ;
#146825 = CARTESIAN_POINT ( 'NONE',  ( 6.011958326525193463, -0.6379227081053112647, 1.803018720113582773 ) ) ;
#146826 = ORIENTED_EDGE ( 'NONE', *, *, #90321, .F. ) ;
#146827 = CARTESIAN_POINT ( 'NONE',  ( -2.093037498677872144, 1.000000000000000888, 11.70868840297834446 ) ) ;
#146828 = CARTESIAN_POINT ( 'NONE',  ( 0.6607010325807397555, -0.6960017893198193750, -1.950014918625786020 ) ) ;
#146829 = CARTESIAN_POINT ( 'NONE',  ( 1.640467198872105348, -1.640604414344963180, 1.038759544029205895 ) ) ;
#146830 = ORIENTED_EDGE ( 'NONE', *, *, #151508, .F. ) ;
#146831 = CARTESIAN_POINT ( 'NONE',  ( -3.526002468005825286, 6.271364091718859335, -1.199719254218450271 ) ) ;
#146833 = CARTESIAN_POINT ( 'NONE',  ( 8.174640274396848483, 8.501778173076651512, 0.7998128361456291469 ) ) ;
#146832 = CARTESIAN_POINT ( 'NONE',  ( -5.966997003790221576, 9.015228033513643879, -1.082531754730549967 ) ) ;
#146835 = CARTESIAN_POINT ( 'NONE',  ( 6.632963465583686435, 8.761543347979550589, -1.599625672291262513 ) ) ;
#146834 = CARTESIAN_POINT ( 'NONE',  ( 3.011755509560889443, -1.030818127458534184, -1.818759449385324078 ) ) ;
#146836 = CARTESIAN_POINT ( 'NONE',  ( 4.217995187182920880, 6.974725914138481642, 1.082531754730549078 ) ) ;
#146838 = ORIENTED_EDGE ( 'NONE', *, *, #60529, .F. ) ;
#146837 = CARTESIAN_POINT ( 'NONE',  ( 6.498695769366850783, -1.876353784076413067, -0.3680397143606057853 ) ) ;
#146839 = CARTESIAN_POINT ( 'NONE',  ( 4.565167970240332274, -1.970479184476852108, -0.9938812724585781577 ) ) ;
#146840 = CARTESIAN_POINT ( 'NONE',  ( 2.608667852368121043, -0.8438080161984360394, -2.039271889284439254 ) ) ;
#146841 = CARTESIAN_POINT ( 'NONE',  ( 6.923409998072794558, 11.22906209772695618, 1.040834085586084257E-14 ) ) ;
#146842 = DIRECTION ( 'NONE',  ( -0.9885327375000381167, 0.000000000000000000, -0.1510067114093955609 ) ) ;
#146843 = CARTESIAN_POINT ( 'NONE',  ( 1.717294761138322912, 1.590556852780611097, 1.061263400373997134 ) ) ;
#146844 = CARTESIAN_POINT ( 'NONE',  ( -0.4356160240586524068, -9.063431457505059186, 9.626717610576628559 ) ) ;
#146845 = CARTESIAN_POINT ( 'NONE',  ( 11.48784849554592924, 13.83049527181923111, -3.469614872287849927 ) ) ;
#146846 = CARTESIAN_POINT ( 'NONE',  ( 4.105968538015460467, 0.7004154448949986289, -1.948405661837959713 ) ) ;
#146847 = ADVANCED_FACE ( 'NONE', ( #37969 ), #40107, .F. ) ;
#146849 = CARTESIAN_POINT ( 'NONE',  ( 1.288190726105652217, -0.9714702286227733241, 1.931199087792371261 ) ) ;
#146848 = CARTESIAN_POINT ( 'NONE',  ( -2.279742385392243165, 5.811449882932888222, -0.7998128361456281477 ) ) ;
#146850 = CARTESIAN_POINT ( 'NONE',  ( 4.036819321710017228, -1.906298169312226953, 1.081085072550565407 ) ) ;
#146851 = CARTESIAN_POINT ( 'NONE',  ( -5.829766698406889880, 6.654474238104274519, 0.9546379765748146395 ) ) ;
#146852 = LINE ( 'NONE', #77550, #148895 ) ;
#146853 = CARTESIAN_POINT ( 'NONE',  ( -0.4444767461201751813, 7.387363020590631990, 2.040826832792407508 ) ) ;
#146854 = CARTESIAN_POINT ( 'NONE',  ( 4.037295881819344956, 7.932205305423046582, -0.7998128361456362523 ) ) ;
#146855 = CARTESIAN_POINT ( 'NONE',  ( -0.6823417656250039265, 14.38020833367473195, -1.181850606188755259 ) ) ;
#146856 = CARTESIAN_POINT ( 'NONE',  ( -4.248501033035892327, 6.049946853332221153, -1.599625672291271394 ) ) ;
#146858 = CARTESIAN_POINT ( 'NONE',  ( -0.1399997263889594112, -0.002789056014654289761, -2.000146600338557956 ) ) ;
#146857 = TOROIDAL_SURFACE ( 'NONE', #98434, 3.970406073902761790, 0.08000000000000000167 ) ;
#146859 = CARTESIAN_POINT ( 'NONE',  ( -9.002250809793991948, 12.48608113052627289, -1.082531754730543971 ) ) ;
#146860 = CARTESIAN_POINT ( 'NONE',  ( 4.452052287080165982, -0.7971045336818067817, 1.910850710330507907 ) ) ;
#146861 = CARTESIAN_POINT ( 'NONE',  ( 2.736843622788497132, 0.2362483484473417716, 1.911901653511848931 ) ) ;
#146862 = CARTESIAN_POINT ( 'NONE',  ( 5.941034585168498694, -1.816085283887830082, -1.088097372982429034 ) ) ;
#146863 = CIRCLE ( 'NONE', #174545, 0.09999999999999982514 ) ;
#146864 = CARTESIAN_POINT ( 'NONE',  ( 5.311043488251262268, 7.219303374425030562, -1.599625672291256295 ) ) ;
#146865 = CARTESIAN_POINT ( 'NONE',  ( 9.534866695232230072, 3.538528462892242654, 7.286654780214751881 ) ) ;
#146866 = CARTESIAN_POINT ( 'NONE',  ( 4.030098220014290078, 1.090402053431119622, 1.639822181875214557 ) ) ;
#146867 = CARTESIAN_POINT ( 'NONE',  ( 6.175753646036172384, -1.231511006544892206, 1.933186584637256678 ) ) ;
#146868 = CARTESIAN_POINT ( 'NONE',  ( 4.037589748876240670, -1.260430739550026047, -1.321009972365666085 ) ) ;
#146869 = CARTESIAN_POINT ( 'NONE',  ( 6.861835142292143530, 8.138467433163244280, 1.082531754730549967 ) ) ;
#146870 = CARTESIAN_POINT ( 'NONE',  ( 3.823036128929238942, 7.404033217152015567, 1.040834085586084257E-14 ) ) ;
#146871 = CARTESIAN_POINT ( 'NONE',  ( -7.144220599758281054, 7.299621885998258897, 0.7998128361456341429 ) ) ;
#146872 = CARTESIAN_POINT ( 'NONE',  ( 4.854701522145073334, 7.821512988214679218, -1.199719254218450271 ) ) ;
#146873 =( BOUNDED_CURVE ( )  B_SPLINE_CURVE ( 2, ( #197211, #79206, #97613, #194013, #114965, #211324, #163670, #62949, #144265 ),
 .UNSPECIFIED., .F., .T. ) 
 B_SPLINE_CURVE_WITH_KNOTS ( ( 3, 2, 2, 2, 3 ),
 ( 0.6160714285714286031, 0.6190476190476190688, 0.6250000000000000000, 0.6309523809523809312, 0.6339285714285713969 ),
 .UNSPECIFIED. ) 
 CURVE ( )  GEOMETRIC_REPRESENTATION_ITEM ( )  RATIONAL_B_SPLINE_CURVE ( ( 0.9330127018922194093, 0.9330127018922194093, 1.000000000000000000, 0.8660254037844387076, 1.000000000000000000, 0.8660254037844387076, 1.000000000000000000, 0.9330127018922194093, 0.9330127018922194093 ) ) 
 REPRESENTATION_ITEM ( '' )  );
#146874 = ORIENTED_EDGE ( 'NONE', *, *, #140470, .F. ) ;
#146875 = CARTESIAN_POINT ( 'NONE',  ( 4.992444313356595664, -1.114831962662912845, 1.676160436541684229 ) ) ;
#146876 = AXIS2_PLACEMENT_3D ( 'NONE', #32889, #116329, #182319 ) ;
#146877 = CARTESIAN_POINT ( 'NONE',  ( 5.977181698541591537, -2.287177818765488091, -0.2295778655121790968 ) ) ;
#146878 = CARTESIAN_POINT ( 'NONE',  ( 4.733228419949464971, 0.004064956161661801778, -1.961936380062332397 ) ) ;
#146879 = CARTESIAN_POINT ( 'NONE',  ( -7.054319997812058318, 7.124461507069184130, 1.040834085586084257E-14 ) ) ;
#146880 = CARTESIAN_POINT ( 'NONE',  ( -5.447678794592645701, 5.250046769979851646, 0.000000000000000000 ) ) ;
#146881 = LINE ( 'NONE', #48307, #78170 ) ;
#146882 = CARTESIAN_POINT ( 'NONE',  ( -6.961185525973791144, 7.086080966583015339, 0.7998128361456341429 ) ) ;
#146884 = CARTESIAN_POINT ( 'NONE',  ( 0.5318453760667535279, 0.9654296485097979552, -1.602142582367314549 ) ) ;
#146883 = CARTESIAN_POINT ( 'NONE',  ( 1.101248736683122953, -0.5045743719560727980, 2.028828713580214771 ) ) ;
#146885 = CARTESIAN_POINT ( 'NONE',  ( 0.7499999999999902300, 2.983333333333351600, 1.299038105676669330 ) ) ;
#146886 = CARTESIAN_POINT ( 'NONE',  ( 6.597608361038971303, -1.941456323438792042, 0.05037571119943275166 ) ) ;
#146887 = CARTESIAN_POINT ( 'NONE',  ( -0.2102771530458276972, -0.008943344768331040057, -2.203482896658352175 ) ) ;
#146888 = CARTESIAN_POINT ( 'NONE',  ( 1.434671803396998291, -1.260233744827907953, -1.200652698350104686 ) ) ;
#146889 = CARTESIAN_POINT ( 'NONE',  ( 6.043183783389218355, 8.073467052085995022, 1.599625672291267398 ) ) ;
#146890 = DIRECTION ( 'NONE',  ( -1.000000000000000000, -1.224646799147346058E-16, 0.000000000000000000 ) ) ;
#146891 = CARTESIAN_POINT ( 'NONE',  ( 2.068594797844982125, -1.576417056545238893, -0.7005022305992656406 ) ) ;
#146892 = CARTESIAN_POINT ( 'NONE',  ( 1.136565065649897344, 0.4323997850379875385, 2.148315308122191514 ) ) ;
#146893 = CARTESIAN_POINT ( 'NONE',  ( 4.283934280384479543, 1.440456688004333019, 1.672026782002330458 ) ) ;
#146894 = CARTESIAN_POINT ( 'NONE',  ( 1.200314488179974326, 0.8819602860624680130, -1.984045050410755406 ) ) ;
#146895 = CARTESIAN_POINT ( 'NONE',  ( 5.339274934379788269E-16, 0.000000000000000000, -3.000000000000000444 ) ) ;
#146896 = CARTESIAN_POINT ( 'NONE',  ( 2.466138310383278132, -1.084178177903678320, 1.818555153620523779 ) ) ;
#146897 = DIRECTION ( 'NONE',  ( -0.000000000000000000, 1.000000000000000000, -0.000000000000000000 ) ) ;
#146898 = VERTEX_POINT ( 'NONE', #87784 ) ;
#146900 = CARTESIAN_POINT ( 'NONE',  ( 0.6823417656249882723, 0.4885416670080827695, -1.181850606188749264 ) ) ;
#146899 = CARTESIAN_POINT ( 'NONE',  ( 2.138584244316643179, 0.5063124247480701445, 2.235611027800854078 ) ) ;
#146901 = FACE_OUTER_BOUND ( 'NONE', #30544, .T. ) ;
#146902 = CARTESIAN_POINT ( 'NONE',  ( 5.705283713252285338, 5.550585841749444249, -0.7998128361456211532 ) ) ;
#146903 = ADVANCED_FACE ( 'NONE', ( #123579 ), #153858, .F. ) ;
#146904 = CARTESIAN_POINT ( 'NONE',  ( 4.951916289638909063, -1.570117426187572107, -1.571520405092931005 ) ) ;
#146905 = CARTESIAN_POINT ( 'NONE',  ( -6.805829924380121909, 8.963220883242035697, 1.443375672974078761 ) ) ;
#146906 = CARTESIAN_POINT ( 'NONE',  ( 3.375617060122621194, 6.882044303544283537, 1.040834085586084257E-14 ) ) ;
#146907 = CARTESIAN_POINT ( 'NONE',  ( -7.171900071504745178, 9.390302721554109056, -1.443375672974058777 ) ) ;
#146908 = CARTESIAN_POINT ( 'NONE',  ( 6.048345925472191631, 6.229027465905275562, 0.7216878364870328300 ) ) ;
#146909 = AXIS2_PLACEMENT_3D ( 'NONE', #81131, #18242, #1979 ) ;
#146910 = VERTEX_POINT ( 'NONE', #105121 ) ;
#146911 = CARTESIAN_POINT ( 'NONE',  ( 3.428361437285933455, -1.528740797599713153, -1.314997250469025936 ) ) ;
#146913 = CARTESIAN_POINT ( 'NONE',  ( 2.043871907009750633, 1.419221230981766668, 1.496905473486829230 ) ) ;
#146912 = CARTESIAN_POINT ( 'NONE',  ( 6.775324078527185989, 8.927630729746953264, -1.599625672291262513 ) ) ;
#146914 = CARTESIAN_POINT ( 'NONE',  ( -11.84104725192634966, 13.60983537451416048, 1.443823348526939165 ) ) ;
#146915 = CARTESIAN_POINT ( 'NONE',  ( 4.706088717274896638, 7.544168365912456764, 1.082531754730548412 ) ) ;
#146916 = DIRECTION ( 'NONE',  ( 0.000000000000000000, 1.000000000000000000, 0.000000000000000000 ) ) ;
#146917 = CARTESIAN_POINT ( 'NONE',  ( 1.364683531249988535, 3.655208333674750509, -0.7879004041258239610 ) ) ;
#146918 = CARTESIAN_POINT ( 'NONE',  ( 4.576244502665470115, -2.125281509430646754, -0.5339713055512520512 ) ) ;
#146919 = CARTESIAN_POINT ( 'NONE',  ( 2.549454116737331244, -1.388485404012842261, 1.462446031800922253 ) ) ;
#146920 = CARTESIAN_POINT ( 'NONE',  ( 0.5910386730991653570, -0.6632029860377097741, 1.717849102829023922 ) ) ;
#146921 = AXIS2_PLACEMENT_3D ( 'NONE', #109024, #92729, #90590 ) ;
#146922 = CARTESIAN_POINT ( 'NONE',  ( 6.109920781252839994, 10.27999134477033216, 1.040834085586084257E-14 ) ) ;
#146923 = ADVANCED_FACE ( 'NONE', ( #107296 ), #171161, .F. ) ;
#146924 = CARTESIAN_POINT ( 'NONE',  ( 5.297797529045338294, -0.6555159417414997414, 1.704002486358429325 ) ) ;
#146925 = CARTESIAN_POINT ( 'NONE',  ( 6.047500043413473136, -1.423963828944514010, 1.427935028000301809 ) ) ;
#146926 = CARTESIAN_POINT ( 'NONE',  ( -8.850775351622791831, 9.220326086515070685, -0.7998128361456291469 ) ) ;
#146928 = CARTESIAN_POINT ( 'NONE',  ( -6.629010762438975135, 6.698543742459062145, -0.7998128361456362523 ) ) ;
#146927 = CARTESIAN_POINT ( 'NONE',  ( 4.750980993940300046, -1.819980134924009452, 1.343945550547174239 ) ) ;
#146929 = CARTESIAN_POINT ( 'NONE',  ( 0.9089716955857042313, 1.593442362523834754, -1.377222155420864347 ) ) ;
#146930 = CARTESIAN_POINT ( 'NONE',  ( -7.584860592202423035, 7.813701877183096833, -0.7998128361456362523 ) ) ;
#146931 = CARTESIAN_POINT ( 'NONE',  ( 4.211429588753928144, -1.719575573843846072, -1.152724658989822348 ) ) ;
#146932 = CARTESIAN_POINT ( 'NONE',  ( 8.028399517586572998, 12.51821653715971472, -0.7998128361456352531 ) ) ;
#146933 = CARTESIAN_POINT ( 'NONE',  ( -4.356712336337761644E-14, 2.859375000341351392, -1.570758158831810247 ) ) ;
#146934 = DIRECTION ( 'NONE',  ( -0.9120491373041521577, 0.000000000000000000, -0.4100809324301146752 ) ) ;
#146935 = CARTESIAN_POINT ( 'NONE',  ( -9.176171038350775078, 9.599954387697719582, -0.7998128361456291469 ) ) ;
#146936 = UNCERTAINTY_MEASURE_WITH_UNIT (LENGTH_MEASURE( 1.000000000000000082E-05 ), #179971, 'distance_accuracy_value', 'NONE');
#146937 = FACE_OUTER_BOUND ( 'NONE', #28509, .T. ) ;
#146938 = CARTESIAN_POINT ( 'NONE',  ( 4.543390873910913896, 5.433615786718446472, 1.082531754730549078 ) ) ;
#146939 = CARTESIAN_POINT ( 'NONE',  ( 4.685856777024981490, 6.842343872427582241, -1.228950205364977899 ) ) ;
#146940 = CARTESIAN_POINT ( 'NONE',  ( -10.33094986393327197, 11.15512238411806578, 0.7216878364870438212 ) ) ;
#146941 = CARTESIAN_POINT ( 'NONE',  ( 1.951734608585634190, -1.981729029064113856, 1.003908989668365948 ) ) ;
#146942 = CARTESIAN_POINT ( 'NONE',  ( 11.84668730067608600, 13.39999999999998259, 1.399999999999998579 ) ) ;
#146943 = CARTESIAN_POINT ( 'NONE',  ( -6.099189001301292379, 8.209082816308541197, 1.599625672291263179 ) ) ;
#146944 = CARTESIAN_POINT ( 'NONE',  ( 5.503720292143644777, 8.508425209887878538, 1.199719254218462483 ) ) ;
#146945 = CARTESIAN_POINT ( 'NONE',  ( 3.209375601822930690, -1.602329130913646926, -1.131729396966949963 ) ) ;
#146946 = CARTESIAN_POINT ( 'NONE',  ( 5.311043488251262268, 7.219303374425030562, -1.599625672291256295 ) ) ;
#146947 = CARTESIAN_POINT ( 'NONE',  ( -4.015218494013213402, 7.625434522713817387, 0.07065147036973244699 ) ) ;
#146948 = CARTESIAN_POINT ( 'NONE',  ( 4.857899112398166075, 4.561970474086296079, 1.040834085586084257E-14 ) ) ;
#146949 = CARTESIAN_POINT ( 'NONE',  ( -4.340018570150306232, 8.077455741901736985, -0.7216878364870338292 ) ) ;
#146950 = CARTESIAN_POINT ( 'NONE',  ( -7.700668062882084719, 8.086460282891644979, -0.7216878364870278340 ) ) ;
#146951 = CARTESIAN_POINT ( 'NONE',  ( 2.760144723603759065, 0.7592700852765141839, -1.980205354017528840 ) ) ;
#146952 = CARTESIAN_POINT ( 'NONE',  ( -6.798487682609798632, 6.896266815991691779, 0.7998128361456341429 ) ) ;
#146953 = CARTESIAN_POINT ( 'NONE',  ( 4.557600102482579629, 0.4766696971462945909, -2.108333899287537339 ) ) ;
#146954 = CARTESIAN_POINT ( 'NONE',  ( 2.753256032281672372, 1.832158412346639453, -0.1828795585285883096 ) ) ;
#146955 = CARTESIAN_POINT ( 'NONE',  ( -4.145011909418054863, 7.447386798385191575, 0.7030492056920457644 ) ) ;
#146956 = CARTESIAN_POINT ( 'NONE',  ( 1.364683531249988757, 0.6968750003414209138, 0.000000000000000000 ) ) ;
#146957 = CARTESIAN_POINT ( 'NONE',  ( 6.175711810462381379, -0.9247362235058408375, 1.474125693279482174 ) ) ;
#146958 = CARTESIAN_POINT ( 'NONE',  ( 10.85277107007934205, 3.956598013261175772, -3.932872935640606915 ) ) ;
#146959 = CARTESIAN_POINT ( 'NONE',  ( 4.772106882330221289, 6.590544000850479200, -1.443375672974051449 ) ) ;
#146960 = CARTESIAN_POINT ( 'NONE',  ( 11.01135777277261951, 10.09499145469730941, -1.400000000000001243 ) ) ;
#146961 = CARTESIAN_POINT ( 'NONE',  ( 3.379894511112140787, 1.369989894601089775, 1.672159933133889442 ) ) ;
#146962 = AXIS2_PLACEMENT_3D ( 'NONE', #165464, #792, #48537 ) ;
#146963 = CARTESIAN_POINT ( 'NONE',  ( 4.270861128529729989, -2.010896307770511537, 0.1455111863851859810 ) ) ;
#146964 = CARTESIAN_POINT ( 'NONE',  ( -7.659993601596706725, 11.88048360193076647, -0.7216878364870267237 ) ) ;
#146965 = CARTESIAN_POINT ( 'NONE',  ( 1.938557520917514987, 2.138169252768943984, 0.3173444169591658204 ) ) ;
#146966 = CARTESIAN_POINT ( 'NONE',  ( 2.917208927397921592, -0.1969847599093167145, 1.961514860040159292 ) ) ;
#146967 = CARTESIAN_POINT ( 'NONE',  ( 6.509000000000011887, 3.696273625755361447, 2.514342382328867753 ) ) ;
#146968 = CARTESIAN_POINT ( 'NONE',  ( 4.089352007823720214, -0.7402336266850146895, 1.795645171352943770 ) ) ;
#146971 = VERTEX_POINT ( 'NONE', #160246 ) ;
#146970 = CARTESIAN_POINT ( 'NONE',  ( 6.471393748265540147, 5.229711127717882491, 2.500000000000011102 ) ) ;
#146969 = CARTESIAN_POINT ( 'NONE',  ( -9.775065565328603157, 11.46695991671396087, -1.082531754730537976 ) ) ;
#146972 = CARTESIAN_POINT ( 'NONE',  ( -6.933015448541747006, 9.181880338089085214, 1.599625672291269396 ) ) ;
#146973 = CARTESIAN_POINT ( 'NONE',  ( 4.869313445963426190, 5.709895770826003414, 1.199719254218452935 ) ) ;
#146975 = ORIENTED_EDGE ( 'NONE', *, *, #82633, .T. ) ;
#146974 = CARTESIAN_POINT ( 'NONE',  ( -6.629010762438975135, 6.698543742459062145, -0.7998128361456362523 ) ) ;
#146976 = CARTESIAN_POINT ( 'NONE',  ( -7.483737604619046913, 11.67485160545682987, 0.000000000000000000 ) ) ;
#146977 = CARTESIAN_POINT ( 'NONE',  ( 0.9564373720404686363, 2.204146663617879476, -0.1098798544595935567 ) ) ;
#146979 = EDGE_CURVE ( 'NONE', #173456, #66261, #64610, .T. ) ;
#146978 = CARTESIAN_POINT ( 'NONE',  ( 1.642778471875001811, -1.392708332855374653, 2.845375778867859751 ) ) ;
#146980 = CARTESIAN_POINT ( 'NONE',  ( 4.996903459272755477, 0.3314677610860050083, 1.933379042443456486 ) ) ;
#146981 = CARTESIAN_POINT ( 'NONE',  ( -0.6823417656250212460, 5.613541667008087543, 1.181850606188767472 ) ) ;
#146982 = CARTESIAN_POINT ( 'NONE',  ( 0.7499999999999902300, 2.764583334016148974, 1.299038105676669330 ) ) ;
#146983 = CARTESIAN_POINT ( 'NONE',  ( 0.07459516483343267557, 2.058153987855536382, -2.173125978204577535 ) ) ;
#146984 = CARTESIAN_POINT ( 'NONE',  ( 4.400242069895500485, 1.421654421768648868, -1.169904355399861595 ) ) ;
#146985 = ORIENTED_EDGE ( 'NONE', *, *, #152817, .F. ) ;
#146986 = CARTESIAN_POINT ( 'NONE',  ( -1.225000000000010747, 2.312500000682803147, -2.081668171172168513E-14 ) ) ;
#146987 = CARTESIAN_POINT ( 'NONE',  ( -7.426115451983156923, 9.686887332112256388, -1.599625672291263179 ) ) ;
#146988 = CARTESIAN_POINT ( 'NONE',  ( 5.185831674374465905, 2.043064739972153543, -0.5678235988075125418 ) ) ;
#146989 = B_SPLINE_CURVE_WITH_KNOTS ( 'NONE', 3,
 ( #27983, #94079, #93011, #11719 ),
 .UNSPECIFIED., .F., .F.,
 ( 4, 4 ),
 ( 2.776912483567743746E-18, 0.0001591530304775611341 ),
 .UNSPECIFIED. ) ;
#146990 = CARTESIAN_POINT ( 'NONE',  ( -5.517647459709249524, 5.988123715949840609, -0.9547278355747212952 ) ) ;
#146991 = CARTESIAN_POINT ( 'NONE',  ( 6.823831386379729302, 6.855558127064808716, -0.7998128361456281477 ) ) ;
#146992 = ORIENTED_EDGE ( 'NONE', *, *, #77330, .T. ) ;
#146993 = CARTESIAN_POINT ( 'NONE',  ( 6.503207061003255518, 1.710746398682884140, 1.148667516769467767 ) ) ;
#146996 = CARTESIAN_POINT ( 'NONE',  ( 3.526749072549471453, -1.699942963128863838, 0.7078653300200200560 ) ) ;
#146995 = CARTESIAN_POINT ( 'NONE',  ( 1.240418688720058560, -1.814558931778247119, -0.4126190233522536444 ) ) ;
#146994 = DIRECTION ( 'NONE',  ( 0.000000000000000000, 0.000000000000000000, -1.000000000000000000 ) ) ;
#146997 = CARTESIAN_POINT ( 'NONE',  ( 9.108380270282433244, 9.520865158284665952, 1.040834085586084257E-14 ) ) ;
#146998 = CARTESIAN_POINT ( 'NONE',  ( 0.000000000000000000, -9.999999999999994671, 0.000000000000000000 ) ) ;
#146999 = CARTESIAN_POINT ( 'NONE',  ( -5.772739544368596043, 9.956889578397179363, -0.7998128361456362523 ) ) ;
#147000 = CARTESIAN_POINT ( 'NONE',  ( -15.75000000000000000, 12.69999999999999929, -3.600000000000000977 ) ) ;
#147001 = CARTESIAN_POINT ( 'NONE',  ( 3.440233207309027375, 0.9924059104887033023, -1.971224004288201881 ) ) ;
#147002 = CARTESIAN_POINT ( 'NONE',  ( 6.520815820410102326, 2.107438871474434983, 0.8233813407293107955 ) ) ;
#147003 = CARTESIAN_POINT ( 'NONE',  ( -6.019457014787517046, 9.006155036351978893, 1.082531754730548412 ) ) ;
#147004 = CARTESIAN_POINT ( 'NONE',  ( 5.537325978022108686, -0.03587880057049273180, 1.811405195203552587 ) ) ;
#147005 = CARTESIAN_POINT ( 'NONE',  ( 5.296063324668989658, -0.8673027158061608066, -1.708257925969633551 ) ) ;
#147006 = CARTESIAN_POINT ( 'NONE',  ( -1.201851678989727383E-14, 5.259375000341421469, -1.575800808251660134 ) ) ;
#147007 = CARTESIAN_POINT ( 'NONE',  ( 6.297708355432167338, -0.6282832542035889922, 1.762108908958268216 ) ) ;
#147008 = CARTESIAN_POINT ( 'NONE',  ( 6.074623017180313944, 1.249363044128497524, -1.379498876745478109 ) ) ;
#147009 = CARTESIAN_POINT ( 'NONE',  ( 6.614108672291515667, -0.8387186360741160085, -1.558468296174354784 ) ) ;
#147010 = CARTESIAN_POINT ( 'NONE',  ( 1.288296401830712368, -0.7303101666344159471, -1.879802715551846859 ) ) ;
#147012 = CARTESIAN_POINT ( 'NONE',  ( 2.614012881481563522, -2.083059734262616036, 0.3096129728813925008 ) ) ;
#147011 = CARTESIAN_POINT ( 'NONE',  ( -8.208571938070008400, 11.66408546346865016, -1.199719254218446718 ) ) ;
#147013 = AXIS2_PLACEMENT_3D ( 'NONE', #67130, #137506, #202459 ) ;
#147014 = CARTESIAN_POINT ( 'NONE',  ( 8.748035429315576650, 11.22912730566677553, -1.599625672291255185 ) ) ;
#147016 = CARTESIAN_POINT ( 'NONE',  ( -8.317037166979361018, 11.79062823052953668, 1.199719254218453823 ) ) ;
#147015 = CARTESIAN_POINT ( 'NONE',  ( 0.000000000000000000, 12.31951671548121219, 0.000000000000000000 ) ) ;
#147018 = ADVANCED_FACE ( 'NONE', ( #211109 ), #126766, .T. ) ;
#147017 = CARTESIAN_POINT ( 'NONE',  ( 1.441672106306312484, -1.900340447277752087, 0.6846001189487918026 ) ) ;
#147019 = CARTESIAN_POINT ( 'NONE',  ( -1.364683531250010295, 4.030208333674751842, 0.7879004041258379498 ) ) ;
#147020 = CARTESIAN_POINT ( 'NONE',  ( 4.708759422647839976, 4.387974169377582001, -0.7998128361456211532 ) ) ;
#147021 = CARTESIAN_POINT ( 'NONE',  ( 3.145949958485740883, 0.7812230816454240889, -2.015650884352723882 ) ) ;
#147022 = CARTESIAN_POINT ( 'NONE',  ( 6.610000000000009202, 6.036727194997777879, 2.594899704271665275 ) ) ;
#147023 = CARTESIAN_POINT ( 'NONE',  ( 5.657495238652423097, 9.822437888394988548, 0.000000000000000000 ) ) ;
#147025 = EDGE_CURVE ( 'NONE', #67059, #204013, #38908, .T. ) ;
#147024 = CARTESIAN_POINT ( 'NONE',  ( 8.798878505144646311, 11.28844422746735532, -1.443375672974052559 ) ) ;
#147026 = CARTESIAN_POINT ( 'NONE',  ( 9.019512274088125281, 14.59495137906214346, -7.915989402198163383 ) ) ;
#147027 = CARTESIAN_POINT ( 'NONE',  ( -8.053180056837398126, 8.497724275839514618, 0.7216878364870578100 ) ) ;
#147028 = EDGE_CURVE ( 'NONE', #157913, #150798, #206699, .T. ) ;
#147029 = CARTESIAN_POINT ( 'NONE',  ( 0.6823417656249899377, 1.342708333674752508, 1.181850606188755259 ) ) ;
#147030 = CARTESIAN_POINT ( 'NONE',  ( 0.5389544483674936215, -1.876709678404146153, 1.131566444868239874 ) ) ;
#147031 = CARTESIAN_POINT ( 'NONE',  ( 0.5059764118015197543, 7.965522150964524428, 1.935091031283028506 ) ) ;
#147032 = CARTESIAN_POINT ( 'NONE',  ( 2.852682258652036840, 0.7612096163719231923, 2.130753183350143409 ) ) ;
#147033 = CARTESIAN_POINT ( 'NONE',  ( -6.672584156219988571, 10.93643194889866521, -0.7998128361456291469 ) ) ;
#147034 = CARTESIAN_POINT ( 'NONE',  ( -3.538314903042294457, 6.111489239315849531, 1.082531754730560403 ) ) ;
#147035 = CARTESIAN_POINT ( 'NONE',  ( -1.201851678989727383E-14, 3.009375000341419248, -1.575800808251660134 ) ) ;
#147036 = CARTESIAN_POINT ( 'NONE',  ( 4.743613802917549194, 8.193193991156523026, -0.7244234545457691743 ) ) ;
#147037 = CARTESIAN_POINT ( 'NONE',  ( -1.500000000000001110, 11.02083333333333393, 0.8660254037844419273 ) ) ;
#147038 = CARTESIAN_POINT ( 'NONE',  ( 3.553118775233146120, 6.302999783484076524, -1.199719254218453823 ) ) ;
#147039 = CARTESIAN_POINT ( 'NONE',  ( 3.584973236653755002, 1.601158291227417152, -0.7540797108817003380 ) ) ;
#147041 = AXIS2_PLACEMENT_3D ( 'NONE', #61513, #63647, #95105 ) ;
#147040 = CARTESIAN_POINT ( 'NONE',  ( 6.739307351729481255, -1.974284904759715298, 0.9861035376414882814 ) ) ;
#147042 = CARTESIAN_POINT ( 'NONE',  ( -8.012344526598182026E-15, 9.046875000341405126, -1.575800808251669460 ) ) ;
#147043 = CARTESIAN_POINT ( 'NONE',  ( -6.557303570864871034, 7.679217583210999010, -1.199719254218452047 ) ) ;
#147044 = CARTESIAN_POINT ( 'NONE',  ( 4.710564641745673242, 1.930423983604495630, 0.5826390268678025564 ) ) ;
#147045 = ORIENTED_EDGE ( 'NONE', *, *, #88712, .T. ) ;
#147046 = EDGE_CURVE ( 'NONE', #71330, #19391, #141048, .T. ) ;
#147047 = CARTESIAN_POINT ( 'NONE',  ( 3.326877442632663939, 0.04465521416292458912, 1.870282673472216439 ) ) ;
#147048 = CARTESIAN_POINT ( 'NONE',  ( 3.450112209602332669, -0.8433740631265237431, 1.890881698631073249 ) ) ;
#147049 = EDGE_CURVE ( 'NONE', #39641, #90767, #168659, .T. ) ;
#147050 = CARTESIAN_POINT ( 'NONE',  ( -5.912764388891193157, 9.912325863766124456, 0.000000000000000000 ) ) ;
#147052 =( GEOMETRIC_REPRESENTATION_CONTEXT ( 3 ) GLOBAL_UNCERTAINTY_ASSIGNED_CONTEXT ( ( #97359 ) ) GLOBAL_UNIT_ASSIGNED_CONTEXT ( ( #56717, #104406, #4722 ) ) REPRESENTATION_CONTEXT ( 'NONE', 'WORKASPACE' ) );
#147051 = CARTESIAN_POINT ( 'NONE',  ( -0.6383513625407253311, 3.364918466673215924, -0.1381026099400331497 ) ) ;
#147053 = FACE_OUTER_BOUND ( 'NONE', #210317, .T. ) ;
#147054 = CARTESIAN_POINT ( 'NONE',  ( 0.6823417656249917140, 4.905208333674755394, 1.181850606188765695 ) ) ;
#147055 = CARTESIAN_POINT ( 'NONE',  ( 1.300873410958070409, -0.2835801433653042380, -1.891145142470892715 ) ) ;
#147056 = VECTOR ( 'NONE', #91982, 1000.000000000000000 ) ;
#147057 = CARTESIAN_POINT ( 'NONE',  ( 2.348037267531626338, -0.8415878996531295231, 1.772339229757218471 ) ) ;
#147058 = CARTESIAN_POINT ( 'NONE',  ( 1.001327120302420548, 1.985796081718914419, 0.3474166314290441648 ) ) ;
#147059 = CARTESIAN_POINT ( 'NONE',  ( -4.339491684825780737, 7.220434844675483355, -1.199719254218455378 ) ) ;
#147061 = CARTESIAN_POINT ( 'NONE',  ( -1.266973501737287178, 3.781478720974876140, -0.4964169966120759447 ) ) ;
#147060 = CARTESIAN_POINT ( 'NONE',  ( 8.772289083241844310, 10.19309100432570148, -1.199719254218446718 ) ) ;
#147062 = CARTESIAN_POINT ( 'NONE',  ( 0.1747926744264660381, 0.006858446013176254172, -1.855468577918440776 ) ) ;
#147063 = CARTESIAN_POINT ( 'NONE',  ( 1.364683531249988535, 2.863541667008082658, 0.7879004041258500513 ) ) ;
#147064 = CARTESIAN_POINT ( 'NONE',  ( 2.074478728756317114, 0.8647236062047275462, 1.818190761793165189 ) ) ;
#147066 = CARTESIAN_POINT ( 'NONE',  ( 2.038805038046047624, -1.634495437704911458, 1.345740563223641217 ) ) ;
#147065 = CARTESIAN_POINT ( 'NONE',  ( -7.727784370109414880, 8.118095974656867497, 0.7216878364870578100 ) ) ;
#147067 = CARTESIAN_POINT ( 'NONE',  ( 8.776573235218638303, 13.27486625357122385, -8.183627694784497919 ) ) ;
#147068 = CARTESIAN_POINT ( 'NONE',  ( 3.877443546529443452, -0.1552652338182025915, 2.064615508632794860 ) ) ;
#147069 = CARTESIAN_POINT ( 'NONE',  ( 5.259637247458703868, 5.100941308315409373, 0.000000000000000000 ) ) ;
#147071 = CARTESIAN_POINT ( 'NONE',  ( 2.920892028740289081, 5.495125569250587816, 1.199719254218452047 ) ) ;
#147070 = CARTESIAN_POINT ( 'NONE',  ( 5.332010518800971433, 2.059573894497103819, 0.3580650863252275440 ) ) ;
#147073 = ORIENTED_EDGE ( 'NONE', *, *, #112984, .T. ) ;
#147072 = CARTESIAN_POINT ( 'NONE',  ( 4.348545414961950684, 0.4871326187540457875, 1.759326811173238303 ) ) ;
#147074 = CARTESIAN_POINT ( 'NONE',  ( 8.971744963941056028, 11.49012176272984931, 1.599625672291281386 ) ) ;
#147075 =( LENGTH_UNIT ( ) NAMED_UNIT ( * ) SI_UNIT ( .MILLI., .METRE. ) );
#147076 = CARTESIAN_POINT ( 'NONE',  ( 11.99987416209243385, 8.248970243831804439, 3.607522456176011971 ) ) ;
#147077 = CARTESIAN_POINT ( 'NONE',  ( 6.440462174652990868, 2.181831651002089423, 0.3301269925025315799 ) ) ;
#147078 = CARTESIAN_POINT ( 'NONE',  ( -8.012344526598182026E-15, 10.60937500034139624, -1.575800808251669460 ) ) ;
#147079 = CARTESIAN_POINT ( 'NONE',  ( 5.443983014310386892, -1.216401775450553169, -1.475513148251464068 ) ) ;
#147080 = CARTESIAN_POINT ( 'NONE',  ( -4.308793891044708779, 3.921347715840572956, 1.214306433183764966E-14 ) ) ;
#147081 = CARTESIAN_POINT ( 'NONE',  ( 5.770966940911189447, 9.884545197705074671, -0.7998128361456291469 ) ) ;
#147082 = CARTESIAN_POINT ( 'NONE',  ( -1.360316468750004448, 1.671875000341424666, -8.673617379884035472E-15 ) ) ;
#147083 = CARTESIAN_POINT ( 'NONE',  ( 4.894130264408854458, 6.732904613275549899, -1.443375672974051449 ) ) ;
#147084 = DIRECTION ( 'NONE',  ( 1.779758311459929505E-16, 0.000000000000000000, -1.000000000000000000 ) ) ;
#147085 = CARTESIAN_POINT ( 'NONE',  ( 7.299895746552897968, 14.53718666743123045, -9.471644787737316662 ) ) ;
#147086 = CARTESIAN_POINT ( 'NONE',  ( 0.8898994657863326108, -0.4472179738511591895, -1.785967584704901912 ) ) ;
#147087 = ORIENTED_EDGE ( 'NONE', *, *, #15780, .T. ) ;
#147088 = CARTESIAN_POINT ( 'NONE',  ( -5.738844160334429567, 9.917344963690652548, 0.000000000000000000 ) ) ;
#147089 = CARTESIAN_POINT ( 'NONE',  ( 4.674985431947434655, 0.001863223488791227334, -1.870726058175266715 ) ) ;
#147090 = CARTESIAN_POINT ( 'NONE',  ( -0.02299388927986567924, 4.093419149701410298, -2.466026074291859160 ) ) ;
#147091 = DIRECTION ( 'NONE',  ( 1.000000000000000000, 0.000000000000000000, 0.000000000000000000 ) ) ;
#147092 = DIRECTION ( 'NONE',  ( -1.207943261119674327E-30, -2.168404344971008079E-15, -1.000000000000000000 ) ) ;
#147093 = AXIS2_PLACEMENT_3D ( 'NONE', #166917, #99779, #81394 ) ;
#147094 = CARTESIAN_POINT ( 'NONE',  ( -5.395781948558855845, 9.238903340053241209, 0.7216878364870458196 ) ) ;
#147095 = CARTESIAN_POINT ( 'NONE',  ( 5.834086172582112262, 5.700855377634248100, 1.040834085586084257E-14 ) ) ;
#147096 = CARTESIAN_POINT ( 'NONE',  ( 1.340603599695965764, -1.920222134930357427, -0.4367614745469716730 ) ) ;
#147097 = CARTESIAN_POINT ( 'NONE',  ( 1.968375273883906429, -1.978056371059619511, -0.3905749819678172585 ) ) ;
#147098 = CARTESIAN_POINT ( 'NONE',  ( -9.169391961543940539, 9.592045464756413509, 1.040834085586084257E-14 ) ) ;
#147099 = CARTESIAN_POINT ( 'NONE',  ( 6.540882763950133238, 6.595727744222092959, 0.000000000000000000 ) ) ;
#147100 = DIRECTION ( 'NONE',  ( 1.000000000000000000, 0.000000000000000000, 0.000000000000000000 ) ) ;
#147101 = CARTESIAN_POINT ( 'NONE',  ( 2.414256260463796711, 1.430409426244143134, -1.660321623440104810 ) ) ;
#147102 = CARTESIAN_POINT ( 'NONE',  ( -5.554920708491585479, 5.909662090865936079, -0.8338897427195167689 ) ) ;
#147103 = CARTESIAN_POINT ( 'NONE',  ( -8.459397779922852578, 11.95671561229694824, 1.199719254218453823 ) ) ;
#147104 = CARTESIAN_POINT ( 'NONE',  ( -1.499999999999997780, 7.388542872122518368, -4.154462424328208670 ) ) ;
#147105 = CARTESIAN_POINT ( 'NONE',  ( 4.609409038966229666, 6.400729850259146758, -1.443375672974051449 ) ) ;
#147106 = CARTESIAN_POINT ( 'NONE',  ( -10.30104275384242740, 4.689840931292195592, -5.506867539468097483 ) ) ;
#147107 = CARTESIAN_POINT ( 'NONE',  ( 8.880754312151170282, 10.31963377138658089, 1.199719254218453823 ) ) ;
#147108 = CARTESIAN_POINT ( 'NONE',  ( -9.445283354644281815, 15.31899899171029666, 7.300214616139077073 ) ) ;
#147109 = CARTESIAN_POINT ( 'NONE',  ( 6.699137298928153683, 7.948653282571920720, 1.082531754730549967 ) ) ;
#147110 = ORIENTED_EDGE ( 'NONE', *, *, #9580, .F. ) ;
#147112 = CARTESIAN_POINT ( 'NONE',  ( 2.297522961200649139, 1.839619113207457524, -0.8179307585152847393 ) ) ;
#147111 = CARTESIAN_POINT ( 'NONE',  ( 5.425302022954732628, -1.172690680311109901, -1.419496581506813904 ) ) ;
#147113 = CARTESIAN_POINT ( 'NONE',  ( 3.638291363623618047, 0.06041265439583366065, -2.297745614018332105 ) ) ;
#147115 = CARTESIAN_POINT ( 'NONE',  ( 1.586513592238134374, 1.791619466816740003, 0.5028711289422735931 ) ) ;
#147114 = CARTESIAN_POINT ( 'NONE',  ( -0.1290005225502432740, 4.081813041011835175, -2.728655865233818201 ) ) ;
#147116 = CARTESIAN_POINT ( 'NONE',  ( 3.285556943750000070, -3.084374999522042415, 0.000000000000000000 ) ) ;
#147117 = CARTESIAN_POINT ( 'NONE',  ( 4.000000000000012434, 0.000000000000000000, 0.7500000000000006661 ) ) ;
#147118 = CARTESIAN_POINT ( 'NONE',  ( 6.135011676971934058, 1.786887936952135991, 0.6819008164158719687 ) ) ;
#147119 = CARTESIAN_POINT ( 'NONE',  ( -7.133561379084627063, 11.47423870890741782, 0.7998128361456481317 ) ) ;
#147120 = CARTESIAN_POINT ( 'NONE',  ( -6.211043768836215229, 8.339580045099285854, 1.443375672974064550 ) ) ;
#147122 = CARTESIAN_POINT ( 'NONE',  ( 3.098369316282158614, -0.5415621961667067552, -1.790553177708480215 ) ) ;
#147121 = CARTESIAN_POINT ( 'NONE',  ( 5.108965175345551835, -0.3053309577524323526, 2.068188354190988676 ) ) ;
#147123 = CARTESIAN_POINT ( 'NONE',  ( 7.782016984564060103, 9.141736572488651902, 1.082531754730558626 ) ) ;
#147124 = CARTESIAN_POINT ( 'NONE',  ( 5.794452930745782382, 1.501506822132542718, -1.065412412061928160 ) ) ;
#147125 = CARTESIAN_POINT ( 'NONE',  ( 2.184835310096557404, 5.700724961754617404, 1.040834085586084257E-14 ) ) ;
#147126 = CARTESIAN_POINT ( 'NONE',  ( 4.843287188579786573, 6.673587691474970107, -1.599625672291256295 ) ) ;
#147127 = CARTESIAN_POINT ( 'NONE',  ( 4.934089290906335634, 0.8825209879863432638, -1.481864930267517089 ) ) ;
#147128 = CARTESIAN_POINT ( 'NONE',  ( -5.038826645773246682, 9.030381520044109322, 0.7998128361456481317 ) ) ;
#147129 =( NAMED_UNIT ( * ) PLANE_ANGLE_UNIT ( ) SI_UNIT ( $, .RADIAN. ) );
#147130 = CARTESIAN_POINT ( 'NONE',  ( -10.39230484541327826, 3.447199233515649386, -5.999999999999975131 ) ) ;
#147132 = CARTESIAN_POINT ( 'NONE',  ( 4.768535058008659178, -0.9225228719554872114, -1.965435229472652479 ) ) ;
#147131 = B_SPLINE_CURVE_WITH_KNOTS ( 'NONE', 3,
 ( #77840, #110420, #191578, #176423, #28030, #73578 ),
 .UNSPECIFIED., .F., .F.,
 ( 4, 2, 4 ),
 ( 0.000000000000000000, 0.0003172254002810694388, 0.0006344508005621388776 ),
 .UNSPECIFIED. ) ;
#147133 = CARTESIAN_POINT ( 'NONE',  ( 3.598116246361187542, -1.823677485248562435, -0.08826725125678223927 ) ) ;
#147134 = CARTESIAN_POINT ( 'NONE',  ( 0.7429250141685153075, -0.2344385519315282107, -1.947609053799495227 ) ) ;
#147135 = CARTESIAN_POINT ( 'NONE',  ( 6.192584684491233560, 1.567513771475435247, -1.423521977300482577 ) ) ;
#147137 = CARTESIAN_POINT ( 'NONE',  ( 0.6823417656249899377, 3.488541667008085323, -1.181850606188754593 ) ) ;
#147136 = CARTESIAN_POINT ( 'NONE',  ( 5.864811835480173485, 0.1724426041235416485, -2.285918041817245783 ) ) ;
#147138 = CARTESIAN_POINT ( 'NONE',  ( -1.499999999999993339, 10.64264068711930733, 1.232676135170975238E-14 ) ) ;
#147139 = CARTESIAN_POINT ( 'NONE',  ( 8.727698198895078363, 11.20540053684285553, -1.599625672291257406 ) ) ;
#147140 = EDGE_CURVE ( 'NONE', #198442, #52032, #132014, .T. ) ;
#147141 = CARTESIAN_POINT ( 'NONE',  ( 1.963691422110905638, -1.704870618661393999, -1.260721693921822428 ) ) ;
#147142 = CARTESIAN_POINT ( 'NONE',  ( -3.253593677599670109, 5.779314476299451719, 1.082531754730560403 ) ) ;
#147143 =( NAMED_UNIT ( * ) SI_UNIT ( $, .STERADIAN. ) SOLID_ANGLE_UNIT ( ) );
#147144 = CARTESIAN_POINT ( 'NONE',  ( -3.240035523541616502, 6.723865844199768738, 0.7216878364870317197 ) ) ;
#147145 = CARTESIAN_POINT ( 'NONE',  ( 6.350449713519967787, -2.159805286613075470, -0.2212482231108928721 ) ) ;
#147147 = CARTESIAN_POINT ( 'NONE',  ( 0.7500000000000006661, 11.94791666734946389, -1.299038105676657340 ) ) ;
#147146 = CARTESIAN_POINT ( 'NONE',  ( 6.983263157960386991, 6.036006179461032239, 2.548702536770989457 ) ) ;
#147150 = VERTEX_POINT ( 'NONE', #42253 ) ;
#147149 = CARTESIAN_POINT ( 'NONE',  ( 2.280208067491045654, 2.177836876428246971, -0.4364916025852043635 ) ) ;
#147148 = COLOUR_RGB ( '', 0.66274510, 0.83137255, 0.94901961) ;
#147151 = CARTESIAN_POINT ( 'NONE',  ( 6.522112240665402183, -1.799906897009293738, 0.9091900463213120620 ) ) ;
#147153 = CARTESIAN_POINT ( 'NONE',  ( 6.034046607691841757, 1.223980295139483809, 1.660032098485002994 ) ) ;
#147152 = CARTESIAN_POINT ( 'NONE',  ( 3.174580523894166006, 6.855427711185178019, 0.7998128361456341429 ) ) ;
#147155 = CARTESIAN_POINT ( 'NONE',  ( 3.475000000000000533, -2.304166666666668473, 2.006292185433948827 ) ) ;
#147154 = CARTESIAN_POINT ( 'NONE',  ( 5.499767588998890844, 6.445425604367387429, 1.199719254218451159 ) ) ;
#147156 = CARTESIAN_POINT ( 'NONE',  ( 4.603875680292229156, 7.528882839386387360, 1.199719254218452047 ) ) ;
#147157 = CARTESIAN_POINT ( 'NONE',  ( 3.285556943750000070, -3.521874999522042859, 0.000000000000000000 ) ) ;
#147158 = CARTESIAN_POINT ( 'NONE',  ( 0.1333542156527582345, 4.089120883327095335, -2.600857804679152174 ) ) ;
#147159 = CARTESIAN_POINT ( 'NONE',  ( 5.442854017605395889, -1.455216020186438364, -1.127989967910733915 ) ) ;
#147160 = CARTESIAN_POINT ( 'NONE',  ( 5.464099601507359516, 6.333536608968757697, 1.199719254218462483 ) ) ;
#147161 = CARTESIAN_POINT ( 'NONE',  ( -0.2104748580754408904, 1.337026610731705700, -2.356057411969681326 ) ) ;
#147162 = CARTESIAN_POINT ( 'NONE',  ( 2.115808521728879565, -0.8096002590626363293, -1.522937571937353241 ) ) ;
#147163 = CARTESIAN_POINT ( 'NONE',  ( 0.09298292169932984019, 1.756857073293972116, 0.9896806593640145033 ) ) ;
#147164 = CARTESIAN_POINT ( 'NONE',  ( 2.233388324916096845, 2.298236692437699791, 0.05235245155727624722 ) ) ;
#147165 = CARTESIAN_POINT ( 'NONE',  ( 1.364683531249990311, 3.946875000341417028, 1.214306433183764966E-14 ) ) ;
#147166 = CARTESIAN_POINT ( 'NONE',  ( 2.689068300184436655, -0.3842959826076980390, -2.229375072012912629 ) ) ;
#147167 = CARTESIAN_POINT ( 'NONE',  ( 4.090527498900095260, -2.083119126933795418, -0.3091809127075405006 ) ) ;
#147168 = CARTESIAN_POINT ( 'NONE',  ( -5.157951095356222204, 4.982307464195829816, 0.000000000000000000 ) ) ;
#147169 = CARTESIAN_POINT ( 'NONE',  ( 2.793947764029936831, -1.764715128225034180, -0.1343432132955291736 ) ) ;
#147170 = CARTESIAN_POINT ( 'NONE',  ( 7.461064606222022277, 7.598996883547496139, 1.040834085586084257E-14 ) ) ;
#147171 = CARTESIAN_POINT ( 'NONE',  ( 4.217995187182920880, 6.974725914138481642, 1.082531754730549078 ) ) ;
#147172 = CARTESIAN_POINT ( 'NONE',  ( -5.388475986427523345, 8.373973519885682393, 1.199719254218452047 ) ) ;
#147173 = UNCERTAINTY_MEASURE_WITH_UNIT (LENGTH_MEASURE( 1.000000000000000082E-05 ), #131230, 'distance_accuracy_value', 'NONE');
#147174 = CARTESIAN_POINT ( 'NONE',  ( -1.499999999999997780, 1.900000000000019673, 0.000000000000000000 ) ) ;
#147175 = CARTESIAN_POINT ( 'NONE',  ( 6.187741696929490054, 2.126074299989196614, -0.6436727651782292448 ) ) ;
#147176 = CARTESIAN_POINT ( 'NONE',  ( 3.679775893577118318, -1.080384588543949809, 1.906543112819548913 ) ) ;
#147177 = CARTESIAN_POINT ( 'NONE',  ( -5.135841261478327979, 4.886236314679810455, 0.7998128361456341429 ) ) ;
#147178 = CARTESIAN_POINT ( 'NONE',  ( 0.3176981287468615966, 7.220460999378246036, -2.081427265489023348 ) ) ;
#147179 = CARTESIAN_POINT ( 'NONE',  ( -3.456965981804629884, 6.976951378839947537, 1.040834085586084257E-14 ) ) ;
#147180 = CARTESIAN_POINT ( 'NONE',  ( 1.364683531249990311, 3.634375000341416584, 1.214306433183764966E-14 ) ) ;
#147181 = CARTESIAN_POINT ( 'NONE',  ( -8.012344526598182026E-15, 8.796875000341401574, -1.575800808251669460 ) ) ;
#147183 = CARTESIAN_POINT ( 'NONE',  ( -2.792616454734997866, 6.201876930592042925, 0.7216878364870317197 ) ) ;
#147182 = AXIS2_PLACEMENT_3D ( 'NONE', #131139, #45578, #178773 ) ;
#147184 = CARTESIAN_POINT ( 'NONE',  ( 5.607717026683647354, 1.607092460389969446, 1.383685132418293495 ) ) ;
#147185 = CARTESIAN_POINT ( 'NONE',  ( -6.807602527837528505, 7.114826835331461652, 0.7216878364870317197 ) ) ;
#147186 = VERTEX_POINT ( 'NONE', #11847 ) ;
#147188 = CARTESIAN_POINT ( 'NONE',  ( 4.221170328939424010, 7.164078207821040323, 1.167600677116547470 ) ) ;
#147187 = CARTESIAN_POINT ( 'NONE',  ( -3.824808732831001201, 7.476377598362539345, 0.7216878364870338292 ) ) ;
#147189 = CARTESIAN_POINT ( 'NONE',  ( 4.320244504248938355, 8.192035688265757898, 1.040834085586084257E-14 ) ) ;
#147190 = CARTESIAN_POINT ( 'NONE',  ( 5.970224376651539266, -1.750504005202535796, -0.5711807346103907612 ) ) ;
#147191 = CARTESIAN_POINT ( 'NONE',  ( 0.04331300497836985952, 7.063164988974223846, -3.968916547456744492 ) ) ;
#147192 = CARTESIAN_POINT ( 'NONE',  ( 1.364683531249988535, 4.217708333674752730, -0.7879004041258239610 ) ) ;
#147193 = CARTESIAN_POINT ( 'NONE',  ( 2.155425581425034487, 0.7450078602235529202, 1.573079536267004030 ) ) ;
#147194 = CARTESIAN_POINT ( 'NONE',  ( -6.274419661981678331, 6.542771797459788097, -0.3271847599185794819 ) ) ;
#147195 = CARTESIAN_POINT ( 'NONE',  ( -9.579764304849261336, -9.999999999999998224, 0.06720017513373673090 ) ) ;
#147196 = CARTESIAN_POINT ( 'NONE',  ( 1.364683531249988757, -0.3031249996585799744, 0.000000000000000000 ) ) ;
#147197 = CARTESIAN_POINT ( 'NONE',  ( 3.811250579217332568, 5.539821323877241355, 1.214306433183764966E-14 ) ) ;
#147198 = CARTESIAN_POINT ( 'NONE',  ( -7.797910906154257304, 12.24931315715533486, 0.000000000000000000 ) ) ;
#147199 = CARTESIAN_POINT ( 'NONE',  ( -6.738039155867462604, 7.923762439009225389, 1.082531754730549967 ) ) ;
#147200 = CIRCLE ( 'NONE', #64175, 2.150000000000006573 ) ;
#147201 = CARTESIAN_POINT ( 'NONE',  ( 5.858325616802108726, 0.8718737102157668728, 1.978260574764856283 ) ) ;
#147203 = ORIENTED_EDGE ( 'NONE', *, *, #117177, .T. ) ;
#147202 = CARTESIAN_POINT ( 'NONE',  ( -3.984117037569407938, 5.741498858621315371, 1.599625672291270506 ) ) ;
#147204 = CARTESIAN_POINT ( 'NONE',  ( 0.6823417656249917140, 4.592708333674755394, 1.181850606188765695 ) ) ;
#147205 = CARTESIAN_POINT ( 'NONE',  ( 5.677018108359257020, -0.04579235393691384604, -1.970973552702318443 ) ) ;
#147206 = CARTESIAN_POINT ( 'NONE',  ( 4.973871655188280450, 1.509253006592145452, 0.8532917887605420137 ) ) ;
#147208 = CARTESIAN_POINT ( 'NONE',  ( 1.980270094416748394, -2.150034404144373301, -0.4237573071887782983 ) ) ;
#147207 = CARTESIAN_POINT ( 'NONE',  ( -1.360316468750034868, -0.8802083329919301313, -0.7853790794159242195 ) ) ;
#147209 = CARTESIAN_POINT ( 'NONE',  ( 3.768876097860610397, -1.551941239651495108, 1.707908033328522146 ) ) ;
#147210 = CARTESIAN_POINT ( 'NONE',  ( 4.815729912100211507, -2.021797975182148654, 0.3980178507551126454 ) ) ;
#147211 = CARTESIAN_POINT ( 'NONE',  ( 1.341630539043844106, 1.939701883965805562, 0.09577479888067677583 ) ) ;
#147212 = CARTESIAN_POINT ( 'NONE',  ( -7.036318535368094373, 7.311385834125318617, 0.7216878364870317197 ) ) ;
#147213 = CIRCLE ( 'NONE', #29553, 0.04999999999999937828 ) ;
#147214 = CARTESIAN_POINT ( 'NONE',  ( -5.276058054373441664, 6.184431147304315424, -1.199719254218453823 ) ) ;
#147215 = DIRECTION ( 'NONE',  ( -8.638326563840814399E-31, 0.000000000000000000, -1.000000000000000000 ) ) ;
#147216 = CARTESIAN_POINT ( 'NONE',  ( 3.744478000529617656, 1.131475959888720295, -1.793321066073015224 ) ) ;
#147217 = FACE_OUTER_BOUND ( 'NONE', #85141, .T. ) ;
#147218 = CARTESIAN_POINT ( 'NONE',  ( 2.760388869050140137, 1.913803604375517109, -0.6351994527180188088 ) ) ;
#147219 = CARTESIAN_POINT ( 'NONE',  ( -4.406036734316882253, 8.084200590104265061, -0.7216878364870257245 ) ) ;
#147220 = CARTESIAN_POINT ( 'NONE',  ( 4.682781310676605635, -2.139571651222616833, -0.5399477217277389718 ) ) ;
#147221 = CARTESIAN_POINT ( 'NONE',  ( -4.741649638052999549, 5.202212439478444139, 1.069586989871945670 ) ) ;
#147222 = CARTESIAN_POINT ( 'NONE',  ( -2.529473476623105288, -3.056106844972871439, 2.371225858872531234 ) ) ;
#147223 = DIRECTION ( 'NONE',  ( 0.000000000000000000, 1.000000000000000000, 0.000000000000000000 ) ) ;
#147224 = CARTESIAN_POINT ( 'NONE',  ( -7.747558435566414659, 8.003516027774422170, -0.7998128361456362523 ) ) ;
#147226 = CARTESIAN_POINT ( 'NONE',  ( 1.499999999999963141, 8.500000000000000000, -9.886859966642596476 ) ) ;
#147225 = CARTESIAN_POINT ( 'NONE',  ( -5.621078624820424530, 7.474595091574217420, 1.344519841555512629 ) ) ;
#147227 = SURFACE_STYLE_USAGE ( .BOTH. , #131028 ) ;
#147228 = ORIENTED_EDGE ( 'NONE', *, *, #115159, .F. ) ;
#147229 = CARTESIAN_POINT ( 'NONE',  ( 4.487218586473323612, 1.841840323776536614, -0.9247287835071598128 ) ) ;
#147230 = CARTESIAN_POINT ( 'NONE',  ( 0.6801582343749952297, 2.807291667008070313, -1.178068619123883165 ) ) ;
#147231 = CARTESIAN_POINT ( 'NONE',  ( -3.428579710538708225E-15, -7.630846356335694303, 9.566809970446875866 ) ) ;
#147232 = CARTESIAN_POINT ( 'NONE',  ( -3.879604511804807032, 7.677955697080923514, 0.7998128361456341429 ) ) ;
#147233 = CARTESIAN_POINT ( 'NONE',  ( 3.352217588874096599, 0.9059935441126705236, -1.805122612331450105 ) ) ;
#147234 = CARTESIAN_POINT ( 'NONE',  ( -1.500000000000001332, 0.1500000000000251132, 0.000000000000000000 ) ) ;
#147235 = CARTESIAN_POINT ( 'NONE',  ( 8.758204044747994743, 12.20135990463928266, 1.082531754730546636 ) ) ;
#147236 = CARTESIAN_POINT ( 'NONE',  ( 6.500244582748090139, 9.671036882259738121, 1.199719254218460707 ) ) ;
#147237 = CARTESIAN_POINT ( 'NONE',  ( 2.782161975763951300, -1.060548055690222702, 1.766919142140084720 ) ) ;
#147238 = CARTESIAN_POINT ( 'NONE',  ( 6.983263157960365675, -0.006178392973848687020, 2.053544886540019210 ) ) ;
#147239 = CARTESIAN_POINT ( 'NONE',  ( 5.854423403002611437, 5.724582146458163656, 1.040834085586084257E-14 ) ) ;
#147240 = CARTESIAN_POINT ( 'NONE',  ( -0.2409995289980038091, 6.947781193150415646, -2.595509233728268583 ) ) ;
#147241 = CARTESIAN_POINT ( 'NONE',  ( 1.482094074889642288, -0.2687121449159133313, -1.821302815977184686 ) ) ;
#147242 = CARTESIAN_POINT ( 'NONE',  ( 0.4698728525199142303, 0.2201595520019784535, -2.297181220480988717 ) ) ;
#147243 = CARTESIAN_POINT ( 'NONE',  ( 7.212011367826596242, 7.378711115411311638, 0.000000000000000000 ) ) ;
#147244 = CARTESIAN_POINT ( 'NONE',  ( 2.091316376603330252, 1.881825464268515269, -1.063406855978922039 ) ) ;
#147245 = CARTESIAN_POINT ( 'NONE',  ( -2.968872451712654126, 6.407508927065978632, 1.040834085586084257E-14 ) ) ;
#147246 = CARTESIAN_POINT ( 'NONE',  ( 2.290250256651988892, -0.7762311197250795214, -1.861343989391924358 ) ) ;
#147247 = CARTESIAN_POINT ( 'NONE',  ( 0.5670072068131201126, 0.1877032549213939472, -1.861219751863735672 ) ) ;
#147248 = CARTESIAN_POINT ( 'NONE',  ( 4.856303703212550893, 0.7536814072931929953, 1.821903339724652460 ) ) ;
#147249 = CARTESIAN_POINT ( 'NONE',  ( 5.173064673083394460, 1.776168143800487043, -0.9548534231369476544 ) ) ;
#147251 = CARTESIAN_POINT ( 'NONE',  ( 8.365017589507326434, 12.70301158782650397, -0.7216878364870338292 ) ) ;
#147250 = CARTESIAN_POINT ( 'NONE',  ( -1.364683531250012516, 3.988541667008088876, -0.7879004041258300672 ) ) ;
#147253 = CARTESIAN_POINT ( 'NONE',  ( 5.848290838822029158, 2.103586024953810085, 0.1047431163101186502 ) ) ;
#147252 = CARTESIAN_POINT ( 'NONE',  ( -5.713871673155502151, 8.753601821068331290, 1.199719254218452047 ) ) ;
#147254 = CARTESIAN_POINT ( 'NONE',  ( 6.092251258522619395, 1.023830597077223903, -1.799436568697235783 ) ) ;
#147255 = CARTESIAN_POINT ( 'NONE',  ( 6.494519276145969577, 7.535692896047149425, -1.199719254218446718 ) ) ;
#147256 = CARTESIAN_POINT ( 'NONE',  ( -6.575868197828002693, 7.630599971342813426, 1.199719254218450271 ) ) ;
#147257 = CARTESIAN_POINT ( 'NONE',  ( -1.551702917632625356, 8.754377144105260911, 2.473499015030076631 ) ) ;
#147258 = CARTESIAN_POINT ( 'NONE',  ( 5.976820969762068003, -1.425406409037911937, 1.431266451708369303 ) ) ;
#147259 = CARTESIAN_POINT ( 'NONE',  ( -0.7500000000000249800, -0.2770833326505156569, 1.299038105676659116 ) ) ;
#147260 = CARTESIAN_POINT ( 'NONE',  ( 4.319161277787673114, 2.108828969982502688, 0.9375607936791326980 ) ) ;
#147261 = CARTESIAN_POINT ( 'NONE',  ( 1.762625871119470000, -0.7384422231204194054, -1.926036706659232323 ) ) ;
#147262 = CARTESIAN_POINT ( 'NONE',  ( 6.968527767744093993, 10.11340424813470662, 1.082531754730558626 ) ) ;
#147263 = CARTESIAN_POINT ( 'NONE',  ( 7.178115983792402233, 7.339166500704784823, 0.7998128361456281477 ) ) ;
#147264 = CARTESIAN_POINT ( 'NONE',  ( 5.408776937209000657, 5.274937613024121674, 0.7998128361456352531 ) ) ;
#147265 = CARTESIAN_POINT ( 'NONE',  ( -1.364683531250014514, 0.8010416670080889867, -0.7879004041258289570 ) ) ;
#147266 = CARTESIAN_POINT ( 'NONE',  ( 2.878073747850912412, 6.579779482459851003, -0.7998128361456362523 ) ) ;
#147267 = CARTESIAN_POINT ( 'NONE',  ( 5.300874872818821082, 9.128178418356554857, 0.7216878364870438212 ) ) ;
#147268 = CARTESIAN_POINT ( 'NONE',  ( 3.754478802441584495, -2.168521383071635000, -0.1100146688530565936 ) ) ;
#147269 = CARTESIAN_POINT ( 'NONE',  ( -4.895902867866254837, 7.765618208269001066, 1.082531754730549967 ) ) ;
#147271 = CARTESIAN_POINT ( 'NONE',  ( 3.438839575862782549, -1.396446551253815782, -1.200180114512699792 ) ) ;
#147270 = CARTESIAN_POINT ( 'NONE',  ( -5.260200412422213923, 6.199617238323108737, -1.082531754730544860 ) ) ;
#147272 = EDGE_CURVE ( 'NONE', #93151, #118697, #103350, .T. ) ;
#147273 = CARTESIAN_POINT ( 'NONE',  ( -0.6823417656250212460, 4.301041667008085767, 1.181850606188767472 ) ) ;
#147274 = CARTESIAN_POINT ( 'NONE',  ( 5.987848539424092564, -2.180829346447300310, -0.2163489798085171945 ) ) ;
#147275 = CARTESIAN_POINT ( 'NONE',  ( 8.226144498209521316, 14.18988382969902418, 8.737432991257948700 ) ) ;
#147276 = CARTESIAN_POINT ( 'NONE',  ( 5.612299388031473768, -1.011774156007083869, -2.023756622241212000 ) ) ;
#147277 = CARTESIAN_POINT ( 'NONE',  ( -5.562564655730993124, 6.373022183664215135, -1.235959600235781330 ) ) ;
#147278 = CARTESIAN_POINT ( 'NONE',  ( 4.607021725950278146, 8.475092030744066918, 0.2235605714990263060 ) ) ;
#147279 = CARTESIAN_POINT ( 'NONE',  ( -6.116136693096208887, 6.308116694799912771, 0.7216878364870257245 ) ) ;
#147280 = CARTESIAN_POINT ( 'NONE',  ( 3.607878275012302627, 7.223292064240769861, 0.7216878364870257245 ) ) ;
#147281 =( BOUNDED_CURVE ( )  B_SPLINE_CURVE ( 2, ( #199614, #133610, #14463, #50190, #213717, #130453, #81615 ),
 .UNSPECIFIED., .F., .T. ) 
 B_SPLINE_CURVE_WITH_KNOTS ( ( 3, 2, 2, 3 ),
 ( 0.1428571428571429880, 0.1488095238095238637, 0.1547619047619047394, 0.1607142857142856152 ),
 .UNSPECIFIED. ) 
 CURVE ( )  GEOMETRIC_REPRESENTATION_ITEM ( )  RATIONAL_B_SPLINE_CURVE ( ( 0.9999999999999968914, 0.8660254037844418162, 1.000000000000000000, 0.8660254037844387076, 1.000000000000000000, 0.8660254037844412611, 0.9999999999999974465 ) ) 
 REPRESENTATION_ITEM ( '' )  );
#147282 = CARTESIAN_POINT ( 'NONE',  ( 6.063686852112752490, 1.743171776219472280, -0.3043750889455443254 ) ) ;
#147283 = CARTESIAN_POINT ( 'NONE',  ( 3.914701103513482661, -0.6334807629873323576, -1.910874176753782461 ) ) ;
#147284 = CARTESIAN_POINT ( 'NONE',  ( 6.421758314367153275, 10.64380180007036891, -0.7998128361456291469 ) ) ;
#147285 = CARTESIAN_POINT ( 'NONE',  ( 2.608543117039106463, -0.8048738574607334773, -1.946287526097515430 ) ) ;
#147286 = CARTESIAN_POINT ( 'NONE',  ( 1.915515091613760656, -1.252924113133683237, -1.449102840280371618 ) ) ;
#147287 = CARTESIAN_POINT ( 'NONE',  ( 3.161022370280501814, 6.839609865302569425, 0.000000000000000000 ) ) ;
#147288 = CARTESIAN_POINT ( 'NONE',  ( 3.719166427026363131, -1.735901824557140927, -0.9304994270666072653 ) ) ;
#147289 = CARTESIAN_POINT ( 'NONE',  ( 4.904559663377827228, -2.005024252762297898, -0.2429568683046164634 ) ) ;
#147290 = CARTESIAN_POINT ( 'NONE',  ( 0.9888773766892227091, 1.651582696977689890, -0.8784067438419729257 ) ) ;
#147291 = CARTESIAN_POINT ( 'NONE',  ( 1.099968687278202406, 0.7983322178258808188, -1.792280776234013828 ) ) ;
#147294 = EDGE_LOOP ( 'NONE', ( #82832, #64860, #138944 ) ) ;
#147293 = CARTESIAN_POINT ( 'NONE',  ( 0.5625819312903357350, 0.5574351770905332515, 1.829310545699929458 ) ) ;
#147292 = CARTESIAN_POINT ( 'NONE',  ( 3.474969472568560480, 0.04075424684168299505, -1.724569731432665121 ) ) ;
#147296 = CARTESIAN_POINT ( 'NONE',  ( 4.772106882330221289, 6.590544000850479200, -1.443375672974051449 ) ) ;
#147295 = CARTESIAN_POINT ( 'NONE',  ( 1.541937560865791479, -1.600244427420342896, -1.519961040588948986 ) ) ;
#147297 = CARTESIAN_POINT ( 'NONE',  ( -1.364683531250012516, 0.8427083336747532849, 0.7879004041258379498 ) ) ;
#147299 = CARTESIAN_POINT ( 'NONE',  ( 11.88156762547254175, 11.37999991545966516, 1.686557021358693786 ) ) ;
#147298 = CIRCLE ( 'NONE', #181891, 11.92000000000000171 ) ;
#147300 = CARTESIAN_POINT ( 'NONE',  ( 6.717278222822382183, -7.246166700180828535, -6.830415307812249814 ) ) ;
#147301 = ORIENTED_EDGE ( 'NONE', *, *, #147396, .T. ) ;
#147302 = CARTESIAN_POINT ( 'NONE',  ( 6.825056245572477032, -1.890314563506745316, -0.8446596084958692963 ) ) ;
#147303 = ADVANCED_FACE ( 'NONE', ( #51841 ), #180758, .T. ) ;
#147304 = CARTESIAN_POINT ( 'NONE',  ( 0.6782873735513493818, -1.106163567672680204, -1.749894625276714688 ) ) ;
#147305 = CARTESIAN_POINT ( 'NONE',  ( -1.402160292154681736E-14, 2.337500000000022560, -1.732050807568863648 ) ) ;
#147306 = CARTESIAN_POINT ( 'NONE',  ( 6.612626235163189925, 8.737816579155630592, -1.599625672291262513 ) ) ;
#147307 = CARTESIAN_POINT ( 'NONE',  ( -7.853197290813634268, 10.18514947741448573, 1.599625672291295375 ) ) ;
#147308 = CARTESIAN_POINT ( 'NONE',  ( 5.367048706163317640, 7.354919138647580290, -1.599625672291281386 ) ) ;
#147309 = CARTESIAN_POINT ( 'NONE',  ( 5.830757645730302308, 1.424217953154560012, -1.571192434731554677 ) ) ;
#147310 = CARTESIAN_POINT ( 'NONE',  ( 5.273195401072370281, 5.116759154198018855, -0.7998128361456481317 ) ) ;
#147311 = CARTESIAN_POINT ( 'NONE',  ( -1.201851678989727383E-14, 1.821875000341421691, 1.575800808251672791 ) ) ;
#147312 = VERTEX_POINT ( 'NONE', #113704 ) ;
#147313 = CARTESIAN_POINT ( 'NONE',  ( -1.499999999999997780, 2.650000000000020339, 1.214306433183764966E-14 ) ) ;
#147315 = CARTESIAN_POINT ( 'NONE',  ( 5.495132332240461714, 5.305409230568988832, 0.7998128361456341429 ) ) ;
#147314 = CARTESIAN_POINT ( 'NONE',  ( 6.320756440275016708, -1.388331291134708767, 1.386421665916007795 ) ) ;
#147316 = CARTESIAN_POINT ( 'NONE',  ( 4.499374939222855474, 1.976653413780619761, 0.3960398538903551757 ) ) ;
#147317 = CARTESIAN_POINT ( 'NONE',  ( 3.643669983026840420, 1.900603903897592595, -0.2398275428802750520 ) ) ;
#147318 = DIRECTION ( 'NONE',  ( 5.551115123125765446E-17, 0.000000000000000000, -1.000000000000000000 ) ) ;
#147319 = CARTESIAN_POINT ( 'NONE',  ( 1.154151856878969928, 0.8927059368322427524, 2.001694687108931170 ) ) ;
#147320 = DIRECTION ( 'NONE',  ( 1.000000000000000000, 0.000000000000000000, 0.000000000000000000 ) ) ;
#147321 = CARTESIAN_POINT ( 'NONE',  ( 3.620239363633662499, 1.188986022374241225, -1.444006105232335191 ) ) ;
#147322 = CARTESIAN_POINT ( 'NONE',  ( -1.402160292154681736E-14, -0.5062499993171791779, 1.732050807568877637 ) ) ;
#147323 = CARTESIAN_POINT ( 'NONE',  ( -6.718228810771495141, 7.796687353110217877, 1.199719254218450271 ) ) ;
#147325 = CARTESIAN_POINT ( 'NONE',  ( 5.167619242541076297, 1.422618751053092101, 1.568198848534626100 ) ) ;
#147324 = CARTESIAN_POINT ( 'NONE',  ( -5.124618876285560454, 5.081069565195661220, 0.7216878364870317197 ) ) ;
#147326 = CARTESIAN_POINT ( 'NONE',  ( -8.012344526598182026E-15, 8.859375000341405126, -1.575800808251669460 ) ) ;
#147328 = CARTESIAN_POINT ( 'NONE',  ( -7.282664789195997912, 8.525472337930658284, 1.199719254218452047 ) ) ;
#147327 = CARTESIAN_POINT ( 'NONE',  ( 2.472313036883976078, -2.001511166234470007, -0.6043430715973686640 ) ) ;
#147330 = ORIENTED_EDGE ( 'NONE', *, *, #127684, .F. ) ;
#147329 = CARTESIAN_POINT ( 'NONE',  ( 0.8149653058732795330, -0.2595981955949409614, 1.704996164590016683 ) ) ;
#147331 = CARTESIAN_POINT ( 'NONE',  ( 6.962275575817444384, 8.081408578997208991, -1.199719254218446718 ) ) ;
#147332 = CARTESIAN_POINT ( 'NONE',  ( 0.05647967004077469183, -9.990726209582318162, 9.579565160031989990 ) ) ;
#147333 = CARTESIAN_POINT ( 'NONE',  ( -6.937452841262722103, -7.242250812743806776, -6.937452841262681247 ) ) ;
#147335 = CARTESIAN_POINT ( 'NONE',  ( 7.904040366642678173, 12.16520482781775137, 0.7216878364870438212 ) ) ;
#147334 = CARTESIAN_POINT ( 'NONE',  ( 6.657217119509961201, 7.725507046638470321, -1.199719254218446718 ) ) ;
#147336 = DIRECTION ( 'NONE',  ( -1.000000000000000000, 0.000000000000000000, 0.000000000000000000 ) ) ;
#147338 = CARTESIAN_POINT ( 'NONE',  ( 1.277659230087615727, 1.784704083969153920, -0.3092532468622013475 ) ) ;
#147337 = CARTESIAN_POINT ( 'NONE',  ( 4.681308178468477799, 8.683552984847038303, 0.000000000000000000 ) ) ;
#147340 = CARTESIAN_POINT ( 'NONE',  ( -6.018930129462987999, 9.109503353427070849, 1.199719254218452047 ) ) ;
#147339 = VECTOR ( 'NONE', #29571, 1000.000000000000000 ) ;
#147341 = CARTESIAN_POINT ( 'NONE',  ( 4.385172619016207918, 7.203452924572514959, 1.199719254218462483 ) ) ;
#147342 = CARTESIAN_POINT ( 'NONE',  ( 6.710359684120930091, 6.793450817754725257, 0.7998128361456352531 ) ) ;
#147343 = CARTESIAN_POINT ( 'NONE',  ( 6.539320575229250032, 3.707580029678263944, 2.311356139567366963 ) ) ;
#147344 = CARTESIAN_POINT ( 'NONE',  ( 0.4019237886466847653, 9.073664549684629321, 1.499999999999997113 ) ) ;
#147345 = CARTESIAN_POINT ( 'NONE',  ( 4.018854549923576158, 7.569224129587659888, 0.3183394790292719545 ) ) ;
#147346 = CARTESIAN_POINT ( 'NONE',  ( 9.246297574839980271, 10.85006392781057905, 1.082531754730549967 ) ) ;
#147347 = EDGE_LOOP ( 'NONE', ( #115577, #149753, #135128, #89001 ) ) ;
#147348 = CARTESIAN_POINT ( 'NONE',  ( 2.840123846975282973, -0.9592540151425684725, 1.594648687322928859 ) ) ;
#147349 = CARTESIAN_POINT ( 'NONE',  ( 0.4740638213791115718, -1.901237768712552345, -0.2334040896743785343 ) ) ;
#147350 = CARTESIAN_POINT ( 'NONE',  ( 6.440456187458303283, 1.905530750978209120, 0.2820203164855574207 ) ) ;
#147351 = DIRECTION ( 'NONE',  ( 1.000000000000000000, 0.000000000000000000, -3.706092522800016599E-15 ) ) ;
#147352 =( GEOMETRIC_REPRESENTATION_CONTEXT ( 3 ) GLOBAL_UNCERTAINTY_ASSIGNED_CONTEXT ( ( #73620 ) ) GLOBAL_UNIT_ASSIGNED_CONTEXT ( ( #75431, #106921, #172945 ) ) REPRESENTATION_CONTEXT ( 'NONE', 'WORKASPACE' ) );
#147353 = CARTESIAN_POINT ( 'NONE',  ( 4.594471896879979589, 8.374412622790375238, -0.01639726577711345112 ) ) ;
#147354 = DIRECTION ( 'NONE',  ( 0.000000000000000000, -0.7996470168499917319, 0.6004703560067797818 ) ) ;
#147355 = CARTESIAN_POINT ( 'NONE',  ( -2.629918611371007575, 6.012062780000711371, 0.7216878364870317197 ) ) ;
#147356 = CARTESIAN_POINT ( 'NONE',  ( 8.676855123066012254, 11.14608361504227574, -1.443375672974052559 ) ) ;
#147357 = CARTESIAN_POINT ( 'NONE',  ( 4.944182365274345514, -0.9318649803399962073, 1.735062577953277563 ) ) ;
#147358 = CARTESIAN_POINT ( 'NONE',  ( 1.453939175038564624, -1.538220317728825393, -1.459821603020584613 ) ) ;
#147359 = CARTESIAN_POINT ( 'NONE',  ( -4.693093728624763372, 8.627026450037540428, 0.7998128361456481317 ) ) ;
#147360 = CARTESIAN_POINT ( 'NONE',  ( -4.622967192135580383, 5.456178481322002227, 1.082531754730558626 ) ) ;
#147361 = DIRECTION ( 'NONE',  ( 0.000000000000000000, 0.000000000000000000, 1.000000000000000000 ) ) ;
#147362 = AXIS2_PLACEMENT_3D ( 'NONE', #24356, #57948, #156533 ) ;
#147363 = CARTESIAN_POINT ( 'NONE',  ( 6.456982561897790518, 0.3786298020890948024, -2.158335565738931816 ) ) ;
#147364 = CARTESIAN_POINT ( 'NONE',  ( 0.000000000000000000, 0.2000000000000057288, 0.000000000000000000 ) ) ;
#147365 = CARTESIAN_POINT ( 'NONE',  ( 4.418917755230268085, 1.760988537516799068, 0.7813691060932350663 ) ) ;
#147366 = CARTESIAN_POINT ( 'NONE',  ( -5.831978632172702071, 9.955725504176825780, 0.7998128361456481317 ) ) ;
#147367 = CARTESIAN_POINT ( 'NONE',  ( 0.3932109892899987025, 1.349039491128176227, 1.230163767592551638 ) ) ;
#147368 = CARTESIAN_POINT ( 'NONE',  ( 0.6278963055918493907, -2.094311335337955882, 0.6960538111202837497 ) ) ;
#147369 = CARTESIAN_POINT ( 'NONE',  ( -3.895996091634230218, 7.334980739573080832, 0.5863762202383783206 ) ) ;
#147370 = CARTESIAN_POINT ( 'NONE',  ( -0.3313999689851416797, -9.006862915010142245, 9.494725171580526535 ) ) ;
#147371 = ORIENTED_EDGE ( 'NONE', *, *, #57965, .T. ) ;
#147372 = CARTESIAN_POINT ( 'NONE',  ( 3.104453987849314700, 4.644948957289396496, 0.000000000000000000 ) ) ;
#147373 = EDGE_LOOP ( 'NONE', ( #125343, #92216, #140486, #131307 ) ) ;
#147374 = CARTESIAN_POINT ( 'NONE',  ( 6.614111185624225620, 1.964402775464332507, -0.1412838390872969141 ) ) ;
#147375 = CARTESIAN_POINT ( 'NONE',  ( 0.9779546479521743496, -1.895077795344397575, -0.4239509559331255395 ) ) ;
#147376 = CARTESIAN_POINT ( 'NONE',  ( 6.714253291261501388, -1.839887274036870357, -1.377324995421406628 ) ) ;
#147378 = CARTESIAN_POINT ( 'NONE',  ( 5.629708122894265365, 1.793948666107824774, -0.4946651665681394139 ) ) ;
#147377 = CARTESIAN_POINT ( 'NONE',  ( -5.094831863685302942, 9.165997284266655498, 0.7998128361456291469 ) ) ;
#147379 = CARTESIAN_POINT ( 'NONE',  ( 4.712340909201580885, 7.655425606447271214, -1.199719254218452047 ) ) ;
#147380 = LINE ( 'NONE', #181977, #11226 ) ;
#147381 = CARTESIAN_POINT ( 'NONE',  ( 4.059495096955338056, 3.983312706056738595, -0.7638817160546188534 ) ) ;
#147382 = CARTESIAN_POINT ( 'NONE',  ( -7.230575994789712801, 7.330093503543126054, 0.7998128361456341429 ) ) ;
#147383 = CARTESIAN_POINT ( 'NONE',  ( -5.250750630242457362, 9.347902511916677426, 0.000000000000000000 ) ) ;
#147384 = CARTESIAN_POINT ( 'NONE',  ( 1.505704256594592838, -2.174480876681058827, 0.2726767719730335826 ) ) ;
#147385 = CARTESIAN_POINT ( 'NONE',  ( 5.829642864196171281, 5.903597551091405826, 0.7216878364870317197 ) ) ;
#147386 = CARTESIAN_POINT ( 'NONE',  ( 2.034713692888019843, 8.461455076002923903, 2.500000000000000444 ) ) ;
#147387 = CARTESIAN_POINT ( 'NONE',  ( 1.681982107312831154, -0.9779208310041755947, 1.541497997293653555 ) ) ;
#147388 = CARTESIAN_POINT ( 'NONE',  ( -3.972702704004144714, 4.593573561881607148, 1.199719254218462483 ) ) ;
#147389 = CARTESIAN_POINT ( 'NONE',  ( -0.2384352647906655132, 3.429829024941791094, -1.989178028829215350 ) ) ;
#147390 = CARTESIAN_POINT ( 'NONE',  ( 6.609000000000010644, 6.035875036286768136, 2.694900582964809388 ) ) ;
#147391 = CARTESIAN_POINT ( 'NONE',  ( 7.892817981449907982, 12.36003807833360391, 0.7998128361456462443 ) ) ;
#147392 = CARTESIAN_POINT ( 'NONE',  ( 0.1352084326644766299, -1.761967750658991028, 0.7794309377431463126 ) ) ;
#147393 = CARTESIAN_POINT ( 'NONE',  ( 4.012515129279304205, 0.7020173944642660313, 1.832041770129029468 ) ) ;
#147394 = CARTESIAN_POINT ( 'NONE',  ( -9.189729191964438826, 9.615772233580322848, 1.040834085586084257E-14 ) ) ;
#147395 = CARTESIAN_POINT ( 'NONE',  ( 5.126954644262057492, 9.133197518281081173, 0.7998128361456462443 ) ) ;
#147396 = EDGE_CURVE ( 'NONE', #91753, #145077, #133609, .T. ) ;
#147397 = CARTESIAN_POINT ( 'NONE',  ( 4.300438532332786501, 1.693616701070689956, -1.390861761948622766 ) ) ;
#147398 = B_SPLINE_CURVE_WITH_KNOTS ( 'NONE', 3,
 ( #67207, #84552, #150641, #3275, #68278, #200415 ),
 .UNSPECIFIED., .F., .F.,
 ( 4, 2, 4 ),
 ( 0.0006551727224218147332, 0.001090474818249038101, 0.001525776914076261252 ),
 .UNSPECIFIED. ) ;
#147399 = CARTESIAN_POINT ( 'NONE',  ( 4.822949958159289174, 6.649860922651057216, -1.599625672291256517 ) ) ;
#147400 = CARTESIAN_POINT ( 'NONE',  ( 3.151297481648129395, 1.777980080355131109, -1.060267355625019503 ) ) ;
#147402 = CARTESIAN_POINT ( 'NONE',  ( -0.6823417656250212460, 1.863541667008083991, 1.181850606188755259 ) ) ;
#147401 = CARTESIAN_POINT ( 'NONE',  ( -1.500000000000008216, 8.390625000341399797, 3.469446951953614189E-15 ) ) ;
#147403 = ORIENTED_EDGE ( 'NONE', *, *, #201684, .F. ) ;
#147404 = CARTESIAN_POINT ( 'NONE',  ( 4.518391418568163509, -2.101855750862766659, 0.9310765106353561249 ) ) ;
#147405 = CARTESIAN_POINT ( 'NONE',  ( 6.155038550924133212, 10.12470270947942730, 0.7216878364870438212 ) ) ;
#147407 = CARTESIAN_POINT ( 'NONE',  ( -5.450014563013541036, 5.460697866378312781, 0.7216878364870346063 ) ) ;
#147406 = CARTESIAN_POINT ( 'NONE',  ( 5.221298555038576872, 9.105615724271411082, 0.000000000000000000 ) ) ;
#147408 = CARTESIAN_POINT ( 'NONE',  ( 6.720655732516650716, 2.993363686233801779, 2.180545405541700177 ) ) ;
#147409 = CARTESIAN_POINT ( 'NONE',  ( -9.604686356149271020, 4.469090097702010489, -7.193747284969076894 ) ) ;
#147410 = CARTESIAN_POINT ( 'NONE',  ( 3.802622829840444751, 1.666041102563616816, 0.9975114776080131751 ) ) ;
#147411 = VERTEX_POINT ( 'NONE', #115822 ) ;
#147413 = EDGE_CURVE ( 'NONE', #143294, #175466, #113076, .T. ) ;
#147412 = CARTESIAN_POINT ( 'NONE',  ( 4.202664430556247055, 6.886563688082179446, 1.082531754730558626 ) ) ;
#147414 = CARTESIAN_POINT ( 'NONE',  ( 4.394721148579957770, -1.856311205515799312, -0.4593126252911489127 ) ) ;
#147415 = CARTESIAN_POINT ( 'NONE',  ( -3.096514578442687515, 6.188910745953249304, -0.7944190528704382359 ) ) ;
#147416 = CARTESIAN_POINT ( 'NONE',  ( 5.543893992536840010, 0.6953672157433439249, -1.578584939873737047 ) ) ;
#147417 = CARTESIAN_POINT ( 'NONE',  ( 5.032435514249763209, 0.5899841883351600869, 1.928258608204669766 ) ) ;
#147418 = CARTESIAN_POINT ( 'NONE',  ( 5.625696599388652963, 0.4453364752643809155, 2.255009244304376992 ) ) ;
#147419 = CARTESIAN_POINT ( 'NONE',  ( 3.985733972737593778, 6.633478153960411738, -1.082531754730548412 ) ) ;
#147420 = CARTESIAN_POINT ( 'NONE',  ( 0.2939702064862387276, 1.638257335637434364, 1.478849500172851217 ) ) ;
#147422 = CARTESIAN_POINT ( 'NONE',  ( -5.804299160426249493, 5.944306240018289778, -0.7216878364870338292 ) ) ;
#147421 = FACE_OUTER_BOUND ( 'NONE', #80999, .T. ) ;
#147423 = CARTESIAN_POINT ( 'NONE',  ( 6.257089712715798058, -1.519072588978742200, -0.9077291607378096261 ) ) ;
#147424 = MECHANICAL_DESIGN_GEOMETRIC_PRESENTATION_REPRESENTATION (  '', ( #140649 ), #12566 ) ;
#147426 = CARTESIAN_POINT ( 'NONE',  ( 1.394904949290655116, 1.871713452925367616, -1.323071089866036276 ) ) ;
#147425 = CARTESIAN_POINT ( 'NONE',  ( 6.387826650694035990, 7.481494509678370264, -1.199719254218452047 ) ) ;
#147427 = CARTESIAN_POINT ( 'NONE',  ( 1.569815774166925859, -1.651746245857487638, -0.5483857920917082351 ) ) ;
#147428 = CARTESIAN_POINT ( 'NONE',  ( 6.298795234281088895, 1.819837665574381091, 1.220625243075368127 ) ) ;
#147429 = CARTESIAN_POINT ( 'NONE',  ( 1.475528429365607019, 1.526226248090801318, 0.8227105958887138693 ) ) ;
#147430 = CARTESIAN_POINT ( 'NONE',  ( 1.360316468749957597, 0.3177083336747154596, -0.7853790794158961308 ) ) ;
#147431 = CARTESIAN_POINT ( 'NONE',  ( -11.48767021851170078, 12.26995772536156437, 3.470194894594595070 ) ) ;
#147432 = CARTESIAN_POINT ( 'NONE',  ( 1.451894146256039519, 1.643730891105445346, 1.418569794807096107 ) ) ;
#147433 = CARTESIAN_POINT ( 'NONE',  ( 2.184780103950241248, 1.616692242240840960, -1.205043568535242304 ) ) ;
#147434 = CARTESIAN_POINT ( 'NONE',  ( -1.402160292154681736E-14, -0.1312499993171854229, -1.732050807568870754 ) ) ;
#147435 = CARTESIAN_POINT ( 'NONE',  ( 5.725206259757900540, -0.04501307181254722567, 1.926136320475122288 ) ) ;
#147436 = CARTESIAN_POINT ( 'NONE',  ( -1.364683531250014514, 13.33854166700806587, -0.7879004041258335089 ) ) ;
#147437 = CARTESIAN_POINT ( 'NONE',  ( 2.830584216690882116, -1.098655552678593716, -1.930667878645520474 ) ) ;
#147438 = VERTEX_POINT ( 'NONE', #117960 ) ;
#147439 = CARTESIAN_POINT ( 'NONE',  ( 6.717748655460326290, -7.473374494057241080, 6.717748655458911422 ) ) ;
#147441 = EDGE_CURVE ( 'NONE', #174147, #106354, #183954, .T. ) ;
#147440 = CARTESIAN_POINT ( 'NONE',  ( 8.866142388332804103, 12.43125098877526113, -1.199719254218446718 ) ) ;
#147442 = CARTESIAN_POINT ( 'NONE',  ( 0.7499999999999920064, 5.264583334016151639, 1.299038105676669330 ) ) ;
#147443 = FILL_AREA_STYLE_COLOUR ( '', #114680 ) ;
#147444 = CARTESIAN_POINT ( 'NONE',  ( 5.337372294182569199, 0.6981903941610733133, -1.594458651668466898 ) ) ;
#147445 = CARTESIAN_POINT ( 'NONE',  ( 3.807043925254738781, -1.605251362286563177, 1.127602784832412386 ) ) ;
#147447 = CARTESIAN_POINT ( 'NONE',  ( -5.572037945536512105, 9.444535336527177805, 0.000000000000000000 ) ) ;
#147446 = CARTESIAN_POINT ( 'NONE',  ( 5.020596955762157698, 4.751784624677624080, 1.040834085586084257E-14 ) ) ;
#147448 = CARTESIAN_POINT ( 'NONE',  ( 5.575758015699216585, 5.849789923344298259, -0.7899890411014517388 ) ) ;
#147449 = CARTESIAN_POINT ( 'NONE',  ( 4.938899882951366394, 0.3800905753248150498, 2.230106783295758177 ) ) ;
#147450 = CIRCLE ( 'NONE', #161365, 11.18000000000000149 ) ;
#147451 = CARTESIAN_POINT ( 'NONE',  ( 1.188016131547619647, -1.306928873568227623, -1.595823035580832272 ) ) ;
#147452 = CARTESIAN_POINT ( 'NONE',  ( -8.016948904382338981, 8.247528564734524892, -0.7998128361456291469 ) ) ;
#147453 = CARTESIAN_POINT ( 'NONE',  ( -2.779058300676980675, 5.225689869889666106, -1.082531754730543083 ) ) ;
#147454 = AXIS2_PLACEMENT_3D ( 'NONE', #74131, #73038, #188935 ) ;
#147455 = CARTESIAN_POINT ( 'NONE',  ( 2.483610925836767791, 2.068663895631245531, -0.9166773448976636152 ) ) ;
#147456 = ORIENTED_EDGE ( 'NONE', *, *, #91508, .T. ) ;
#147458 = ADVANCED_FACE ( 'NONE', ( #17171 ), #164948, .T. ) ;
#147457 = CARTESIAN_POINT ( 'NONE',  ( -1.201851678989727383E-14, 1.243750000682821044, 1.732050807568877637 ) ) ;
#147459 = CARTESIAN_POINT ( 'NONE',  ( 2.899504437521780442, -0.5904213222340527478, 1.774967144274109287 ) ) ;
#147460 = CARTESIAN_POINT ( 'NONE',  ( 1.318582137269165733, 0.8549262331399180015, -1.508633131004229133 ) ) ;
#147461 = CARTESIAN_POINT ( 'NONE',  ( 5.882419586753742102, -0.3201050945752722532, -2.167950725039065052 ) ) ;
#147462 = CARTESIAN_POINT ( 'NONE',  ( 6.821333373144921275, -0.1693730316576994299, 2.270769535942236406 ) ) ;
#147463 = CARTESIAN_POINT ( 'NONE',  ( 4.346650381253648554, 0.5737703434565506466, 2.084106190491950006 ) ) ;
#147464 = CARTESIAN_POINT ( 'NONE',  ( 4.980387307702104138, -0.2395764092862572303, -1.927055426435628327 ) ) ;
#147465 = CARTESIAN_POINT ( 'NONE',  ( -10.66756793585402363, 11.33991743478486391, 0.7998128361456462443 ) ) ;
#147466 = EDGE_CURVE ( 'NONE', #160603, #172377, #33442, .T. ) ;
#147467 = LINE ( 'NONE', #196210, #157384 ) ;
#147468 = CARTESIAN_POINT ( 'NONE',  ( 0.6875000000000004441, -1.451031289061094132, 1.451031289061148755 ) ) ;
#147469 = CARTESIAN_POINT ( 'NONE',  ( 4.029290343944737174, 7.554674111305462070, -0.3786771240106376890 ) ) ;
#147470 = DIRECTION ( 'NONE',  ( -0.000000000000000000, -1.000000000000000000, -0.000000000000000000 ) ) ;
#147471 = CARTESIAN_POINT ( 'NONE',  ( 0.5263138230170816279, -3.232243495192089089, 3.254015791315836736 ) ) ;
#147472 = CARTESIAN_POINT ( 'NONE',  ( -3.094265954482842140, 2.800000000000024691, -2.490342512183689294 ) ) ;
#147473 = CARTESIAN_POINT ( 'NONE',  ( 5.221327349844218091, 1.987046161919112430, 0.3419379449052239450 ) ) ;
#147474 = CARTESIAN_POINT ( 'NONE',  ( -9.236128959407555072, 11.79856975744075598, -1.599625672291263179 ) ) ;
#147475 =( BOUNDED_CURVE ( )  B_SPLINE_CURVE ( 3, ( #137685, #24971, #72655, #203706 ),
 .UNSPECIFIED., .F., .T. ) 
 B_SPLINE_CURVE_WITH_KNOTS ( ( 4, 4 ),
 ( 1.570796326794821729, 2.479086375274792253 ),
 .UNSPECIFIED. ) 
 CURVE ( )  GEOMETRIC_REPRESENTATION_ITEM ( )  RATIONAL_B_SPLINE_CURVE ( ( 1.000000000000000000, 0.9324242863010213656, 0.9324242863010213656, 1.000000000000000000 ) ) 
 REPRESENTATION_ITEM ( '' )  );
#147476 = CARTESIAN_POINT ( 'NONE',  ( 8.281332899848809603, 8.555976559445431562, 0.7998128361456481317 ) ) ;
#147477 = CARTESIAN_POINT ( 'NONE',  ( 5.065906673361608270, 5.939254536123854677, -1.199719254218450271 ) ) ;
#147478 = CARTESIAN_POINT ( 'NONE',  ( 3.176193443437186126, -1.086901434622984830, 1.466744820640853098 ) ) ;
#147479 = CARTESIAN_POINT ( 'NONE',  ( 3.469446951953614189E-15, 5.167241622962441383, 1.214306433183764966E-14 ) ) ;
#147480 = ORIENTED_EDGE ( 'NONE', *, *, #88206, .F. ) ;
#147481 = CARTESIAN_POINT ( 'NONE',  ( -3.797692425159308716, 7.444741906078900406, 0.000000000000000000 ) ) ;
#147482 = CARTESIAN_POINT ( 'NONE',  ( -1.642778471875000035, -3.755208332855374476, -2.845375778867859751 ) ) ;
#147483 = CARTESIAN_POINT ( 'NONE',  ( -7.309817376062285099, 11.67987070538135264, 0.000000000000000000 ) ) ;
#147484 = CARTESIAN_POINT ( 'NONE',  ( 0.4221360882172753293, -2.009675015244154483, 0.2020994116621494530 ) ) ;
#147485 = CARTESIAN_POINT ( 'NONE',  ( 1.014494059972574691, -2.120667955011676487, 0.003750198165439199392 ) ) ;
#147486 = ORIENTED_EDGE ( 'NONE', *, *, #177138, .F. ) ;
#147487 = CARTESIAN_POINT ( 'NONE',  ( -4.288121723672178476, 8.224835454251337552, -0.7998128361456362523 ) ) ;
#147488 = CARTESIAN_POINT ( 'NONE',  ( 5.542585869888291938, 5.360771691158120689, -0.7998128361456211532 ) ) ;
#147489 = CARTESIAN_POINT ( 'NONE',  ( 6.280161615599199720, -1.104627599893250434, 1.739653883609869833 ) ) ;
#147490 = CARTESIAN_POINT ( 'NONE',  ( 5.344375030997434273, 0.3906003880304632636, -1.978050218768567792 ) ) ;
#147491 = ORIENTED_EDGE ( 'NONE', *, *, #146747, .F. ) ;
#147492 = CARTESIAN_POINT ( 'NONE',  ( -8.947491310014823895, 12.52615806407091803, 1.199719254218462483 ) ) ;
#147493 = CYLINDRICAL_SURFACE ( 'NONE', #175895, 1.250000000000000000 ) ;
#147494 = VECTOR ( 'NONE', #121561, 1000.000000000000000 ) ;
#147496 = DIRECTION ( 'NONE',  ( -1.224646799147353207E-16, 0.000000000000000000, -1.000000000000000000 ) ) ;
#147495 = CARTESIAN_POINT ( 'NONE',  ( -5.712781623311813384, 7.758274208654143855, -1.599625672291271394 ) ) ;
#147497 = CARTESIAN_POINT ( 'NONE',  ( 5.901825473515108555, 7.257632781371366804, 1.250113620240392631 ) ) ;
#147498 = CARTESIAN_POINT ( 'NONE',  ( 5.272814466252145671, -2.006652483137221665, 0.1948127969565379425 ) ) ;
#147499 = CARTESIAN_POINT ( 'NONE',  ( 4.980324010294663317, -0.2286266671043569454, -1.826820671449409295 ) ) ;
#147500 = CARTESIAN_POINT ( 'NONE',  ( -4.951779652976519230, 6.537757797665403992, 2.442612065051306125 ) ) ;
#147501 = CARTESIAN_POINT ( 'NONE',  ( 2.772455145383013519, 1.235390390761299306, 1.949004725048721243 ) ) ;
#147502 = CARTESIAN_POINT ( 'NONE',  ( 5.773793314573267388, 7.829454515125894964, 1.599625672291268286 ) ) ;
#147503 = CARTESIAN_POINT ( 'NONE',  ( 5.659502677682959337, 0.4278135246765999988, -2.118672983663777654 ) ) ;
#147504 = CARTESIAN_POINT ( 'NONE',  ( 6.771407655021410399, 9.987393799911945536, -1.199719254218441611 ) ) ;
#147505 = CARTESIAN_POINT ( 'NONE',  ( 1.118581540066618141, -0.04615595083166770807, 1.941663063996822869 ) ) ;
#147506 = CARTESIAN_POINT ( 'NONE',  ( -3.086452525405351643, 6.752611712948207057, 0.7998128361456341429 ) ) ;
#147507 = ORIENTED_EDGE ( 'NONE', *, *, #381, .F. ) ;
#147508 = PRESENTATION_LAYER_ASSIGNMENT (  '', '', ( #57967 ) ) ;
#147509 = CARTESIAN_POINT ( 'NONE',  ( 5.026898302747025760, 2.274369689431681163, -0.3307130315356506256 ) ) ;
#147510 = CARTESIAN_POINT ( 'NONE',  ( 0.000000000000000000, 8.999999999999998224, 0.000000000000000000 ) ) ;
#147511 = CARTESIAN_POINT ( 'NONE',  ( -4.899292406491858820, 6.809203455697518947, -1.599625672291271394 ) ) ;
#147512 = CARTESIAN_POINT ( 'NONE',  ( 3.766346201128992988, -1.256895078192099335, 1.385637336983977397 ) ) ;
#147515 = CARTESIAN_POINT ( 'NONE',  ( -5.261446130555064826, 8.296048364692991228, 1.199719254218452935 ) ) ;
#147514 = CARTESIAN_POINT ( 'NONE',  ( 1.499999999999987121, 0.5354166673494816786, 0.8660254037844524744 ) ) ;
#147513 = CARTESIAN_POINT ( 'NONE',  ( 1.248149539447914735, 0.9399939672071171426, -1.665319807275446706 ) ) ;
#147516 = CARTESIAN_POINT ( 'NONE',  ( 2.860232119962682784, 2.196193069775736362, -0.2169517147150926140 ) ) ;
#147517 = CARTESIAN_POINT ( 'NONE',  ( 6.983263157960340806, 6.037546352565132501, 2.441087094350186337 ) ) ;
#147518 = CARTESIAN_POINT ( 'NONE',  ( -3.707465945607718805, 7.355851012256872323, 0.5743249234583160945 ) ) ;
#147519 = CARTESIAN_POINT ( 'NONE',  ( 5.180624093753221970, 9.058162186105164437, 0.000000000000000000 ) ) ;
#147520 = CARTESIAN_POINT ( 'NONE',  ( -3.327636637150278798, 5.969660945728899826, -1.199719254218452935 ) ) ;
#147521 = CIRCLE ( 'NONE', #192477, 0.08000000000000020983 ) ;
#147522 = CARTESIAN_POINT ( 'NONE',  ( 0.8957027828950543391, -0.7134963830764933235, 1.837871659531468804 ) ) ;
#147523 = CARTESIAN_POINT ( 'NONE',  ( 1.448709080243043124, 2.305037702096077723, 0.1111474144101440020 ) ) ;
#147524 = CARTESIAN_POINT ( 'NONE',  ( 1.785527960060459440, -1.848404783191982315, 0.6579185095809261252 ) ) ;
#147525 = CARTESIAN_POINT ( 'NONE',  ( 5.682507089483013196, 1.232960659210121879, -1.653321649057968967 ) ) ;
#147526 = CARTESIAN_POINT ( 'NONE',  ( 4.772106882330221289, 6.590544000850479200, -1.443375672974051449 ) ) ;
#147527 = CARTESIAN_POINT ( 'NONE',  ( 6.540882763950133238, 6.595727744222092959, 0.000000000000000000 ) ) ;
#147528 = EDGE_LOOP ( 'NONE', ( #169985, #100709, #90068, #118523, #17325, #92474 ) ) ;
#147529 = CARTESIAN_POINT ( 'NONE',  ( 1.364683531249990311, 5.176041667008085767, 0.7879004041258500513 ) ) ;
#147530 = CARTESIAN_POINT ( 'NONE',  ( 10.86205067566995552, -6.804704122739854810, -0.3107038660269284547 ) ) ;
#147531 = CARTESIAN_POINT ( 'NONE',  ( 3.619663824724254741, 6.206396314611513532, -1.082531754730543971 ) ) ;
#147532 = CARTESIAN_POINT ( 'NONE',  ( 1.393694035345336424, -1.963709693186867833, 0.9261614696171887040 ) ) ;
#147534 = CARTESIAN_POINT ( 'NONE',  ( 5.864778394761136049, 0.1288883805774850844, -1.836796581567698539 ) ) ;
#147533 = CARTESIAN_POINT ( 'NONE',  ( -1.786647479811285890E-05, -9.954793286625749360, -11.00029511060593634 ) ) ;
#147535 = EDGE_CURVE ( 'NONE', #29314, #23394, #165496, .T. ) ;
#147536 = CARTESIAN_POINT ( 'NONE',  ( 11.55950211276791428, 11.37999999999999901, -3.221476510067115662 ) ) ;
#147537 = DIRECTION ( 'NONE',  ( 1.000000000000000000, -0.000000000000000000, -0.000000000000000000 ) ) ;
#147538 = CARTESIAN_POINT ( 'NONE',  ( 1.247088714334358750, -1.471066981041386335, -1.155250539242147045 ) ) ;
#147539 = CARTESIAN_POINT ( 'NONE',  ( 5.923154835166896781, -0.05960684409221649049, 2.160954015416292506 ) ) ;
#147540 = CARTESIAN_POINT ( 'NONE',  ( -6.118227108790639690, 6.008232112836603633, 0.2598000991895776934 ) ) ;
#147541 = CARTESIAN_POINT ( 'NONE',  ( -0.02264175331117417728, 0.7142767504201595896, -2.172799776233569791 ) ) ;
#147542 = CARTESIAN_POINT ( 'NONE',  ( -1.364683531250014514, -0.7614583329919104582, -0.7879004041258359514 ) ) ;
#147543 = CARTESIAN_POINT ( 'NONE',  ( 2.332540574144434053, 1.247770424613745543, -1.449200414897835909 ) ) ;
#147544 = CARTESIAN_POINT ( 'NONE',  ( 3.344378923012015115, 0.4290688666262321149, 1.716912437317794415 ) ) ;
#147545 = CARTESIAN_POINT ( 'NONE',  ( 0.4867802866235851345, -1.800715477623024086, -0.6440170976053718466 ) ) ;
#147547 = CARTESIAN_POINT ( 'NONE',  ( 5.554270809058080793, -1.211575977211576172, 1.483806794280813302 ) ) ;
#147546 = CARTESIAN_POINT ( 'NONE',  ( 7.667935170093241659, -6.766388843766955929, 7.887197531381555216 ) ) ;
#147548 = CARTESIAN_POINT ( 'NONE',  ( 6.215292997425397203, -1.688482396400727170, -1.013753615619580106 ) ) ;
#147549 = CARTESIAN_POINT ( 'NONE',  ( -1.499999999999997780, 4.650000000000022560, 1.214306433183764966E-14 ) ) ;
#147550 = CARTESIAN_POINT ( 'NONE',  ( 0.9672155168029163974, -1.668165459610539081, 1.309123814877902969 ) ) ;
#147551 = CARTESIAN_POINT ( 'NONE',  ( 0.03889815725003424596, -8.115420858948564131, -10.94377971103912195 ) ) ;
#147552 = CARTESIAN_POINT ( 'NONE',  ( 4.698043743269282757, -1.870269067358639958, -0.04562963166049315705 ) ) ;
#147554 = VERTEX_POINT ( 'NONE', #48643 ) ;
#147553 = CARTESIAN_POINT ( 'NONE',  ( 0.1877650043593872553, -0.8638833939697135866, 1.608357707688967242 ) ) ;
#147556 = CARTESIAN_POINT ( 'NONE',  ( 9.886825906824942223, 3.934660213246443661, 6.000867881395502756 ) ) ;
#147555 = CARTESIAN_POINT ( 'NONE',  ( 4.653060005753134831, -1.773635849817876586, 1.313014255023836618 ) ) ;
#147557 = CARTESIAN_POINT ( 'NONE',  ( -1.364683531249997417, 5.071875000341417916, 1.214306433183764966E-14 ) ) ;
#147558 = CARTESIAN_POINT ( 'NONE',  ( 1.855998075696059901, -0.6969055236651957586, 1.941492863836144611 ) ) ;
#147559 = CARTESIAN_POINT ( 'NONE',  ( 5.961834861707224320, 7.978559976790334574, -1.599625672291262513 ) ) ;
#147560 = CARTESIAN_POINT ( 'NONE',  ( -7.771848369131641121, 10.09024240211882351, -1.599625672291263179 ) ) ;
#147561 =( NAMED_UNIT ( * ) SI_UNIT ( $, .STERADIAN. ) SOLID_ANGLE_UNIT ( ) );
#147562 = CARTESIAN_POINT ( 'NONE',  ( -3.473320263822863740, -0.001938837310419191983, -0.06665759106987857729 ) ) ;
#147563 = CARTESIAN_POINT ( 'NONE',  ( 6.373214726875630731, 9.593111727067046957, 1.199719254218452047 ) ) ;
#147564 = VERTEX_POINT ( 'NONE', #83245 ) ;
#147565 = CARTESIAN_POINT ( 'NONE',  ( 4.053231837324381637, 1.750648263899981849, -1.104974720517466480 ) ) ;
#147566 = CARTESIAN_POINT ( 'NONE',  ( -1.001543065824772872E-14, 5.462500000000020783, 1.732050807568877637 ) ) ;
#147567 = CARTESIAN_POINT ( 'NONE',  ( 1.757319832705085627, -1.853012815387704570, -1.112828241397870066 ) ) ;
#147568 = CARTESIAN_POINT ( 'NONE',  ( -5.178050853460543834, 7.761234873892349562, -1.181743852105126669 ) ) ;
#147569 = CARTESIAN_POINT ( 'NONE',  ( 2.104171369714701534, -0.8614446868937111201, 1.826873676003283320 ) ) ;
#147570 = CARTESIAN_POINT ( 'NONE',  ( 0.3866937364864087567, 3.956598013261175772, -11.53692321988872926 ) ) ;
#147571 = PRODUCT_DEFINITION_SHAPE ( 'NONE', 'NONE',  #214419 ) ;
#147572 = ORIENTED_EDGE ( 'NONE', *, *, #20726, .F. ) ;
#147573 = EDGE_CURVE ( 'NONE', #175232, #89693, #167719, .T. ) ;
#147575 = CARTESIAN_POINT ( 'NONE',  ( 7.239690840017413365, 10.42976116578691403, -1.082531754730537976 ) ) ;
#147574 = CARTESIAN_POINT ( 'NONE',  ( -1.737500000000000266, -2.508333333333334636, -3.009438278150923907 ) ) ;
#147576 = CARTESIAN_POINT ( 'NONE',  ( 0.2726351642629436522, -5.197079954928608636, 10.99683038201373719 ) ) ;
#147577 = CARTESIAN_POINT ( 'NONE',  ( 0.3742329010679063539, -2.001858617179689492, -0.2420261300371470137 ) ) ;
#147578 = CARTESIAN_POINT ( 'NONE',  ( 5.319949580897746166, 1.306013235697962571, -1.759773446019400778 ) ) ;
#147580 = STYLED_ITEM ( 'NONE', ( #207237 ), #16748 ) ;
#147579 = CARTESIAN_POINT ( 'NONE',  ( 0.7499999999999902300, 4.347916667349481123, -1.299038105676658228 ) ) ;
#147581 = CARTESIAN_POINT ( 'NONE',  ( 4.060738401289211374, 0.5150538496448524572, 1.841637258418599155 ) ) ;
#147582 = CARTESIAN_POINT ( 'NONE',  ( -3.741160322367112379, 6.452105245148518797, 1.199719254218464037 ) ) ;
#147583 = CARTESIAN_POINT ( 'NONE',  ( 6.331294547457450683, 7.449227062530913379, -1.082531754730543083 ) ) ;
#147585 = CARTESIAN_POINT ( 'NONE',  ( 1.968375273883906429, -1.978056371059619511, -0.3905749819678172585 ) ) ;
#147584 = CARTESIAN_POINT ( 'NONE',  ( 0.3999999999999576672, 3.949999999999981526, 0.8338124244295311849 ) ) ;
#147586 = CARTESIAN_POINT ( 'NONE',  ( 1.364683531249996529, 13.02604166700806410, 0.7879004041258405033 ) ) ;
#147588 = CARTESIAN_POINT ( 'NONE',  ( -3.817502770699643388, 6.611447778194983194, 1.199719254218452935 ) ) ;
#147587 = CARTESIAN_POINT ( 'NONE',  ( 0.04695162158900589161, -1.836028162657590501, 1.372410674757597704 ) ) ;
#147589 = CARTESIAN_POINT ( 'NONE',  ( 4.682452625960944026, -1.673401091975829091, -0.4171936932430859168 ) ) ;
#147590 = CARTESIAN_POINT ( 'NONE',  ( 8.039058738260216330, 8.343599714250547805, -0.7998128361456341429 ) ) ;
#147591 = CARTESIAN_POINT ( 'NONE',  ( 4.857899112398166075, 4.561970474086296079, 1.040834085586084257E-14 ) ) ;
#147592 = CARTESIAN_POINT ( 'NONE',  ( -9.348561386899502779, 3.999985931113709814, -7.001914024221965960 ) ) ;
#147593 = CARTESIAN_POINT ( 'NONE',  ( 0.07516593201273635838, 0.2333279341363985182, -2.077802470623245856 ) ) ;
#147594 = ORIENTED_EDGE ( 'NONE', *, *, #95387, .F. ) ;
#147595 = ORIENTED_EDGE ( 'NONE', *, *, #164073, .T. ) ;
#147596 = CARTESIAN_POINT ( 'NONE',  ( 5.567019150587803722, -1.423986762948417972, 1.119560556780722083 ) ) ;
#147597 = ORIENTED_EDGE ( 'NONE', *, *, #64524, .T. ) ;
#147598 = CARTESIAN_POINT ( 'NONE',  ( 8.809047120577066181, 11.30030761213851953, 1.599625672291281386 ) ) ;
#147599 = CARTESIAN_POINT ( 'NONE',  ( 5.890091390494168522, 5.836471141856793388, 0.000000000000000000 ) ) ;
#147600 = DIRECTION ( 'NONE',  ( 0.000000000000000000, 1.000000000000000000, 0.000000000000000000 ) ) ;
#147601 = CARTESIAN_POINT ( 'NONE',  ( 5.988875474321468495, -1.722281623382706073, -0.5616633497566495548 ) ) ;
#147602 = CARTESIAN_POINT ( 'NONE',  ( 7.160114521348466710, 7.526090827760914870, 0.000000000000000000 ) ) ;
#147603 = CARTESIAN_POINT ( 'NONE',  ( -11.80251051724186695, 9.799999999999998934, -1.695257889419022890 ) ) ;
#147604 = CARTESIAN_POINT ( 'NONE',  ( 3.293114190187882429, 1.727671002657789057, 1.348082825637614279 ) ) ;
#147605 = EDGE_CURVE ( 'NONE', #24517, #18401, #8048, .T. ) ;
#147606 = AXIS2_PLACEMENT_3D ( 'NONE', #93122, #205768, #189525 ) ;
#147608 = CARTESIAN_POINT ( 'NONE',  ( 9.399880572976245574, 9.860948844760784482, 0.7998128361456462443 ) ) ;
#147607 = CARTESIAN_POINT ( 'NONE',  ( 6.619592957969418379, 0.3166511089685022928, -1.833750044983559535 ) ) ;
#147609 = CARTESIAN_POINT ( 'NONE',  ( 3.444859266486454352, -1.690994526066817105, -0.8999980677824627184 ) ) ;
#147610 = CARTESIAN_POINT ( 'NONE',  ( 1.500000000000039524, 7.064371086078061523, 10.89416074946469770 ) ) ;
#147611 = CIRCLE ( 'NONE', #16136, 8.300000000000000711 ) ;
#147612 = FILL_AREA_STYLE ('',( #111976 ) ) ;
#147613 = CARTESIAN_POINT ( 'NONE',  ( -1.364683531250014514, -0.2614583329919080157, -0.7879004041258359514 ) ) ;
#147614 = CARTESIAN_POINT ( 'NONE',  ( 6.019457014787495730, 6.125047393447951016, -0.7216878364870257245 ) ) ;
#147616 = CARTESIAN_POINT ( 'NONE',  ( 5.278551870535488355, -0.5171574069430958653, -2.053072726559619365 ) ) ;
#147615 = CARTESIAN_POINT ( 'NONE',  ( -3.735435015764967837, 4.316761258935923884, -1.199719254218452047 ) ) ;
#147617 = CARTESIAN_POINT ( 'NONE',  ( 0.9190830904215806507, 1.997680973563022766, 0.8264451868333838602 ) ) ;
#147618 = CARTESIAN_POINT ( 'NONE',  ( -3.935609729716867289, 7.813571461303467913, 0.7998128361456352531 ) ) ;
#147619 = CARTESIAN_POINT ( 'NONE',  ( 5.415556014015861841, 5.282846535965431300, -0.7998128361456481317 ) ) ;
#147620 = CARTESIAN_POINT ( 'NONE',  ( 1.131563826228650038, -1.154680578942975044, -1.414029504508321100 ) ) ;
#147621 = CARTESIAN_POINT ( 'NONE',  ( -5.251085567194491155, 5.020688004682002159, -0.7998128361456221525 ) ) ;
#147622 = CARTESIAN_POINT ( 'NONE',  ( 3.276193339942961913, -1.088440757138483539, 1.465454812695582865 ) ) ;
#147623 = CARTESIAN_POINT ( 'NONE',  ( 8.431556522904017470, 12.79655328865047892, 8.481395780940484741 ) ) ;
#147624 = CARTESIAN_POINT ( 'NONE',  ( 2.777492966359981441, 0.2764497561681695803, -1.892163382976944419 ) ) ;
#147625 = VERTEX_POINT ( 'NONE', #101645 ) ;
#147626 = CARTESIAN_POINT ( 'NONE',  ( 2.910559396907284047, 0.6610699718948702674, 1.855445417178583911 ) ) ;
#147627 = ORIENTED_EDGE ( 'NONE', *, *, #112518, .T. ) ;
#147628 = CARTESIAN_POINT ( 'NONE',  ( 4.563973399113295137, -1.265747467430546225, 1.473022616845516053 ) ) ;
#147629 = CARTESIAN_POINT ( 'NONE',  ( -6.237633190739009237, 9.434933268240943249, 1.199719254218452047 ) ) ;
#147631 = CARTESIAN_POINT ( 'NONE',  ( 5.326475955075804514, -0.9554483686352827077, -1.893264085526874974 ) ) ;
#147630 = CARTESIAN_POINT ( 'NONE',  ( 7.530627977747744062, 7.750430493652658015, -0.7998128361456341429 ) ) ;
#147632 = CARTESIAN_POINT ( 'NONE',  ( 0.003376046620557637129, -7.161464053357565973, 9.586610838029432813 ) ) ;
#147633 = CARTESIAN_POINT ( 'NONE',  ( 2.842330330863319876, 1.060513762474508015, -1.591057744338888913 ) ) ;
#147634 = CARTESIAN_POINT ( 'NONE',  ( 4.877963630130927264, 6.902327454639943127, -1.420620101560632342 ) ) ;
#147635 = CARTESIAN_POINT ( 'NONE',  ( -2.279673327430177476, 5.603443282069742182, 1.040551764627347231E-14 ) ) ;
#147636 = CARTESIAN_POINT ( 'NONE',  ( 3.393283585170187688, 7.180857625999046867, 0.7998128361456271485 ) ) ;
#147637 = CARTESIAN_POINT ( 'NONE',  ( 4.442045433088864570, -1.240138855636420567, -1.585653348822992026 ) ) ;
#147638 = CARTESIAN_POINT ( 'NONE',  ( -6.007394966791244961, 6.077829431809393945, -0.6506939885215150543 ) ) ;
#147639 = CARTESIAN_POINT ( 'NONE',  ( 4.951681858558426796, 0.5695450498939165218, -1.734646904759745700 ) ) ;
#147640 = CARTESIAN_POINT ( 'NONE',  ( 0.8189040078958352842, -1.500748464528355974, 1.426492703164506937 ) ) ;
#147641 = CARTESIAN_POINT ( 'NONE',  ( -7.863365906246054138, 11.15738207638699464, -1.082531754730543971 ) ) ;
#147642 = CIRCLE ( 'NONE', #64603, 0.08000000000000020983 ) ;
#147643 = CARTESIAN_POINT ( 'NONE',  ( -6.546709703855362328, 6.802806841334552601, 0.4695730141109008549 ) ) ;
#147644 = CARTESIAN_POINT ( 'NONE',  ( -0.4000000000000338840, 3.949999999999977973, -0.8338124244295983534 ) ) ;
#147645 = CARTESIAN_POINT ( 'NONE',  ( 6.192256348250350761, -1.861847689568534081, -0.1814220289034565448 ) ) ;
#147646 = CARTESIAN_POINT ( 'NONE',  ( 5.777746017718023097, 9.892454120646377191, 0.7998128361456462443 ) ) ;
#147647 = CARTESIAN_POINT ( 'NONE',  ( -4.412288926243578935, 7.235088616337731260, 1.199719254218464037 ) ) ;
#147648 = EDGE_CURVE ( 'NONE', #118044, #12777, #92326, .T. ) ;
#147649 = CIRCLE ( 'NONE', #158011, 6.399999999999999467 ) ;
#147650 = CARTESIAN_POINT ( 'NONE',  ( 2.544126380858701797, 6.119897877643793116, 0.7998128361456462443 ) ) ;
#147651 = CARTESIAN_POINT ( 'NONE',  ( -1.402160292154681736E-14, 10.73437500034139802, 1.575800808251682339 ) ) ;
#147652 = CARTESIAN_POINT ( 'NONE',  ( -5.925076824372040640, 6.871343368977510302, 1.199719254218450271 ) ) ;
#147654 = CARTESIAN_POINT ( 'NONE',  ( -3.485854892044998543, 6.120562236477518070, -1.082531754730546636 ) ) ;
#147653 = CARTESIAN_POINT ( 'NONE',  ( 4.857899112398166075, 4.561970474086296079, 1.040834085586084257E-14 ) ) ;
#147655 = CARTESIAN_POINT ( 'NONE',  ( -3.919715807682309094, 6.626733304721049933, 1.082531754730549967 ) ) ;
#147656 = CARTESIAN_POINT ( 'NONE',  ( -6.728924311084075960, 6.744833205886536120, 1.040834085586084257E-14 ) ) ;
#147657 = CARTESIAN_POINT ( 'NONE',  ( 0.9716355300813659390, -0.3074278181635254348, 2.047203142020392441 ) ) ;
#147658 = CARTESIAN_POINT ( 'NONE',  ( 2.566138216211190759, -1.085845923642224209, 1.817437617555809792 ) ) ;
#147659 = CARTESIAN_POINT ( 'NONE',  ( 7.889955328148847258, 11.29236608522730911, -1.199719254218446718 ) ) ;
#147660 = DIRECTION ( 'NONE',  ( -1.000000000000000000, 5.459311322609750190E-16, 0.000000000000000000 ) ) ;
#147661 = CARTESIAN_POINT ( 'NONE',  ( 0.3737962156708526384, -1.932529848913757897, 0.3785758322861746406 ) ) ;
#147662 = CARTESIAN_POINT ( 'NONE',  ( 4.626555186793138930, 7.126393038833472637, 1.348983236782254957 ) ) ;
#147663 = CARTESIAN_POINT ( 'NONE',  ( 4.284013352238246419, 6.021101549076499637, -1.443375672974051449 ) ) ;
#147665 = DIRECTION ( 'NONE',  ( 0.000000000000000000, 0.000000000000000000, 1.000000000000000000 ) ) ;
#147664 = CARTESIAN_POINT ( 'NONE',  ( -4.688878646772413283, 4.892074522590037056, 0.6607662533205791444 ) ) ;
#147666 = CARTESIAN_POINT ( 'NONE',  ( 2.484683925703546237, -0.3935552064166462083, -2.258081804418234473 ) ) ;
#147667 = CARTESIAN_POINT ( 'NONE',  ( 0.6124999999999707345, 0.4166666666666901664, -1.060881119635969094 ) ) ;
#147668 = CARTESIAN_POINT ( 'NONE',  ( 2.566550162062298579, 0.6480892470011965223, 1.799338185917313870 ) ) ;
#147669 = VERTEX_POINT ( 'NONE', #50758 ) ;
#147671 = EDGE_CURVE ( 'NONE', #124, #141526, #154449, .T. ) ;
#147670 = CARTESIAN_POINT ( 'NONE',  ( 8.419250203962011625, 8.924806114151579095, -0.7216878364870267237 ) ) ;
#147672 = CARTESIAN_POINT ( 'NONE',  ( 0.2639318008525155523, 0.6274397771241714272, -1.913028341257965170 ) ) ;
#147673 = CARTESIAN_POINT ( 'NONE',  ( 1.358172466202983042, -1.961936380284023063, -0.005482119489134959674 ) ) ;
#147674 = CARTESIAN_POINT ( 'NONE',  ( -9.592557376868645846, 11.15007068022363157, -1.199719254218441611 ) ) ;
#147675 = CARTESIAN_POINT ( 'NONE',  ( -6.256197817702116026, 9.386315656372753224, -1.199719254218440723 ) ) ;
#147676 = CARTESIAN_POINT ( 'NONE',  ( -3.904385050611244079, 7.498940292447679568, 1.040834085586084257E-14 ) ) ;
#147678 = CARTESIAN_POINT ( 'NONE',  ( 2.904884094325186350, 1.494127413938572069, 0.9483235522904243098 ) ) ;
#147677 = CARTESIAN_POINT ( 'NONE',  ( 3.345728622622257564, 2.090823719190892049, -0.0003901280219448939298 ) ) ;
#147679 = DIRECTION ( 'NONE',  ( 1.276756478318932585E-15, -1.000000000000000000, 1.665334536937738262E-16 ) ) ;
#147681 = CARTESIAN_POINT ( 'NONE',  ( 5.191491443341288203, -0.8287821522852161227, 2.137368679509048963 ) ) ;
#147680 = CARTESIAN_POINT ( 'NONE',  ( -11.57263578245408908, 7.021380543846468036, 3.181795205153499673 ) ) ;
#147682 = CARTESIAN_POINT ( 'NONE',  ( 4.734162553523208139, 0.3016713478377709423, 1.713805963711847680 ) ) ;
#147683 = CARTESIAN_POINT ( 'NONE',  ( 10.07778825365955733, 10.65184113889131012, -0.7998128361456281477 ) ) ;
#147684 = SURFACE_STYLE_FILL_AREA ( #192133 ) ;
#147685 = CARTESIAN_POINT ( 'NONE',  ( 3.901445378353602944, 0.2529189268129055090, 1.715120161964154510 ) ) ;
#147686 = CARTESIAN_POINT ( 'NONE',  ( 4.211506895594858690, -1.802957179857124448, -1.209418758558492568 ) ) ;
#147687 = CARTESIAN_POINT ( 'NONE',  ( 2.835626683552519012, 6.459981564119914310, 0.000000000000000000 ) ) ;
#147688 = CARTESIAN_POINT ( 'NONE',  ( 5.876185452347599814, -2.007255679753978228, -0.1928398672442974138 ) ) ;
#147689 = CARTESIAN_POINT ( 'NONE',  ( 0.000000000000000000, 0.000000000000000000, -1.999999999999999556 ) ) ;
#147690 = CARTESIAN_POINT ( 'NONE',  ( -1.500000000000013101, 3.910416667349482012, -0.8660254037844313801 ) ) ;
#147691 = CARTESIAN_POINT ( 'NONE',  ( 3.539987092570716865, 0.8674169631235107980, -1.720131978839019693 ) ) ;
#147692 = CARTESIAN_POINT ( 'NONE',  ( -0.7500000000000179856, 10.07291666734946922, 1.299038105676658228 ) ) ;
#147693 = CARTESIAN_POINT ( 'NONE',  ( 5.783471039277606529, 0.1639875503032099946, -2.215378355603670357 ) ) ;
#147694 = ORIENTED_EDGE ( 'NONE', *, *, #3410, .F. ) ;
#147695 = CARTESIAN_POINT ( 'NONE',  ( 6.883263157960407774, 1.288564682660230831, 1.962666442651111565 ) ) ;
#147696 = CARTESIAN_POINT ( 'NONE',  ( 0.7499999999999885647, 2.816666666666689522, -1.299038105676658228 ) ) ;
#147697 = CARTESIAN_POINT ( 'NONE',  ( 4.961394147597008697, 7.875711374583454827, -1.199719254218452047 ) ) ;
#147698 = CARTESIAN_POINT ( 'NONE',  ( 1.682608811002960447, 1.145563986048125704, 1.903002289297763605 ) ) ;
#147699 = CARTESIAN_POINT ( 'NONE',  ( 6.672321430365630412, -0.9237476215336395402, -1.730755693189582667 ) ) ;
#147700 = CARTESIAN_POINT ( 'NONE',  ( 8.270110514656037637, 8.750809809961280550, 0.7216878364870458196 ) ) ;
#147701 = CARTESIAN_POINT ( 'NONE',  ( -8.609064354553318310, 12.98773281371349775, 0.7216878364870317197 ) ) ;
#147702 = CARTESIAN_POINT ( 'NONE',  ( 3.553118775233146120, 6.302999783484076524, -1.199719254218453823 ) ) ;
#147703 = CARTESIAN_POINT ( 'NONE',  ( -3.350273356352693188, 6.922752992471175482, 0.000000000000000000 ) ) ;
#147705 = CARTESIAN_POINT ( 'NONE',  ( 4.809062498722087575, -1.658680843151142392, 1.225972815312638353 ) ) ;
#147704 = CARTESIAN_POINT ( 'NONE',  ( -0.4347878448725298051, 3.060161718936324160, -0.4204403343213366506 ) ) ;
#147706 = CARTESIAN_POINT ( 'NONE',  ( -5.413783410558481002, 5.210502155273325720, -0.7998128361456221525 ) ) ;
#147708 = EDGE_CURVE ( 'NONE', #147554, #73672, #61051, .T. ) ;
#147707 = CARTESIAN_POINT ( 'NONE',  ( 0.7499999999999902300, 5.597916667349482900, -1.299038105676658228 ) ) ;
#147709 = CARTESIAN_POINT ( 'NONE',  ( -1.402160292154681736E-14, -0.5531249996585814177, -1.575800808251665908 ) ) ;
#147710 = CARTESIAN_POINT ( 'NONE',  ( 6.450466390465378730, 0.5869013949594548141, 1.776180802621520005 ) ) ;
#147711 = CARTESIAN_POINT ( 'NONE',  ( 5.186046676097956443, 1.422060760911178390, 0.9921614550853893322 ) ) ;
#147712 = CARTESIAN_POINT ( 'NONE',  ( 4.616618505336416156, -0.07905358554981949115, 1.738770568734932853 ) ) ;
#147713 = CARTESIAN_POINT ( 'NONE',  ( 2.686486993802192913, 6.285985259411197568, 0.7998128361456362523 ) ) ;
#147714 = CARTESIAN_POINT ( 'NONE',  ( 1.892491709730130145, -0.6158747592755541289, -2.208019654398277520 ) ) ;
#147715 = CARTESIAN_POINT ( 'NONE',  ( -0.6823417656250212460, 5.363541667008087543, 1.181850606188767472 ) ) ;
#147716 = CARTESIAN_POINT ( 'NONE',  ( 5.882390464068013358, -0.3075192527470702042, -2.067890480286633803 ) ) ;
#147717 = CARTESIAN_POINT ( 'NONE',  ( 0.8316833483592298570, 1.813467871694788069, 0.3170515863319539052 ) ) ;
#147718 = EDGE_CURVE ( 'NONE', #1071, #76194, #137297, .T. ) ;
#147719 = CARTESIAN_POINT ( 'NONE',  ( -0.3000000000000414002, 3.999999999999974243, 1.007084189318353973 ) ) ;
#147720 = CARTESIAN_POINT ( 'NONE',  ( 2.397230751819504402, 1.409552409829779140, 1.160114028286141075 ) ) ;
#147721 = CARTESIAN_POINT ( 'NONE',  ( 3.041638857185970046, -1.525043868314728934, 1.319228477497782714 ) ) ;
#147722 = CARTESIAN_POINT ( 'NONE',  ( 1.289316216709124996, 1.661312375189183399, 1.429258102917586815 ) ) ;
#147723 = CARTESIAN_POINT ( 'NONE',  ( 9.681426354872444406, 13.43812210156014686, -8.165041025796163865 ) ) ;
#147724 = CARTESIAN_POINT ( 'NONE',  ( -7.901704598666176693, 8.113076874732334076, 0.7998128361456602331 ) ) ;
#147725 = CARTESIAN_POINT ( 'NONE',  ( 1.152881054890652957, -0.5012615762394446728, -2.008655542368184221 ) ) ;
#147726 = CARTESIAN_POINT ( 'NONE',  ( 4.008406971134620633, 7.828225232965717595, 0.7998128361456321445 ) ) ;
#147727 = CARTESIAN_POINT ( 'NONE',  ( 1.360316468749989793, -0.4322916663252800995, -0.7853790794158961308 ) ) ;
#147729 = B_SPLINE_CURVE_WITH_KNOTS ( 'NONE', 3,
 ( #141205, #127130, #110856, #94567, #160610, #12212, #177938, #164870 ),
 .UNSPECIFIED., .F., .F.,
 ( 4, 2, 2, 4 ),
 ( 0.000000000000000000, 0.001495953190030211571, 0.002991906380060423143, 0.005983812760120844551 ),
 .UNSPECIFIED. ) ;
#147728 = CARTESIAN_POINT ( 'NONE',  ( 4.108145954595856075, -0.8103754143699601897, 1.959725966023172727 ) ) ;
#147730 = TOROIDAL_SURFACE ( 'NONE', #37155, 0.8300000000000010703, 0.08000000000000000167 ) ;
#147731 = CARTESIAN_POINT ( 'NONE',  ( -1.364683531250014514, 0.03020833367475737191, 0.7879004041258379498 ) ) ;
#147732 = CARTESIAN_POINT ( 'NONE',  ( 6.199803715563785289, -0.6102442156579389598, 1.720816905678754782 ) ) ;
#147733 = ORIENTED_EDGE ( 'NONE', *, *, #11410, .T. ) ;
#147734 = CARTESIAN_POINT ( 'NONE',  ( -6.479871072688648148, 6.524547437750345402, 0.000000000000000000 ) ) ;
#147735 = CARTESIAN_POINT ( 'NONE',  ( 9.642873567817520808, 12.27310513391906532, 1.599625672291279388 ) ) ;
#147736 = CARTESIAN_POINT ( 'NONE',  ( 6.007671464186823407, 9.062681570643055906, 1.082531754730549967 ) ) ;
#147737 = CARTESIAN_POINT ( 'NONE',  ( 3.475000000000000533, -2.610416665710752593, 2.006292185433948827 ) ) ;
#147738 = CARTESIAN_POINT ( 'NONE',  ( -6.449928391799210736, 8.548002428564306143, -1.599625672291263179 ) ) ;
#147739 = CARTESIAN_POINT ( 'NONE',  ( 3.234633093136650928, 1.278207680322031026, -1.563912617747134970 ) ) ;
#147740 = CARTESIAN_POINT ( 'NONE',  ( 0.9210891864466156376, 1.945811402625597486, 0.8060233215861163369 ) ) ;
#147741 = CARTESIAN_POINT ( 'NONE',  ( -5.661411662158206681, 8.762674818229999829, -1.199719254218452047 ) ) ;
#147742 = CARTESIAN_POINT ( 'NONE',  ( 7.391166297744269365, 11.77477778067701664, 1.040834085586084257E-14 ) ) ;
#147743 = CARTESIAN_POINT ( 'NONE',  ( 4.961672996587167539, -0.4989766864872626217, 1.792691909438326681 ) ) ;
#147744 = CARTESIAN_POINT ( 'NONE',  ( 7.228468454380276853, 11.58496363008569574, 1.040834085586084257E-14 ) ) ;
#147745 = CARTESIAN_POINT ( 'NONE',  ( -0.4841233049523207543, 4.104380949686882829, 0.4351758553768784177 ) ) ;
#147746 = CARTESIAN_POINT ( 'NONE',  ( -3.469997250093771246, 6.135748327496311383, -1.199719254218452935 ) ) ;
#147747 = CARTESIAN_POINT ( 'NONE',  ( -5.856232286098998152, 8.919689202835742847, 1.199719254218452047 ) ) ;
#147748 = CARTESIAN_POINT ( 'NONE',  ( 6.157116169989634180, -1.766321488544853935, -1.061543263526150138 ) ) ;
#147750 = CARTESIAN_POINT ( 'NONE',  ( -4.637175514440688318, 7.109613026884349374, 1.382187809737724704 ) ) ;
#147749 = CARTESIAN_POINT ( 'NONE',  ( -6.771371375382467583, 6.864631124226471037, -0.7998128361456362523 ) ) ;
#147751 = CARTESIAN_POINT ( 'NONE',  ( -1.364683531250000748, 0.5093750003414208027, 0.000000000000000000 ) ) ;
#147752 = CARTESIAN_POINT ( 'NONE',  ( 2.319350913329641717, -1.342983818224493531, 1.096632721805221200 ) ) ;
#147753 = CARTESIAN_POINT ( 'NONE',  ( 1.499541640181512481, -0.6240335575410212998, -1.624780663456944385 ) ) ;
#147755 = CARTESIAN_POINT ( 'NONE',  ( 7.510853912290742507, 8.825379654836435606, -1.082531754730537976 ) ) ;
#147754 = CARTESIAN_POINT ( 'NONE',  ( 6.516287943725491694, -1.081378002916585368, -2.038673766938512877 ) ) ;
#147756 = CARTESIAN_POINT ( 'NONE',  ( -10.93365108933372198, 4.740440605563193799, -4.433365903526399698 ) ) ;
#147757 = CARTESIAN_POINT ( 'NONE',  ( 2.618495166727810908, 1.348686541216067347, -1.558216953862724408 ) ) ;
#147758 = CARTESIAN_POINT ( 'NONE',  ( 4.710568305744190276, 7.583081225755162968, 1.199719254218462483 ) ) ;
#147759 = CARTESIAN_POINT ( 'NONE',  ( 1.528672481244568448, 1.986742605292156405, -0.3418812301651391605 ) ) ;
#147760 = CARTESIAN_POINT ( 'NONE',  ( 6.925078400183526384, 2.431821113958906544, 2.425929786733098226 ) ) ;
#147761 = CARTESIAN_POINT ( 'NONE',  ( -4.502189528189771472, 7.410248995266807803, -1.199719254218453823 ) ) ;
#147762 = CARTESIAN_POINT ( 'NONE',  ( 0.8484322082523039210, 0.5699466304493487900, 1.887293252202123739 ) ) ;
#147763 = AXIS2_PLACEMENT_3D ( 'NONE', #71060, #41822, #6066 ) ;
#147765 = CARTESIAN_POINT ( 'NONE',  ( -6.861835142292179057, 9.098836647464588978, 1.443375672974064550 ) ) ;
#147764 = CARTESIAN_POINT ( 'NONE',  ( 4.728717205193702533, 1.314622909153417174, -1.389140896021365368 ) ) ;
#147766 = CARTESIAN_POINT ( 'NONE',  ( 5.971336403843030105, 0.1662174427981797931, -2.200672837095698497 ) ) ;
#147767 = CARTESIAN_POINT ( 'NONE',  ( -5.573810548549546162, 9.516879716700865188, 0.7216878364870267237 ) ) ;
#147768 = CARTESIAN_POINT ( 'NONE',  ( 5.352436782344940802, 9.466536356036257871, 0.000000000000000000 ) ) ;
#147769 = CARTESIAN_POINT ( 'NONE',  ( -4.624739795592948788, 5.528522862014106920, -1.082531754730549967 ) ) ;
#147770 = CARTESIAN_POINT ( 'NONE',  ( 0.2584707923105635796, 2.014430608512500775, 0.1461574478831758339 ) ) ;
#147771 = DIRECTION ( 'NONE',  ( 1.000000000000000000, -7.771561172376097755E-16, -4.440892098500627148E-16 ) ) ;
#147772 = CARTESIAN_POINT ( 'NONE',  ( 4.348838485402671594, 0.6111939248801941948, 2.225120539556017629 ) ) ;
#147773 = CARTESIAN_POINT ( 'NONE',  ( 5.037533845850875380, 1.831247050742194515, -0.7043679133837479345 ) ) ;
#147774 = CARTESIAN_POINT ( 'NONE',  ( 1.410910527293834260, -1.549868713165471590, 1.202602906592651788 ) ) ;
#147775 = CARTESIAN_POINT ( 'NONE',  ( 8.211434591371064684, 12.73175745657494851, -0.7998128361456352531 ) ) ;
#147776 = CARTESIAN_POINT ( 'NONE',  ( 1.499999999999990896, 6.280000000000042881, 2.873333333333337070 ) ) ;
#147777 = ORIENTED_EDGE ( 'NONE', *, *, #10652, .T. ) ;
#147778 = CARTESIAN_POINT ( 'NONE',  ( -0.02988430322643093051, -0.9920087411236072628, 1.870552836459241419 ) ) ;
#147780 = CARTESIAN_POINT ( 'NONE',  ( -6.170932472514347289, 10.35117165124207972, 0.000000000000000000 ) ) ;
#147779 = CARTESIAN_POINT ( 'NONE',  ( -5.922214171070950606, 5.803671375871217286, -0.7998128361456291469 ) ) ;
#147781 = CARTESIAN_POINT ( 'NONE',  ( 0.5328340850149284602, -1.300071877079148841, -1.303948673260245439 ) ) ;
#147782 = ORIENTED_EDGE ( 'NONE', *, *, #111061, .F. ) ;
#147783 = CARTESIAN_POINT ( 'NONE',  ( 4.276368498475341617, -1.111101898244113872, -1.865058090000100366 ) ) ;
#147784 = CARTESIAN_POINT ( 'NONE',  ( 0.2829853868402352757, 2.699735994070968204, 1.982489694896476973 ) ) ;
#147785 = CARTESIAN_POINT ( 'NONE',  ( 2.303126745213024851, -0.3670769733005623814, -2.088442229865586697 ) ) ;
#147786 = CARTESIAN_POINT ( 'NONE',  ( 0.7499999999999902300, 3.514583334016149863, 1.299038105676669330 ) ) ;
#147787 = CARTESIAN_POINT ( 'NONE',  ( 7.703003830858588863, 12.13858823597705872, -0.7998128361456291469 ) ) ;
#147788 = CYLINDRICAL_SURFACE ( 'NONE', #39077, 11.99999999999999112 ) ;
#147789 = CARTESIAN_POINT ( 'NONE',  ( 6.489313741793890422, 6.842916442627623219, -0.5960428994750706089 ) ) ;
#147790 = CARTESIAN_POINT ( 'NONE',  ( 2.302092711735738373, -2.060399031734764463, 0.04731154407941646350 ) ) ;
#147792 = DIRECTION ( 'NONE',  ( -3.451266460341926649E-31, -5.200010849845536803E-32, 1.000000000000000000 ) ) ;
#147791 = CARTESIAN_POINT ( 'NONE',  ( -7.720478407978036195, 11.09464301169468037, -1.199719254218446718 ) ) ;
#147793 = CARTESIAN_POINT ( 'NONE',  ( 1.364683531249988535, 3.655208333674750509, -0.7879004041258239610 ) ) ;
#147794 = CARTESIAN_POINT ( 'NONE',  ( 0.07755575628181145265, 0.6932613274447991802, -2.271134039238668301 ) ) ;
#147795 = CARTESIAN_POINT ( 'NONE',  ( 5.737007114546517350, 7.374902727567925531, -1.359833108435629656 ) ) ;
#147796 = CARTESIAN_POINT ( 'NONE',  ( 6.076807558263135789, -1.348954070496380941, 1.355674883165632227 ) ) ;
#147797 = VECTOR ( 'NONE', #191969, 1000.000000000000000 ) ;
#147798 = CARTESIAN_POINT ( 'NONE',  ( 6.661184041420940005, 7.849261790823902629, -6.773376349083132908 ) ) ;
#147799 = CARTESIAN_POINT ( 'NONE',  ( 1.704739465036476442, -0.8136145326368517949, -2.111227425349770481 ) ) ;
#147800 = CARTESIAN_POINT ( 'NONE',  ( -10.33094986393327197, 11.15512238411806578, 0.7216878364870438212 ) ) ;
#147801 = CARTESIAN_POINT ( 'NONE',  ( 1.124954419467529831, 1.598432135740068372, 0.8524628987082534248 ) ) ;
#147802 = CARTESIAN_POINT ( 'NONE',  ( 2.430754934859931549, -1.590173441703069956, 1.067998681346548961 ) ) ;
#147803 = CARTESIAN_POINT ( 'NONE',  ( 2.594261239525695206, 0.9781076984213372683, -1.824767828009652426 ) ) ;
#147804 = CARTESIAN_POINT ( 'NONE',  ( 0.6823417656249899377, 1.405208333674752508, 1.181850606188755259 ) ) ;
#147805 = AXIS2_PLACEMENT_3D ( 'NONE', #173084, #152546, #120123 ) ;
#147806 = CARTESIAN_POINT ( 'NONE',  ( 1.147272922670502515, -1.552894836003695600, -1.214464739729806730 ) ) ;
#147807 = CARTESIAN_POINT ( 'NONE',  ( 5.127533266204091333, -1.828772253489078237, 0.6060055780525953617 ) ) ;
#147809 = CARTESIAN_POINT ( 'NONE',  ( 6.330867959801246059, 6.852818249511213544, -0.6651261847785728820 ) ) ;
#147808 = CARTESIAN_POINT ( 'NONE',  ( 0.6808296902291348651, -1.277277952767090774, 1.921808783382691788 ) ) ;
#147810 = CARTESIAN_POINT ( 'NONE',  ( 1.364683531249988757, 2.384375000341422357, 1.214306433183764966E-14 ) ) ;
#147811 = CARTESIAN_POINT ( 'NONE',  ( 5.002416047594211435, 2.056911163480923843, 0.1552035700525862538 ) ) ;
#147812 = CARTESIAN_POINT ( 'NONE',  ( -6.098470168048611306, 6.009303372345148553, 1.040834085586084257E-14 ) ) ;
#147813 = CARTESIAN_POINT ( 'NONE',  ( 8.274553823041976841, 8.548067636504127265, 1.040834085586084257E-14 ) ) ;
#147814 = CARTESIAN_POINT ( 'NONE',  ( 0.000000000000000000, 8.600000000000017408, 0.4000000000000045186 ) ) ;
#147816 = CARTESIAN_POINT ( 'NONE',  ( -1.500000000000011324, 5.170833333333356485, 0.8660254037844403729 ) ) ;
#147815 = CARTESIAN_POINT ( 'NONE',  ( 6.176810970088661534, -1.998525488361714508, -0.6642400113570454678 ) ) ;
#147817 = CARTESIAN_POINT ( 'NONE',  ( -1.201851678989727383E-14, 2.384375000341416584, 1.575800808251672791 ) ) ;
#147818 = CARTESIAN_POINT ( 'NONE',  ( 5.079442160427912967, 2.018932005888602887, -0.7727740077691500620 ) ) ;
#147819 = CARTESIAN_POINT ( 'NONE',  ( 5.250651393837939551, 1.990147761501987800, 0.3430726210427292311 ) ) ;
#147820 = DIRECTION ( 'NONE',  ( 0.000000000000000000, -7.228014483236694583E-17, 1.000000000000000000 ) ) ;
#147821 =( GEOMETRIC_REPRESENTATION_CONTEXT ( 3 ) GLOBAL_UNCERTAINTY_ASSIGNED_CONTEXT ( ( #85658 ) ) GLOBAL_UNIT_ASSIGNED_CONTEXT ( ( #35766, #151673, #3244 ) ) REPRESENTATION_CONTEXT ( 'NONE', 'WORKASPACE' ) );
#147822 = CARTESIAN_POINT ( 'NONE',  ( -4.256897045010916258, 7.910204285913967404, 0.7216878364870317197 ) ) ;
#147825 = CARTESIAN_POINT ( 'NONE',  ( 5.097502569058200983, 6.970172302033127210, -1.443375672974051449 ) ) ;
#147824 = CARTESIAN_POINT ( 'NONE',  ( 1.642778471875000035, -0.9260416661887073131, -2.845375778867859751 ) ) ;
#147823 = CARTESIAN_POINT ( 'NONE',  ( 6.068156270568149324, 9.237210194708310951, 1.199719254218452047 ) ) ;
#147826 = CARTESIAN_POINT ( 'NONE',  ( -5.224688093219839402, 7.188831756880171397, -1.599625672291271394 ) ) ;
#147827 = CARTESIAN_POINT ( 'NONE',  ( 4.012907874177486178, 0.1037781579101039742, 2.014008197856680393 ) ) ;
#147828 = CARTESIAN_POINT ( 'NONE',  ( -8.148614017013223076, 9.465470093725620870, -1.199719254218446718 ) ) ;
#147830 = DIRECTION ( 'NONE',  ( 0.000000000000000000, 0.000000000000000000, -1.000000000000000000 ) ) ;
#147829 = CARTESIAN_POINT ( 'NONE',  ( -10.46653140006992899, 11.31330084294416771, -0.7216878364870267237 ) ) ;
#147831 = CARTESIAN_POINT ( 'NONE',  ( 1.364683531249990311, 5.134375000341417916, 1.214306433183764966E-14 ) ) ;
#147833 = CARTESIAN_POINT ( 'NONE',  ( 1.364683531249997417, 9.484375000341396245, 2.602085213965210642E-15 ) ) ;
#147832 = CARTESIAN_POINT ( 'NONE',  ( 4.821240550277555492, -0.1094919189667045711, 2.159058991224649393 ) ) ;
#147834 = DIRECTION ( 'NONE',  ( 0.000000000000000000, -1.000000000000000000, 0.000000000000000000 ) ) ;
#147835 = CARTESIAN_POINT ( 'NONE',  ( -11.67711829288551328, 7.340396131222296283, -2.774295504980774485 ) ) ;
#147837 = CARTESIAN_POINT ( 'NONE',  ( 5.888296041240274725, -0.7283935311428509918, -1.880430420734761965 ) ) ;
#147836 = CARTESIAN_POINT ( 'NONE',  ( -6.331294547457448019, 10.33033470543493770, 0.7216878364870458196 ) ) ;
#147838 = CARTESIAN_POINT ( 'NONE',  ( 0.6823417656249882723, -0.09479166632524876901, 1.181850606188755259 ) ) ;
#147839 = CARTESIAN_POINT ( 'NONE',  ( 0.6622201036875573488, -1.252624510564132931, 1.186060005986578014 ) ) ;
#147840 = CARTESIAN_POINT ( 'NONE',  ( 5.598591087800349086, 5.496387455380669529, -0.7998128361456481317 ) ) ;
#147842 = CARTESIAN_POINT ( 'NONE',  ( 7.340813827156391191, 7.528980651296110160, 0.7998128361456281477 ) ) ;
#147841 = CARTESIAN_POINT ( 'NONE',  ( 7.998947442382716488, 9.394822106610419610, -1.082531754730543083 ) ) ;
#147843 = CARTESIAN_POINT ( 'NONE',  ( 6.257094453949625823, -1.604276942902042480, -0.9616840659161307592 ) ) ;
#147844 = CARTESIAN_POINT ( 'NONE',  ( 0.9264321329857813092, -0.9072109017984790746, -1.797169606962043309 ) ) ;
#147845 = CARTESIAN_POINT ( 'NONE',  ( 3.348500752450942031, 4.929670182657964084, 1.443375672974066548 ) ) ;
#147846 = CARTESIAN_POINT ( 'NONE',  ( 3.399657359236216703, 1.738403758043248759, 1.359216269546263511 ) ) ;
#147847 = CARTESIAN_POINT ( 'NONE',  ( -6.414416072596845986, 8.576847732820027659, -1.443375672974066548 ) ) ;
#147848 = VERTEX_POINT ( 'NONE', #86465 ) ;
#147849 = CARTESIAN_POINT ( 'NONE',  ( 7.876924059415351564, 12.13356913605253240, -0.7216878364870267237 ) ) ;
#147851 = CARTESIAN_POINT ( 'NONE',  ( 1.634388897023292486, 0.6352195160324504153, 1.913798142305182415 ) ) ;
#147850 = CARTESIAN_POINT ( 'NONE',  ( 2.244932509249154329, 2.057497683098849617, 0.5125483897536405875 ) ) ;
#147853 = ORIENTED_EDGE ( 'NONE', *, *, #77726, .T. ) ;
#147852 = CARTESIAN_POINT ( 'NONE',  ( 2.056637812947777810, 0.3998733141725440698, 1.766706770180977548 ) ) ;
#147854 = CARTESIAN_POINT ( 'NONE',  ( 8.025500584646550806, 8.327781868367935658, 0.000000000000000000 ) ) ;
#147855 = EDGE_CURVE ( 'NONE', #212637, #71815, #147649, .T. ) ;
#147856 = ORIENTED_EDGE ( 'NONE', *, *, #114075, .T. ) ;
#147857 = EDGE_CURVE ( 'NONE', #20507, #154752, #70884, .T. ) ;
#147858 = CARTESIAN_POINT ( 'NONE',  ( 4.638861114170084399, 8.563755066507100722, 0.7998128361456462443 ) ) ;
#147860 = CARTESIAN_POINT ( 'NONE',  ( -0.2411972340276360705, -0.002466136893084554509, -1.900252416837118430 ) ) ;
#147859 = CARTESIAN_POINT ( 'NONE',  ( -3.242371291962510504, 6.934516940598226320, 1.040834085586084257E-14 ) ) ;
#147861 = DIRECTION ( 'NONE',  ( 0.000000000000000000, -1.000000000000000000, 0.000000000000000000 ) ) ;
#147862 = CARTESIAN_POINT ( 'NONE',  ( 9.605391220871890567, -6.900199406649618616, -0.04765083308771667775 ) ) ;
#147863 =( BOUNDED_CURVE ( )  B_SPLINE_CURVE ( 2, ( #126393, #192352, #176140, #102327, #116508, #3727, #181443, #19997, #119713 ),
 .UNSPECIFIED., .F., .T. ) 
 B_SPLINE_CURVE_WITH_KNOTS ( ( 3, 2, 2, 2, 3 ),
 ( 0.3660714285714286031, 0.3690476190476190688, 0.3750000000000000000, 0.3809523809523809312, 0.3839285714285713969 ),
 .UNSPECIFIED. ) 
 CURVE ( )  GEOMETRIC_REPRESENTATION_ITEM ( )  RATIONAL_B_SPLINE_CURVE ( ( 0.9330127018922194093, 0.9330127018922199644, 1.000000000000000000, 0.8660254037844387076, 1.000000000000000000, 0.8660254037844387076, 1.000000000000000000, 0.9330127018922199644, 0.9330127018922194093 ) ) 
 REPRESENTATION_ITEM ( '' )  );
#147864 = CARTESIAN_POINT ( 'NONE',  ( 5.626270559546821204, 6.626699076635176766, 1.082531754730560403 ) ) ;
#147865 = CARTESIAN_POINT ( 'NONE',  ( -0.6823417656250003738, 0.7802083336747520637, -1.181850606188749264 ) ) ;
#147866 = DIRECTION ( 'NONE',  ( -0.3321398189114292965, 0.9432301631592805435, 0.000000000000000000 ) ) ;
#147867 = CARTESIAN_POINT ( 'NONE',  ( -8.123306592882240551, 12.62894145833798376, 0.000000000000000000 ) ) ;
#147868 = B_SPLINE_CURVE_WITH_KNOTS ( 'NONE', 3,
 ( #155708, #122229, #141632, #207640, #59258, #142689 ),
 .UNSPECIFIED., .F., .F.,
 ( 4, 2, 4 ),
 ( 0.000000000000000000, 0.0003472644472073818721, 0.0006945288944147637441 ),
 .UNSPECIFIED. ) ;
#147869 = CARTESIAN_POINT ( 'NONE',  ( 3.590839768554392908, -0.4196827604958653923, -2.120402733634827452 ) ) ;
#147870 = CARTESIAN_POINT ( 'NONE',  ( -5.641601317062247212, 7.675230518029648508, -1.443375672974066548 ) ) ;
#147871 = CARTESIAN_POINT ( 'NONE',  ( 5.289089323106923146, 6.303597310780433283, -1.082531754730548412 ) ) ;
#147872 = CARTESIAN_POINT ( 'NONE',  ( 1.564851893998190135, 0.6701894319398638000, 2.011955567234039677 ) ) ;
#147873 = CARTESIAN_POINT ( 'NONE',  ( 4.177814833339410505, 3.976464848425038223, -0.02210016498919950903 ) ) ;
#147874 = CARTESIAN_POINT ( 'NONE',  ( 3.216049615590831579, -0.9687177021495720908, -1.716833007709689607 ) ) ;
#147875 = CARTESIAN_POINT ( 'NONE',  ( 5.554919272666569263, 0.3793472168572444292, 1.874222000232607765 ) ) ;
#147876 = ORIENTED_EDGE ( 'NONE', *, *, #47895, .T. ) ;
#147877 = SURFACE_STYLE_FILL_AREA ( #14645 ) ;
#147878 = CARTESIAN_POINT ( 'NONE',  ( 6.672316266636414639, -0.9270569987065898632, -1.737699753229291710 ) ) ;
#147879 = CARTESIAN_POINT ( 'NONE',  ( 1.077954490650166575, -1.894526023430597617, -0.4258829084243920260 ) ) ;
#147880 = EDGE_LOOP ( 'NONE', ( #72720, #207015, #188054, #20673 ) ) ;
#147881 = FACE_OUTER_BOUND ( 'NONE', #148833, .T. ) ;
#147883 = CARTESIAN_POINT ( 'NONE',  ( 0.4655726814510594003, -8.186910006429393150, 9.501690549794789220 ) ) ;
#147882 = CARTESIAN_POINT ( 'NONE',  ( -6.129694847154211423, 9.205042184104968328, -1.082531754730549967 ) ) ;
#147885 = CARTESIAN_POINT ( 'NONE',  ( 7.467843683028853263, 7.606905806488803101, 0.7998128361456341429 ) ) ;
#147884 = CARTESIAN_POINT ( 'NONE',  ( 2.378955762007132435, 1.911079870108543410, -0.8480884496332024014 ) ) ;
#147887 = CARTESIAN_POINT ( 'NONE',  ( 4.217995187182915551, 7.935095128439824563, 0.7216878364870257245 ) ) ;
#147886 = CARTESIAN_POINT ( 'NONE',  ( 6.632963465583686435, 8.761543347979550589, -1.599625672291262513 ) ) ;
#147889 = ORIENTED_EDGE ( 'NONE', *, *, #158942, .T. ) ;
#147888 = CARTESIAN_POINT ( 'NONE',  ( 5.584596538761583240, -1.209766832763665034, 1.480987728393488245 ) ) ;
#147890 = CARTESIAN_POINT ( 'NONE',  ( 4.899154391205060577, 1.836108854712194649, -1.224054507610386366 ) ) ;
#147891 = CARTESIAN_POINT ( 'NONE',  ( 1.870444250305805856, 1.134645063044220858, 1.892580404734986121 ) ) ;
#147892 = CARTESIAN_POINT ( 'NONE',  ( -11.01135777277262306, 12.59376995022298473, 1.399999999999998579 ) ) ;
#147893 = CARTESIAN_POINT ( 'NONE',  ( 0.5219363917940004205, -1.903054291476031112, 0.1877445768119419822 ) ) ;
#147894 = CARTESIAN_POINT ( 'NONE',  ( -10.49999999999999822, 13.50840886959780462, -3.600000000000000977 ) ) ;
#147895 = DIRECTION ( 'NONE',  ( 0.1700204568168880159, -0.9655305911742139147, 0.1970881066187147312 ) ) ;
#147896 = CARTESIAN_POINT ( 'NONE',  ( 4.088381982606685838, 1.110138344689771239, -1.747393465062855311 ) ) ;
#147898 = CARTESIAN_POINT ( 'NONE',  ( 1.182749364907993206, -2.109161078630458430, -0.4729781282231394490 ) ) ;
#147897 = CARTESIAN_POINT ( 'NONE',  ( -2.764973262183167968, 5.313220341600567664, 1.199719254218462483 ) ) ;
#147899 = CARTESIAN_POINT ( 'NONE',  ( 4.107102485094754840, -0.3736803571842538529, 2.159302612355806339 ) ) ;
#147900 = LINE ( 'NONE', #98095, #65833 ) ;
#147901 = DIRECTION ( 'NONE',  ( -8.638326563840814399E-31, -0.000000000000000000, -1.000000000000000000 ) ) ;
#147902 = CARTESIAN_POINT ( 'NONE',  ( 1.468321960012000549, 7.242494692103044862, 4.289992922803952169 ) ) ;
#147903 = CARTESIAN_POINT ( 'NONE',  ( -1.364683531250000748, 14.17187500034140157, 0.000000000000000000 ) ) ;
#147904 = CARTESIAN_POINT ( 'NONE',  ( -4.197131071882288289, 7.054347462908075350, -1.199719254218455378 ) ) ;
#147905 = UNCERTAINTY_MEASURE_WITH_UNIT (LENGTH_MEASURE( 1.000000000000000082E-05 ), #51279, 'distance_accuracy_value', 'NONE');
#147906 = CARTESIAN_POINT ( 'NONE',  ( 0.3873425458618062200, -0.6819987885887256462, -1.897696807414723796 ) ) ;
#147907 = CARTESIAN_POINT ( 'NONE',  ( -8.161645285746702783, 12.46574390010577105, 0.7216878364870478180 ) ) ;
#147908 = AXIS2_PLACEMENT_3D ( 'NONE', #198740, #165201, #16793 ) ;
#147909 = CARTESIAN_POINT ( 'NONE',  ( 4.258688845354158481, -0.6446009455991276171, -1.967446834807617284 ) ) ;
#147910 = CARTESIAN_POINT ( 'NONE',  ( 5.308266703545434062, 1.260341450243172678, -1.701113402177101053 ) ) ;
#147911 = CARTESIAN_POINT ( 'NONE',  ( 5.991813822235618758, 9.077867661661846554, 1.199719254218462483 ) ) ;
#147912 = CARTESIAN_POINT ( 'NONE',  ( 9.534369015033190564, 4.462424917548984737, 7.287319680779482667 ) ) ;
#147913 = CARTESIAN_POINT ( 'NONE',  ( 3.696117419531047776, 0.8894436365228419739, -1.757264023730123581 ) ) ;
#147914 = CARTESIAN_POINT ( 'NONE',  ( 5.753944192167276483, 0.9242165444633635429, 2.097870995526931015 ) ) ;
#147915 = CARTESIAN_POINT ( 'NONE',  ( 3.439906511156048285, 0.8199118703316324863, -1.631291955839441865 ) ) ;
#147916 = CARTESIAN_POINT ( 'NONE',  ( 4.577813143269636065, 5.369812084349879555, -1.199719254218450271 ) ) ;
#147918 = ADVANCED_FACE ( 'NONE', ( #105966 ), #5177, .F. ) ;
#147917 = CARTESIAN_POINT ( 'NONE',  ( 5.802526556524483681, 5.871961858807763335, 1.040834085586084257E-14 ) ) ;
#147919 = CARTESIAN_POINT ( 'NONE',  ( -7.528855374290365887, 7.678086112960552434, -0.7998128361456291469 ) ) ;
#147920 = CARTESIAN_POINT ( 'NONE',  ( 6.690022453700429139, 6.769724048930809701, 0.7998128361456331437 ) ) ;
#147921 = EDGE_LOOP ( 'NONE', ( #29155, #188793, #9084, #172503 ) ) ;
#147922 = CARTESIAN_POINT ( 'NONE',  ( 5.308844932141564499, -0.4931833774270472648, -1.951727149811402828 ) ) ;
#147923 = CARTESIAN_POINT ( 'NONE',  ( 6.153027625867640182, 1.178261263523974645, 1.973664585577431518 ) ) ;
#147924 = CARTESIAN_POINT ( 'NONE',  ( 4.451973756923766068, -0.7546651901383871763, 1.810992078419524365 ) ) ;
#147925 = CARTESIAN_POINT ( 'NONE',  ( -6.449928391799210736, 8.548002428564306143, -1.599625672291263179 ) ) ;
#147926 = CARTESIAN_POINT ( 'NONE',  ( -4.786191920824102830, 5.542644314838231168, 1.199719254218462483 ) ) ;
#147927 = FACE_OUTER_BOUND ( 'NONE', #80895, .T. ) ;
#147928 = CARTESIAN_POINT ( 'NONE',  ( -6.771371375382467583, 6.864631124226471037, -0.7998128361456362523 ) ) ;
#147930 = CARTESIAN_POINT ( 'NONE',  ( 5.612081123951941919, -0.7985520710115794341, -1.579504676149855458 ) ) ;
#147929 = CARTESIAN_POINT ( 'NONE',  ( 0.5563344311030217204, -1.511574431613523117, 1.444666882759609194 ) ) ;
#147931 = CARTESIAN_POINT ( 'NONE',  ( 10.91970695577495931, -5.907420853759283830, 1.951563910473907981E-15 ) ) ;
#147932 = CARTESIAN_POINT ( 'NONE',  ( 2.361504994916805877, 2.148894721571582789, -0.4289216190115978100 ) ) ;
#147933 = CARTESIAN_POINT ( 'NONE',  ( 1.469815953039468326, -1.652492729624547962, -0.5465173985150991731 ) ) ;
#147934 = CARTESIAN_POINT ( 'NONE',  ( 7.447506452608354088, 7.583179037664891098, 0.7998128361456341429 ) ) ;
#147935 = CARTESIAN_POINT ( 'NONE',  ( 0.2333690889706682703, 1.352610664630080839, -2.308230059406161772 ) ) ;
#147936 = CARTESIAN_POINT ( 'NONE',  ( 1.189626395179286478, -0.7786649258869399182, 1.539184141221685787 ) ) ;
#147938 = EDGE_CURVE ( 'NONE', #127758, #106229, #212128, .T. ) ;
#147937 = CARTESIAN_POINT ( 'NONE',  ( 1.822082775007987543, 1.258534617508931586, -1.793986466278547853 ) ) ;
#147939 = CARTESIAN_POINT ( 'NONE',  ( 3.950008152305323428, 0.7444041667201054535, -2.077678867657362538 ) ) ;
#147940 = AXIS2_PLACEMENT_3D ( 'NONE', #83255, #214285, #68050 ) ;
#147941 =( BOUNDED_SURFACE ( )  B_SPLINE_SURFACE ( 1, 2, ( 
 ( #148669, #135623, #53291, #85793, #99916, #151873, #185411, #37029, #103115, #20766, #165977, #86860, #152925, #4503, #120507, #186482, #38115, #140985, #89012, #39179, #22896, #155065, #6653, #87925, #72730, #203781, #205930, #204845, #40251, #190738, #91148, #139899, #90076, #42402, #172386, #138825, #57563, #187549, #107443, #7722, #8800, #154000, #56498, #157203, #170236, #21820, #122656, #188619, #106362, #25047, #5568, #206995, #173468, #189683, #74879, #123720, #23974, #58626, #121578, #124779, #105263, #171304, #156139, #73805, #41335, #71647, #137761, #55425, #152550, #120129, #169862, #69138, #203404, #153627, #200211, #70205, #100598, #102742, #51863, #2000, #121208, #136318, #67000, #183977, #185031, #167736, #150436, #166674, #186105, #117985, #187177, #137388, #21451, #18264, #86485, #170929, #4137, #135261, #38805, #50782, #104887, #199137, #116910, #35588, #202336, #201274, #22526, #53988, #68065, #149354, #37737, #934, #55057, #101667, #133138, #19336, #182910, #134201, #87559, #168797, #119047, #34526, #85415, #151498, #84348, #3068, #52914, #5199, #20404, #36657, #103813, #71274, #101719, #120179, #100650, #35640, #167790, #19385, #84402, #71324, #186155, #169912, #67053, #52962, #70257, #51914, #149407, #68120, #121256, #136371, #2049, #55110, #150490, #135310, #37789, #21501, #202390, #988, #199190, #103863, #50838, #87609, #151550, #134256, #85464, #153679, #3119, #18319, #54042, #69189, #201324, #20452, #83319, #34578, #119100, #5249, #200263, #187228, #118037, #185082, #137439, #203455, #38857, #133190, #116965, #104941, #182963, #170981, #36706, #184024, #102793, #166728, #168849, #86535, #152601, #4187, #74562, #174219, #22580, #188293, #90826, #59370, #58308, #39933, #56175, #25794, #124464, #24723, #190423, #156888, #204525, #122336, #142797, #23657, #42080, #108195, #75627, #92965, #106041, #172064, #73479, #89768, #155814, #140662, #60431, #7398, #206677, #57243, #8476, #91903, #139579, #88686, #6329, #157959, #110327, #76681, #208802, #72402, #9552, #141737, #207744, #125528, #205605, #107119, #154746, #191486, #43155, #123403, #189367, #109267, #41009, #175275, #26861, #173142, #159011, #10605, #126591, #192552, #138502, #44207, #210936, #82007, #144929, #29010, #12732, #62561, #78806, #160073, #128725, #127668, #163278, #112454, #79876, #197885, #180580, #97225, #195773, #49515, #145986, #194697, #14861, #177397, #130839, #113526, #164336, #11675, #46339, #213064, #193630, #178466, #30076, #96167, #95097, #15924, #64694, #48472, #77750, #211998, #80950, #162217, #27939, #161145, #214100, #147042, #63638, #196831, #13804, #94034, #129794, #65729, #114589, #47412, #148097, #179533, #31152, #32201, #98277, #131876, #143871, #209864, #176332, #61502, #45272, #111393, #116701, #54588, #139056, #136917, #50579, #171532, #120735, #170462, #55651, #115634, #66789, #186708, #155293 ),
 ( #16986, #40488, #83066, #723, #100394, #202944, #104413, #70804, #22047, #89242, #121807, #6876, #205083, #38337, #172620, #122893, #169401, #39406, #132928, #71875, #20987, #182701, #90299, #105500, #33259, #153154, #154226, #88158, #34319, #198934, #72954, #87084, #156369, #106592, #56725, #4729, #187774, #140135, #23125, #5798, #7953, #149143, #74045, #165391, #137985, #204002, #188852, #24196, #206161, #181630, #99342, #79374, #94581, #95658, #177952, #108743, #161709, #158496, #13301, #58855, #144423, #11152, #27416, #25280, #42634, #125011, #9036, #141221, #174769, #128222, #77229, #75110, #43697, #160624, #127144, #145493, #10095, #143348, #60991, #209343, #28490, #91382, #193116, #111950, #110873, #207231, #76169, #142274, #208285, #190968, #45829, #12225, #210425, #41563, #93514, #44765, #26344, #123949, #92457, #57789, #176878, #59916, #29566, #126073, #109814, #78298, #62067, #194184, #189918, #173705, #107676, #157442, #192034, #175823, #159556, #147586, #17537, #15417, #146542, #50077, #213604, #49018, #148646, #211488, #162774, #65230, #33812, #32753, #14352, #30641, #212, #98835, #131381, #164885, #197377, #179023, #96725, #117262, #212560, #16479, #82559, #116198, #67347, #80442, #64199, #47973, #130340, #196329, #115137, #34865, #114089, #181132, #31703, #66283, #132430, #180080, #63125, #195265, #198431, #84700, #51139, #183261, #46899, #182185, #99891, #165953, #83626, #97778, #81507, #129289, #149709, #1289, #163838, #133492, #199495, #100939, #167026, #18621, #113014, #102020, #88986, #135597, #103088, #134554, #200557, #185387, #56470, #119398, #3423, #201618, #37006, #53267, #52205, #169145, #168088, #137736, #86834, #54342, #172359, #155039, #71623, #170209, #23948, #120481, #20739, #203755, #151846, #105237, #87902, #138799, #118331, #152898, #187524, #55399, #4477, #2350, #70548, #188594, #121553, #69489, #122632, #136667, #202692, #171278, #22870, #39155, #68426, #184316, #6625, #35940, #72704, #186453, #38090, #104161, #204819, #21793, #85766, #40226, #153975, #5542, #106337, #150787, #19688, #158253, #126887, #125821, #107417, #123697, #93261, #191782, #92203, #43438, #9841, #57539, #189658, #210160, #91121, #109562, #175566, #143096, #160367, #173442, #41309, #140960, #25021, #157180, #208035, #127970, #74858, #59662, #124756, #75917, #27157, #8775, #90053, #73778, #142020, #177692, #144168, #61801, #139874, #159295, #10894, #76969, #209089, #206971, #174512, #156112, #60724, #192845, #58601, #190716, #44504, #42378, #110621, #176621, #108488, #26087, #28233, #94326, #11970, #205905, #78044, #193922, #45568, #111685, #7695, #80174, #63925, #146280, #13029, #196075, #194995, #16212, #179821, #147326, #50876, #33553, #164627, #48757, #116998, #213354, #212292, #82296, #30377, #198174, #180871, #17281, #79106, #47707, #66019, #46629, #113822, #31440, #97519, #96463, #83357 ) ),
 .UNSPECIFIED., .F., .F., .T. ) 
 B_SPLINE_SURFACE_WITH_KNOTS ( ( 2, 2 ),
 ( 3, 2, 2, 2, 2, 2, 2, 2, 2, 2, 2, 2, 2, 2, 2, 2, 2, 2, 2, 2, 2, 2, 2, 2, 2, 2, 2, 2, 2, 2, 2, 2, 2, 2, 2, 2, 2, 2, 2, 2, 2, 2, 2, 2, 2, 2, 2, 2, 2, 2, 2, 2, 2, 2, 2, 2, 2, 2, 2, 2, 2, 2, 2, 2, 2, 2, 2, 2, 2, 2, 2, 2, 2, 2, 2, 2, 2, 2, 2, 2, 2, 2, 2, 2, 2, 2, 2, 2, 2, 2, 2, 2, 2, 2, 2, 2, 2, 2, 2, 2, 2, 2, 2, 2, 2, 2, 2, 2, 2, 2, 2, 2, 2, 2, 2, 2, 2, 2, 2, 2, 2, 2, 2, 2, 2, 2, 2, 2, 2, 2, 2, 2, 2, 2, 2, 2, 2, 2, 2, 2, 2, 2, 2, 2, 2, 2, 2, 2, 2, 2, 2, 2, 2, 2, 2, 2, 2, 2, 2, 2, 2, 2, 2, 2, 2, 2, 2, 2, 3 ),
 ( 0.000000000000000000, 1.000000000000000000 ),
 ( 0.000000000000000000, 0.005952380952380952051, 0.01190476190476190410, 0.01785714285714285615, 0.02380952380952380820, 0.02976190476190476025, 0.03571428571428571230, 0.04166666666666666435, 0.04761904761904761640, 0.05357142857142856845, 0.05952380952380952051, 0.06547619047619047949, 0.07142857142857142461, 0.07738095238095238360, 0.08333333333333332871, 0.08928571428571428770, 0.09523809523809523281, 0.1011904761904761918, 0.1071428571428571369, 0.1130952380952380959, 0.1190476190476190410, 0.1250000000000000000, 0.1309523809523809590, 0.1369047619047619180, 0.1428571428571428492, 0.1488095238095238082, 0.1547619047619047672, 0.1607142857142857262, 0.1666666666666666574, 0.1726190476190476164, 0.1785714285714285754, 0.1845238095238095344, 0.1904761904761904656, 0.1964285714285714246, 0.2023809523809523836, 0.2083333333333333426, 0.2142857142857142738, 0.2202380952380952328, 0.2261904761904761918, 0.2321428571428571508, 0.2380952380952380820, 0.2440476190476190410, 0.2500000000000000000, 0.2559523809523809312, 0.2619047619047619180, 0.2678571428571428492, 0.2738095238095238360, 0.2797619047619047672, 0.2857142857142856984, 0.2916666666666666852, 0.2976190476190476164, 0.3035714285714285476, 0.3095238095238095344, 0.3154761904761904656, 0.3214285714285714524, 0.3273809523809523836, 0.3333333333333333148, 0.3392857142857143016, 0.3452380952380952328, 0.3511904761904761640, 0.3571428571428571508, 0.3630952380952380820, 0.3690476190476190688, 0.3750000000000000000, 0.3809523809523809312, 0.3869047619047619180, 0.3928571428571428492, 0.3988095238095238360, 0.4047619047619047672, 0.4107142857142856984, 0.4166666666666666852, 0.4226190476190476164, 0.4285714285714285476, 0.4345238095238095344, 0.4404761904761904656, 0.4464285714285714524, 0.4523809523809523836, 0.4583333333333333148, 0.4642857142857143016, 0.4702380952380952328, 0.4761904761904761640, 0.4821428571428571508, 0.4880952380952380820, 0.4940476190476190688, 0.5000000000000000000, 0.5059523809523809312, 0.5119047619047618625, 0.5178571428571429047, 0.5238095238095238360, 0.5297619047619047672, 0.5357142857142856984, 0.5416666666666666297, 0.5476190476190476719, 0.5535714285714286031, 0.5595238095238095344, 0.5654761904761904656, 0.5714285714285713969, 0.5773809523809523281, 0.5833333333333333703, 0.5892857142857143016, 0.5952380952380952328, 0.6011904761904761640, 0.6071428571428570953, 0.6130952380952381375, 0.6190476190476190688, 0.6250000000000000000, 0.6309523809523809312, 0.6369047619047618625, 0.6428571428571429047, 0.6488095238095238360, 0.6547619047619047672, 0.6607142857142856984, 0.6666666666666666297, 0.6726190476190476719, 0.6785714285714286031, 0.6845238095238095344, 0.6904761904761904656, 0.6964285714285713969, 0.7023809523809523281, 0.7083333333333333703, 0.7142857142857143016, 0.7202380952380952328, 0.7261904761904761640, 0.7321428571428570953, 0.7380952380952381375, 0.7440476190476190688, 0.7500000000000000000, 0.7559523809523809312, 0.7619047619047618625, 0.7678571428571429047, 0.7738095238095238360, 0.7797619047619047672, 0.7857142857142856984, 0.7916666666666666297, 0.7976190476190476719, 0.8035714285714286031, 0.8095238095238095344, 0.8154761904761904656, 0.8214285714285713969, 0.8273809523809523281, 0.8333333333333333703, 0.8392857142857143016, 0.8452380952380952328, 0.8511904761904761640, 0.8571428571428570953, 0.8630952380952381375, 0.8690476190476190688, 0.8750000000000000000, 0.8809523809523809312, 0.8869047619047618625, 0.8928571428571429047, 0.8988095238095238360, 0.9047619047619047672, 0.9107142857142856984, 0.9166666666666666297, 0.9226190476190476719, 0.9285714285714286031, 0.9345238095238095344, 0.9404761904761904656, 0.9464285714285713969, 0.9523809523809523281, 0.9583333333333333703, 0.9642857142857143016, 0.9702380952380952328, 0.9761904761904761640, 0.9821428571428570953, 0.9880952380952381375, 0.9940476190476190688, 1.000000000000000000 ),
 .UNSPECIFIED. ) 
 GEOMETRIC_REPRESENTATION_ITEM ( )  RATIONAL_B_SPLINE_SURFACE ( (
 ( 1.000000000000000000, 0.8660254037844387076, 1.000000000000000000, 0.8660254037844387076, 1.000000000000000000, 0.8660254037844387076, 1.000000000000000000, 0.8660254037844387076, 1.000000000000000000, 0.8660254037844387076, 1.000000000000000000, 0.8660254037844387076, 1.000000000000000000, 0.8660254037844387076, 1.000000000000000000, 0.8660254037844387076, 1.000000000000000000, 0.8660254037844387076, 1.000000000000000000, 0.8660254037844387076, 1.000000000000000000, 0.8660254037844387076, 1.000000000000000000, 0.8660254037844387076, 1.000000000000000000, 0.8660254037844387076, 1.000000000000000000, 0.8660254037844387076, 1.000000000000000000, 0.8660254037844387076, 1.000000000000000000, 0.8660254037844387076, 1.000000000000000000, 0.8660254037844387076, 1.000000000000000000, 0.8660254037844387076, 1.000000000000000000, 0.8660254037844387076, 1.000000000000000000, 0.8660254037844387076, 1.000000000000000000, 0.8660254037844387076, 1.000000000000000000, 0.8660254037844387076, 1.000000000000000000, 0.8660254037844387076, 1.000000000000000000, 0.8660254037844387076, 1.000000000000000000, 0.8660254037844387076, 1.000000000000000000, 0.8660254037844387076, 1.000000000000000000, 0.8660254037844387076, 1.000000000000000000, 0.8660254037844387076, 1.000000000000000000, 0.8660254037844387076, 1.000000000000000000, 0.8660254037844387076, 1.000000000000000000, 0.8660254037844387076, 1.000000000000000000, 0.8660254037844387076, 1.000000000000000000, 0.8660254037844387076, 1.000000000000000000, 0.8660254037844387076, 1.000000000000000000, 0.8660254037844387076, 1.000000000000000000, 0.8660254037844387076, 1.000000000000000000, 0.8660254037844387076, 1.000000000000000000, 0.8660254037844387076, 1.000000000000000000, 0.8660254037844387076, 1.000000000000000000, 0.8660254037844387076, 1.000000000000000000, 0.8660254037844387076, 1.000000000000000000, 0.8660254037844387076, 1.000000000000000000, 0.8660254037844387076, 1.000000000000000000, 0.8660254037844387076, 1.000000000000000000, 0.8660254037844387076, 1.000000000000000000, 0.8660254037844387076, 1.000000000000000000, 0.8660254037844387076, 1.000000000000000000, 0.8660254037844387076, 1.000000000000000000, 0.8660254037844387076, 1.000000000000000000, 0.8660254037844387076, 1.000000000000000000, 0.8660254037844387076, 1.000000000000000000, 0.8660254037844387076, 1.000000000000000000, 0.8660254037844387076, 1.000000000000000000, 0.8660254037844387076, 1.000000000000000000, 0.8660254037844387076, 1.000000000000000000, 0.8660254037844387076, 1.000000000000000000, 0.8660254037844387076, 1.000000000000000000, 0.8660254037844387076, 1.000000000000000000, 0.8660254037844387076, 1.000000000000000000, 0.8660254037844387076, 1.000000000000000000, 0.8660254037844387076, 1.000000000000000000, 0.8660254037844387076, 1.000000000000000000, 0.8660254037844387076, 1.000000000000000000, 0.8660254037844387076, 1.000000000000000000, 0.8660254037844387076, 1.000000000000000000, 0.8660254037844387076, 1.000000000000000000, 0.8660254037844387076, 1.000000000000000000, 0.8660254037844387076, 1.000000000000000000, 0.8660254037844387076, 1.000000000000000000, 0.8660254037844387076, 1.000000000000000000, 0.8660254037844387076, 1.000000000000000000, 0.8660254037844387076, 1.000000000000000000, 0.8660254037844387076, 1.000000000000000000, 0.8660254037844387076, 1.000000000000000000, 0.8660254037844387076, 1.000000000000000000, 0.8660254037844387076, 1.000000000000000000, 0.8660254037844387076, 1.000000000000000000, 0.8660254037844387076, 1.000000000000000000, 0.8660254037844387076, 1.000000000000000000, 0.8660254037844387076, 1.000000000000000000, 0.8660254037844387076, 1.000000000000000000, 0.8660254037844387076, 1.000000000000000000, 0.8660254037844387076, 1.000000000000000000, 0.8660254037844387076, 1.000000000000000000, 0.8660254037844387076, 1.000000000000000000, 0.8660254037844387076, 1.000000000000000000, 0.8660254037844387076, 1.000000000000000000, 0.8660254037844387076, 1.000000000000000000, 0.8660254037844387076, 1.000000000000000000, 0.8660254037844387076, 1.000000000000000000, 0.8660254037844387076, 1.000000000000000000, 0.8660254037844387076, 1.000000000000000000, 0.8660254037844387076, 1.000000000000000000, 0.8660254037844387076, 1.000000000000000000, 0.8660254037844387076, 1.000000000000000000, 0.8660254037844387076, 1.000000000000000000, 0.8660254037844387076, 1.000000000000000000, 0.8660254037844387076, 1.000000000000000000, 0.8660254037844387076, 1.000000000000000000, 0.8660254037844387076, 1.000000000000000000, 0.8660254037844387076, 1.000000000000000000, 0.8660254037844387076, 1.000000000000000000, 0.8660254037844387076, 1.000000000000000000, 0.8660254037844387076, 1.000000000000000000, 0.8660254037844387076, 1.000000000000000000, 0.8660254037844387076, 1.000000000000000000, 0.8660254037844387076, 1.000000000000000000, 0.8660254037844387076, 1.000000000000000000, 0.8660254037844387076, 1.000000000000000000, 0.8660254037844387076, 1.000000000000000000, 0.8660254037844387076, 1.000000000000000000, 0.8660254037844387076, 1.000000000000000000, 0.8660254037844387076, 1.000000000000000000, 0.8660254037844387076, 1.000000000000000000, 0.8660254037844387076, 1.000000000000000000, 0.8660254037844387076, 1.000000000000000000, 0.8660254037844387076, 1.000000000000000000, 0.8660254037844387076, 1.000000000000000000, 0.8660254037844387076, 1.000000000000000000, 0.8660254037844387076, 1.000000000000000000, 0.8660254037844387076, 1.000000000000000000, 0.8660254037844387076, 1.000000000000000000, 0.8660254037844387076, 1.000000000000000000, 0.8660254037844387076, 1.000000000000000000, 0.8660254037844387076, 1.000000000000000000, 0.8660254037844387076, 1.000000000000000000, 0.8660254037844387076, 1.000000000000000000, 0.8660254037844387076, 1.000000000000000000, 0.8660254037844387076, 1.000000000000000000, 0.8660254037844387076, 1.000000000000000000, 0.8660254037844387076, 1.000000000000000000, 0.8660254037844387076, 1.000000000000000000, 0.8660254037844387076, 1.000000000000000000, 0.8660254037844387076, 1.000000000000000000, 0.8660254037844387076, 1.000000000000000000, 0.8660254037844387076, 1.000000000000000000, 0.8660254037844387076, 1.000000000000000000, 0.8660254037844387076, 1.000000000000000000, 0.8660254037844387076, 1.000000000000000000, 0.8660254037844387076, 1.000000000000000000, 0.8660254037844387076, 1.000000000000000000, 0.8660254037844387076, 1.000000000000000000, 0.8660254037844387076, 1.000000000000000000, 0.8660254037844387076, 1.000000000000000000, 0.8660254037844387076, 1.000000000000000000, 0.8660254037844387076, 1.000000000000000000, 0.8660254037844387076, 1.000000000000000000, 0.8660254037844387076, 1.000000000000000000, 0.8660254037844387076, 1.000000000000000000, 0.8660254037844387076, 1.000000000000000000, 0.8660254037844387076, 1.000000000000000000, 0.8660254037844387076, 1.000000000000000000, 0.8660254037844387076, 1.000000000000000000, 0.8660254037844387076, 1.000000000000000000, 0.8660254037844387076, 1.000000000000000000, 0.8660254037844387076, 1.000000000000000000, 0.8660254037844387076, 1.000000000000000000, 0.8660254037844387076, 1.000000000000000000, 0.8660254037844387076, 1.000000000000000000, 0.8660254037844387076, 1.000000000000000000, 0.8660254037844387076, 1.000000000000000000, 0.8660254037844387076, 1.000000000000000000, 0.8660254037844387076, 1.000000000000000000, 0.8660254037844387076, 1.000000000000000000, 0.8660254037844387076, 1.000000000000000000, 0.8660254037844387076, 1.000000000000000000, 0.8660254037844387076, 1.000000000000000000, 0.8660254037844387076, 1.000000000000000000),
 ( 1.000000000000000000, 0.8660254037844387076, 1.000000000000000000, 0.8660254037844387076, 1.000000000000000000, 0.8660254037844387076, 1.000000000000000000, 0.8660254037844387076, 1.000000000000000000, 0.8660254037844387076, 1.000000000000000000, 0.8660254037844387076, 1.000000000000000000, 0.8660254037844387076, 1.000000000000000000, 0.8660254037844387076, 1.000000000000000000, 0.8660254037844387076, 1.000000000000000000, 0.8660254037844387076, 1.000000000000000000, 0.8660254037844387076, 1.000000000000000000, 0.8660254037844387076, 1.000000000000000000, 0.8660254037844387076, 1.000000000000000000, 0.8660254037844387076, 1.000000000000000000, 0.8660254037844387076, 1.000000000000000000, 0.8660254037844387076, 1.000000000000000000, 0.8660254037844387076, 1.000000000000000000, 0.8660254037844387076, 1.000000000000000000, 0.8660254037844387076, 1.000000000000000000, 0.8660254037844387076, 1.000000000000000000, 0.8660254037844387076, 1.000000000000000000, 0.8660254037844387076, 1.000000000000000000, 0.8660254037844387076, 1.000000000000000000, 0.8660254037844387076, 1.000000000000000000, 0.8660254037844387076, 1.000000000000000000, 0.8660254037844387076, 1.000000000000000000, 0.8660254037844387076, 1.000000000000000000, 0.8660254037844387076, 1.000000000000000000, 0.8660254037844387076, 1.000000000000000000, 0.8660254037844387076, 1.000000000000000000, 0.8660254037844387076, 1.000000000000000000, 0.8660254037844387076, 1.000000000000000000, 0.8660254037844387076, 1.000000000000000000, 0.8660254037844387076, 1.000000000000000000, 0.8660254037844387076, 1.000000000000000000, 0.8660254037844387076, 1.000000000000000000, 0.8660254037844387076, 1.000000000000000000, 0.8660254037844387076, 1.000000000000000000, 0.8660254037844387076, 1.000000000000000000, 0.8660254037844387076, 1.000000000000000000, 0.8660254037844387076, 1.000000000000000000, 0.8660254037844387076, 1.000000000000000000, 0.8660254037844387076, 1.000000000000000000, 0.8660254037844387076, 1.000000000000000000, 0.8660254037844387076, 1.000000000000000000, 0.8660254037844387076, 1.000000000000000000, 0.8660254037844387076, 1.000000000000000000, 0.8660254037844387076, 1.000000000000000000, 0.8660254037844387076, 1.000000000000000000, 0.8660254037844387076, 1.000000000000000000, 0.8660254037844387076, 1.000000000000000000, 0.8660254037844387076, 1.000000000000000000, 0.8660254037844387076, 1.000000000000000000, 0.8660254037844387076, 1.000000000000000000, 0.8660254037844387076, 1.000000000000000000, 0.8660254037844387076, 1.000000000000000000, 0.8660254037844387076, 1.000000000000000000, 0.8660254037844387076, 1.000000000000000000, 0.8660254037844387076, 1.000000000000000000, 0.8660254037844387076, 1.000000000000000000, 0.8660254037844387076, 1.000000000000000000, 0.8660254037844387076, 1.000000000000000000, 0.8660254037844387076, 1.000000000000000000, 0.8660254037844387076, 1.000000000000000000, 0.8660254037844387076, 1.000000000000000000, 0.8660254037844387076, 1.000000000000000000, 0.8660254037844387076, 1.000000000000000000, 0.8660254037844387076, 1.000000000000000000, 0.8660254037844387076, 1.000000000000000000, 0.8660254037844387076, 1.000000000000000000, 0.8660254037844387076, 1.000000000000000000, 0.8660254037844387076, 1.000000000000000000, 0.8660254037844387076, 1.000000000000000000, 0.8660254037844387076, 1.000000000000000000, 0.8660254037844387076, 1.000000000000000000, 0.8660254037844387076, 1.000000000000000000, 0.8660254037844387076, 1.000000000000000000, 0.8660254037844387076, 1.000000000000000000, 0.8660254037844387076, 1.000000000000000000, 0.8660254037844387076, 1.000000000000000000, 0.8660254037844387076, 1.000000000000000000, 0.8660254037844387076, 1.000000000000000000, 0.8660254037844387076, 1.000000000000000000, 0.8660254037844387076, 1.000000000000000000, 0.8660254037844387076, 1.000000000000000000, 0.8660254037844387076, 1.000000000000000000, 0.8660254037844387076, 1.000000000000000000, 0.8660254037844387076, 1.000000000000000000, 0.8660254037844387076, 1.000000000000000000, 0.8660254037844387076, 1.000000000000000000, 0.8660254037844387076, 1.000000000000000000, 0.8660254037844387076, 1.000000000000000000, 0.8660254037844387076, 1.000000000000000000, 0.8660254037844387076, 1.000000000000000000, 0.8660254037844387076, 1.000000000000000000, 0.8660254037844387076, 1.000000000000000000, 0.8660254037844387076, 1.000000000000000000, 0.8660254037844387076, 1.000000000000000000, 0.8660254037844387076, 1.000000000000000000, 0.8660254037844387076, 1.000000000000000000, 0.8660254037844387076, 1.000000000000000000, 0.8660254037844387076, 1.000000000000000000, 0.8660254037844387076, 1.000000000000000000, 0.8660254037844387076, 1.000000000000000000, 0.8660254037844387076, 1.000000000000000000, 0.8660254037844387076, 1.000000000000000000, 0.8660254037844387076, 1.000000000000000000, 0.8660254037844387076, 1.000000000000000000, 0.8660254037844387076, 1.000000000000000000, 0.8660254037844387076, 1.000000000000000000, 0.8660254037844387076, 1.000000000000000000, 0.8660254037844387076, 1.000000000000000000, 0.8660254037844387076, 1.000000000000000000, 0.8660254037844387076, 1.000000000000000000, 0.8660254037844387076, 1.000000000000000000, 0.8660254037844387076, 1.000000000000000000, 0.8660254037844387076, 1.000000000000000000, 0.8660254037844387076, 1.000000000000000000, 0.8660254037844387076, 1.000000000000000000, 0.8660254037844387076, 1.000000000000000000, 0.8660254037844387076, 1.000000000000000000, 0.8660254037844387076, 1.000000000000000000, 0.8660254037844387076, 1.000000000000000000, 0.8660254037844387076, 1.000000000000000000, 0.8660254037844387076, 1.000000000000000000, 0.8660254037844387076, 1.000000000000000000, 0.8660254037844387076, 1.000000000000000000, 0.8660254037844387076, 1.000000000000000000, 0.8660254037844387076, 1.000000000000000000, 0.8660254037844387076, 1.000000000000000000, 0.8660254037844387076, 1.000000000000000000, 0.8660254037844387076, 1.000000000000000000, 0.8660254037844387076, 1.000000000000000000, 0.8660254037844387076, 1.000000000000000000, 0.8660254037844387076, 1.000000000000000000, 0.8660254037844387076, 1.000000000000000000, 0.8660254037844387076, 1.000000000000000000, 0.8660254037844387076, 1.000000000000000000, 0.8660254037844387076, 1.000000000000000000, 0.8660254037844387076, 1.000000000000000000, 0.8660254037844387076, 1.000000000000000000, 0.8660254037844387076, 1.000000000000000000, 0.8660254037844387076, 1.000000000000000000, 0.8660254037844387076, 1.000000000000000000, 0.8660254037844387076, 1.000000000000000000, 0.8660254037844387076, 1.000000000000000000, 0.8660254037844387076, 1.000000000000000000, 0.8660254037844387076, 1.000000000000000000, 0.8660254037844387076, 1.000000000000000000, 0.8660254037844387076, 1.000000000000000000, 0.8660254037844387076, 1.000000000000000000, 0.8660254037844387076, 1.000000000000000000, 0.8660254037844387076, 1.000000000000000000, 0.8660254037844387076, 1.000000000000000000, 0.8660254037844387076, 1.000000000000000000, 0.8660254037844387076, 1.000000000000000000, 0.8660254037844387076, 1.000000000000000000, 0.8660254037844387076, 1.000000000000000000, 0.8660254037844387076, 1.000000000000000000, 0.8660254037844387076, 1.000000000000000000, 0.8660254037844387076, 1.000000000000000000, 0.8660254037844387076, 1.000000000000000000, 0.8660254037844387076, 1.000000000000000000, 0.8660254037844387076, 1.000000000000000000, 0.8660254037844387076, 1.000000000000000000, 0.8660254037844387076, 1.000000000000000000, 0.8660254037844387076, 1.000000000000000000, 0.8660254037844387076, 1.000000000000000000) ) ) 
 REPRESENTATION_ITEM ( '' )  SURFACE ( )  );
#147942 = CARTESIAN_POINT ( 'NONE',  ( 1.411231479646192222, -1.713112901771263630, 1.333658509791965097 ) ) ;
#147943 = CARTESIAN_POINT ( 'NONE',  ( 0.02954982209854748257, -1.120125052174587577, -1.442194003765177257 ) ) ;
#147944 = CARTESIAN_POINT ( 'NONE',  ( 2.430995767774553062, -1.757534028733166442, 1.180493747047051567 ) ) ;
#147945 = CARTESIAN_POINT ( 'NONE',  ( 6.539320575229274901, 7.629137130509072051, 2.496737603865983424 ) ) ;
#147946 = VERTEX_POINT ( 'NONE', #154668 ) ;
#147948 = CARTESIAN_POINT ( 'NONE',  ( -1.364683531250014514, -0.4072916663252447167, 0.7879004041258379498 ) ) ;
#147947 = CARTESIAN_POINT ( 'NONE',  ( 2.349550187768103093, 0.6076851952682017499, -2.210314646808369421 ) ) ;
#147949 = CARTESIAN_POINT ( 'NONE',  ( -11.78331023100045627, 12.30000000000000071, -1.800000000000001155 ) ) ;
#147950 = CARTESIAN_POINT ( 'NONE',  ( 3.845709127770629010, 7.638411082374393146, 0.7998128361456321445 ) ) ;
#147951 = VECTOR ( 'NONE', #30353, 1000.000000000000000 ) ;
#147952 = CARTESIAN_POINT ( 'NONE',  ( 4.881579437514656838, 0.2187098293420664807, -2.210487333941961285 ) ) ;
#147953 = CARTESIAN_POINT ( 'NONE',  ( -6.222829318992474157, 10.20379193889247382, 0.000000000000000000 ) ) ;
#147954 = CARTESIAN_POINT ( 'NONE',  ( -1.127943160727153060, 3.300000000000025135, -0.7749999999999935829 ) ) ;
#147955 = CARTESIAN_POINT ( 'NONE',  ( 5.504247177468190699, 5.523969249908757817, 0.7216878364870317197 ) ) ;
#147956 = CARTESIAN_POINT ( 'NONE',  ( -6.182154857707119255, 10.15633840072622363, 0.000000000000000000 ) ) ;
#147957 = CARTESIAN_POINT ( 'NONE',  ( 4.909461021924254709, 5.860697626067345567, 1.082531754730549078 ) ) ;
#147958 = EDGE_LOOP ( 'NONE', ( #39871, #107125, #96736 ) ) ;
#147959 = CARTESIAN_POINT ( 'NONE',  ( 3.463517678199812266, -1.944071305346905643, -0.5350885120067662148 ) ) ;
#147961 = CARTESIAN_POINT ( 'NONE',  ( 0.8134211793521692879, -1.740389775365951186, -1.106656028277221537 ) ) ;
#147960 = CARTESIAN_POINT ( 'NONE',  ( 7.637320603199683866, 7.804628880021436288, -0.7998128361456281477 ) ) ;
#147962 = DIRECTION ( 'NONE',  ( -7.387867266669436732E-31, -1.000000000000000000, 8.546850786086437571E-32 ) ) ;
#147963 = CARTESIAN_POINT ( 'NONE',  ( 4.353576723319599218, 8.093273587265928271, -0.7216878364870357165 ) ) ;
#147965 = ADVANCED_FACE ( 'NONE', ( #168776 ), #151056, .T. ) ;
#147964 = CARTESIAN_POINT ( 'NONE',  ( -9.611339018008548507, -6.606549254265005722, 0.3046331935817704895 ) ) ;
#147966 = CARTESIAN_POINT ( 'NONE',  ( 0.6823417656249899377, 3.426041667008085323, -1.181850606188754593 ) ) ;
#147967 = CARTESIAN_POINT ( 'NONE',  ( 4.312563266315373234, 2.003113633248252867, 0.8892094534625747393 ) ) ;
#147968 = CARTESIAN_POINT ( 'NONE',  ( 2.830704105008190030, 0.7231396562890278767, -1.882474209725725434 ) ) ;
#147969 = CARTESIAN_POINT ( 'NONE',  ( 1.065666191918061445, -1.167978014494171823, 1.423405568861766168 ) ) ;
#147970 = ADVANCED_FACE ( 'NONE', ( #169842 ), #103792, .F. ) ;
#147971 = CARTESIAN_POINT ( 'NONE',  ( 7.039708073993665494, 9.236078724457858158, 1.599625672291281386 ) ) ;
#147972 =( LENGTH_UNIT ( ) NAMED_UNIT ( * ) SI_UNIT ( .MILLI., .METRE. ) );
#147973 = CARTESIAN_POINT ( 'NONE',  ( 5.456004705108882469, 1.823398332572896186, -0.09148835057352226741 ) ) ;
#147974 = CARTESIAN_POINT ( 'NONE',  ( 5.854138739207011888, 0.1455364397412381439, -2.011204036175239018 ) ) ;
#147975 = CARTESIAN_POINT ( 'NONE',  ( -6.855619230004478482, 11.14997286831390788, -0.7998128361456291469 ) ) ;
#147977 = CARTESIAN_POINT ( 'NONE',  ( -5.108390017298964914, 9.181815130149269422, 0.000000000000000000 ) ) ;
#147976 = CARTESIAN_POINT ( 'NONE',  ( 4.170984489290855635, -2.109804223432755865, -0.8175660662063081174 ) ) ;
#147978 = CARTESIAN_POINT ( 'NONE',  ( 1.102331697304242297, -2.106257354988652075, 0.001776637707836397316 ) ) ;
#147979 = CARTESIAN_POINT ( 'NONE',  ( -6.668631453075260396, 8.873432343378178544, -1.599625672291271394 ) ) ;
#147980 = CARTESIAN_POINT ( 'NONE',  ( 4.422371208857902580, 0.9731212702417373350, 1.827393648576709717 ) ) ;
#147981 = CARTESIAN_POINT ( 'NONE',  ( 8.540746701604824409, 12.05162268759261224, -1.199719254218446718 ) ) ;
#147982 = CARTESIAN_POINT ( 'NONE',  ( -15.75000000000000000, 11.29999999999999893, -1.800000000000001155 ) ) ;
#147983 =( NAMED_UNIT ( * ) SI_UNIT ( $, .STERADIAN. ) SOLID_ANGLE_UNIT ( ) );
#147984 = B_SPLINE_CURVE_WITH_KNOTS ( 'NONE', 3,
 ( #210947, #29026, #152109, #66547, #83891, #481, #182454, #117533, #199768, #183527, #45285, #184585, #149982, #95108, #178476, #34082, #200819, #132690, #133759, #161157, #151054, #198697, #116461, #50341, #127682, #99102, #84965, #177409, #82831, #19948, #61517, #33025, #101208, #168355, #100152, #165155, #12744, #111405, #78818, #144940, #62573, #46349, #167294, #35135, #166216, #16747, #18881, #17808, #128735, #1553, #2621, #118596, #67614, #52470, #51413, #194709, #68692, #36203, #102278, #212839, #126358, #161990, #110094, #45048, #112229, #64476, #144702, #211771, #176105, #14635, #164117, #28778, #98061, #163055, #193404, #129560, #192317, #97002, #62341, #13580, #208562, #179305, #31983, #160914, #111160, #27705, #15700, #142556, #43975, #60197, #94860, #180357, #46111, #93800, #159840, #143638, #11441, #195547, #77516, #78580, #209632, #145770, #130616, #12509, #61272, #127434, #113297, #177160, #210713, #47184, #128501, #194469, #178237, #29853, #95934, #79653, #63409, #30926, #80729, #146819, #196608, #48248, #114363, #131653, #50353, #51425, #49302, #53546, #148918, #167305, #100165, #1564, #199779, #117545, #132702, #152122, #116475, #182465, #68703, #169429, #197656, #82842, #67626, #69769, #16759, #33037, #134825, #133771, #183539, #115418, #34094, #201894, #166229, #165164, #184596, #81786, #492, #86046, #35145, #151068, #99115, #101221, #135875, #83903, #17819, #181410, #84976, #66560, #3692, #198708, #2630, #149993, #119678, #102293, #200829, #52480, #185665, #18892, #118608, #37294, #36214, #168367, #19962, #103367, #65506, #147869, #213884, #42662, #23155, #40517, #171558, #139083, #74070, #156395, #140163, #4755, #141248, #106619, #202973, #138013, #205110, #89269, #170490, #204028, #122918, #189943, #155319, #72980, #6903, #87111, #55676, #41592, #136947, #39431, #190996, #21013, #121832, #57814, #125040, #105524, #187803, #5832, #7981, #207257, #188876, #56753, #71904, #123976, #206186, #172648, #24224, #107704, #90326, #22074, #173730, #25307, #75139, #91409, #157469, #9064, #154258, #108771, #88186, #58885, #153181, #70830, #54614, #120762, #186740, #38362, #104441, #48000, #144452, #111981, #29597, #10121, #208316, #26372, #176907, #76196, #143376, #210455, #93541, #80471, #92485, #113044, #95683, #179050, #128252, #174796, #28522, #94612, #44796, #30669, #158524, #160655, #110901, #175854, #12253, #162802, #109840, #27443, #96752, #212588, #45860, #159585, #126102, #78330, #195295, #14379, #59946, #194215, #146570, #64227, #129319, #161737, #62093, #177982, #130369, #13328, #79402, #11183, #196359, #142305, #145519, #192062, #43725, #77262, #211518, #63154, #209375, #46926, #61019, #127178, #193146, #102055, #49049, #65261, #167060, #99924, #17571, #115169, #131408, #33843, #134589, #184353, #213635, #133523, #118364, #35975, #68461, #100971, #83655, #1322, #168121, #116229, #50108, #147617, #117296, #181164, #19722, #197408, #32788, #85801, #183293, #199530, #98864, #81535, #135631, #182220, #51173, #165985, #149745, #18652, #34898, #84731, #97807, #151881, #150820, #164916, #16509, #3455, #67383, #2383, #82591, #200589, #201651, #246, #69524, #52237, #148678, #114118, #163870, #180110, #31734, #15446, #66318, #132462, #198464, #41347, #139912, #152934, #140999, #157217, #169180, #53301, #5576 ),
 .UNSPECIFIED., .F., .F.,
 ( 4, 1, 1, 1, 1, 1, 1, 1, 1, 1, 1, 1, 1, 1, 1, 1, 1, 1, 1, 1, 1, 1, 1, 1, 1, 1, 1, 1, 1, 1, 1, 1, 1, 1, 1, 1, 1, 1, 1, 1, 1, 1, 1, 1, 1, 1, 1, 1, 1, 1, 1, 1, 1, 1, 1, 1, 1, 1, 1, 1, 1, 1, 1, 1, 1, 1, 1, 1, 1, 1, 1, 1, 1, 1, 1, 1, 1, 1, 1, 1, 1, 1, 1, 1, 1, 1, 1, 1, 1, 1, 1, 1, 1, 1, 1, 1, 1, 1, 1, 1, 1, 1, 1, 1, 1, 1, 1, 1, 1, 1, 1, 1, 1, 1, 1, 1, 1, 1, 1, 1, 1, 1, 1, 1, 1, 1, 1, 1, 1, 1, 1, 1, 1, 1, 1, 1, 1, 1, 1, 1, 1, 1, 1, 1, 1, 1, 1, 1, 1, 1, 1, 1, 1, 1, 1, 1, 1, 1, 1, 1, 1, 1, 1, 1, 1, 1, 1, 1, 1, 1, 1, 1, 1, 1, 1, 1, 1, 1, 1, 1, 1, 1, 1, 1, 1, 1, 1, 1, 1, 1, 1, 1, 1, 1, 1, 1, 1, 1, 1, 1, 1, 1, 1, 1, 1, 1, 1, 1, 1, 1, 1, 1, 1, 1, 1, 1, 1, 1, 1, 1, 1, 1, 1, 1, 1, 1, 1, 1, 1, 1, 1, 1, 1, 1, 1, 1, 1, 1, 1, 1, 1, 1, 1, 1, 1, 1, 1, 1, 1, 1, 1, 1, 1, 1, 1, 1, 1, 1, 1, 1, 1, 1, 1, 1, 1, 1, 1, 1, 1, 1, 1, 1, 1, 1, 1, 1, 1, 1, 1, 1, 1, 1, 1, 1, 1, 1, 1, 1, 1, 1, 1, 1, 1, 1, 1, 1, 1, 1, 1, 1, 1, 1, 1, 1, 1, 1, 1, 1, 1, 1, 1, 1, 1, 1, 1, 1, 1, 1, 1, 1, 1, 1, 1, 1, 1, 1, 1, 1, 1, 1, 1, 1, 1, 1, 1, 1, 1, 1, 1, 1, 1, 1, 1, 1, 1, 1, 1, 1, 1, 1, 1, 1, 1, 1, 1, 1, 1, 1, 1, 1, 1, 1, 1, 1, 1, 1, 1, 1, 1, 1, 1, 1, 1, 1, 1, 1, 1, 1, 1, 1, 1, 1, 1, 1, 4 ),
 ( 0.000000000000000000, 0.002599909708945224215, 0.005208776875251038344, 0.007813105021672143990, 0.01041684075506122895, 0.01302033053878596733, 0.01562516449037322508, 0.01822901888718816976, 0.02083333248856494152, 0.02343767784666880849, 0.02604151204071371642, 0.02864616705684025488, 0.03124974664057501156, 0.03385445107693609706, 0.03645811663825353210, 0.03906264587105176544, 0.04166673705245293319, 0.04427082116499847508, 0.04687535697974040683, 0.04947901875943551409, 0.05208372524935509645, 0.05468730636643894666, 0.05729195276349181160, 0.05989578571700067411, 0.06250012971910297310, 0.06510448174046053194, 0.06770830932160050442, 0.07031296016926287529, 0.07291653972921435800, 0.07552124384959360559, 0.07812490789241745281, 0.08072943556986492131, 0.08333352577934262373, 0.08593760861062926804, 0.08854214333088818167, 0.09114580385899402615, 0.09375050919907033931, 0.09635408915385039463, 0.09895873428887830281, 0.1015625661591952889, 0.1041669088510773916, 0.1067712598504420435, 0.1093750861808121810, 0.1119797359579501050, 0.1145833143474069837, 0.1171880172914337714, 0.1197916802446672702, 0.1223962066585842084, 0.1250002958591681090, 0.1276043774339237491, 0.1302089111537957367, 0.1328125705047451810, 0.1354172747579587832, 0.1380208536162275679, 0.1406254975582941213, 0.1432293284131295197, 0.1458336698625422867, 0.1484380199076493767, 0.1510418450546419100, 0.1536464938294531402, 0.1562500711155297428, 0.1588547729514310503, 0.1614584348822658832, 0.1640629601007041471, 0.1666670483599762276, 0.1692711287458052438, 0.1718756615333107141, 0.1744793197742946778, 0.1770840230088624179, 0.1796876008377196188, 0.1822922436549848091, 0.1848960735616705098, 0.1875004138364584350, 0.1901047629951247708, 0.1927085870260826783, 0.1953132348667029061, 0.1979168111164897881, 0.2005215119124719170, 0.2031251728880697216, 0.2057296969790492203, 0.2083337843645647058, 0.2109378636290424602, 0.2135423955521746908, 0.2161460527503557827, 0.2187507550344668650, 0.2213543319009846355, 0.2239589736615800464, 0.2265628026874214052, 0.2291671418554001027, 0.2317714901954165685, 0.2343753131776551424, 0.2369799601521939414, 0.2395835354327550959, 0.2421882352569974250, 0.2447918953444941648, 0.2473964183760076208, 0.2500005049552969649, 0.2526045831659717300, 0.2552091142926994904, 0.2578127705152143956, 0.2604174719170327390, 0.2630210478882585856, 0.2656256886602897938, 0.2682295168725681855, 0.2708338550015275126, 0.2734382025906618163, 0.2760420245914711468, 0.2786466707680146371, 0.2812502451463897990, 0.2838549440670474211, 0.2864586033335557724, 0.2890631253735708728, 0.2916672112141422968, 0.2942712884385379479, 0.2968758188368077477, 0.2994794741507696423, 0.3020841747384366283, 0.3046877498813952978, 0.3072923897329448151, 0.3098962171989202430, 0.3125005543566263810, 0.3151049012626256918, 0.3177087223492732204, 0.3203133677958864278, 0.3229169413390938770, 0.3255216394243000688, 0.3281252979369121969, 0.3307298190533745630, 0.3333339042227165261, 0.3359379805283350118, 0.3385425102660742369, 0.3411461647385755636, 0.3437508645802123675, 0.3463544389619092612, 0.3489590779610384774, 0.3515629047479519320, 0.3541672410021501904, 0.3567715872927431642, 0.3593754075324762653, 0.3619800523172059803, 0.3645836250922447341, 0.3671883224101137877, 0.3697919802359038166, 0.3723965004967392245, 0.3750005850623230885, 0.3776046605166471504, 0.3802091896617659783, 0.3828128433598806946, 0.3854175425235913388, 0.3880211162110140388, 0.3906257544257662473, 0.3932295806008425099, 0.3958339160192597128, 0.3984382617621595180, 0.4010420812222079689, 0.4036467254130849946, 0.4062502974869375283, 0.4088549941055670267, 0.4114586513115932598, 0.4140631707847102772, 0.4166672548139925825, 0.4192713294844879757, 0.4218758581048823730, 0.4244795110956688933, 0.4270842096495421902, 0.4296877827096635682, 0.4322924202080664635, 0.4348962458385162155, 0.4375005804888632555, 0.4401049257517701263, 0.4427087444993486054, 0.4453133881643903114, 0.4479169596040251111, 0.4505216555914985932, 0.4531253122448062887, 0.4557298309980991058, 0.4583339145585244578, 0.4609379885126426157, 0.4635425166761967808, 0.4661461690266998081, 0.4687508670388120247, 0.4713544395385928509, 0.4739590763886608604, 0.4765629015416836811, 0.4791672354916582388, 0.4817715803422617515, 0.4843753984445725025, 0.4869800416517858221, 0.4895836125241597725, 0.4921883079485492862, 0.4947919641161733773, 0.4973964822175238609, 0.5000005653765271507, 0.5026046386817077938, 0.5052091664562964324, 0.5078128182335502894, 0.5104175157719683664, 0.5130210877783591972, 0.5156257240480961457, 0.5182295487908826770, 0.5208338821081714975, 0.5234382266141532902, 0.5260420441383883983, 0.5286466869557716608, 0.5312502573278325979, 0.5338549522572011430, 0.5364586080061681805, 0.5390631255234488162, 0.5416672083484578293, 0.5442712810721315186, 0.5468758085256230084, 0.5494794597966533578, 0.5520841569294364648, 0.5546877285093810839, 0.5572923642667827471, 0.5598961886665174692, 0.5625005214187991376, 0.5651048656478350196, 0.5677086826611791315, 0.5703133251567252815, 0.5729168950954143247, 0.5755215895978186280, 0.5781252449951498340, 0.5807297619962258350, 0.5833338445546641937, 0.5859379167642547737, 0.5885424439645127181, 0.5911460947963396162, 0.5937507915915425372, 0.5963543628119793993, 0.5989589981250363904, 0.6015628222488997867, 0.6041671545038470592, 0.6067714985236103420, 0.6093753150932430529, 0.6119799573349418154, 0.6145835269071964202, 0.6171882210506893784, 0.6197918761634028106, 0.6223963927161352272, 0.6250004750754242222, 0.6276045468383509851, 0.6302090738532378777, 0.6328127243128783830, 0.6354174208385534595, 0.6380209917664191321, 0.6406256267031188445, 0.6432294506182901772, 0.6458337824435727015, 0.6484381263217364744, 0.6510419425148348260, 0.6536465845706755928, 0.6562501538434313275, 0.6588548476960643940, 0.6614585025911776661, 0.6640630187634258830, 0.6666671009909873602, 0.6692711723746683772, 0.6718756992720475996, 0.6744793494265174383, 0.6770840457507175669, 0.6796876164529486175, 0.6822922510812780006, 0.6848960748549377531, 0.6875004063182246217, 0.6901047501224634173, 0.6927085660062048955, 0.6953132079441787239, 0.6979167769843723779, 0.7005214706141982273, 0.7031251253587310623, 0.7057296412183544643, 0.7083337233816132672, 0.7109377944534676086, 0.7135423213012055399, 0.7161459712175226588, 0.7187506674083037339, 0.7213542379518396164, 0.7239588723397878400, 0.7265626960391206035, 0.7291670272080824633, 0.7317713710060759214, 0.7343751866476402324, 0.7369798285357428425, 0.7395833974103146469, 0.7421880908853900616, 0.7447917455463664016, 0.7473962611612280371, 0.7500003433276148934, 0.7526044141550642941, 0.7552089410210337528, 0.7578125907662203176, 0.7604172868916432293, 0.7630208573434285046, 0.7656254915589897347, 0.7682293152511859846, 0.7708336461934980344, 0.7734379900529331220, 0.7760418055195050790, 0.7786464474257392965, 0.7812500162016354777, 0.7838547095900232353, 0.7864583642344741277, 0.7890628796724428184, 0.7916669619093961163, 0.7942710325598689725, 0.7968755595119511037, 0.7994792091530360523, 0.8020839052811703507, 0.8046874757081575735, 0.8072921098193328593, 0.8098959335715922858, 0.8125002643549369408, 0.8151046083435100620, 0.8177084237022821389, 0.8203130656946604482, 0.8229166344388356702, 0.8255213278086077633, 0.8281249825035741363, 0.8307294978325265866, 0.8333335802074958165, 0.8359376507484286289, 0.8385421778545157911, 0.8411458274585372763, 0.8437505236574627254, 0.8463540941266142204, 0.8489587282014147140, 0.8515625520809478877, 0.8541668827730166669, 0.8567712269584367712, 0.8593750422766117669, 0.8619796844231587540, 0.8645832532025788941, 0.8671879466218186394, 0.8697916014343529678, 0.8723961167221769841, 0.8750001993026245151, 0.8776042698014647758, 0.8802087971294628721, 0.8828124467634709260, 0.8854171431012803906, 0.8880207136795719158, 0.8906253477860208712, 0.8932291718600525732, 0.8958335025285494302, 0.8984378469785403443, 0.9010416623233333810, 0.9036463046920883979, 0.9062498735737328781, 0.9088545671105374701, 0.9114582221077071056, 0.9140627374223044832, 0.9166668202757080053, 0.9192708907999164181, 0.9218754184177497812, 0.9244790681488107564, 0.9270837646936044285, 0.9296873354480212903, 0.9322919696541906998, 0.9348957939899811276, 0.9375001247025137596, 0.9401044694846933947, 0.9427082849236875228, 0.9453129275835465695, 0.9479164966330613229, 0.9505211903504858784, 0.9531248456066239161, 0.9557293610412391782, 0.9583334441921064206, 0.9609375147049603605, 0.9635420428945489224, 0.9661456931510739032, 0.9687503890924937799, 0.9713539588735070618, 0.9739585961357111188, 0.9765624261165479769, 0.9791667493207181217, 0.9817710620974646751, 0.9843748983037424738, 0.9869797303524157073, 0.9895832060093603388, 0.9921869237806116848, 0.9947912468131487884, 0.9974000922265050528, 0.9999999999999998890 ),
 .UNSPECIFIED. ) ;
#147985 = CARTESIAN_POINT ( 'NONE',  ( -6.842061076390810292, 11.13415502243129218, 0.000000000000000000 ) ) ;
#147986 = CARTESIAN_POINT ( 'NONE',  ( 0.4410926847035671616, 6.460511719969816546, 3.247348959959607484 ) ) ;
#147987 = CARTESIAN_POINT ( 'NONE',  ( 7.038618024149998043, 8.240751112043669835, -1.199719254218452047 ) ) ;
#147988 = CARTESIAN_POINT ( 'NONE',  ( 5.688518940989607309, 6.102662425301288884, -0.7322136710279708582 ) ) ;
#147989 = CARTESIAN_POINT ( 'NONE',  ( -3.735435015764967837, 4.316761258935923884, -1.199719254218452047 ) ) ;
#147991 = CARTESIAN_POINT ( 'NONE',  ( 1.705654399339423311, 1.929789488239462836, -1.100201954495036549 ) ) ;
#147990 = CARTESIAN_POINT ( 'NONE',  ( 1.230900525853476868, 1.420129835883350955, -1.575055732827963295 ) ) ;
#147992 = CARTESIAN_POINT ( 'NONE',  ( 3.264161633363777959, 6.412690354096299394, -0.9273118095389889515 ) ) ;
#147993 = CARTESIAN_POINT ( 'NONE',  ( -6.831329296439251131, 9.063246493969506545, -1.599625672291271394 ) ) ;
#147994 = CARTESIAN_POINT ( 'NONE',  ( 4.774442650306744085, 8.721933525333202653, -0.7998128361456281477 ) ) ;
#147995 = CARTESIAN_POINT ( 'NONE',  ( 3.631260574587381829, 0.05062604155347744800, -1.961386756325018021 ) ) ;
#147996 = CARTESIAN_POINT ( 'NONE',  ( 6.145923705696426431, 6.064665832934283962, 0.7998128361456341429 ) ) ;
#147997 = CARTESIAN_POINT ( 'NONE',  ( -4.117634752470962667, 7.483002602015099924, 0.6335975934644126895 ) ) ;
#147998 = CARTESIAN_POINT ( 'NONE',  ( 4.521807925357579805, 5.234196320127330715, -1.199719254218452047 ) ) ;
#147999 = CARTESIAN_POINT ( 'NONE',  ( -4.312902262922974295, 8.045820050136510915, 0.7216878364870338292 ) ) ;
#148000 = CARTESIAN_POINT ( 'NONE',  ( -7.727784370109414880, 8.118095974656867497, 0.7216878364870578100 ) ) ;
#148001 = CARTESIAN_POINT ( 'NONE',  ( 1.986737319265439394, -1.300789755646198476, 1.674730562594067829 ) ) ;
#148002 = CARTESIAN_POINT ( 'NONE',  ( -5.315678745009726924, 8.359319748223434487, -1.199719254218453823 ) ) ;
#148003 = CARTESIAN_POINT ( 'NONE',  ( 5.828557447170540584, -1.245780601409246957, 1.515539014345569147 ) ) ;
#148004 = CARTESIAN_POINT ( 'NONE',  ( 3.256853613824191029, -1.637998819981079990, 1.410756932016984377 ) ) ;
#148005 = CARTESIAN_POINT ( 'NONE',  ( 3.016969003575611818, -1.773741936391802332, 0.4936923545346691977 ) ) ;
#148006 = CARTESIAN_POINT ( 'NONE',  ( -4.160056744896282410, 7.428205994021240599, -0.7369721661574859528 ) ) ;
#148007 = CARTESIAN_POINT ( 'NONE',  ( -1.402160292154681736E-14, -0.6156249996585817508, 1.575800808251672791 ) ) ;
#148008 = CARTESIAN_POINT ( 'NONE',  ( 4.154071219024037198, -1.287471232310585467, 1.171156097612672253 ) ) ;
#148009 = CARTESIAN_POINT ( 'NONE',  ( 0.05368761658891522265, 14.48153887695537456, 11.99990993953711893 ) ) ;
#148010 = CARTESIAN_POINT ( 'NONE',  ( 4.528060117284240071, 5.345453560662148718, 1.082531754730560403 ) ) ;
#148011 = FACE_OUTER_BOUND ( 'NONE', #8482, .T. ) ;
#148012 = CARTESIAN_POINT ( 'NONE',  ( 1.428841412761387986, 2.083414371474631377, 0.5762002773818803991 ) ) ;
#148013 = CARTESIAN_POINT ( 'NONE',  ( 4.657577273293715514, -0.4389639308803178208, -1.967586094827819654 ) ) ;
#148014 = CARTESIAN_POINT ( 'NONE',  ( -8.473482818416664841, 11.86918514058604757, -1.082531754730543083 ) ) ;
#148015 = CARTESIAN_POINT ( 'NONE',  ( 1.288190726105652217, -0.9714702286227733241, 1.931199087792371261 ) ) ;
#148016 = CARTESIAN_POINT ( 'NONE',  ( 2.301971997355524824, -1.971002988154029412, 0.04462483508816358219 ) ) ;
#148017 = CARTESIAN_POINT ( 'NONE',  ( -6.544399909239620783, 6.796922107324852469, 0.5836599600529659426 ) ) ;
#148018 = CARTESIAN_POINT ( 'NONE',  ( 3.421366544187495418, -1.159031000169882475, -1.558129983894075865 ) ) ;
#148021 = ORIENTED_EDGE ( 'NONE', *, *, #71393, .F. ) ;
#148020 = CARTESIAN_POINT ( 'NONE',  ( -3.634994582239682526, 6.294558541704648569, 1.082531754730549967 ) ) ;
#148019 = CARTESIAN_POINT ( 'NONE',  ( -10.58855478214856660, 11.45566145536924552, -0.7216878364870217277 ) ) ;
#148022 = CARTESIAN_POINT ( 'NONE',  ( -7.095713291905736853, 9.371694488680407886, 1.599625672291269396 ) ) ;
#148023 = CARTESIAN_POINT ( 'NONE',  ( 3.410758162289653672, 6.136912401716668519, -1.199719254218453823 ) ) ;
#148025 = ORIENTED_EDGE ( 'NONE', *, *, #145457, .F. ) ;
#148024 = CARTESIAN_POINT ( 'NONE',  ( -4.932134020321308654, 8.976183133675331050, 0.7998128361456291469 ) ) ;
#148026 = CARTESIAN_POINT ( 'NONE',  ( -8.134528978075012517, 12.43410820782212767, 1.040834085586084257E-14 ) ) ;
#148027 = CARTESIAN_POINT ( 'NONE',  ( 1.343116161061377545, 0.4315099961175078436, 2.164003993775004187 ) ) ;
#148028 = CARTESIAN_POINT ( 'NONE',  ( 0.000000000000000000, -3.346874999522042149, -3.793834371823813001 ) ) ;
#148029 = CARTESIAN_POINT ( 'NONE',  ( 5.541838416980684023, 1.314774629379747539, 1.456173869884537675 ) ) ;
#148030 = CARTESIAN_POINT ( 'NONE',  ( 3.802059961758995854, -1.092030603714509551, -1.813900157284773496 ) ) ;
#148031 = CARTESIAN_POINT ( 'NONE',  ( -0.7500000000000215383, 2.472916667349486897, 1.299038105676671107 ) ) ;
#148032 = CARTESIAN_POINT ( 'NONE',  ( 0.1747926744264451659, 0.2546335194838904581, -1.890750172325323275 ) ) ;
#148033 = CARTESIAN_POINT ( 'NONE',  ( 4.681507052731401330, -0.8653998779965512700, 1.625073734443114759 ) ) ;
#148034 = EDGE_LOOP ( 'NONE', ( #157548, #125448, #150604, #119919 ) ) ;
#148035 = ADVANCED_FACE ( 'NONE', ( #187154 ), #104864, .F. ) ;
#148036 = UNCERTAINTY_MEASURE_WITH_UNIT (LENGTH_MEASURE( 1.000000000000000082E-05 ), #49298, 'distance_accuracy_value', 'NONE');
#148037 = CARTESIAN_POINT ( 'NONE',  ( -7.147119532698295252, 11.49005655479003174, 0.000000000000000000 ) ) ;
#148038 = CARTESIAN_POINT ( 'NONE',  ( -1.235837185320847853, 1.391320699396851395E-14, 0.2124088322884870594 ) ) ;
#148039 = CARTESIAN_POINT ( 'NONE',  ( 5.590118541908202232, 1.264772504208915072, 1.701965355810124203 ) ) ;
#148040 = CARTESIAN_POINT ( 'NONE',  ( 6.636879889089462026, 7.701780277814560982, -1.199719254218446718 ) ) ;
#148041 = VERTEX_POINT ( 'NONE', #73400 ) ;
#148042 = CARTESIAN_POINT ( 'NONE',  ( 6.538362368396775537, 2.037695317216736246, 0.3068575337649599444 ) ) ;
#148045 = CARTESIAN_POINT ( 'NONE',  ( 3.122423488780329492, 0.04808623196613136253, 1.840796284283818585 ) ) ;
#148044 = CARTESIAN_POINT ( 'NONE',  ( 0.8185401059354965314, -1.351722143400556631, 1.279475349031534259 ) ) ;
#148043 = CARTESIAN_POINT ( 'NONE',  ( 6.773846765307987461, -7.473374494058229622, 6.773846765307971474 ) ) ;
#148046 = CARTESIAN_POINT ( 'NONE',  ( 7.086107841436786181, 11.41887624831828418, 1.040834085586084257E-14 ) ) ;
#148047 = CARTESIAN_POINT ( 'NONE',  ( -10.87634538855766841, 3.956598013261175772, 3.867819554622464739 ) ) ;
#148048 = CARTESIAN_POINT ( 'NONE',  ( -7.391130018105325661, 8.652015104991543026, -1.199719254218452047 ) ) ;
#148049 = CARTESIAN_POINT ( 'NONE',  ( -0.1899713450103351353, -8.048696291100961631, -9.532262708098288684 ) ) ;
#148050 = EDGE_CURVE ( 'NONE', #103686, #13123, #161418, .T. ) ;
#148051 = CIRCLE ( 'NONE', #203357, 0.07999999999999998779 ) ;
#148052 = CARTESIAN_POINT ( 'NONE',  ( 2.983271218942393332, -0.1628219013674602478, -2.200934326520533446 ) ) ;
#148053 = CARTESIAN_POINT ( 'NONE',  ( 4.464347054923422320, 1.061364745222750372, 1.997979292561928633 ) ) ;
#148054 = CARTESIAN_POINT ( 'NONE',  ( -7.551528373131759508, 7.912463978182924684, 1.040834085586084257E-14 ) ) ;
#148055 = CARTESIAN_POINT ( 'NONE',  ( 4.218897050542698146, 1.396175630728054173, -1.154312599804697914 ) ) ;
#148056 = CARTESIAN_POINT ( 'NONE',  ( 5.471877088563796399, -0.8550440501978623375, 1.714365851762880144 ) ) ;
#148057 = CARTESIAN_POINT ( 'NONE',  ( 1.364683531249992088, 5.696875000341418804, 1.214306433183764966E-14 ) ) ;
#148058 = CARTESIAN_POINT ( 'NONE',  ( 5.717618200960680852, -1.824738551054584379, 0.4112096411929695439 ) ) ;
#148059 = CARTESIAN_POINT ( 'NONE',  ( 5.582414374887135544, 1.108435676577405937, -1.494769603722338802 ) ) ;
#148060 = DIRECTION ( 'NONE',  ( 0.000000000000000000, -1.000000000000000000, 0.000000000000000000 ) ) ;
#148061 = CARTESIAN_POINT ( 'NONE',  ( 0.1099206271272800961, -0.7955684105149689600, -1.691499381818922343 ) ) ;
#148063 = CIRCLE ( 'NONE', #206785, 10.91999999999999105 ) ;
#148062 = PRESENTATION_LAYER_ASSIGNMENT (  '', '', ( #137711 ) ) ;
#148064 = CARTESIAN_POINT ( 'NONE',  ( 1.446500318503377125, -1.422605717829699801, 1.429450658469958668 ) ) ;
#148066 = CARTESIAN_POINT ( 'NONE',  ( 3.229229631591294503, 0.05193219833012594627, 2.105601595880735033 ) ) ;
#148065 = CARTESIAN_POINT ( 'NONE',  ( -3.375617059678305054, 5.921675088724528635, 1.082531754730560403 ) ) ;
#148067 = CARTESIAN_POINT ( 'NONE',  ( 8.048736748007069508, 12.54194330598362406, -0.7998128361456352531 ) ) ;
#148069 = CARTESIAN_POINT ( 'NONE',  ( -9.504429378379839477, 11.04725468198666150, 1.199719254218462483 ) ) ;
#148068 = CARTESIAN_POINT ( 'NONE',  ( 1.499999999999996891, 11.92708333401613174, -0.8660254037844378194 ) ) ;
#148070 = DIRECTION ( 'NONE',  ( 0.000000000000000000, -0.000000000000000000, 1.000000000000000000 ) ) ;
#148071 = CARTESIAN_POINT ( 'NONE',  ( 1.635027243301078848, 1.886126948880119780, 0.7230602950082564151 ) ) ;
#148072 = CARTESIAN_POINT ( 'NONE',  ( -0.6823417656250003738, 1.967708333674753174, -1.181850606188749264 ) ) ;
#148073 = CARTESIAN_POINT ( 'NONE',  ( 3.011882680530176604, 6.665613560593854459, 0.7998128361456341429 ) ) ;
#148074 = CARTESIAN_POINT ( 'NONE',  ( 2.882270108570818223, -1.113908571083363164, 1.852364028112465810 ) ) ;
#148075 = CARTESIAN_POINT ( 'NONE',  ( 6.610000000000006537, 7.629137130509094256, 2.600000000000001421 ) ) ;
#148078 = CARTESIAN_POINT ( 'NONE',  ( -15.75000000000000000, 10.19999999999999929, 1.099999999999996758 ) ) ;
#148077 = CARTESIAN_POINT ( 'NONE',  ( 11.96209379583854115, 9.772070594057634452, -0.9572398070798752157 ) ) ;
#148076 = CARTESIAN_POINT ( 'NONE',  ( 3.464990776744291345, 6.200183785247111778, 1.199719254218452047 ) ) ;
#148079 = CARTESIAN_POINT ( 'NONE',  ( 7.904040366642678173, 12.16520482781775137, 0.7216878364870438212 ) ) ;
#148080 = CARTESIAN_POINT ( 'NONE',  ( -2.280006499904862149, 5.600973625046616000, -0.2919740144436631102 ) ) ;
#148081 = CARTESIAN_POINT ( 'NONE',  ( -6.561783159334130922, 9.638868871656395498, -1.082531754730538864 ) ) ;
#148082 = CARTESIAN_POINT ( 'NONE',  ( 1.364683531249986537, 0.8635416670080893198, 0.7879004041258500513 ) ) ;
#148083 = CARTESIAN_POINT ( 'NONE',  ( 1.118978350340808614, -0.04878210919301298465, 2.191179638975069732 ) ) ;
#148084 = CARTESIAN_POINT ( 'NONE',  ( 0.4782691259469203371, 7.503280781840964586, 1.943353214563591003 ) ) ;
#148085 = CARTESIAN_POINT ( 'NONE',  ( 0.9192595896337816264, 2.091463038127399532, 0.8634530567685079205 ) ) ;
#148086 = CARTESIAN_POINT ( 'NONE',  ( -8.616370316684697883, 10.01118577667568132, -1.199719254218446718 ) ) ;
#148087 = CARTESIAN_POINT ( 'NONE',  ( -4.487385655998893164, 6.258369236797239665, 1.443375672974064550 ) ) ;
#148088 = CARTESIAN_POINT ( 'NONE',  ( -1.201851678989727383E-14, 3.509375000341421469, -1.575800808251660134 ) ) ;
#148089 = CARTESIAN_POINT ( 'NONE',  ( 4.620579464570812256, 8.341333509328540785, -0.3192730525469981151 ) ) ;
#148090 = EDGE_CURVE ( 'NONE', #138779, #79641, #116463, .T. ) ;
#148091 = CARTESIAN_POINT ( 'NONE',  ( -0.7500000000000006661, 11.20833333333333393, -1.299038105676657340 ) ) ;
#148092 = CARTESIAN_POINT ( 'NONE',  ( 4.415115299905642665, 5.179997933758551554, -1.199719254218450271 ) ) ;
#148093 = CARTESIAN_POINT ( 'NONE',  ( 3.057584390254026729, 1.761565543986362670, -0.1695560061622681525 ) ) ;
#148094 = AXIS2_PLACEMENT_3D ( 'NONE', #71379, #72454, #56227 ) ;
#148095 = CARTESIAN_POINT ( 'NONE',  ( 9.748476143425788720, 11.33197590787365172, -1.199719254218440723 ) ) ;
#148096 = CARTESIAN_POINT ( 'NONE',  ( 6.581111309608331794, -0.1016299978719436697, -2.204559905201553427 ) ) ;
#148097 = CARTESIAN_POINT ( 'NONE',  ( -1.364683531250000748, 8.859375000341396245, 0.000000000000000000 ) ) ;
#148098 = ORIENTED_EDGE ( 'NONE', *, *, #152381, .F. ) ;
#148099 = CARTESIAN_POINT ( 'NONE',  ( -5.424143973919053785, 8.485862515284315677, 1.199719254218454489 ) ) ;
#148100 = CARTESIAN_POINT ( 'NONE',  ( 5.431267612114304200, -1.591330327768199382, -1.238307421737715019 ) ) ;
#148101 = ORIENTED_EDGE ( 'NONE', *, *, #204535, .F. ) ;
#148103 = ADVANCED_FACE ( 'NONE', ( #209793 ), #42009, .T. ) ;
#148102 = AXIS2_PLACEMENT_3D ( 'NONE', #78056, #62866, #173455 ) ;
#148104 = CARTESIAN_POINT ( 'NONE',  ( 2.360033908006432757, 0.7977434165707707470, 1.692156362554583460 ) ) ;
#148105 = CARTESIAN_POINT ( 'NONE',  ( 3.537997267176114846, 1.309675639058418550, 1.603382541711120490 ) ) ;
#148106 = CARTESIAN_POINT ( 'NONE',  ( -6.983858524370814003, 9.241197259889665006, 1.443375672974064550 ) ) ;
#148107 = CARTESIAN_POINT ( 'NONE',  ( 1.546972149855216472, 0.1906517044060058730, 1.902890584052991940 ) ) ;
#148108 = CARTESIAN_POINT ( 'NONE',  ( -0.5727794709109862437, 3.454100923638389720, 0.3117576387476111432 ) ) ;
#148109 = CARTESIAN_POINT ( 'NONE',  ( -9.813523197712067159, 5.212597839642568509, -6.298667959258508198 ) ) ;
#148110 = DIRECTION ( 'NONE',  ( 1.214306433183764966E-17, 1.000000000000000000, 5.200010849845536803E-32 ) ) ;
#148111 = CARTESIAN_POINT ( 'NONE',  ( -1.364683531250010295, 4.842708333674756283, 0.7879004041258379498 ) ) ;
#148112 = CARTESIAN_POINT ( 'NONE',  ( 0.8614045922798493349, -1.509235727096858826, -1.174430983434851195 ) ) ;
#148113 = CARTESIAN_POINT ( 'NONE',  ( 3.156644782993088150, -0.5669402238272451822, -1.878178299617596192 ) ) ;
#148114 = CARTESIAN_POINT ( 'NONE',  ( 0.3157796101352361440, -1.620936768121715499, 1.198674607299075934 ) ) ;
#148115 = EDGE_CURVE ( 'NONE', #167173, #11923, #112382, .T. ) ;
#148116 = CARTESIAN_POINT ( 'NONE',  ( -4.797606254389363833, 6.690569611577942943, 1.599625672291263179 ) ) ;
#148118 = CARTESIAN_POINT ( 'NONE',  ( 10.96785329849812562, -5.223431457505089526, -0.4373225248172959434 ) ) ;
#148117 = CARTESIAN_POINT ( 'NONE',  ( 10.07100917685271035, 10.64393221595000938, 0.7998128361456462443 ) ) ;
#148119 =( BOUNDED_SURFACE ( )  B_SPLINE_SURFACE ( 3, 2, ( 
 ( #29147, #96300, #11813 ),
 ( #211072, #176465, #60569 ),
 ( #13935, #178606, #126728 ),
 ( #64833, #196970, #77889 ),
 ( #142934, #94172, #98412 ),
 ( #47554, #32346, #146121 ),
 ( #144010, #95236, #161285 ),
 ( #46471, #129929, #208935 ),
 ( #145069, #210002, #63770 ),
 ( #147178, #112594, #163422 ),
 ( #61644, #162355, #164476 ),
 ( #127812, #62695, #113665 ),
 ( #76815, #213204, #128856 ),
 ( #130979, #48607, #45412 ) ),
 .UNSPECIFIED., .F., .F., .T. ) 
 B_SPLINE_SURFACE_WITH_KNOTS ( ( 4, 2, 2, 2, 2, 2, 4 ),
 ( 3, 3 ),
 ( 0.001912008033049058262, 0.002390010041311322556, 0.002629011045442455029, 0.002868012049573587068, 0.003346014057835851145, 0.003585015061966983184, 0.003824016066098115656 ),
 ( 0.000000000000000000, 1.000000000000000000 ),
 .UNSPECIFIED. ) 
 GEOMETRIC_REPRESENTATION_ITEM ( )  RATIONAL_B_SPLINE_SURFACE ( (
 ( 1.000000000000000000, 0.8708456909032173954, 1.000000000000000000),
 ( 1.000000000000000000, 0.8699862225465916366, 1.000000000000000000),
 ( 1.000000000000000000, 0.8740515128125330158, 1.000000000000000000),
 ( 1.000000000000000000, 0.8627336009020147856, 1.000000000000000000),
 ( 1.000000000000000000, 0.8557431983335841430, 1.000000000000000000),
 ( 1.000000000000000000, 0.8314605231442517841, 1.000000000000000000),
 ( 1.000000000000000000, 0.8141324793653522685, 1.000000000000000000),
 ( 1.000000000000000000, 0.7486317046913882889, 1.000000000000000000),
 ( 1.000000000000000000, 0.6849789572268089044, 1.000000000000000000),
 ( 1.000000000000000000, 0.5903265755408019233, 1.000000000000000000),
 ( 1.000000000000000000, 0.5583523351997250472, 1.000000000000000000),
 ( 1.000000000000000000, 0.5090820572710972325, 1.000000000000000000),
 ( 1.000000000000000000, 0.4920791080017826169, 1.000000000000000000),
 ( 1.000000000000000000, 0.4915962107220928079, 1.000000000000000000) ) ) 
 REPRESENTATION_ITEM ( '' )  SURFACE ( )  );
#148120 = CARTESIAN_POINT ( 'NONE',  ( 6.643826690903999577, 0.7566192825128185140, -1.820567107441137589 ) ) ;
#148121 = CARTESIAN_POINT ( 'NONE',  ( 1.364683531249988535, 2.113541667008087099, 0.7879004041258500513 ) ) ;
#148122 = CARTESIAN_POINT ( 'NONE',  ( 1.547136693356679249, 0.2016598947911317496, 2.003107868921078616 ) ) ;
#148123 = B_SPLINE_CURVE_WITH_KNOTS ( 'NONE', 3,
 ( #106365, #55428, #90079, #92226, #172389, #140989, #26114, #57566, #9867, #25050, #187551, #23977, #206998, #156142, #91152, #123723, #58629, #107446, #75943, #39181, #124782, #157207, #190741, #42405, #108512, #174539, #44529, #143123, #195026 ),
 .UNSPECIFIED., .F., .F.,
 ( 4, 2, 2, 2, 2, 2, 2, 2, 2, 2, 2, 1, 2, 2, 4 ),
 ( 0.2067929556721437023, 0.2152132502632845279, 0.2236335448544253535, 0.2320538394455661790, 0.2341589130933515450, 0.2362639867411369388, 0.2404741340367071989, 0.2488944286278472751, 0.2531045759234175074, 0.2573147232189876843, 0.2594197968667729670, 0.2615248705145582497, 0.2636299441623435325, 0.2657350178101288707, 0.2741553124012698905 ),
 .UNSPECIFIED. ) ;
#148125 = CARTESIAN_POINT ( 'NONE',  ( 2.302504360600155842, 1.380385731239835323, -1.605472654339132887 ) ) ;
#148124 = CARTESIAN_POINT ( 'NONE',  ( -7.700668062882078502, 9.046829497192987901, -1.082531754730543971 ) ) ;
#148126 = CARTESIAN_POINT ( 'NONE',  ( -6.486624235763164492, 6.835203243035253173, 0.7121179707554707861 ) ) ;
#148127 = CARTESIAN_POINT ( 'NONE',  ( 4.035645461687249913, 1.950487776689105557, -0.6946759356915442885 ) ) ;
#148128 = CARTESIAN_POINT ( 'NONE',  ( 3.888156192069020634, 7.758209000714329839, 1.040834085586084257E-14 ) ) ;
#148130 = CARTESIAN_POINT ( 'NONE',  ( 2.842405760359353106, 6.467890487061221272, -0.7998128361456291469 ) ) ;
#148129 = CARTESIAN_POINT ( 'NONE',  ( 6.175741434174033984, -1.119382356216396479, 1.765513623829425116 ) ) ;
#148132 = ORIENTED_EDGE ( 'NONE', *, *, #185183, .F. ) ;
#148131 = CARTESIAN_POINT ( 'NONE',  ( 4.383705365265609721, 1.192707349210776036, 1.382196219385352309 ) ) ;
#148133 = CARTESIAN_POINT ( 'NONE',  ( 10.05353459973327368, 11.68787744023238417, -1.199719254218440723 ) ) ;
#148134 = DIRECTION ( 'NONE',  ( -5.578564026256490882E-16, -1.000000000000000000, -9.066213480720158442E-32 ) ) ;
#148135 = CARTESIAN_POINT ( 'NONE',  ( 9.300803202052959406, 13.23374025275723120, 6.731078372561743350 ) ) ;
#148136 = CARTESIAN_POINT ( 'NONE',  ( 5.034293675167555548, 1.138177661764948834, -1.890478833441497031 ) ) ;
#148137 = CARTESIAN_POINT ( 'NONE',  ( -0.6823417656250003738, 10.71354166700806765, 1.181850606188754593 ) ) ;
#148138 = EDGE_LOOP ( 'NONE', ( #205186, #154913, #105867, #173534, #133677 ) ) ;
#148139 = CARTESIAN_POINT ( 'NONE',  ( 3.492734469894549942, -1.843672829398453228, -0.5074192597756199685 ) ) ;
#148140 = CARTESIAN_POINT ( 'NONE',  ( -8.435144125996554720, 12.99275191363802229, 0.7998128361456341429 ) ) ;
#148141 = CARTESIAN_POINT ( 'NONE',  ( 6.174848896020108668, 9.291408581077091000, 1.199719254218460707 ) ) ;
#148142 = CARTESIAN_POINT ( 'NONE',  ( 1.360316468749964480, 2.046875000341397133, -4.857225732735059864E-14 ) ) ;
#148143 = CARTESIAN_POINT ( 'NONE',  ( 5.192409643909512873, 6.120528008391641350, -1.082531754730549078 ) ) ;
#148144 = CARTESIAN_POINT ( 'NONE',  ( 10.99998664267163484, -6.472053282365753724, 0.02741317976724608543 ) ) ;
#148145 = CARTESIAN_POINT ( 'NONE',  ( 8.434158656714652480, 13.95694151194098431, -8.536592743144272077 ) ) ;
#148146 = CARTESIAN_POINT ( 'NONE',  ( 0.5558949066124979632, -1.334021266253348381, 1.269314063962426076 ) ) ;
#148147 = ORIENTED_EDGE ( 'NONE', *, *, #181711, .T. ) ;
#148148 = AXIS2_PLACEMENT_3D ( 'NONE', #106287, #187474, #71575 ) ;
#148149 = CARTESIAN_POINT ( 'NONE',  ( -7.370792787684826486, 8.628288336167626582, -1.199719254218452047 ) ) ;
#148150 = CARTESIAN_POINT ( 'NONE',  ( 4.604681543780857034, 1.447206075137374759, -1.185162884121161442 ) ) ;
#148151 = CARTESIAN_POINT ( 'NONE',  ( -6.772456105771887280, -7.184999792969690269, -6.662120174140245155 ) ) ;
#148152 = CARTESIAN_POINT ( 'NONE',  ( 0.05083683574733967314, 14.51110989222127223, 11.99422657299097494 ) ) ;
#148153 = CARTESIAN_POINT ( 'NONE',  ( -7.700668062882084719, 8.086460282891644979, -0.7216878364870278340 ) ) ;
#148154 = CARTESIAN_POINT ( 'NONE',  ( 4.123651276850781144, 7.962676922967908411, -0.7998128361456221525 ) ) ;
#148155 = CARTESIAN_POINT ( 'NONE',  ( 1.358185265713553136, -1.969629313231166856, -0.005369267927731942967 ) ) ;
#148156 = CARTESIAN_POINT ( 'NONE',  ( 2.759388848745081280, 1.913798524274639812, -0.6352183541234107667 ) ) ;
#148157 = CARTESIAN_POINT ( 'NONE',  ( -8.483651433849100698, 10.92067931095586886, 1.599625672291269396 ) ) ;
#148158 = CARTESIAN_POINT ( 'NONE',  ( 6.703580607314123085, 6.785541894813420072, 0.000000000000000000 ) ) ;
#148159 = CARTESIAN_POINT ( 'NONE',  ( 6.773376349083136461, -7.246166700180801001, 6.661184041420955104 ) ) ;
#148160 = CARTESIAN_POINT ( 'NONE',  ( 2.238457302780196390, 0.4817095239468481283, 2.137691825660259948 ) ) ;
#148161 = FILL_AREA_STYLE_COLOUR ( '', #147148 ) ;
#148162 = CARTESIAN_POINT ( 'NONE',  ( -7.797910906154257304, 12.24931315715533486, 0.000000000000000000 ) ) ;
#148163 = CARTESIAN_POINT ( 'NONE',  ( 3.823036128929238942, 7.404033217152015567, 1.040834085586084257E-14 ) ) ;
#148164 = CARTESIAN_POINT ( 'NONE',  ( 0.000000000000000000, -7.154544010627095219, 0.000000000000000000 ) ) ;
#148165 = CARTESIAN_POINT ( 'NONE',  ( 3.933273961740286317, 7.602920365423422311, 0.7216878364870257245 ) ) ;
#148167 = EDGE_CURVE ( 'NONE', #63091, #78277, #188587, .T. ) ;
#148166 = CARTESIAN_POINT ( 'NONE',  ( 7.072549687823125097, 11.40305840243567381, -0.7998128361456291469 ) ) ;
#148168 = CARTESIAN_POINT ( 'NONE',  ( 4.241003122976366058, 3.842258486427521103, -0.7998128361456211532 ) ) ;
#148169 = CARTESIAN_POINT ( 'NONE',  ( 7.187230829020130329, 7.557726520044554697, 0.7216878364870267237 ) ) ;
#148170 = ORIENTED_EDGE ( 'NONE', *, *, #30193, .T. ) ;
#148172 = CARTESIAN_POINT ( 'NONE',  ( 1.524088986950965730, -1.997618534301074833, 0.2487294023021668354 ) ) ;
#148171 = CARTESIAN_POINT ( 'NONE',  ( 5.091278345985558396, -0.6575378499774006125, 1.720029930423284448 ) ) ;
#148173 = CARTESIAN_POINT ( 'NONE',  ( 3.392261881094984055, 0.05328783134446976599, 2.297904267588930960 ) ) ;
#148175 = CARTESIAN_POINT ( 'NONE',  ( 1.305250306655120207, -1.462593314309963866, -1.150481100809984891 ) ) ;
#148174 = CARTESIAN_POINT ( 'NONE',  ( -0.1290005225502675879, 5.719648796287211567, -2.768066027128403217 ) ) ;
#148176 = CARTESIAN_POINT ( 'NONE',  ( 1.001543065824772753E-15, -2.821874999522044458, 3.793834371823811669 ) ) ;
#148177 = CARTESIAN_POINT ( 'NONE',  ( -9.453429865429503920, 15.47131253150566721, -7.391430728740559175 ) ) ;
#148178 = CARTESIAN_POINT ( 'NONE',  ( 5.625241921295836889, 1.689600096388569561, 0.8957793909229803120 ) ) ;
#148179 = CARTESIAN_POINT ( 'NONE',  ( -9.318531651294266638, 9.766041769465124034, -0.7998128361456291469 ) ) ;
#148180 = CARTESIAN_POINT ( 'NONE',  ( -7.105881907338169157, 8.423188659050232729, -1.082531754730549967 ) ) ;
#148182 = CARTESIAN_POINT ( 'NONE',  ( 1.885419139999934934, 1.287927767047767125, 1.356919574424742203 ) ) ;
#148181 = CARTESIAN_POINT ( 'NONE',  ( 3.702747019872438372, 1.794327276830971707, 1.072858563533698018 ) ) ;
#148183 = CARTESIAN_POINT ( 'NONE',  ( 7.619319141200070256, 8.951922421897323900, 1.082531754730558626 ) ) ;
#148184 = CARTESIAN_POINT ( 'NONE',  ( 0.6823417656249917140, 4.905208333674755394, 1.181850606188765695 ) ) ;
#148185 = CARTESIAN_POINT ( 'NONE',  ( 6.146043377905669125, 0.5841948715668408010, 1.746183665442810007 ) ) ;
#148186 = CARTESIAN_POINT ( 'NONE',  ( 2.333974999846879061, 5.874721266463329705, -0.7998128361456291469 ) ) ;
#148187 = CARTESIAN_POINT ( 'NONE',  ( -7.446209719563359641, -5.223431457505076203, -8.064677165291183059 ) ) ;
#148188 = CARTESIAN_POINT ( 'NONE',  ( 4.969259055160575755, 0.1640942704066571667, -1.717058449848630985 ) ) ;
#148189 = CARTESIAN_POINT ( 'NONE',  ( -5.703176172842872482, 9.805455968292021041, 0.000000000000000000 ) ) ;
#148190 = CARTESIAN_POINT ( 'NONE',  ( 0.4219819185556292207, -1.224561070735529444, -1.228170329033271724 ) ) ;
#148191 = PRESENTATION_STYLE_ASSIGNMENT (( #146073 ) ) ;
#148192 = CARTESIAN_POINT ( 'NONE',  ( -10.39025099420816467, 3.467171072964058354, -5.998814208453826069 ) ) ;
#148193 = AXIS2_PLACEMENT_3D ( 'NONE', #178550, #45360, #146069 ) ;
#148194 = CARTESIAN_POINT ( 'NONE',  ( -1.225000000000003864, 0.8125000006827948207, -3.469446951953614189E-15 ) ) ;
#148195 = CARTESIAN_POINT ( 'NONE',  ( 4.434556658511819016, -1.254960995779637045, 1.771429847731820661 ) ) ;
#148196 = CARTESIAN_POINT ( 'NONE',  ( 3.457459740917231628, 0.4424662778084071935, -1.771134634090239190 ) ) ;
#148197 = CARTESIAN_POINT ( 'NONE',  ( 1.393326438508041942, -1.775833184744341375, 0.8338576968042878956 ) ) ;
#148198 = CARTESIAN_POINT ( 'NONE',  ( 5.735599800244862045, 0.6120854273203913953, -2.026975329707622731 ) ) ;
#148200 = CARTESIAN_POINT ( 'NONE',  ( -1.364683531250012516, 4.551041667008082214, -0.7879004041258300672 ) ) ;
#148199 = CARTESIAN_POINT ( 'NONE',  ( 5.443040390997877509, -1.805468894110316080, -1.412473186189531438 ) ) ;
#148201 = CARTESIAN_POINT ( 'NONE',  ( -4.304117108723031215, 3.915891469798615354, -0.2758893754505397644 ) ) ;
#148202 = CARTESIAN_POINT ( 'NONE',  ( 7.889955328148847258, 11.29236608522730911, -1.199719254218446718 ) ) ;
#148203 = CARTESIAN_POINT ( 'NONE',  ( 1.366058183223411771, 0.6122477967837879342, -2.030190212274018524 ) ) ;
#148204 = CARTESIAN_POINT ( 'NONE',  ( -2.792616454734997866, 6.201876930592042925, 0.7216878364870317197 ) ) ;
#148205 = DIRECTION ( 'NONE',  ( 0.7592566023653003482, 0.6507913734559641616, 0.000000000000000000 ) ) ;
#148206 = CARTESIAN_POINT ( 'NONE',  ( -3.728129053633589152, 7.293308295973741195, 0.7216878364870317197 ) ) ;
#148207 = CARTESIAN_POINT ( 'NONE',  ( 5.981339239477990510, -0.06126731230964890806, 2.170386710549534470 ) ) ;
#148209 = CARTESIAN_POINT ( 'NONE',  ( 1.500000000000001332, 11.90625000068279427, 0.000000000000000000 ) ) ;
#148208 = CARTESIAN_POINT ( 'NONE',  ( 6.983263157960386991, 3.689421308571324776, 2.567857239638075217 ) ) ;
#148211 = VERTEX_POINT ( 'NONE', #141661 ) ;
#148210 = CARTESIAN_POINT ( 'NONE',  ( 2.016565898353571473, -2.220703888365501921, 0.05821906423880519182 ) ) ;
#148212 = CARTESIAN_POINT ( 'NONE',  ( 6.610000000000006537, 0.002781820520842553934, 2.000159646111852929 ) ) ;
#148214 = CARTESIAN_POINT ( 'NONE',  ( 5.436407774000851845, -1.150348206634976833, 1.711801118168945202 ) ) ;
#148213 = CARTESIAN_POINT ( 'NONE',  ( 5.118366684358879759, 5.930181538962194132, 1.199719254218462483 ) ) ;
#148216 = CARTESIAN_POINT ( 'NONE',  ( 3.475000000000000533, -2.974999999999998312, 0.000000000000000000 ) ) ;
#148215 = CARTESIAN_POINT ( 'NONE',  ( 6.066347387471824781, 6.042103138330730872, -0.7998128361456481317 ) ) ;
#148217 = CARTESIAN_POINT ( 'NONE',  ( 5.387385936583818591, 7.378645907471495846, -1.599625672291283607 ) ) ;
#148219 = EDGE_CURVE ( 'NONE', #59141, #179291, #177322, .T. ) ;
#148218 = CARTESIAN_POINT ( 'NONE',  ( 3.285556943750000514, -3.901041666188710177, 1.896917185911906500 ) ) ;
#148220 = CARTESIAN_POINT ( 'NONE',  ( 0.1331565106231329398, 0.7299000548664087429, -2.029785554894456556 ) ) ;
#148221 = CARTESIAN_POINT ( 'NONE',  ( 4.686955257832659427, 1.367739038236553517, 1.232883728221023212 ) ) ;
#148222 = CARTESIAN_POINT ( 'NONE',  ( 3.994848817520957773, 7.812407387083109001, 1.040834085586084257E-14 ) ) ;
#148223 = CARTESIAN_POINT ( 'NONE',  ( 1.430204257492089903, 1.660765249891223316, 0.4652242431656942179 ) ) ;
#148224 = LINE ( 'NONE', #115765, #6178 ) ;
#148225 = CARTESIAN_POINT ( 'NONE',  ( 2.040019973291283151, -1.774186676285171460, 1.461575674325124252 ) ) ;
#148226 = CARTESIAN_POINT ( 'NONE',  ( 0.6823417656249917140, 3.405208333674754506, 1.181850606188765695 ) ) ;
#148227 = CARTESIAN_POINT ( 'NONE',  ( 1.599281762659544137, 1.849886183345637258, -1.302228464298058830 ) ) ;
#148228 = CARTESIAN_POINT ( 'NONE',  ( 4.002637171539184635, -0.6605693356034693098, -1.999858192447926397 ) ) ;
#148229 = CARTESIAN_POINT ( 'NONE',  ( -5.939880696562884310, 9.943961556049767836, 0.7216878364870267237 ) ) ;
#148230 = CARTESIAN_POINT ( 'NONE',  ( 1.985279565377489508, 1.216254750358658487, 1.285827030011628347 ) ) ;
#148232 = EDGE_CURVE ( 'NONE', #138814, #86850, #56937, .T. ) ;
#148231 = CARTESIAN_POINT ( 'NONE',  ( 6.612626235163189925, 8.737816579155630592, -1.599625672291262513 ) ) ;
#148233 = CARTESIAN_POINT ( 'NONE',  ( 4.326460416092276162, 7.101268681199365496, -1.082531754730548412 ) ) ;
#148234 = CARTESIAN_POINT ( 'NONE',  ( -4.577849422908604637, 8.492574760035358494, -0.7998128361456281477 ) ) ;
#148235 = CARTESIAN_POINT ( 'NONE',  ( 0.7499999999999885647, 1.816666666666688634, -1.299038105676652899 ) ) ;
#148236 = CARTESIAN_POINT ( 'NONE',  ( 5.625276811391259457, 1.958927336128764241, 1.047432077188856780 ) ) ;
#148237 = CARTESIAN_POINT ( 'NONE',  ( 3.697391623616069101, -0.6365095100077067247, 2.096977347260075231 ) ) ;
#148238 = CARTESIAN_POINT ( 'NONE',  ( -3.750802052474980108, 7.527686161196117887, 1.040834085586084257E-14 ) ) ;
#148239 = CARTESIAN_POINT ( 'NONE',  ( -4.390861645979385663, 6.216034235099629157, -1.599625672291271394 ) ) ;
#148240 = CARTESIAN_POINT ( 'NONE',  ( 10.89999999999920632, -3.437048488108780906E-15, -0.2598076211376266764 ) ) ;
#148241 = CARTESIAN_POINT ( 'NONE',  ( 1.364683531249988535, 3.155208333674756283, -0.7879004041258239610 ) ) ;
#148242 = CARTESIAN_POINT ( 'NONE',  ( 6.610000000000010090, 0.5825982378308904863, 2.053072689460200273 ) ) ;
#148243 = CARTESIAN_POINT ( 'NONE',  ( -4.934804725694231564, 5.819988937140460727, -1.082531754730544860 ) ) ;
#148244 = CARTESIAN_POINT ( 'NONE',  ( 5.537388447972660721, -0.05000006065614125139, 2.120159173171487055 ) ) ;
#148245 = CARTESIAN_POINT ( 'NONE',  ( -7.322812365156824654, 8.676274193172000437, 1.082531754730549078 ) ) ;
#148246 = VERTEX_POINT ( 'NONE', #174145 ) ;
#148247 = CARTESIAN_POINT ( 'NONE',  ( -4.773879485787619892, 7.623257595843924150, 1.082531754730549967 ) ) ;
#148248 = CARTESIAN_POINT ( 'NONE',  ( 5.355634372598031767, 6.206993841907870291, -1.199719254218445830 ) ) ;
#148249 = CARTESIAN_POINT ( 'NONE',  ( 6.040549724581927293, -1.551790349881351450, 0.9907606852931831742 ) ) ;
#148250 = UNCERTAINTY_MEASURE_WITH_UNIT (LENGTH_MEASURE( 1.000000000000000082E-05 ), #121366, 'distance_accuracy_value', 'NONE');
#148251 = DIRECTION ( 'NONE',  ( 1.000000000000000000, -0.000000000000000000, -0.000000000000000000 ) ) ;
#148252 = DIRECTION ( 'NONE',  ( 0.000000000000000000, -1.000000000000000000, 0.000000000000000000 ) ) ;
#148253 = CARTESIAN_POINT ( 'NONE',  ( -1.364683531250012516, 2.301041667008087988, -0.7879004041258289570 ) ) ;
#148254 = CARTESIAN_POINT ( 'NONE',  ( 1.540153114873343609, -1.470452955542918660, 0.9307524122482965234 ) ) ;
#148255 = CARTESIAN_POINT ( 'NONE',  ( 3.708318708537623021, 4.285125567170706695, -1.199719254218446718 ) ) ;
#148257 = CARTESIAN_POINT ( 'NONE',  ( 11.84668730067608600, 12.69999999999998153, 1.399999999999998579 ) ) ;
#148256 = AXIS2_PLACEMENT_3D ( 'NONE', #169677, #116716, #154508 ) ;
#148258 = CARTESIAN_POINT ( 'NONE',  ( 1.364683531249986537, -0.5322916663252452718, -0.7879004041258309554 ) ) ;
#148259 = CARTESIAN_POINT ( 'NONE',  ( -0.3868389748197708644, 3.100956225802684596, -0.4583768147623576428 ) ) ;
#148260 = CARTESIAN_POINT ( 'NONE',  ( 5.137646372127643524, -1.526005641499485810, -1.531359247741073570 ) ) ;
#148261 = CARTESIAN_POINT ( 'NONE',  ( -4.471491734408701291, 4.111161866431900513, 1.214306433183764966E-14 ) ) ;
#148262 = EDGE_CURVE ( 'NONE', #23435, #64464, #78362, .T. ) ;
#148263 = CARTESIAN_POINT ( 'NONE',  ( -7.334597914868743018, 7.659378443542744996, -0.7216878364870267237 ) ) ;
#148264 = CARTESIAN_POINT ( 'NONE',  ( 4.346650381253648554, 0.5737703434565506466, 2.084106190491950006 ) ) ;
#148266 = ORIENTED_EDGE ( 'NONE', *, *, #15354, .T. ) ;
#148265 = CARTESIAN_POINT ( 'NONE',  ( -4.228163802615396705, 6.026220084508304708, -1.599625672291271394 ) ) ;
#148267 = CARTESIAN_POINT ( 'NONE',  ( -1.201851678989727383E-14, 3.196875000341420137, -1.575800808251660134 ) ) ;
#148268 = CARTESIAN_POINT ( 'NONE',  ( 6.063742386902314152, 1.942598920255795392, -0.3345802184639041776 ) ) ;
#148269 = CARTESIAN_POINT ( 'NONE',  ( 4.692597494581693063, -1.067344209891357032, -1.366281018423552762 ) ) ;
#148271 = CARTESIAN_POINT ( 'NONE',  ( 2.243918346939121733, 2.191141468336772036, 0.05030144379260945153 ) ) ;
#148270 = CARTESIAN_POINT ( 'NONE',  ( -1.352083138863443345E-14, -0.9218749996585863249, -1.570758158831792262 ) ) ;
#148272 = CARTESIAN_POINT ( 'NONE',  ( 3.680997481958053541, -2.223193225534472628, -0.6181044232122161475 ) ) ;
#148273 = CARTESIAN_POINT ( 'NONE',  ( 4.903620131156614548, -0.5536938069644473659, 1.984910608926907960 ) ) ;
#148274 = CARTESIAN_POINT ( 'NONE',  ( 0.07597880344310371792, -1.883441279811811642, -0.4727451468593062422 ) ) ;
#148275 = CARTESIAN_POINT ( 'NONE',  ( -6.005898860729463884, 9.950706404252290582, 0.7216878364870458196 ) ) ;
#148276 = CARTESIAN_POINT ( 'NONE',  ( -3.793249116773374396, 7.647484079536056356, 0.7998128361456352531 ) ) ;
#148277 = DIRECTION ( 'NONE',  ( 0.000000000000000000, 0.000000000000000000, -1.000000000000000000 ) ) ;
#148278 = CARTESIAN_POINT ( 'NONE',  ( 3.621431001533811589, 1.820626359085864454, 1.087046460333654485 ) ) ;
#148279 = DIRECTION ( 'NONE',  ( 0.000000000000000000, 0.000000000000000000, -1.000000000000000000 ) ) ;
#148280 = CARTESIAN_POINT ( 'NONE',  ( 1.477185633673218534, -2.006960102380969779, -0.1948397147320118372 ) ) ;
#148281 = CARTESIAN_POINT ( 'NONE',  ( -7.009202228140764213, 7.279750142360097875, -0.7216878364870267237 ) ) ;
#148282 = CARTESIAN_POINT ( 'NONE',  ( 4.840968367003476658, 0.3731960759543617723, 2.174832070070693568 ) ) ;
#148283 = DIRECTION ( 'NONE',  ( -1.000000000000000000, 1.016547956922408957E-15, 1.479114432388267300E-31 ) ) ;
#148284 = CARTESIAN_POINT ( 'NONE',  ( -1.123270288250318494, 3.297697346350006331, -0.7749999999993560929 ) ) ;
#148285 = CARTESIAN_POINT ( 'NONE',  ( 0.000000000000000000, 0.5000000000000000000, 0.000000000000000000 ) ) ;
#148286 = CARTESIAN_POINT ( 'NONE',  ( -7.587723245503481095, 8.881373870289390737, 1.199719254218452047 ) ) ;
#148288 = CARTESIAN_POINT ( 'NONE',  ( -2.788906526875773208E-15, 8.968750000682797818, -1.499999999999998446 ) ) ;
#148287 = CARTESIAN_POINT ( 'NONE',  ( -4.712608863230891565, 8.343829661033030476, -0.7091526064728018719 ) ) ;
#148289 = DIRECTION ( 'NONE',  ( 0.000000000000000000, 0.000000000000000000, -1.000000000000000000 ) ) ;
#148290 = ORIENTED_EDGE ( 'NONE', *, *, #186210, .F. ) ;
#148291 = CARTESIAN_POINT ( 'NONE',  ( 3.977457805978751093, 1.941116309567689324, -0.6927405623450531014 ) ) ;
#148292 = CARTESIAN_POINT ( 'NONE',  ( -0.6801582343750213200, 1.348958333674710186, -1.178068619123886718 ) ) ;
#148293 = CARTESIAN_POINT ( 'NONE',  ( -4.446184310277715213, 7.274633231044262516, -1.199719254218452047 ) ) ;
#148294 = CARTESIAN_POINT ( 'NONE',  ( 3.492836188673923647, -1.947007740449010926, -0.5366636104956448161 ) ) ;
#148295 = CARTESIAN_POINT ( 'NONE',  ( -1.500000000000015099, -0.8291666666666407393, 0.8660254037844403729 ) ) ;
#148296 = AXIS2_PLACEMENT_3D ( 'NONE', #129211, #96642, #11075 ) ;
#148297 = CARTESIAN_POINT ( 'NONE',  ( 10.39874063200158893, 11.23421161353111586, 0.000000000000000000 ) ) ;
#148298 = CARTESIAN_POINT ( 'NONE',  ( 8.471147050440139381, 8.777426401801974976, -0.7998128361456281477 ) ) ;
#148299 = CARTESIAN_POINT ( 'NONE',  ( 2.957942382388091040, 2.051108442962752409, -0.2004023863233852509 ) ) ;
#148300 = CARTESIAN_POINT ( 'NONE',  ( 4.177814833343409084, 3.976464848429826393, 1.040551764647542070E-14 ) ) ;
#148301 = CARTESIAN_POINT ( 'NONE',  ( 4.819033534653518025, 7.709623992816043270, -1.199719254218452047 ) ) ;
#148302 = CARTESIAN_POINT ( 'NONE',  ( -0.1409997244346122836, 0.7174646053854060179, -2.082770303449644977 ) ) ;
#148303 = CARTESIAN_POINT ( 'NONE',  ( 1.833694255977034615, 1.820935426717207317, 0.2711280389895084353 ) ) ;
#148304 = CARTESIAN_POINT ( 'NONE',  ( 0.2238089703245670359, -0.1066217210726662923, 2.305362286893299917 ) ) ;
#148305 = CARTESIAN_POINT ( 'NONE',  ( 4.525389411911321602, 8.501647757197021704, -0.7998128361456381397 ) ) ;
#148306 = CARTESIAN_POINT ( 'NONE',  ( 1.476082264964494906, 1.286352913914396545, 1.737049067733025032 ) ) ;
#148307 = AXIS2_PLACEMENT_3D ( 'NONE', #88406, #139299, #205328 ) ;
#148308 = CARTESIAN_POINT ( 'NONE',  ( -4.622967192579922724, 4.495809267539077503, 1.214306433183764966E-14 ) ) ;
#148309 = CARTESIAN_POINT ( 'NONE',  ( 1.903530124611974017, -1.954778955200174861, 0.4946342604733033887 ) ) ;
#148310 = CARTESIAN_POINT ( 'NONE',  ( 6.471393748265519719, 5.229711127717882491, -2.499999999999995115 ) ) ;
#148311 = CARTESIAN_POINT ( 'NONE',  ( 0.3033014811697418711, -0.5033704626738467747, 1.801585485020948951 ) ) ;
#148312 = CARTESIAN_POINT ( 'NONE',  ( 5.067239680553584869, 0.1942248685237786265, -1.961885565008324006 ) ) ;
#148313 = CARTESIAN_POINT ( 'NONE',  ( 4.171111447311355747, 1.799123655847803205, -0.9110083886025857058 ) ) ;
#148315 = CARTESIAN_POINT ( 'NONE',  ( 8.554831740098649107, 11.96409221588171157, 1.082531754730546636 ) ) ;
#148314 = CARTESIAN_POINT ( 'NONE',  ( -1.402160292154681736E-14, 1.696875000341421469, -1.575800808251659024 ) ) ;
#148317 = CARTESIAN_POINT ( 'NONE',  ( 5.901026713257129686, 1.722607154707327615, -1.211383145191318400 ) ) ;
#148316 = CARTESIAN_POINT ( 'NONE',  ( -7.660520486921249983, 8.896027641951645748, -1.199719254218446718 ) ) ;
#148318 = CARTESIAN_POINT ( 'NONE',  ( 5.160626937512653001, -0.6942339714755951796, -1.950645400549338104 ) ) ;
#148319 = CARTESIAN_POINT ( 'NONE',  ( 6.817052309572890323, 6.847649204123507083, 0.7998128361456341429 ) ) ;
#148320 = CARTESIAN_POINT ( 'NONE',  ( -5.228640796364566690, 9.251831362400652736, -0.7998128361456231517 ) ) ;
#148321 = CARTESIAN_POINT ( 'NONE',  ( 6.539320575229230492, 2.428701779328062749, 2.485127258459709054 ) ) ;
#148322 = CARTESIAN_POINT ( 'NONE',  ( 5.730724961554885866, 1.353511160402442570, -1.499384403026276180 ) ) ;
#148323 = CARTESIAN_POINT ( 'NONE',  ( 1.499999999999985123, -0.6729166659838520248, -0.8660254037844323793 ) ) ;
#148324 = CARTESIAN_POINT ( 'NONE',  ( 3.932480676516422413, 1.235928489987428325, -1.948660470369364628 ) ) ;
#148325 = CARTESIAN_POINT ( 'NONE',  ( 1.393505825229651052, -1.866293207157668776, 0.8783701326641482066 ) ) ;
#148326 = CARTESIAN_POINT ( 'NONE',  ( 8.432808358020025707, 9.900993174853955026, 1.082531754730558626 ) ) ;
#148327 = CARTESIAN_POINT ( 'NONE',  ( 4.993145711582793744, 9.047363440147082159, -0.7998128361456481317 ) ) ;
#148328 = CARTESIAN_POINT ( 'NONE',  ( 4.701645408888975197, 8.707279753670952971, 0.000000000000000000 ) ) ;
#148329 = CARTESIAN_POINT ( 'NONE',  ( 0.6823417656249899377, 0.6552083336747518416, 1.181850606188755259 ) ) ;
#148330 = CARTESIAN_POINT ( 'NONE',  ( 5.174371902270911150, 6.065797303184739420, 1.199719254218452047 ) ) ;
#148331 = CARTESIAN_POINT ( 'NONE',  ( 7.090551149822739596, 8.335026431957096804, 1.082531754730558626 ) ) ;
#148333 = CARTESIAN_POINT ( 'NONE',  ( 11.48243876534946217, 12.29999999999998295, 3.199999999999997957 ) ) ;
#148332 = CARTESIAN_POINT ( 'NONE',  ( 4.686072593652621521, -1.332121122860012052, -1.714431229949509250 ) ) ;
#148334 = CARTESIAN_POINT ( 'NONE',  ( -3.280072367755099361, -0.8887487162373143290, 0.2896574332902090432 ) ) ;
#148336 = CARTESIAN_POINT ( 'NONE',  ( 3.087279721815265443, -0.7436087841871074078, 1.684586988852328160 ) ) ;
#148335 = CARTESIAN_POINT ( 'NONE',  ( -3.958617665510272943, 6.601842462195195438, -1.082531754730549967 ) ) ;
#148337 = CARTESIAN_POINT ( 'NONE',  ( -0.6823417656249969321, 4.967708333674755394, -1.181850606188749264 ) ) ;
#148338 = CARTESIAN_POINT ( 'NONE',  ( 4.300438532332786501, 1.693616701070689956, -1.390861761948622766 ) ) ;
#148339 = CARTESIAN_POINT ( 'NONE',  ( 8.359932177502960471, 14.08591219777413528, 8.547035205493129340 ) ) ;
#148340 = CARTESIAN_POINT ( 'NONE',  ( 5.788003261412111300, -1.023269635773180752, 2.017978558835635372 ) ) ;
#148341 = DIRECTION ( 'NONE',  ( -0.000000000000000000, -1.000000000000000000, -0.000000000000000000 ) ) ;
#148342 = CARTESIAN_POINT ( 'NONE',  ( 5.303225773876714122, 7.631601692149430072, -1.229104931163179426 ) ) ;
#148343 = CARTESIAN_POINT ( 'NONE',  ( -4.895902867866254837, 7.765618208269001066, 1.082531754730549967 ) ) ;
#148344 = CARTESIAN_POINT ( 'NONE',  ( 4.746763178560261309, 5.670883475476017566, 1.082531754730549078 ) ) ;
#148345 = CARTESIAN_POINT ( 'NONE',  ( 6.292257686217937795, -1.761477974832075244, -0.1709902323579186867 ) ) ;
#148347 = CARTESIAN_POINT ( 'NONE',  ( 3.844392992367959838, 1.075074360472785928, -1.701806764060603161 ) ) ;
#148346 = AXIS2_PLACEMENT_3D ( 'NONE', #157796, #40849, #153519 ) ;
#148348 = CARTESIAN_POINT ( 'NONE',  ( 5.635385404774530649, 9.726366738878972740, 0.7998128361456462443 ) ) ;
#148349 = CARTESIAN_POINT ( 'NONE',  ( 3.258910125681306891, -1.595695288142566337, 1.374458643164514937 ) ) ;
#148350 = CARTESIAN_POINT ( 'NONE',  ( 1.634256478289298320, 0.6027960111968011514, 1.818337931642779903 ) ) ;
#148351 = CARTESIAN_POINT ( 'NONE',  ( 3.174580523894166006, 6.855427711185178019, 0.7998128361456341429 ) ) ;
#148352 = B_SPLINE_CURVE_WITH_KNOTS ( 'NONE', 3,
 ( #127678, #129802, #161153, #163286, #195782, #179540, #80958, #147051, #193638, #32212, #15934, #82017, #148108, #214111, #65738, #143881, #181640, #49523 ),
 .UNSPECIFIED., .F., .F.,
 ( 4, 2, 2, 2, 2, 2, 2, 2, 4 ),
 ( 2.649649035303588278E-18, 0.0002050783776814521433, 0.0004101567553629016302, 0.0006152351330443510359, 0.0008203135107258005499, 0.001025391888407249956, 0.001230470266088699470, 0.001435548643770148984, 0.001640627021451598498 ),
 .UNSPECIFIED. ) ;
#148353 = CARTESIAN_POINT ( 'NONE',  ( 3.314863512866594863, -1.493043793209645864, 1.284631214971102775 ) ) ;
#148354 = CARTESIAN_POINT ( 'NONE',  ( 4.799084794409138155, -0.2512425647771680537, -2.004053532012660455 ) ) ;
#148355 = CARTESIAN_POINT ( 'NONE',  ( 0.7603692911175019553, -1.357789551990191246, 1.287012767582619510 ) ) ;
#148356 = CARTESIAN_POINT ( 'NONE',  ( 0.5901948623465642640, 1.011764341257429978, -1.680720577067334354 ) ) ;
#148358 = ORIENTED_EDGE ( 'NONE', *, *, #77906, .F. ) ;
#148357 = CARTESIAN_POINT ( 'NONE',  ( 0.2110004604562870645, 1.588762659912812403, -1.064147093309028680 ) ) ;
#148359 = CARTESIAN_POINT ( 'NONE',  ( 5.097502569058200983, 6.970172302033127210, -1.443375672974051449 ) ) ;
#148360 = ADVANCED_FACE ( 'NONE', ( #127595 ), #12713, .T. ) ;
#148361 = CARTESIAN_POINT ( 'NONE',  ( -1.364683531250000748, 0.8218750003414210248, 0.000000000000000000 ) ) ;
#148362 = CARTESIAN_POINT ( 'NONE',  ( 6.280143113937574739, -0.9989825818290422044, 1.581392243879369053 ) ) ;
#148363 = CARTESIAN_POINT ( 'NONE',  ( 8.353795204314554468, 12.89784483834236184, -0.7998128361456352531 ) ) ;
#148364 = CARTESIAN_POINT ( 'NONE',  ( -2.482948226198874231, 5.072301959192136778, -2.499999999999995115 ) ) ;
#148365 = CARTESIAN_POINT ( 'NONE',  ( 6.491088764554701740, 0.1969099459505334604, 2.060843999385448821 ) ) ;
#148366 =( NAMED_UNIT ( * ) PLANE_ANGLE_UNIT ( ) SI_UNIT ( $, .RADIAN. ) );
#148367 = CARTESIAN_POINT ( 'NONE',  ( 0.5024991115675537801, 2.064720838319131779, 0.1538615064654233477 ) ) ;
#148368 = CARTESIAN_POINT ( 'NONE',  ( -1.402160292154681736E-14, 1.337500000000025446, -1.732050807568863648 ) ) ;
#148369 = CARTESIAN_POINT ( 'NONE',  ( 7.558834334818744338, 8.777393797832065303, 1.199719254218462483 ) ) ;
#148370 = CARTESIAN_POINT ( 'NONE',  ( -8.259941899223614215, 10.65968485389279508, -1.599625672291263179 ) ) ;
#148371 = CARTESIAN_POINT ( 'NONE',  ( 3.691562964670865199, 7.528850235416478576, -0.7998128361456362523 ) ) ;
#148372 = CARTESIAN_POINT ( 'NONE',  ( 5.057343377742961721, -1.818460011135439869, 1.090507627184752693 ) ) ;
#148373 = CARTESIAN_POINT ( 'NONE',  ( 0.6823417656249882723, 1.676041667008083769, -1.181850606188749264 ) ) ;
#148374 = CARTESIAN_POINT ( 'NONE',  ( -1.201851678989727383E-14, 3.087500000000026112, -1.732050807568863648 ) ) ;
#148376 = CARTESIAN_POINT ( 'NONE',  ( 5.345992642490140057, 5.131412925860272090, 1.040834085586084257E-14 ) ) ;
#148375 = CARTESIAN_POINT ( 'NONE',  ( 5.969191311310417802, 1.729517061547349632, 0.9261464158661563140 ) ) ;
#148377 = CARTESIAN_POINT ( 'NONE',  ( 4.306017418194902469, -1.755500069608874281, 0.9912479507018998603 ) ) ;
#148378 = CARTESIAN_POINT ( 'NONE',  ( 3.169047557264609072, 1.729775434385946831, -0.8236773211035466336 ) ) ;
#148379 = EDGE_CURVE ( 'NONE', #160219, #14247, #128656, .T. ) ;
#148380 = FACE_OUTER_BOUND ( 'NONE', #43223, .T. ) ;
#148381 = CARTESIAN_POINT ( 'NONE',  ( 1.206853476500208133, 1.935082376036290075, 1.028754739392373496 ) ) ;
#148382 = CARTESIAN_POINT ( 'NONE',  ( -5.608757509019059562, 5.629766575900002401, 2.420000000000000373 ) ) ;
#148383 = CARTESIAN_POINT ( 'NONE',  ( 3.637841704585748293, 0.8437669887123750989, -1.669527271503386201 ) ) ;
#148384 = CARTESIAN_POINT ( 'NONE',  ( -0.7500000000000006661, -0.3604166659838467512, -1.299038105676652011 ) ) ;
#148385 = CARTESIAN_POINT ( 'NONE',  ( 4.711194051470749322, 1.671412949727559383, -1.121937078508246755 ) ) ;
#148386 = CARTESIAN_POINT ( 'NONE',  ( -6.507023659554960204, 9.678945805201045971, 1.199719254218452047 ) ) ;
#148388 = CARTESIAN_POINT ( 'NONE',  ( 5.607064690329227830, -0.05131010805739347896, 2.116756054987908531 ) ) ;
#148387 = CARTESIAN_POINT ( 'NONE',  ( -3.118012141462980669, 6.581505231774690046, 0.7216878364870317197 ) ) ;
#148389 = CARTESIAN_POINT ( 'NONE',  ( -1.242799958986342546, 13.28403883893647119, -0.7783234177255069497 ) ) ;
#148390 = CARTESIAN_POINT ( 'NONE',  ( 6.707487347292075519, -1.660346423639452951, -1.236579608897829363 ) ) ;
#148392 = FACE_OUTER_BOUND ( 'NONE', #138695, .T. ) ;
#148391 = CARTESIAN_POINT ( 'NONE',  ( 2.226223261843117918, 2.028672367434441792, 0.5052007718874002018 ) ) ;
#148394 = ORIENTED_EDGE ( 'NONE', *, *, #198992, .T. ) ;
#148393 = CARTESIAN_POINT ( 'NONE',  ( 0.7622199101927947806, -1.253934870956091352, 1.184532473512718509 ) ) ;
#148395 = CARTESIAN_POINT ( 'NONE',  ( 5.276094334012385367, 9.307193822989793475, 1.040834085586084257E-14 ) ) ;
#148396 = DIRECTION ( 'NONE',  ( -1.000000000000000000, 0.000000000000000000, 0.000000000000000000 ) ) ;
#148397 = DIRECTION ( 'NONE',  ( 1.000000000000000000, 1.276756478318932585E-15, 4.555315873022827019E-16 ) ) ;
#148398 = PRESENTATION_LAYER_ASSIGNMENT (  '', '', ( #61809 ) ) ;
#148399 = DIRECTION ( 'NONE',  ( 0.6250000000000000000, 1.408756634010579545E-16, -0.7806247497997997886 ) ) ;
#148401 = CARTESIAN_POINT ( 'NONE',  ( 8.310784975052673218, 10.71900177569337487, -1.443375672974063439 ) ) ;
#148400 = CARTESIAN_POINT ( 'NONE',  ( 5.798083248138522272, 9.916180889470295412, 0.7998128361456462443 ) ) ;
#148402 = FACE_OUTER_BOUND ( 'NONE', #178614, .T. ) ;
#148404 = CARTESIAN_POINT ( 'NONE',  ( 2.139049582973771457, 0.0009909630806471080022, 1.811656970554485602 ) ) ;
#148403 = CARTESIAN_POINT ( 'NONE',  ( 6.364626766972446781, 6.390095747748157251, 0.7998128361456352531 ) ) ;
#148405 = CARTESIAN_POINT ( 'NONE',  ( -8.030507057996002729, 8.263346410617135263, 1.040834085586084257E-14 ) ) ;
#148406 = CARTESIAN_POINT ( 'NONE',  ( 4.867540842506059562, 5.637551390133895168, -1.199719254218452047 ) ) ;
#148407 = CARTESIAN_POINT ( 'NONE',  ( -5.850575378433040541, 7.204527765336914413, 1.160475518089182811 ) ) ;
#148408 = CARTESIAN_POINT ( 'NONE',  ( 5.712781623311797397, 7.758274208654143855, -1.599625672291283607 ) ) ;
#148409 = CARTESIAN_POINT ( 'NONE',  ( 6.539320575229245591, 2.459069921018588900, 2.280790101157427419 ) ) ;
#148410 = CARTESIAN_POINT ( 'NONE',  ( -2.535011536075354677, 5.133042487381361596, -7.499999999999997335 ) ) ;
#148411 = FACE_OUTER_BOUND ( 'NONE', #129071, .T. ) ;
#148412 = CARTESIAN_POINT ( 'NONE',  ( 8.080296364064698977, 12.37083682481011060, -0.7216878364870328300 ) ) ;
#148413 = ORIENTED_EDGE ( 'NONE', *, *, #71089, .T. ) ;
#148414 = CARTESIAN_POINT ( 'NONE',  ( 3.068646357036347361, 1.349867735329785434, -1.281425607799644206 ) ) ;
#148415 = CARTESIAN_POINT ( 'NONE',  ( 0.5619445578959707532, -1.063298924184744587, 1.593181094007071863 ) ) ;
#148416 = CARTESIAN_POINT ( 'NONE',  ( 6.194356126197313017, -1.917168722191398000, -0.1884046653951119699 ) ) ;
#148417 = DIRECTION ( 'NONE',  ( 1.000000000000000000, -0.000000000000000000, -0.000000000000000000 ) ) ;
#148418 = CARTESIAN_POINT ( 'NONE',  ( 4.624009687016504166, 8.337032093926254106, -0.3390773965592456252 ) ) ;
#148419 = FACE_OUTER_BOUND ( 'NONE', #37021, .T. ) ;
#148420 = CARTESIAN_POINT ( 'NONE',  ( -3.904385051055635270, 6.538571078664754843, 1.082531754730560403 ) ) ;
#148421 = CARTESIAN_POINT ( 'NONE',  ( 8.514157279702022407, 10.95626946445095307, -1.443375672974063439 ) ) ;
#148422 = CARTESIAN_POINT ( 'NONE',  ( 4.117982337901913148, 1.955079553045156127, -0.2365992483164043592 ) ) ;
#148423 = CARTESIAN_POINT ( 'NONE',  ( 1.524255003590764046, -2.104078925693805502, 0.2628582283784736684 ) ) ;
#148424 = CARTESIAN_POINT ( 'NONE',  ( -5.799137018343247796, 7.788745826199009237, -1.599625672291256295 ) ) ;
#148425 = CARTESIAN_POINT ( 'NONE',  ( 1.499999999999989120, 3.525000000000021227, 1.214306433183764966E-14 ) ) ;
#148426 = CARTESIAN_POINT ( 'NONE',  ( 0.9311234436981455920, -2.696869630441517618, 3.475000000000003197 ) ) ;
#148427 = CARTESIAN_POINT ( 'NONE',  ( 5.367185978643659539, 2.112682091867735146, -0.5819856738719306755 ) ) ;
#148428 = DIRECTION ( 'NONE',  ( -1.000000000000000000, 0.000000000000000000, 0.000000000000000000 ) ) ;
#148429 = CARTESIAN_POINT ( 'NONE',  ( 4.120081753510516975, -0.9896868749219210892, -1.652585292789155558 ) ) ;
#148430 = CARTESIAN_POINT ( 'NONE',  ( -7.152089726408780379, 8.302858421353754181, -1.199719254218446718 ) ) ;
#148431 = CARTESIAN_POINT ( 'NONE',  ( 0.5865807246496178573, -0.2182756592755269454, -1.812417144444453232 ) ) ;
#148432 = CARTESIAN_POINT ( 'NONE',  ( 1.155211076828046801, -1.737760091701185283, 1.360235214042208263 ) ) ;
#148433 = EDGE_LOOP ( 'NONE', ( #55306, #214374, #154135, #63417 ) ) ;
#148434 = CARTESIAN_POINT ( 'NONE',  ( 8.500000000000000000, 6.280000000000042881, -2.873333333333334405 ) ) ;
#148435 = ORIENTED_EDGE ( 'NONE', *, *, #111829, .T. ) ;
#148436 = CARTESIAN_POINT ( 'NONE',  ( 6.596547011414190642, 1.947522214285227760, 0.2922974700911728507 ) ) ;
#148437 = CARTESIAN_POINT ( 'NONE',  ( 1.681094245561355560, 1.340559147886428271, 1.405378567840375403 ) ) ;
#148438 = CARTESIAN_POINT ( 'NONE',  ( 6.222043071159490957, -1.966323047081437014, -1.189884408624383383 ) ) ;
#148440 = CARTESIAN_POINT ( 'NONE',  ( 4.469486699700035537, -0.3212591861478170663, 1.832842066241076040 ) ) ;
#148439 = CARTESIAN_POINT ( 'NONE',  ( -5.745623237141265882, 9.925253886631958622, 0.7998128361456291469 ) ) ;
#148441 = CARTESIAN_POINT ( 'NONE',  ( 5.737035277238070385, 6.722237907313067140, -1.199719254218452047 ) ) ;
#148442 = CARTESIAN_POINT ( 'NONE',  ( 0.4800000000000000933, 2.999999999999999112, -2.420000000000000373 ) ) ;
#148443 = CARTESIAN_POINT ( 'NONE',  ( -6.566226467720086113, 6.555019055295208119, 1.040834085586084257E-14 ) ) ;
#148444 = CARTESIAN_POINT ( 'NONE',  ( -4.340018570150322219, 5.196348098997705556, -1.082531754730551743 ) ) ;
#148445 = CARTESIAN_POINT ( 'NONE',  ( 0.3983070667218471805, -0.7439898890007863308, -2.061537379893277677 ) ) ;
#148446 = CARTESIAN_POINT ( 'NONE',  ( 4.365362273920238678, 7.076377838673507448, 1.082531754730558626 ) ) ;
#148447 = ORIENTED_EDGE ( 'NONE', *, *, #52547, .T. ) ;
#148448 = CIRCLE ( 'NONE', #165755, 0.09999999999999999167 ) ;
#148449 = CARTESIAN_POINT ( 'NONE',  ( 0.2999999999999841682, 3.975028841772316301, -0.9637995837462943749 ) ) ;
#148450 = CARTESIAN_POINT ( 'NONE',  ( 1.910518402784128433, 1.353611321597010253, -1.225282022559864625 ) ) ;
#148451 = CARTESIAN_POINT ( 'NONE',  ( -4.273844736805832767, 6.009238164405336313, 1.599625672291267398 ) ) ;
#148452 = CARTESIAN_POINT ( 'NONE',  ( 3.621445620172254021, 0.2585195360361118300, 1.714627356041095840 ) ) ;
#148453 = CARTESIAN_POINT ( 'NONE',  ( -0.4139337043657510540, 2.993729876475310636, -1.957981511387787865 ) ) ;
#148454 = CARTESIAN_POINT ( 'NONE',  ( 6.609000000000036401, 7.629137130509092479, 2.600000000000000977 ) ) ;
#148455 = CARTESIAN_POINT ( 'NONE',  ( 0.1331565106231363538, 2.033293680964400885, -2.362282156872722805 ) ) ;
#148456 = CARTESIAN_POINT ( 'NONE',  ( 6.217409598193539999, -0.2183660865492654257, 1.812524795094340835 ) ) ;
#148457 = CARTESIAN_POINT ( 'NONE',  ( 4.821123798404616245, -1.750560105953799184, -0.8856655065374098301 ) ) ;
#148458 = MECHANICAL_DESIGN_GEOMETRIC_PRESENTATION_REPRESENTATION (  '', ( #120838 ), #193292 ) ;
#148459 = CARTESIAN_POINT ( 'NONE',  ( -8.850775351622791831, 9.220326086515070685, -0.7998128361456291469 ) ) ;
#148460 = CARTESIAN_POINT ( 'NONE',  ( 5.438792177376376991, 9.497007973581119700, 1.040834085586084257E-14 ) ) ;
#148461 = VECTOR ( 'NONE', #167275, 1000.000000000000000 ) ;
#148462 = CARTESIAN_POINT ( 'NONE',  ( 5.215537505735290402, 1.733765862324820439, 1.220609238144418240 ) ) ;
#148463 = CARTESIAN_POINT ( 'NONE',  ( -8.565000355531095622, 11.01558638625153286, -1.599625672291263179 ) ) ;
#148464 = CARTESIAN_POINT ( 'NONE',  ( 4.039439701867726384, 6.800097854565950506, 1.199719254218462483 ) ) ;
#148466 = ADVANCED_FACE ( 'NONE', ( #178394 ), #156814, .F. ) ;
#148465 = CARTESIAN_POINT ( 'NONE',  ( 3.256751887857904926, -0.5965066610371800859, -1.982489643792232137 ) ) ;
#148468 = CARTESIAN_POINT ( 'NONE',  ( 1.364683531249986537, 0.2177083336747502595, -0.7879004041258309554 ) ) ;
#148467 = CARTESIAN_POINT ( 'NONE',  ( 0.000000000000000000, 4.006659545634088992, 0.000000000000000000 ) ) ;
#148469 = ORIENTED_EDGE ( 'NONE', *, *, #151730, .F. ) ;
#148470 = CARTESIAN_POINT ( 'NONE',  ( 2.918861131495727790, -1.545587104802835565, -1.701642145805809303 ) ) ;
#148471 = CARTESIAN_POINT ( 'NONE',  ( 9.273413882067330860, 9.921330405274451536, -0.7216878364870257245 ) ) ;
#148473 = CARTESIAN_POINT ( 'NONE',  ( 1.001543065824772753E-15, -2.121874999522043836, 3.793834371823811669 ) ) ;
#148472 = CARTESIAN_POINT ( 'NONE',  ( 5.831415467653547680, 8.857049574687536619, -1.082531754730548412 ) ) ;
#148474 = CARTESIAN_POINT ( 'NONE',  ( 6.720655732516666703, 0.5845450044974825898, 1.978693153076715783 ) ) ;
#148475 = FILL_AREA_STYLE ('',( #68247 ) ) ;
#148476 = ORIENTED_EDGE ( 'NONE', *, *, #88601, .F. ) ;
#148477 = CARTESIAN_POINT ( 'NONE',  ( -11.28709712336964444, 1.000000000000000888, 3.871943585349969741 ) ) ;
#148478 = CARTESIAN_POINT ( 'NONE',  ( 4.078302138561982204, 0.9061299177482335931, 1.684124486321957104 ) ) ;
#148479 = CARTESIAN_POINT ( 'NONE',  ( 4.946200454639571475, 1.720373684868029329, 0.1241775145462056112 ) ) ;
#148480 = CARTESIAN_POINT ( 'NONE',  ( 3.766814776335784209, -0.2024620155892907503, -2.006371719556559796 ) ) ;
#148481 = CARTESIAN_POINT ( 'NONE',  ( 5.414730038718025718, -1.455890720088355961, -1.778839290973016629 ) ) ;
#148482 = CARTESIAN_POINT ( 'NONE',  ( 1.224999999999976108, 1.187500000682802037, -3.469446951953614189E-14 ) ) ;
#148483 = CARTESIAN_POINT ( 'NONE',  ( 0.2236267563471248943, -0.1037379595543522215, 2.204571545119632603 ) ) ;
#148484 = CARTESIAN_POINT ( 'NONE',  ( -3.851925040058337579, 6.547644075826416277, -1.082531754730546636 ) ) ;
#148485 = CARTESIAN_POINT ( 'NONE',  ( 5.501144674179510474, 1.447219185280288700, 1.018257267444661496 ) ) ;
#148486 = EDGE_CURVE ( 'NONE', #76973, #53173, #79153, .T. ) ;
#148488 = CARTESIAN_POINT ( 'NONE',  ( 2.027642443044708198, -1.499220162234589093, -1.734095823995058794 ) ) ;
#148487 = CARTESIAN_POINT ( 'NONE',  ( 6.574778147984297938, 6.635272358928617997, -0.7998128361456481317 ) ) ;
#148489 = CARTESIAN_POINT ( 'NONE',  ( 6.246043375366982175, 0.5822610321466625827, 1.746719530172704538 ) ) ;
#148490 = CARTESIAN_POINT ( 'NONE',  ( -3.929058411375401683, 5.999999999999998224, -0.7500000000000006661 ) ) ;
#148491 = CARTESIAN_POINT ( 'NONE',  ( 3.188928480291387313, 8.980740528189222971, 2.451733079074398969 ) ) ;
#148492 = CARTESIAN_POINT ( 'NONE',  ( -3.383641855062333281, 6.105276709951447778, -1.199719254218452047 ) ) ;
#148493 = CARTESIAN_POINT ( 'NONE',  ( 0.6801582343749917881, 1.005208333674747934, 1.178068619123807004 ) ) ;
#148494 = CARTESIAN_POINT ( 'NONE',  ( 6.602015318333181781, 0.7961593463888805289, -1.911361562896146671 ) ) ;
#148495 = CARTESIAN_POINT ( 'NONE',  ( 2.149625371984189126, 1.976669504256656218, -0.3981124878784659815 ) ) ;
#148496 = CARTESIAN_POINT ( 'NONE',  ( -1.201851678989727383E-14, 0.7437500006828187127, 1.732050807568877637 ) ) ;
#148497 = CARTESIAN_POINT ( 'NONE',  ( 5.672470344399177300, -1.220246509433765558, 1.490775554449337070 ) ) ;
#148498 = CARTESIAN_POINT ( 'NONE',  ( 0.6823417656249934904, 11.44270833367473728, 1.181850606188764807 ) ) ;
#148499 = CARTESIAN_POINT ( 'NONE',  ( 1.934110000270176322, -2.153362505827714823, 0.5451143137677332273 ) ) ;
#148500 = ORIENTED_EDGE ( 'NONE', *, *, #76635, .F. ) ;
#148501 = CARTESIAN_POINT ( 'NONE',  ( -9.579417154662856149, -9.998067499250632650, 0.08973735058633736106 ) ) ;
#148502 = CARTESIAN_POINT ( 'NONE',  ( 8.044078759455164374, -6.893137084989842123, -7.385065802799731571 ) ) ;
#148503 = CARTESIAN_POINT ( 'NONE',  ( 10.38962578677386084, 11.01565159419135043, 0.000000000000000000 ) ) ;
#148504 = CARTESIAN_POINT ( 'NONE',  ( -1.499999999999997780, 5.181250000682820378, 1.214306433183764966E-14 ) ) ;
#148505 = CARTESIAN_POINT ( 'NONE',  ( -0.6823417656250246877, -1.198958332991911790, 1.181850606188755259 ) ) ;
#148506 = CARTESIAN_POINT ( 'NONE',  ( 5.882304624916216973, -0.2641129477329319242, -1.720170474299307806 ) ) ;
#148507 = CARTESIAN_POINT ( 'NONE',  ( 3.297265573180406584, -1.731424309613574852, 0.9225008839797432802 ) ) ;
#148509 = CARTESIAN_POINT ( 'NONE',  ( -8.053180056837398126, 8.497724275839514618, 0.7216878364870578100 ) ) ;
#148508 = CARTESIAN_POINT ( 'NONE',  ( 5.684946482831785275, 5.526859072925533134, -0.7998128361456231517 ) ) ;
#148510 = CARTESIAN_POINT ( 'NONE',  ( -5.779651213448679492, 6.079991247305356339, 0.5991391260298760679 ) ) ;
#148511 = CARTESIAN_POINT ( 'NONE',  ( 4.446707141204663039, 0.5976617499744775186, 2.181999625662895959 ) ) ;
#148512 = CARTESIAN_POINT ( 'NONE',  ( 0.6958484739430546018, -1.457389369856504358, -1.459923026165359516 ) ) ;
#148513 = CARTESIAN_POINT ( 'NONE',  ( -7.751511138711140170, 10.06651563329490529, -1.599625672291263179 ) ) ;
#148514 = EDGE_CURVE ( 'NONE', #14615, #148901, #71382, .T. ) ;
#148515 = CARTESIAN_POINT ( 'NONE',  ( -4.921246571636213929, 4.843801876438091902, 0.7216878364870317197 ) ) ;
#148516 = CARTESIAN_POINT ( 'NONE',  ( 2.887862062735581326, 1.599188571496454658, 1.600737006856695288 ) ) ;
#148517 = ORIENTED_EDGE ( 'NONE', *, *, #60529, .T. ) ;
#148518 = CARTESIAN_POINT ( 'NONE',  ( -1.500000000000001332, 0.4312500006828159926, 0.000000000000000000 ) ) ;
#148519 = CARTESIAN_POINT ( 'NONE',  ( 2.143623209005097507, 0.7202431893391960660, -1.726524797105493336 ) ) ;
#148520 = CARTESIAN_POINT ( 'NONE',  ( 1.916292283401900720, -1.133531090463487212, -1.312443884513394554 ) ) ;
#148521 = CARTESIAN_POINT ( 'NONE',  ( 5.653911837654605144, 0.8871495062587383407, 2.004161502255866090 ) ) ;
#148522 = CARTESIAN_POINT ( 'NONE',  ( 0.4466624375424713689, 2.201045718399210038, 0.1599725512250807224 ) ) ;
#148523 = CARTESIAN_POINT ( 'NONE',  ( 1.639600518753115521, -1.491979387419887892, -1.421952917470001632 ) ) ;
#148524 = CARTESIAN_POINT ( 'NONE',  ( 4.031144971506396502, -1.339966268285474715, -1.405800288483616045 ) ) ;
#148525 = CARTESIAN_POINT ( 'NONE',  ( -4.406036734316898240, 6.163462161501577441, -1.443375672974051449 ) ) ;
#148526 = DIRECTION ( 'NONE',  ( 0.000000000000000000, 1.000000000000000000, 0.000000000000000000 ) ) ;
#148527 = CARTESIAN_POINT ( 'NONE',  ( 1.687500000000001110, -1.451031289061048835, 1.451031289061190055 ) ) ;
#148528 = CARTESIAN_POINT ( 'NONE',  ( 1.233697830709073795, 13.31203353598178829, 0.7436150061141216794 ) ) ;
#148529 = CARTESIAN_POINT ( 'NONE',  ( 6.643907658006512840, -0.09612306880287316280, -2.013924184692199137 ) ) ;
#148530 = CARTESIAN_POINT ( 'NONE',  ( -5.157946788997579689E-14, 1.203125000341463746, 1.570758158831762286 ) ) ;
#148531 = CARTESIAN_POINT ( 'NONE',  ( 5.045546153961558922, -1.458558117013383892, 1.392544180963309230 ) ) ;
#148532 = CARTESIAN_POINT ( 'NONE',  ( -9.775592450653132204, 11.36361159963886891, -1.199719254218441611 ) ) ;
#148533 = CARTESIAN_POINT ( 'NONE',  ( 7.096803341749390981, 10.36702210109460154, -1.199719254218441611 ) ) ;
#148534 = CARTESIAN_POINT ( 'NONE',  ( 4.309512724297349884, 6.121127159803966933, 1.599625672291261402 ) ) ;
#148536 = CARTESIAN_POINT ( 'NONE',  ( 1.284279953904121641, 2.800000000000024691, -0.7749999999999892530 ) ) ;
#148535 = CARTESIAN_POINT ( 'NONE',  ( 2.332394550857110893, 1.770734860448031300, 0.4440693575865002907 ) ) ;
#148537 = CARTESIAN_POINT ( 'NONE',  ( -1.500000000000025091, 5.170833333333355597, 0.8660254037844322683 ) ) ;
#148538 = CARTESIAN_POINT ( 'NONE',  ( -0.6125000000000123679, 1.770833334016133520, -1.060881119635941339 ) ) ;
#148539 = ORIENTED_EDGE ( 'NONE', *, *, #156570, .T. ) ;
#148540 = CARTESIAN_POINT ( 'NONE',  ( -4.950135482320914271, 8.789258806100786359, -0.7216878364870338292 ) ) ;
#148541 = UNCERTAINTY_MEASURE_WITH_UNIT (LENGTH_MEASURE( 1.000000000000000082E-05 ), #53701, 'distance_accuracy_value', 'NONE');
#148542 = CARTESIAN_POINT ( 'NONE',  ( 1.734723475976807094E-15, 14.57349900225068495, 11.91973154060107376 ) ) ;
#148543 = CARTESIAN_POINT ( 'NONE',  ( -9.969323024750229578, 10.52529837183042716, -0.7998128361456291469 ) ) ;
#148544 = CARTESIAN_POINT ( 'NONE',  ( -0.08762443420157886576, -2.019435065594810119, -0.04520711721162430641 ) ) ;
#148545 = CARTESIAN_POINT ( 'NONE',  ( 0.2586463447097427926, 2.115114616003030079, 0.1516365082330217162 ) ) ;
#148546 = ORIENTED_EDGE ( 'NONE', *, *, #85823, .F. ) ;
#148547 = CARTESIAN_POINT ( 'NONE',  ( -6.448838341955544173, 7.552674816150118708, 1.199719254218452047 ) ) ;
#148548 = CARTESIAN_POINT ( 'NONE',  ( 4.157546660884947620, 8.002221537674429896, 1.040834085586084257E-14 ) ) ;
#148549 = TOROIDAL_SURFACE ( 'NONE', #141626, 2.080000000000000071, 0.08000000000000000167 ) ;
#148550 = CARTESIAN_POINT ( 'NONE',  ( 0.1105426557568081891, -0.9253945370547181914, -1.951590883024490353 ) ) ;
#148551 = CARTESIAN_POINT ( 'NONE',  ( 4.553361389630797618, -1.314998166741451868, 1.528740011303417523 ) ) ;
#148552 = ORIENTED_EDGE ( 'NONE', *, *, #170324, .T. ) ;
#148553 = ORIENTED_EDGE ( 'NONE', *, *, #189032, .F. ) ;
#148554 =( BOUNDED_CURVE ( )  B_SPLINE_CURVE ( 2, ( #42295, #58521, #159215, #172283, #28152, #123620, #10815, #207956, #74778 ),
 .UNSPECIFIED., .F., .T. ) 
 B_SPLINE_CURVE_WITH_KNOTS ( ( 3, 2, 2, 2, 3 ),
 ( 0.1406250000000002776, 0.1458333333333333426, 0.1562500000000000000, 0.1666666666666666574, 0.1718749999999998335 ),
 .UNSPECIFIED. ) 
 CURVE ( )  GEOMETRIC_REPRESENTATION_ITEM ( )  RATIONAL_B_SPLINE_CURVE ( ( 0.9330127018922194093, 0.9330127018922229620, 1.000000000000000000, 0.8660254037844387076, 1.000000000000000000, 0.8660254037844387076, 1.000000000000000000, 0.9330127018922215187, 0.9330127018922194093 ) ) 
 REPRESENTATION_ITEM ( '' )  );
#148555 = FACE_OUTER_BOUND ( 'NONE', #32765, .T. ) ;
#148558 = ORIENTED_EDGE ( 'NONE', *, *, #92359, .F. ) ;
#148557 = CARTESIAN_POINT ( 'NONE',  ( -1.217358635584794291, 3.191465920220512231, -0.7749999999999883649 ) ) ;
#148556 = CARTESIAN_POINT ( 'NONE',  ( -6.981522756394290319, 7.109807735406931783, 0.7998128361456341429 ) ) ;
#148559 = CARTESIAN_POINT ( 'NONE',  ( 5.469253881944042384, 7.602781119232224327, 1.336104631850141944 ) ) ;
#148560 = CARTESIAN_POINT ( 'NONE',  ( 4.780624950969222020, -1.977747464269607347, 0.3905396900540994420 ) ) ;
#148561 = CARTESIAN_POINT ( 'NONE',  ( 4.347483306186128438, 1.840691044367316120, -0.04759384897683878457 ) ) ;
#148562 = CARTESIAN_POINT ( 'NONE',  ( -0.6224592253956000576, -4.250299932362466393, -0.9218689959748761487 ) ) ;
#148563 = CARTESIAN_POINT ( 'NONE',  ( 3.598509747979701690, -2.304983022191483766, -0.1141929325871558626 ) ) ;
#148564 = CARTESIAN_POINT ( 'NONE',  ( 7.842465510862060896, 8.114240948952696542, 0.000000000000000000 ) ) ;
#148565 = CARTESIAN_POINT ( 'NONE',  ( 5.290363030411685763, -2.144575937485785566, -0.2703735795691122323 ) ) ;
#148566 = CARTESIAN_POINT ( 'NONE',  ( 1.364679817366498904, 0.1413127912619481230, -1.936958241114185020 ) ) ;
#148567 = CARTESIAN_POINT ( 'NONE',  ( -3.815730167242251003, 6.539103397502874948, -1.199719254218452047 ) ) ;
#148568 = ORIENTED_EDGE ( 'NONE', *, *, #63399, .F. ) ;
#148569 = PLANE ( 'NONE',  #23949 ) ;
#148570 = CARTESIAN_POINT ( 'NONE',  ( -5.330290668828105538, 6.247702530834755130, 1.199719254218452935 ) ) ;
#148571 = CARTESIAN_POINT ( 'NONE',  ( 3.572993900519233712, 0.04689164532409998559, -1.870237235490713079 ) ) ;
#148574 = CARTESIAN_POINT ( 'NONE',  ( -5.936491157937300756, 8.019268665717216749, 1.599625672291263179 ) ) ;
#148573 = CARTESIAN_POINT ( 'NONE',  ( 1.499999999999985123, -0.9229166659838452524, -0.8660254037844323793 ) ) ;
#148572 = CARTESIAN_POINT ( 'NONE',  ( 1.160255710619631397, 1.910328232974867868, 0.09094507755665059978 ) ) ;
#148575 = CARTESIAN_POINT ( 'NONE',  ( 2.526237079854487089, -1.271617311931704686, -1.803507373242494438 ) ) ;
#148576 = CARTESIAN_POINT ( 'NONE',  ( -1.580000000000721716, 8.674529973576886377, -2.499999999999952038 ) ) ;
#148577 = CARTESIAN_POINT ( 'NONE',  ( 2.758194185376297902, 5.305311418659259814, 1.199719254218452047 ) ) ;
#148578 = CARTESIAN_POINT ( 'NONE',  ( 6.495764994278809823, 7.711385593814346073, 1.082531754730549967 ) ) ;
#148579 = CARTESIAN_POINT ( 'NONE',  ( -3.436101866059630527, 6.096203712789787232, 1.199719254218462483 ) ) ;
#148580 = CARTESIAN_POINT ( 'NONE',  ( -7.065207446052813367, 8.375735120883982532, -1.082531754730549967 ) ) ;
#148581 = CARTESIAN_POINT ( 'NONE',  ( 0.3156150085598420363, -1.934196717871897953, 0.3801348212975861895 ) ) ;
#148582 = CARTESIAN_POINT ( 'NONE',  ( 0.4116873800214932988, 2.009943462479982124, 1.133530718095694168 ) ) ;
#148583 = CARTESIAN_POINT ( 'NONE',  ( 1.750371521623844462, -1.952110535733902585, -0.1955497077021361163 ) ) ;
#148584 = CARTESIAN_POINT ( 'NONE',  ( 5.700070374860989553, 0.8410407859656986451, -1.883500665774339833 ) ) ;
#148585 = CARTESIAN_POINT ( 'NONE',  ( 3.375617060122621194, 6.882044303544283537, 1.040834085586084257E-14 ) ) ;
#148586 = CARTESIAN_POINT ( 'NONE',  ( 5.668190738965027897, 8.770583741171307679, -1.199719254218452047 ) ) ;
#148587 = VERTEX_POINT ( 'NONE', #17978 ) ;
#148588 = CARTESIAN_POINT ( 'NONE',  ( -1.201851678989727383E-14, 4.759375000341419693, -1.575800808251660134 ) ) ;
#148589 = CARTESIAN_POINT ( 'NONE',  ( -3.474999999999997868, -1.370833333333331350, 2.006292185433951047 ) ) ;
#148590 = CARTESIAN_POINT ( 'NONE',  ( 2.697709378994964879, 6.091152008895348580, 0.7216878364870338292 ) ) ;
#148591 = CARTESIAN_POINT ( 'NONE',  ( 0.6202906599508707375, 2.147645164210740365, -0.3171128231679083975 ) ) ;
#148593 = CARTESIAN_POINT ( 'NONE',  ( 6.286648950733226826, 1.598451336667701339, -0.9137711784916457969 ) ) ;
#148592 = CARTESIAN_POINT ( 'NONE',  ( 9.499606442108960991, -9.746166700193986898, -0.08647222121512777859 ) ) ;
#148594 = CARTESIAN_POINT ( 'NONE',  ( 1.749999999999999778, 0.000000000000000000, 0.000000000000000000 ) ) ;
#148595 = CARTESIAN_POINT ( 'NONE',  ( -11.91826848330605770, 12.59270354043021989, -1.400000080589191898 ) ) ;
#148596 = CARTESIAN_POINT ( 'NONE',  ( 1.211929638205839765, -0.8359089839212189288, -1.673436591668895357 ) ) ;
#148597 = CARTESIAN_POINT ( 'NONE',  ( 5.395850447034295172, -0.7835752172833524432, 2.014745138864987073 ) ) ;
#148598 = CARTESIAN_POINT ( 'NONE',  ( -6.123425537405413621, 6.005001634332811200, 0.2246051741978810634 ) ) ;
#148599 = CARTESIAN_POINT ( 'NONE',  ( -0.02264175331117677936, 4.084751018978694859, -2.643765695431527174 ) ) ;
#148600 = CARTESIAN_POINT ( 'NONE',  ( 6.395636025722083673, 6.905704815116233242, -0.7835738547974178125 ) ) ;
#148601 = CARTESIAN_POINT ( 'NONE',  ( 0.6823417656249899377, 5.488541667008087543, -1.181850606188754593 ) ) ;
#148602 = CARTESIAN_POINT ( 'NONE',  ( 1.646971982979036131, 0.1886418863925183043, 1.902964618272010799 ) ) ;
#148603 = CARTESIAN_POINT ( 'NONE',  ( 3.080641367082480819, -0.1285219475026712632, -1.765225098288242256 ) ) ;
#148604 = CARTESIAN_POINT ( 'NONE',  ( 0.7153071762652126742, 1.563590412251715911, 1.100639817434710954 ) ) ;
#148606 = CARTESIAN_POINT ( 'NONE',  ( 5.413669558995096054, -1.219043080348445329, -1.477637860945772763 ) ) ;
#148605 = CARTESIAN_POINT ( 'NONE',  ( 6.726765609221548203, -8.198316280115703236, -6.726765609221573960 ) ) ;
#148607 = CARTESIAN_POINT ( 'NONE',  ( 6.074653383054481104, 1.324031319358546677, -1.458257743282452834 ) ) ;
#148608 = CARTESIAN_POINT ( 'NONE',  ( -1.001543065824772872E-14, 5.212500000000019895, 1.732050807568877637 ) ) ;
#148609 = CARTESIAN_POINT ( 'NONE',  ( 0.7914572142167939361, -0.05789999323873443182, -2.119991495365561640 ) ) ;
#148610 = CARTESIAN_POINT ( 'NONE',  ( 2.474627113408591761, -0.3228523939998609871, -0.3300564308867471319 ) ) ;
#148611 = CARTESIAN_POINT ( 'NONE',  ( 3.572993900519233712, 0.04689164532409998559, -1.870237235490713079 ) ) ;
#148613 = ORIENTED_EDGE ( 'NONE', *, *, #176104, .F. ) ;
#148612 = CARTESIAN_POINT ( 'NONE',  ( 0.04711308451243316486, -1.408776630263553375, -1.161003007932148501 ) ) ;
#148615 = CARTESIAN_POINT ( 'NONE',  ( -5.953438849732211047, 6.118302544208587435, 0.7216878364870287221 ) ) ;
#148614 = CARTESIAN_POINT ( 'NONE',  ( 4.055453297694236348, -1.834216022232620702, -1.226887332174103173 ) ) ;
#148616 = EDGE_CURVE ( 'NONE', #168570, #103667, #95716, .T. ) ;
#148617 = CARTESIAN_POINT ( 'NONE',  ( 1.364683531249990311, 4.696875000341417916, 1.214306433183764966E-14 ) ) ;
#148618 = CARTESIAN_POINT ( 'NONE',  ( 1.996602216506689453, 2.039906831610329263, 0.3049752315822819027 ) ) ;
#148619 = CARTESIAN_POINT ( 'NONE',  ( 6.823831386379729302, 6.855558127064808716, -0.7998128361456281477 ) ) ;
#148620 = CARTESIAN_POINT ( 'NONE',  ( -9.826962411806732689, 10.35921099006301382, -0.7998128361456291469 ) ) ;
#148621 = CARTESIAN_POINT ( 'NONE',  ( 0.000000000000000000, 0.000000000000000000, 0.000000000000000000 ) ) ;
#148622 = DIRECTION ( 'NONE',  ( 0.000000000000000000, 1.000000000000000000, 0.000000000000000000 ) ) ;
#148623 = B_SPLINE_CURVE_WITH_KNOTS ( 'NONE', 3,
 ( #179828, #31448, #64982, #97526, #10901, #163583, #143104, #15165, #81253, #60732, #147332, #213361, #131137, #197126, #48764, #159303 ),
 .UNSPECIFIED., .F., .F.,
 ( 4, 3, 3, 3, 3, 4 ),
 ( 0.000000000000000000, 3.357617230303741650E-05, 6.715207102180727422E-05, 0.0001007279560762672547, 0.0001343044553218119316, 0.0001562161319167451969 ),
 .UNSPECIFIED. ) ;
#148624 = CARTESIAN_POINT ( 'NONE',  ( 6.533470333208203584, -0.1312131129157616261, 1.882018712217728318 ) ) ;
#148625 = ORIENTED_EDGE ( 'NONE', *, *, #30821, .F. ) ;
#148626 = ADVANCED_FACE ( 'NONE', ( #166386 ), #196814, .T. ) ;
#148627 = CARTESIAN_POINT ( 'NONE',  ( 3.930184216435282707, 1.147649575447948100, 1.722966636330313550 ) ) ;
#148628 = CARTESIAN_POINT ( 'NONE',  ( -1.500000000000011324, 5.170833333333356485, 0.8660254037844403729 ) ) ;
#148629 = CARTESIAN_POINT ( 'NONE',  ( 1.458524589769864210, 0.8745999688587955401, 1.976921506453344080 ) ) ;
#148630 = CARTESIAN_POINT ( 'NONE',  ( -6.171773824192762881, 6.975641918443353795, -0.9092550976456583722 ) ) ;
#148631 = CARTESIAN_POINT ( 'NONE',  ( 1.664719335976164283, 0.6358223015159381042, 1.917034779120100341 ) ) ;
#148632 = DIRECTION ( 'NONE',  ( 0.000000000000000000, -1.000000000000000000, 0.000000000000000000 ) ) ;
#148633 = VERTEX_POINT ( 'NONE', #24680 ) ;
#148635 = CARTESIAN_POINT ( 'NONE',  ( 7.782016984564049444, 11.06247500109133064, 1.082531754730557072 ) ) ;
#148634 = CARTESIAN_POINT ( 'NONE',  ( 1.001543065824772753E-15, -3.762499999999999289, 4.012584370867899430 ) ) ;
#148636 = CARTESIAN_POINT ( 'NONE',  ( 6.883263157960367806, 7.629137130509066722, 2.653810918356712900 ) ) ;
#148637 = CARTESIAN_POINT ( 'NONE',  ( -0.2058462039469660110, -0.8663896114125648751, -1.819200108291472606 ) ) ;
#148638 = CARTESIAN_POINT ( 'NONE',  ( 6.639320575229255894, 6.035237531390704291, 2.698156163645454964 ) ) ;
#148639 = CARTESIAN_POINT ( 'NONE',  ( 4.757479570170550787, 2.167726397749652367, -0.3216086267831194112 ) ) ;
#148640 = CARTESIAN_POINT ( 'NONE',  ( -1.500000000000013101, 3.910416667349482012, -0.8660254037844313801 ) ) ;
#148641 = CARTESIAN_POINT ( 'NONE',  ( 3.867365959033176814, -1.592763314076732106, -1.058159689705892692 ) ) ;
#148642 = CARTESIAN_POINT ( 'NONE',  ( -3.405069135326500351, 7.124331091189553433, 1.040834085586084257E-14 ) ) ;
#148643 = CARTESIAN_POINT ( 'NONE',  ( 4.053524740361575063, 4.791828954252362216, -1.082531754730543083 ) ) ;
#148645 = CARTESIAN_POINT ( 'NONE',  ( 1.739861462675455828, 2.010826045486389102, -0.1511602461454417123 ) ) ;
#148644 = DIRECTION ( 'NONE',  ( 0.9632918427306595976, 0.000000000000000000, 0.2684563758389253985 ) ) ;
#148646 = CARTESIAN_POINT ( 'NONE',  ( -0.6823417656250039265, 12.88020833367473017, -1.181850606188755259 ) ) ;
#148648 = CARTESIAN_POINT ( 'NONE',  ( -4.132202957115018727, 8.042930226601317401, 0.000000000000000000 ) ) ;
#148647 = CARTESIAN_POINT ( 'NONE',  ( 0.5742758271649881507, -1.267216683205124150, 1.910101658145799020 ) ) ;
#148649 = CARTESIAN_POINT ( 'NONE',  ( 3.768305045387724928, -1.158492864085089114, 1.277938026295278418 ) ) ;
#148650 = CARTESIAN_POINT ( 'NONE',  ( 6.502017186205484300, 9.743381262951846367, -1.199719254218452047 ) ) ;
#148651 = CARTESIAN_POINT ( 'NONE',  ( 4.871457266011829823, 4.577788319968905562, -0.7998128361456221525 ) ) ;
#148652 = CARTESIAN_POINT ( 'NONE',  ( -1.270916165646603035, 2.916024509562820111, -0.7749999999999892530 ) ) ;
#148653 = CARTESIAN_POINT ( 'NONE',  ( -1.500000000000022204, 7.388542872122518368, 4.154462424328226433 ) ) ;
#148654 = CARTESIAN_POINT ( 'NONE',  ( 3.704402285031850539, 5.344888637335695414, -1.599625672291262513 ) ) ;
#148655 = CARTESIAN_POINT ( 'NONE',  ( 0.07556134207193675179, -0.004209888911949499594, -2.244269416743961187 ) ) ;
#148656 = VERTEX_POINT ( 'NONE', #58268 ) ;
#148657 = FACE_OUTER_BOUND ( 'NONE', #48779, .T. ) ;
#148658 = VERTEX_POINT ( 'NONE', #149639 ) ;
#148659 = CARTESIAN_POINT ( 'NONE',  ( 5.479120714502029976, -1.640381486070506156, -0.7687909062009666838 ) ) ;
#148660 = ORIENTED_EDGE ( 'NONE', *, *, #55578, .T. ) ;
#148661 = CARTESIAN_POINT ( 'NONE',  ( 6.364626766972446781, 6.390095747748157251, 0.7998128361456352531 ) ) ;
#148663 = EDGE_CURVE ( 'NONE', #177025, #205532, #155771, .T. ) ;
#148662 = CARTESIAN_POINT ( 'NONE',  ( 6.777912011469600095, -7.189630408300057951, -6.776323704810597981 ) ) ;
#148664 = CARTESIAN_POINT ( 'NONE',  ( 5.531847899045232886, -1.765878665049234186, 0.4030928165594855339 ) ) ;
#148665 = CARTESIAN_POINT ( 'NONE',  ( 5.628043163004202931, 8.619781885929965526, -1.082531754730548412 ) ) ;
#148666 = CARTESIAN_POINT ( 'NONE',  ( 2.278644679984271892, 5.611497393830711111, -0.5843877675706611319 ) ) ;
#148667 = CARTESIAN_POINT ( 'NONE',  ( 4.762865522572231392, 6.775349848016087861, -1.243673390893657471 ) ) ;
#148669 = CARTESIAN_POINT ( 'NONE',  ( -1.364683531250000748, 15.35937500034140157, 0.000000000000000000 ) ) ;
#148668 = CARTESIAN_POINT ( 'NONE',  ( 6.426204213344836269, 0.9576725794440078543, 1.595564698446788388 ) ) ;
#148670 = CARTESIAN_POINT ( 'NONE',  ( 3.620622283765279725, 0.2843237153829519248, 1.894267977526209012 ) ) ;
#148671 = CARTESIAN_POINT ( 'NONE',  ( 0.000000000000000000, -1.600000000000000755, 0.000000000000000000 ) ) ;
#148672 = ADVANCED_FACE ( 'NONE', ( #7355 ), #1221, .T. ) ;
#148673 = CARTESIAN_POINT ( 'NONE',  ( -1.500000000000008216, 11.99999999999999645, 3.469446951953614189E-15 ) ) ;
#148674 = CARTESIAN_POINT ( 'NONE',  ( 1.364683531249984538, -1.094791666325247936, -0.7879004041258309554 ) ) ;
#148675 = CARTESIAN_POINT ( 'NONE',  ( 6.534666852106798096, 7.686494751288491578, -1.082531754730543083 ) ) ;
#148677 = CARTESIAN_POINT ( 'NONE',  ( 5.911343334927605220, -1.992878553188395463, 0.7155076844978009998 ) ) ;
#148676 = CARTESIAN_POINT ( 'NONE',  ( -8.500599126088349777, 12.86119004717103209, 1.040834085586084257E-14 ) ) ;
#148678 = CARTESIAN_POINT ( 'NONE',  ( 0.3390366800232989530, 0.3710982241871863541, 2.129449491308422537 ) ) ;
#148679 = CARTESIAN_POINT ( 'NONE',  ( -4.990283058281743678, 7.979691447040783814, -1.199719254218453823 ) ) ;
#148680 = CARTESIAN_POINT ( 'NONE',  ( 4.634908411025333130, 6.500755460986618495, 1.599625672291268286 ) ) ;
#148681 = CARTESIAN_POINT ( 'NONE',  ( 0.9030137451815029026, 1.489685209907613439, 1.054989265776705709 ) ) ;
#148682 = CARTESIAN_POINT ( 'NONE',  ( -4.952806187693842510, 4.672695395264567786, 0.7998128361456341429 ) ) ;
#148683 = CARTESIAN_POINT ( 'NONE',  ( 3.627796970749700201, -1.086779551322129445, -1.466705181690882709 ) ) ;
#148684 = CARTESIAN_POINT ( 'NONE',  ( 8.356287327758902705, 13.10650915898924751, 8.534003350902178653 ) ) ;
#148685 = VERTEX_POINT ( 'NONE', #90786 ) ;
#148686 = CARTESIAN_POINT ( 'NONE',  ( 2.435944266227826116, 1.209484882827957630, 1.554366883019624668 ) ) ;
#148687 = CARTESIAN_POINT ( 'NONE',  ( 5.196799823744689739, 1.589972550305688070, 1.114921412299192172 ) ) ;
#148688 = CARTESIAN_POINT ( 'NONE',  ( -5.327428015527048366, 5.180030537728460338, -0.7998128361456362523 ) ) ;
#148690 = CARTESIAN_POINT ( 'NONE',  ( 4.992489932941452935, -1.175987964647656536, 1.764448611491518548 ) ) ;
#148689 = CARTESIAN_POINT ( 'NONE',  ( 7.018280793729500644, 8.217024343219755167, -1.199719254218452047 ) ) ;
#148691 = FACE_OUTER_BOUND ( 'NONE', #184594, .T. ) ;
#148692 = CARTESIAN_POINT ( 'NONE',  ( 2.525908831824146716, -1.891188341833284881, 0.2824699455093656053 ) ) ;
#148693 = CARTESIAN_POINT ( 'NONE',  ( 6.046415161660691595, 6.058605959254545148, 0.4744590674741564484 ) ) ;
#148694 = CARTESIAN_POINT ( 'NONE',  ( -2.550000000000000266, -7.105553651663779391, -1.849324200890692271 ) ) ;
#148695 = CARTESIAN_POINT ( 'NONE',  ( 4.797606254389322089, 6.690569611577942943, 1.599625672291268286 ) ) ;
#148696 = CARTESIAN_POINT ( 'NONE',  ( 4.847203612085560387, 5.613824621309978724, -1.199719254218452047 ) ) ;
#148697 = CARTESIAN_POINT ( 'NONE',  ( 3.756497301808682465, 2.003587623774540472, 0.1952383342433745284 ) ) ;
#148698 = CARTESIAN_POINT ( 'NONE',  ( 0.07933194154487524519, -9.900000000000005684, 9.499668754385634628 ) ) ;
#148699 = CARTESIAN_POINT ( 'NONE',  ( 4.635264976507449397, -1.668059998867366778, 0.7425182445051290436 ) ) ;
#148700 = CARTESIAN_POINT ( 'NONE',  ( 0.3794556558127279433, -0.1030994254981998093, 2.067933115924729837 ) ) ;
#148701 = CARTESIAN_POINT ( 'NONE',  ( -7.375272376154077492, 11.54830883891436422, -0.7216878364870267237 ) ) ;
#148702 = CARTESIAN_POINT ( 'NONE',  ( -6.606676129765223671, 6.763588582595081000, -0.1820296311667093936 ) ) ;
#148703 = CARTESIAN_POINT ( 'NONE',  ( 0.9311234436981579154, -2.859380368602566502, -3.474999999999996536 ) ) ;
#148704 = CARTESIAN_POINT ( 'NONE',  ( 5.664887262500884368, -1.691755685069219695, -0.7986314380193232365 ) ) ;
#148705 = CARTESIAN_POINT ( 'NONE',  ( 7.100719765255169236, 9.307259030929609267, -1.599625672291262513 ) ) ;
#148706 = CARTESIAN_POINT ( 'NONE',  ( -3.262708522383007903, 6.958243709422141876, 1.040834085586084257E-14 ) ) ;
#148707 = CARTESIAN_POINT ( 'NONE',  ( 3.999819011231439347, 4.625209253646830554, 1.199719254218464037 ) ) ;
#148708 = CARTESIAN_POINT ( 'NONE',  ( 1.364683531249997417, 10.54687500034139802, 2.602085213965210642E-15 ) ) ;
#148709 = CARTESIAN_POINT ( 'NONE',  ( -6.586563698140583512, 6.578745824119123675, 1.040834085586084257E-14 ) ) ;
#148710 = CARTESIAN_POINT ( 'NONE',  ( 4.681643115420508039, 4.356338477612361260, 0.7998128361456341429 ) ) ;
#148711 = AXIS2_PLACEMENT_3D ( 'NONE', #160092, #193647, #27958 ) ;
#148712 = CARTESIAN_POINT ( 'NONE',  ( -2.984203208339354152, 6.495671153122273722, 0.000000000000000000 ) ) ;
#148713 = CARTESIAN_POINT ( 'NONE',  ( -6.338600509588822263, 7.353787668397130162, -1.199719254218446718 ) ) ;
#148714 = CARTESIAN_POINT ( 'NONE',  ( 6.789883322502159757, -1.411316560962400768, -1.649898940422918514 ) ) ;
#148715 = CARTESIAN_POINT ( 'NONE',  ( 2.443091204979094044, -1.843612287508783920, -1.040880819149572201 ) ) ;
#148716 = CARTESIAN_POINT ( 'NONE',  ( 9.185812768458653466, 10.67553530374532045, 1.199719254218453823 ) ) ;
#148717 = CARTESIAN_POINT ( 'NONE',  ( -1.772846837484827631, 2.502368107626190774, 2.500000000000000444 ) ) ;
#148718 = CARTESIAN_POINT ( 'NONE',  ( 6.034052368894809781, 1.228512962337786396, 1.666229478724051027 ) ) ;
#148719 = CARTESIAN_POINT ( 'NONE',  ( 4.597200498174307981, 6.922409349013787683, -1.201048452015600843 ) ) ;
#148720 = CARTESIAN_POINT ( 'NONE',  ( 4.338245966692901412, 8.005111361209628740, -0.7216878364870197293 ) ) ;
#148722 = DIRECTION ( 'NONE',  ( 2.949029909160572061E-17, 1.000000000000000000, -8.673600428462541149E-15 ) ) ;
#148721 = CARTESIAN_POINT ( 'NONE',  ( 11.33772463945036968, 10.09097530385349728, -3.600000000000000977 ) ) ;
#148723 = CARTESIAN_POINT ( 'NONE',  ( 2.185838763446645849, -0.9780977115210144346, 2.073240998862643458 ) ) ;
#148725 = DIRECTION ( 'NONE',  ( 0.000000000000000000, 1.000000000000000000, 0.000000000000000000 ) ) ;
#148724 = CARTESIAN_POINT ( 'NONE',  ( -3.147653791585948380, 8.919999999999841833, 2.500000000000000444 ) ) ;
#148726 = CARTESIAN_POINT ( 'NONE',  ( 2.619282413590624525, 1.617716081779559278, 1.019604094833974628 ) ) ;
#148727 = ORIENTED_EDGE ( 'NONE', *, *, #63358, .F. ) ;
#148728 = CARTESIAN_POINT ( 'NONE',  ( 6.412643469139427843, 10.42524178073059993, -0.7216878364870267237 ) ) ;
#148729 =( BOUNDED_CURVE ( )  B_SPLINE_CURVE ( 2, ( #89699, #155749, #7334, #73411, #156825, #8412, #124399 ),
 .UNSPECIFIED., .F., .T. ) 
 B_SPLINE_CURVE_WITH_KNOTS ( ( 3, 2, 2, 3 ),
 ( 0.07142857142857149400, 0.07738095238095236972, 0.08333333333333324544, 0.08928571428571412116 ),
 .UNSPECIFIED. ) 
 CURVE ( )  GEOMETRIC_REPRESENTATION_ITEM ( )  RATIONAL_B_SPLINE_CURVE ( ( 0.9999999999999984457, 0.8660254037844402619, 1.000000000000000000, 0.8660254037844387076, 1.000000000000000000, 0.8660254037844424824, 0.9999999999999962252 ) ) 
 REPRESENTATION_ITEM ( '' )  );
#148730 = CARTESIAN_POINT ( 'NONE',  ( 0.1936082253880376802, 1.876963271429439750, -0.7284200309826213138 ) ) ;
#148731 = CARTESIAN_POINT ( 'NONE',  ( 1.076917802502619592, 1.810449747239597951, 0.7559744942375111743 ) ) ;
#148732 = CARTESIAN_POINT ( 'NONE',  ( 0.2333690889706682703, 0.003390530909083006028, -2.053566628440507635 ) ) ;
#148733 = CARTESIAN_POINT ( 'NONE',  ( -7.283754839039664475, 9.520799950344851936, -1.599625672291263179 ) ) ;
#148734 = CARTESIAN_POINT ( 'NONE',  ( -3.285556943749998737, -0.5177083328553757635, 1.896917185911908499 ) ) ;
#148736 = CARTESIAN_POINT ( 'NONE',  ( 2.588433964080754546, -0.3000524435079615637, -1.744042203426913629 ) ) ;
#148735 = CARTESIAN_POINT ( 'NONE',  ( 3.925792317461401559, 1.118293097838483074, -1.766204078809136657 ) ) ;
#148737 = CARTESIAN_POINT ( 'NONE',  ( 3.980184376345591968, 7.587372839137763059, -0.2953998019899722882 ) ) ;
#148738 = EDGE_CURVE ( 'NONE', #86356, #182295, #140716, .T. ) ;
#148739 = CARTESIAN_POINT ( 'NONE',  ( 5.543040349607136541, -1.804139640619137230, -1.413977440569001542 ) ) ;
#148740 = CARTESIAN_POINT ( 'NONE',  ( 3.960698422707895627, 0.2102999545306425688, -1.727497421908174458 ) ) ;
#148741 = CARTESIAN_POINT ( 'NONE',  ( 7.892817981449907982, 12.36003807833360391, 0.7998128361456462443 ) ) ;
#148742 = CARTESIAN_POINT ( 'NONE',  ( 6.384963997392946844, 6.413822516572072807, 0.7998128361456350310 ) ) ;
#148743 = CARTESIAN_POINT ( 'NONE',  ( 3.075252150474018009, 1.257817891742564642, -1.193625562640305615 ) ) ;
#148744 = CARTESIAN_POINT ( 'NONE',  ( 4.861888260954045471, -0.5834894554452072502, 2.091229948656031734 ) ) ;
#148745 = CARTESIAN_POINT ( 'NONE',  ( 3.011882680530176604, 6.665613560593854459, 0.7998128361456341429 ) ) ;
#148746 = CARTESIAN_POINT ( 'NONE',  ( 5.770720322323381168, -0.3006437417610394736, -1.993894057904864514 ) ) ;
#148747 = CARTESIAN_POINT ( 'NONE',  ( 6.562500042754934704, -1.451030237095789266, -1.451031289060847440 ) ) ;
#148748 = CARTESIAN_POINT ( 'NONE',  ( 1.499999999999990896, 3.806250000682819046, 1.214306433183764966E-14 ) ) ;
#148749 = CARTESIAN_POINT ( 'NONE',  ( 2.327063250521405724, -0.002089543651138252821, 1.926566264030280307 ) ) ;
#148750 = CARTESIAN_POINT ( 'NONE',  ( -1.500000000000015099, 9.760416667349467446, -0.8660254037844309360 ) ) ;
#148751 = CARTESIAN_POINT ( 'NONE',  ( 5.396815004230996138, -2.167347303010109805, -0.4865036897706440100 ) ) ;
#148752 = ORIENTED_EDGE ( 'NONE', *, *, #1852, .T. ) ;
#148753 = CARTESIAN_POINT ( 'NONE',  ( 6.983263157960335477, 4.692686028926381425, 2.608776679625654182 ) ) ;
#148754 = CARTESIAN_POINT ( 'NONE',  ( -1.201851678989727383E-14, 1.712500000000019229, 1.732050807568877637 ) ) ;
#148755 = CARTESIAN_POINT ( 'NONE',  ( 7.122110765880372618, 7.203550736482235095, 0.7998128361456341429 ) ) ;
#148756 = CARTESIAN_POINT ( 'NONE',  ( 4.568734577680873876, 6.353276312092901890, -1.443375672974051449 ) ) ;
#148758 = CARTESIAN_POINT ( 'NONE',  ( 6.795372052238223048, -1.752927774724974297, 0.8811163259476796350 ) ) ;
#148757 = MECHANICAL_DESIGN_GEOMETRIC_PRESENTATION_REPRESENTATION (  '', ( #83029 ), #141993 ) ;
#148759 = CARTESIAN_POINT ( 'NONE',  ( 7.565086526745395723, 10.80938946696957004, -1.082531754730543083 ) ) ;
#148760 = CARTESIAN_POINT ( 'NONE',  ( 0.4461838333975307602, 2.877219473291476426, 1.949594826320503849 ) ) ;
#148761 = CARTESIAN_POINT ( 'NONE',  ( 3.718679271898170491, 7.560485927181699317, 0.7998128361456271485 ) ) ;
#148762 = CARTESIAN_POINT ( 'NONE',  ( 0.1412502902482688505, 0.7743183493036235321, 1.862015731718666078 ) ) ;
#148763 = CARTESIAN_POINT ( 'NONE',  ( 4.369619704168957952, -0.3557292467365941180, 2.031631830423554774 ) ) ;
#148764 = CARTESIAN_POINT ( 'NONE',  ( -2.740719608256871442, 6.349256642941639051, 0.7998128361456341429 ) ) ;
#148765 = CARTESIAN_POINT ( 'NONE',  ( 0.7499999999999920064, 5.514583334016151639, 1.299038105676669330 ) ) ;
#148766 = CARTESIAN_POINT ( 'NONE',  ( -1.402160292154681736E-14, 0.3218750003414227456, 1.575800808251672791 ) ) ;
#148767 = CARTESIAN_POINT ( 'NONE',  ( 5.518772846390051612, 1.727975122137341613, 0.7167417953098526029 ) ) ;
#148768 = CARTESIAN_POINT ( 'NONE',  ( 5.273917847569165929, 1.525789468548454986, -0.8241785451228255122 ) ) ;
#148769 = CARTESIAN_POINT ( 'NONE',  ( 5.003314770209169815, -1.731378854590956307, 0.1774945436790342501 ) ) ;
#148770 = CARTESIAN_POINT ( 'NONE',  ( 3.684065054611349144, 5.321161868511784299, -1.599625672291262513 ) ) ;
#148771 = CARTESIAN_POINT ( 'NONE',  ( 1.804612524702827514, 1.695363242818634930, -1.543121881923440020 ) ) ;
#148772 = CARTESIAN_POINT ( 'NONE',  ( -1.364683531249997417, 5.571875000341417916, 1.214306433183764966E-14 ) ) ;
#148773 = CARTESIAN_POINT ( 'NONE',  ( 5.284749326355624888, 1.843379893440146633, -0.9865243283948360586 ) ) ;
#148774 = CARTESIAN_POINT ( 'NONE',  ( 0.6558947131179297951, -1.335331635844772880, 1.267786537210900510 ) ) ;
#148775 = CARTESIAN_POINT ( 'NONE',  ( -0.4000000000000408229, 3.949999999999971756, 0.8338124244295227472 ) ) ;
#148776 = CARTESIAN_POINT ( 'NONE',  ( 1.600232647554021392, -0.2440283035436350279, 2.001511509883910911 ) ) ;
#148777 = CARTESIAN_POINT ( 'NONE',  ( 0.000000000000000000, -8.407420853759283830, 10.91970695577495931 ) ) ;
#148778 = CARTESIAN_POINT ( 'NONE',  ( 7.913958811377831637, 15.96374183207315944, -9.911989391671550464 ) ) ;
#148779 = CARTESIAN_POINT ( 'NONE',  ( -7.888146445052511169, 8.097259028849730811, 1.040834085586084257E-14 ) ) ;
#148780 = CARTESIAN_POINT ( 'NONE',  ( 3.683011284406639607, 7.448596931783069586, 0.7998128361456321445 ) ) ;
#148781 = CARTESIAN_POINT ( 'NONE',  ( 0.6801582343749952297, 2.807291667008070313, -1.178068619123883165 ) ) ;
#148782 = CARTESIAN_POINT ( 'NONE',  ( 3.299587915756982515, 1.916203934664402198, -0.9084051299479002362 ) ) ;
#148783 = CARTESIAN_POINT ( 'NONE',  ( 0.6823417656249864960, -1.073958332991911568, -1.181850606188749264 ) ) ;
#148784 = CARTESIAN_POINT ( 'NONE',  ( 5.900976575431972293, 1.489821718068456979, -1.054992404821846863 ) ) ;
#148785 = ORIENTED_EDGE ( 'NONE', *, *, #182043, .F. ) ;
#148786 = CARTESIAN_POINT ( 'NONE',  ( -5.061990249855848667, 6.999017606288844284, -1.599625672291271394 ) ) ;
#148787 = FACE_OUTER_BOUND ( 'NONE', #53271, .T. ) ;
#148788 = CARTESIAN_POINT ( 'NONE',  ( 7.038091138825468107, 8.344099429118761790, -1.082531754730548412 ) ) ;
#148789 = CARTESIAN_POINT ( 'NONE',  ( -3.475000000000000533, -2.785416665710751527, -2.006292185433948827 ) ) ;
#148790 = CARTESIAN_POINT ( 'NONE',  ( -5.018489415352746619, 9.006654751220198207, 0.7998128361456481317 ) ) ;
#148791 = CARTESIAN_POINT ( 'NONE',  ( 3.410420005539113841, -2.017668111602511694, -0.09479391224248739922 ) ) ;
#148792 = CARTESIAN_POINT ( 'NONE',  ( 6.616270032800761314, -1.034323699838369359, -1.949367651511712207 ) ) ;
#148793 = CARTESIAN_POINT ( 'NONE',  ( -6.656127069666307072, 6.730179434224282886, 0.7998128361456341429 ) ) ;
#148794 = CARTESIAN_POINT ( 'NONE',  ( 8.380911511541880188, 12.92948053010758258, 0.7998128361456462443 ) ) ;
#148795 = CARTESIAN_POINT ( 'NONE',  ( 4.715577910371310466, 0.4106090485030155501, -1.814890118206938574 ) ) ;
#148796 = CARTESIAN_POINT ( 'NONE',  ( 8.860417081730671995, 10.29590700256267155, 1.199719254218453823 ) ) ;
#148797 = CARTESIAN_POINT ( 'NONE',  ( 3.344425985610775864, 6.383782420805063751, 0.9919173777418579530 ) ) ;
#148798 = CARTESIAN_POINT ( 'NONE',  ( -3.898132859128961236, 4.506575409527250997, -1.199719254218452047 ) ) ;
#148799 = AXIS2_PLACEMENT_3D ( 'NONE', #140273, #203071, #54715 ) ;
#148800 = CARTESIAN_POINT ( 'NONE',  ( -6.995117189646935962, 10.24838825697502109, 1.199719254218453823 ) ) ;
#148801 = CARTESIAN_POINT ( 'NONE',  ( 6.719606831986117967, -1.999679869198322413, 0.4981698227890380970 ) ) ;
#148803 = CARTESIAN_POINT ( 'NONE',  ( -5.283800884368243800, 6.573997454655339467, 1.390413726763789937 ) ) ;
#148802 = CARTESIAN_POINT ( 'NONE',  ( -5.264308783856126439, 9.363720357799287797, -0.7998128361456362523 ) ) ;
#148804 = CARTESIAN_POINT ( 'NONE',  ( -0.6823417656250003738, 0.7177083336747519526, -1.181850606188749264 ) ) ;
#148805 = CARTESIAN_POINT ( 'NONE',  ( 1.369977976685434751, -0.4280273037657927881, 1.680018549819038531 ) ) ;
#148806 = CARTESIAN_POINT ( 'NONE',  ( 0.7787878715554141795, 1.165832476461704292, 1.292284986363402055 ) ) ;
#148808 = CARTESIAN_POINT ( 'NONE',  ( 6.968527767744088663, 11.07377346243604599, 0.7216878364870438212 ) ) ;
#148807 = CARTESIAN_POINT ( 'NONE',  ( 0.4996044509122186672, 1.916167126895538031, -1.285522792546058390 ) ) ;
#148809 = CARTESIAN_POINT ( 'NONE',  ( 6.533977301828627127, 6.812828965020023553, -0.5176801306737014441 ) ) ;
#148810 = CARTESIAN_POINT ( 'NONE',  ( 2.302092711735738373, -2.060399031734764463, 0.04731154407941646350 ) ) ;
#148811 = CARTESIAN_POINT ( 'NONE',  ( 0.8782795706883707032, -0.2985837142155840507, 1.993765709762222782 ) ) ;
#148812 = CARTESIAN_POINT ( 'NONE',  ( 0.000000000000000000, 13.49999999999999822, 0.000000000000000000 ) ) ;
#148813 = CARTESIAN_POINT ( 'NONE',  ( -5.123001941117347080, 7.070197912760590064, 1.599625672291263179 ) ) ;
#148814 = CARTESIAN_POINT ( 'NONE',  ( 0.5847652604651293329, -0.2391135408384200411, -1.956842742423828829 ) ) ;
#148816 = CARTESIAN_POINT ( 'NONE',  ( -6.400857919427531684, 9.521399101757175742, 1.082531754730549967 ) ) ;
#148815 = CARTESIAN_POINT ( 'NONE',  ( 4.658414424252744546, 1.907665749568526747, 0.1350064596054162680 ) ) ;
#148817 = CARTESIAN_POINT ( 'NONE',  ( 6.727182134110200273, -0.004969159814478123736, 2.189081792362323586 ) ) ;
#148818 = CARTESIAN_POINT ( 'NONE',  ( -5.899206235277530297, 9.896508017883515862, 0.7216878364870267237 ) ) ;
#148819 = CARTESIAN_POINT ( 'NONE',  ( 6.502017186205484300, 9.743381262951846367, -1.199719254218452047 ) ) ;
#148820 = CARTESIAN_POINT ( 'NONE',  ( -8.093291352714894415, 8.406871097780989288, -0.7998128361456362523 ) ) ;
#148821 = CARTESIAN_POINT ( 'NONE',  ( 0.3815177477655702920, 0.1955376695662625619, -2.010167716959633033 ) ) ;
#148822 = ORIENTED_EDGE ( 'NONE', *, *, #72042, .T. ) ;
#148823 = CARTESIAN_POINT ( 'NONE',  ( 4.383989010750934945, 1.503879422573949132, 1.750323999079455684 ) ) ;
#148824 = CARTESIAN_POINT ( 'NONE',  ( 4.967221142815226642, 1.706001049663580460, 0.9686458024478412643 ) ) ;
#148825 = CARTESIAN_POINT ( 'NONE',  ( 1.463640819124707004, -0.4818986642843925972, 1.901505326443528876 ) ) ;
#148826 = CARTESIAN_POINT ( 'NONE',  ( 8.374132434735052755, 12.92157160716627295, -0.7998128361456352531 ) ) ;
#148827 = CARTESIAN_POINT ( 'NONE',  ( -9.453965129859655647, 15.47074423828725109, 7.390745084306966639 ) ) ;
#148828 = ORIENTED_EDGE ( 'NONE', *, *, #171612, .T. ) ;
#148829 = CARTESIAN_POINT ( 'NONE',  ( 0.02287343425391458532, 0.3688939426326736104, 2.084831875159770753 ) ) ;
#148831 = CARTESIAN_POINT ( 'NONE',  ( -8.507905087775398556, 9.884643009614800135, 1.199719254218462483 ) ) ;
#148830 = CARTESIAN_POINT ( 'NONE',  ( -3.978428010606240850, 6.728917548094202949, -1.199719254218452047 ) ) ;
#148832 = CARTESIAN_POINT ( 'NONE',  ( 0.4449246239494052402, 0.5802587426733482046, -1.747387232072565189 ) ) ;
#148833 = EDGE_LOOP ( 'NONE', ( #149826, #131740, #33895, #11429 ) ) ;
#148834 = CARTESIAN_POINT ( 'NONE',  ( 4.346645206408905615, -2.146589105242337592, -0.3245344146646060302 ) ) ;
#148835 = CARTESIAN_POINT ( 'NONE',  ( 9.905912401576173920, 11.51299872167799343, -6.694621976437109545 ) ) ;
#148836 = CARTESIAN_POINT ( 'NONE',  ( 2.127334043950947606, 1.896359100603739911, 0.9491756072362851349 ) ) ;
#148837 = CARTESIAN_POINT ( 'NONE',  ( 1.499999999999989120, 3.035416667349485564, 0.8660254037844524744 ) ) ;
#148838 = CARTESIAN_POINT ( 'NONE',  ( 7.727257484784855635, 11.10255193463598111, -1.199719254218446718 ) ) ;
#148839 = CARTESIAN_POINT ( 'NONE',  ( -0.4373225248172993851, -5.223431457505089526, -10.96785329849811497 ) ) ;
#148840 = CARTESIAN_POINT ( 'NONE',  ( 6.410638904775656677, 6.895589754593423493, 0.7569561588358000304 ) ) ;
#148841 = CARTESIAN_POINT ( 'NONE',  ( 2.442714938195661212, 0.4483736453565168589, 2.011251146304892767 ) ) ;
#148843 = CARTESIAN_POINT ( 'NONE',  ( 7.402824606385355111, 14.51624126053141595, -9.389026765318357448 ) ) ;
#148842 = CARTESIAN_POINT ( 'NONE',  ( -7.669108446824431269, 12.09904362127053545, -0.7998128361456291469 ) ) ;
#148844 = CARTESIAN_POINT ( 'NONE',  ( -1.364683531250012516, 3.530208333674758059, 0.7879004041258379498 ) ) ;
#148845 = CARTESIAN_POINT ( 'NONE',  ( 0.07755575628181145265, 0.2276780653837663093, -2.222404768597834757 ) ) ;
#148846 = CARTESIAN_POINT ( 'NONE',  ( 5.802484273800978087, 7.324075294900190158, -1.340195914752571271 ) ) ;
#148847 = CARTESIAN_POINT ( 'NONE',  ( 5.004515039866801906, -1.898294113557968510, -0.2302225566794338651 ) ) ;
#148848 = CARTESIAN_POINT ( 'NONE',  ( 11.84668729410392274, 12.59379487675467324, -1.400000000000001688 ) ) ;
#148849 = CARTESIAN_POINT ( 'NONE',  ( 1.862946185591638049, -1.600570176636705089, 1.599199478044037059 ) ) ;
#148850 = CARTESIAN_POINT ( 'NONE',  ( -4.451154503988200339, 4.087435097607984957, 1.214306433183764966E-14 ) ) ;
#148851 = CARTESIAN_POINT ( 'NONE',  ( 0.9842725786804270571, -1.148342222048874595, 1.401147620581437048 ) ) ;
#148852 = EDGE_CURVE ( 'NONE', #71330, #201806, #170721, .T. ) ;
#148853 = CARTESIAN_POINT ( 'NONE',  ( 1.551812156574260637, 0.9880582627100834570, 1.641127140810652252 ) ) ;
#148854 = CARTESIAN_POINT ( 'NONE',  ( 3.279797552538410876, -1.996039814156633785, 0.5495672325947635883 ) ) ;
#148855 = CARTESIAN_POINT ( 'NONE',  ( -1.364683531250012516, 1.092708333674754506, 0.7879004041258379498 ) ) ;
#148856 = CARTESIAN_POINT ( 'NONE',  ( 1.006637970050362929, 1.494420418981519338, -1.285951363188575058 ) ) ;
#148857 = CARTESIAN_POINT ( 'NONE',  ( 6.076777883369302913, -1.830186849185039044, -0.6017253874085000120 ) ) ;
#148859 = CARTESIAN_POINT ( 'NONE',  ( 5.318333368960210805, 7.618274611128187601, -1.232678415538956518 ) ) ;
#148858 = CARTESIAN_POINT ( 'NONE',  ( 1.419075709855713630, 1.546787523640520856, -1.712735560227249820 ) ) ;
#148860 = EDGE_CURVE ( 'NONE', #71636, #179842, #183361, .T. ) ;
#148861 = CARTESIAN_POINT ( 'NONE',  ( 1.364683531249986537, 1.113541667008082658, 0.7879004041258500513 ) ) ;
#148862 = CARTESIAN_POINT ( 'NONE',  ( 5.230950406320217461, -1.941087326682365832, -0.6980428833110083886 ) ) ;
#148863 = CARTESIAN_POINT ( 'NONE',  ( -4.791917227426195858, 7.677988301050826969, -1.199719254218452047 ) ) ;
#148864 = CARTESIAN_POINT ( 'NONE',  ( 5.750629710490689384, 9.860818428881154674, -0.7998128361456291469 ) ) ;
#148865 = CARTESIAN_POINT ( 'NONE',  ( 0.000000000000000000, 6.468705557303652931, -4.925226524755051294 ) ) ;
#148867 = CARTESIAN_POINT ( 'NONE',  ( -0.7500000000000215383, 4.441666666666691299, 1.299038105676671107 ) ) ;
#148866 = CARTESIAN_POINT ( 'NONE',  ( 5.772525194315006658, -1.338739070262290110, 1.625669279078660878 ) ) ;
#148868 = CARTESIAN_POINT ( 'NONE',  ( -1.402160292154681736E-14, 2.509375000341417028, -1.575800808251660134 ) ) ;
#148869 = CARTESIAN_POINT ( 'NONE',  ( 4.763041337456088264, -1.928505312680216521, -0.9765951867335493919 ) ) ;
#148870 = CARTESIAN_POINT ( 'NONE',  ( 5.865880358592049149, 0.5843737978505449959, -1.933295926576389379 ) ) ;
#148871 = FACE_OUTER_BOUND ( 'NONE', #150582, .T. ) ;
#148872 = CARTESIAN_POINT ( 'NONE',  ( -6.426201623197489887, 6.599582769926260362, 0.7216878364870317197 ) ) ;
#148873 = PRODUCT_DEFINITION_SHAPE ( 'NONE', 'NONE',  #19950 ) ;
#148874 = ADVANCED_FACE ( 'NONE', ( #92927 ), #209827, .F. ) ;
#148877 = CARTESIAN_POINT ( 'NONE',  ( 6.317736394288147039, 6.473040002865377396, 0.7216878364870317197 ) ) ;
#148876 = CARTESIAN_POINT ( 'NONE',  ( 0.000000000000000000, -1.946874999522044014, -3.793834371823813001 ) ) ;
#148875 = CARTESIAN_POINT ( 'NONE',  ( 7.862802741282558294, 8.137967717776607657, 0.000000000000000000 ) ) ;
#148878 = CARTESIAN_POINT ( 'NONE',  ( -4.655245641445871385, 6.524482229810530498, 1.599625672291263179 ) ) ;
#148879 = CARTESIAN_POINT ( 'NONE',  ( 3.362517798112668821, -1.944730434982215650, -0.5331690889110105580 ) ) ;
#148880 = CARTESIAN_POINT ( 'NONE',  ( -8.015895134177625891, 10.37496362800581018, 1.599625672291295375 ) ) ;
#148882 = DIRECTION ( 'NONE',  ( 7.387867266669436732E-31, -1.000000000000000000, -8.546850786086424434E-32 ) ) ;
#148881 = CARTESIAN_POINT ( 'NONE',  ( -8.649738815838677652, 13.03518635187974262, 0.7216878364870357165 ) ) ;
#148883 = CARTESIAN_POINT ( 'NONE',  ( 1.364683531249992088, 5.634375000341417916, 1.214306433183764966E-14 ) ) ;
#148885 = DIRECTION ( 'NONE',  ( -0.6507913734559640506, -0.7592566023653003482, 0.000000000000000000 ) ) ;
#148884 = CARTESIAN_POINT ( 'NONE',  ( 5.331013795412237855, 0.1550192300789655642, 2.156197635354038411 ) ) ;
#148886 = CARTESIAN_POINT ( 'NONE',  ( 1.836970198721030181E-16, 13.49999999999999822, 1.500000000000000222 ) ) ;
#148887 = CARTESIAN_POINT ( 'NONE',  ( -11.99137977967679092, 8.009002857758401817, -0.5240188267039559422 ) ) ;
#148889 = CARTESIAN_POINT ( 'NONE',  ( 5.765249964824501028, 1.862012222821707308, -0.7743297468396084238 ) ) ;
#148888 = CARTESIAN_POINT ( 'NONE',  ( -7.687109908824056426, 8.070642436490613747, 0.7216878364870438212 ) ) ;
#148890 = CARTESIAN_POINT ( 'NONE',  ( 0.6823417656249882723, -0.5947916663252492686, 1.181850606188755259 ) ) ;
#148891 = CARTESIAN_POINT ( 'NONE',  ( 0.2578720826223569462, 0.6548769427211723615, 1.595941719785697988 ) ) ;
#148892 = CARTESIAN_POINT ( 'NONE',  ( 3.790386463472274148, 6.579812086429759788, 1.199719254218452047 ) ) ;
#148894 = CARTESIAN_POINT ( 'NONE',  ( 5.481239241674765950, 9.616805891921051952, -0.7998128361456481317 ) ) ;
#148893 = CARTESIAN_POINT ( 'NONE',  ( 7.944714827928050838, 9.331550723079971021, 1.082531754730558626 ) ) ;
#148895 = VECTOR ( 'NONE', #147901, 1000.000000000000000 ) ;
#148896 = CARTESIAN_POINT ( 'NONE',  ( -11.78331023100045627, 13.87999999999998302, 1.799999999999999600 ) ) ;
#148897 = CARTESIAN_POINT ( 'NONE',  ( 6.362560269511371658, -1.322780316340057549, 1.322825847358683138 ) ) ;
#148898 = CARTESIAN_POINT ( 'NONE',  ( 0.9967404297962767501, -1.964529542677856622, -0.4388597091333420463 ) ) ;
#148899 = CARTESIAN_POINT ( 'NONE',  ( -4.257741265285667431, 3.982435197156672491, 0.4597581080974452727 ) ) ;
#148900 = CARTESIAN_POINT ( 'NONE',  ( -6.251718229232846369, 9.347402796530044355, -1.082531754730549967 ) ) ;
#148901 = VERTEX_POINT ( 'NONE', #91864 ) ;
#148902 = CARTESIAN_POINT ( 'NONE',  ( 9.042925270190625753, 11.57316545335434199, 1.443375672974076540 ) ) ;
#148904 = CARTESIAN_POINT ( 'NONE',  ( 2.161732667986946410, 1.242745142284812365, 1.587824664567152766 ) ) ;
#148903 = CARTESIAN_POINT ( 'NONE',  ( 2.385534290476189145, 0.1013982516714604792, -2.118174289320504666 ) ) ;
#148905 = CARTESIAN_POINT ( 'NONE',  ( 2.039049738775432719, 0.002999869061550211602, 1.811767226593180569 ) ) ;
#148906 = CARTESIAN_POINT ( 'NONE',  ( 7.700104897918568447, 7.948153567185284096, 0.000000000000000000 ) ) ;
#148907 = CARTESIAN_POINT ( 'NONE',  ( -2.680963302752293664, 0.4788041664877169534, -0.1016165050528608921 ) ) ;
#148908 = VECTOR ( 'NONE', #105881, 1000.000000000000000 ) ;
#148909 = CARTESIAN_POINT ( 'NONE',  ( 7.461064606222022277, 7.598996883547496139, 1.040834085586084257E-14 ) ) ;
#148911 = CARTESIAN_POINT ( 'NONE',  ( 0.6728745832610707467, 1.688094080341449033, -0.9057684134900626516 ) ) ;
#148910 = CARTESIAN_POINT ( 'NONE',  ( -3.906720819032141190, 7.709591388846142479, -0.7998128361456281477 ) ) ;
#148912 = FILL_AREA_STYLE ('',( #200825 ) ) ;
#148913 = CARTESIAN_POINT ( 'NONE',  ( 6.453317929980448397, 6.631218461173066459, 1.040834085586084257E-14 ) ) ;
#148914 = EDGE_CURVE ( 'NONE', #118348, #7674, #9514, .T. ) ;
#148915 = CARTESIAN_POINT ( 'NONE',  ( -1.402160292154681736E-14, 0.6343750003414162508, 1.575800808251672791 ) ) ;
#148916 = CARTESIAN_POINT ( 'NONE',  ( 3.063779527008311021, 5.557864633942907417, 1.082531754730546636 ) ) ;
#148917 = CARTESIAN_POINT ( 'NONE',  ( -10.32183501870554387, 10.93656236477829502, 0.7998128361456462443 ) ) ;
#148918 = CARTESIAN_POINT ( 'NONE',  ( 4.592742373648754040, -0.4705147408641910944, -2.109722102427157964 ) ) ;
#148919 = ADVANCED_FACE ( 'NONE', ( #59330 ), #199417, .F. ) ;
#148920 = CARTESIAN_POINT ( 'NONE',  ( -4.990809943606269172, 8.836712344267034780, -0.7216878364870338292 ) ) ;
#148921 = CARTESIAN_POINT ( 'NONE',  ( 5.153507786970260796, 7.105788066255672497, -1.443375672974078761 ) ) ;
#148922 = CARTESIAN_POINT ( 'NONE',  ( 1.986737319265439394, -1.300789755646198476, 1.674730562594067829 ) ) ;
#148923 = CARTESIAN_POINT ( 'NONE',  ( 6.493173258741942178, 1.586635928914212013, -0.9027890188317911901 ) ) ;
#148924 = CARTESIAN_POINT ( 'NONE',  ( 3.374254075663080332, -1.176934739253515438, 1.581319453489488325 ) ) ;
#148925 = CARTESIAN_POINT ( 'NONE',  ( 5.660397963661894849, 1.910509065610028090, 0.08734628876111423523 ) ) ;
#148926 = ORIENTED_EDGE ( 'NONE', *, *, #161121, .T. ) ;
#148927 = LINE ( 'NONE', #153190, #66535 ) ;
#148928 = CARTESIAN_POINT ( 'NONE',  ( 5.582459562482231519, 1.174703874196600495, -1.580708309230594688 ) ) ;
#148929 = CARTESIAN_POINT ( 'NONE',  ( 1.113109651085980811, -1.894741734565345004, 0.4249041608528710823 ) ) ;
#148930 = VERTEX_POINT ( 'NONE', #61463 ) ;
#148931 = CARTESIAN_POINT ( 'NONE',  ( -5.144392941742557568, 4.966489618313220333, -0.7998128361456362523 ) ) ;
#148933 = CARTESIAN_POINT ( 'NONE',  ( -2.331034670843834533E-15, -7.287292266289724374, 9.765991025965632844 ) ) ;
#148932 = CARTESIAN_POINT ( 'NONE',  ( -6.292392690518202159, 9.394856334696294553, -1.082531754730549967 ) ) ;
#148935 = CARTESIAN_POINT ( 'NONE',  ( 6.012151052656117933, 9.101594430485762999, 1.199719254218460707 ) ) ;
#148934 = CARTESIAN_POINT ( 'NONE',  ( 1.974669457019386787, -0.1036536715517746843, -2.088194013563466012 ) ) ;
#148937 = CARTESIAN_POINT ( 'NONE',  ( 5.356880090730872013, 6.382686539675070492, 1.082531754730549078 ) ) ;
#148936 = CARTESIAN_POINT ( 'NONE',  ( 5.770966940911189447, 9.884545197705074671, -0.7998128361456291469 ) ) ;
#148939 = ORIENTED_EDGE ( 'NONE', *, *, #63399, .T. ) ;
#148938 = CARTESIAN_POINT ( 'NONE',  ( 6.358066468859800757, 0.7272683628555456359, -1.768788954293845528 ) ) ;
#148940 = CARTESIAN_POINT ( 'NONE',  ( 4.723365791888975096, -0.1103408873950258995, 2.204240794804641190 ) ) ;
#148941 = CARTESIAN_POINT ( 'NONE',  ( 1.448561363430532989, 2.204290700723564811, 0.1073905156721635390 ) ) ;
#148942 = CARTESIAN_POINT ( 'NONE',  ( -11.92619526248521034, 12.57255386085832605, 1.328859120100916558 ) ) ;
#148943 = CARTESIAN_POINT ( 'NONE',  ( 0.6801455168885979230, 0.9429141125626202546, 1.663586755705208420 ) ) ;
#148945 = DIRECTION ( 'NONE',  ( 1.000000000000000000, 0.000000000000000000, 0.000000000000000000 ) ) ;
#148944 =( GEOMETRIC_REPRESENTATION_CONTEXT ( 3 ) GLOBAL_UNCERTAINTY_ASSIGNED_CONTEXT ( ( #85015 ) ) GLOBAL_UNIT_ASSIGNED_CONTEXT ( ( #24089, #7837, #119537 ) ) REPRESENTATION_CONTEXT ( 'NONE', 'WORKASPACE' ) );
#148946 = CARTESIAN_POINT ( 'NONE',  ( 11.41381675112459959, 13.40000000000001101, -3.704697986577260682 ) ) ;
#148947 = CARTESIAN_POINT ( 'NONE',  ( 3.701679681979888503, -1.565833156357125278, -1.354537944502069102 ) ) ;
#148948 = CARTESIAN_POINT ( 'NONE',  ( -6.600121851754250812, 6.594563670001734046, 0.7998128361456341429 ) ) ;
#148950 = CARTESIAN_POINT ( 'NONE',  ( 1.604591590977550108, -0.7782141685120853580, -2.016947388195994062 ) ) ;
#148949 = CARTESIAN_POINT ( 'NONE',  ( 0.3852658704378412735, -6.836271227032193032, 10.85717823004580751 ) ) ;
#148951 = CARTESIAN_POINT ( 'NONE',  ( 4.159861740090546434, 1.033864333764370702, 1.932389678422803181 ) ) ;
#148952 = CARTESIAN_POINT ( 'NONE',  ( -1.127943160727153060, 3.300000000000025135, -0.7749999999999935829 ) ) ;
#148953 = DIRECTION ( 'NONE',  ( 0.000000000000000000, 0.000000000000000000, 1.000000000000000000 ) ) ;
#148954 = CARTESIAN_POINT ( 'NONE',  ( 7.777967379493318845, -6.134628647623484810, 7.744830294503448620 ) ) ;
#148955 = CARTESIAN_POINT ( 'NONE',  ( 1.364683531249997417, 14.04687500034140157, 2.602085213965210642E-15 ) ) ;
#148956 = CARTESIAN_POINT ( 'NONE',  ( -5.330290668828105538, 6.247702530834755130, 1.199719254218452935 ) ) ;
#148957 = CARTESIAN_POINT ( 'NONE',  ( 6.188101721744481587, 1.447254432076927166, 0.9550205611794166938 ) ) ;
#148958 = CARTESIAN_POINT ( 'NONE',  ( -9.490344339885977476, 11.13478515369756217, -1.082531754730539753 ) ) ;
#148959 = CARTESIAN_POINT ( 'NONE',  ( 3.520434184366732389, 0.9265386974339048232, 1.851387837889128640 ) ) ;
#148960 = CARTESIAN_POINT ( 'NONE',  ( 5.378551862015316765, -0.5151900214499178787, -2.053461258077380336 ) ) ;
#148961 = CARTESIAN_POINT ( 'NONE',  ( 7.284808609244363353, 7.393364887073558656, 0.7998128361456341429 ) ) ;
#148962 = CARTESIAN_POINT ( 'NONE',  ( 0.6823417656249899377, 5.426041667008087543, -1.181850606188754593 ) ) ;
#148963 = CARTESIAN_POINT ( 'NONE',  ( 2.887507918447276722, -1.839357967585793840, 0.7044240162308276210 ) ) ;
#148964 = CARTESIAN_POINT ( 'NONE',  ( 5.683585447934278001, -1.035311694948486183, 2.045203486727443121 ) ) ;
#148965 = CARTESIAN_POINT ( 'NONE',  ( 2.982817717652554101, -0.1347461720548545627, -1.820777111243766733 ) ) ;
#148966 = CARTESIAN_POINT ( 'NONE',  ( 2.891631901464575272, 6.595597328342462262, 0.000000000000000000 ) ) ;
#148967 = CARTESIAN_POINT ( 'NONE',  ( 4.107757354816228279, 6.775838766385488654, -1.082531754730548412 ) ) ;
#148968 = CARTESIAN_POINT ( 'NONE',  ( -6.449928391799210736, 8.548002428564306143, -1.599625672291263179 ) ) ;
#148969 = ORIENTED_EDGE ( 'NONE', *, *, #5255, .T. ) ;
#148970 = CARTESIAN_POINT ( 'NONE',  ( 3.638934968716364793, 1.913053428401530809, 0.6273635501436899409 ) ) ;
#148971 = CARTESIAN_POINT ( 'NONE',  ( 4.153139481255548660, 1.659551801668930793, -1.045809187271130591 ) ) ;
#148972 = CARTESIAN_POINT ( 'NONE',  ( -5.181187258716735577, 9.196468901811520880, 0.7998128361456481317 ) ) ;
#148973 = CARTESIAN_POINT ( 'NONE',  ( -5.108724954250998707, 4.854600622914589714, -0.7998128361456221525 ) ) ;
#148974 = DIRECTION ( 'NONE',  ( 0.000000000000000000, 8.546850786086437571E-32, 1.000000000000000000 ) ) ;
#148976 = CARTESIAN_POINT ( 'NONE',  ( 5.963686863811354932, 1.742942877579903405, -0.3063674984340163387 ) ) ;
#148975 = CARTESIAN_POINT ( 'NONE',  ( -0.02372336622697389028, -2.029015295047017720, -0.5039539365503820090 ) ) ;
#148977 = DIRECTION ( 'NONE',  ( 0.6507913734559640506, -0.7592566023653004592, 0.000000000000000000 ) ) ;
#148978 = CARTESIAN_POINT ( 'NONE',  ( 2.080269975650438585, -2.149535124392497831, -0.4257020960420563882 ) ) ;
#148979 = CARTESIAN_POINT ( 'NONE',  ( 0.6436349260668382533, 0.5032331446216579129, 1.666064694988089512 ) ) ;
#148980 = CARTESIAN_POINT ( 'NONE',  ( 4.788000803920411386, 8.737751371215816576, 1.040834085586084257E-14 ) ) ;
#148981 = CARTESIAN_POINT ( 'NONE',  ( 0.2335667940003048615, 5.721530573166598188, -2.747389403444942868 ) ) ;
#148982 = CARTESIAN_POINT ( 'NONE',  ( 0.3633288501447570207, 1.706897997983588322, -0.2475752363529682698 ) ) ;
#148983 = CARTESIAN_POINT ( 'NONE',  ( 1.001802975355575054, 2.264736134964080438, 0.3911735967057332064 ) ) ;
#148984 = CARTESIAN_POINT ( 'NONE',  ( 0.1522426329377546128, 0.8445714516599597266, 2.022489037641273857 ) ) ;
#148985 = CARTESIAN_POINT ( 'NONE',  ( 2.578998426009218470, -2.112161100990978202, -0.6396139477699357423 ) ) ;
#148986 = CARTESIAN_POINT ( 'NONE',  ( 0.9542540200799983774, -0.7831509020928304476, 2.025049046554725063 ) ) ;
#148987 = CARTESIAN_POINT ( 'NONE',  ( 0.2053145577999641036, -0.4904175937916722128, 1.758528939493007481 ) ) ;
#148988 = CARTESIAN_POINT ( 'NONE',  ( 2.782529222840863348, -0.6191273052778034636, -2.024769726974411377 ) ) ;
#148989 = CARTESIAN_POINT ( 'NONE',  ( 6.827182134110219458, 3.682144966263278363, 2.702925436647874324 ) ) ;
#148990 = CARTESIAN_POINT ( 'NONE',  ( 5.983413252614310451, 1.779745538724048171, -0.7376744472527080321 ) ) ;
#148991 = ORIENTED_EDGE ( 'NONE', *, *, #19510, .F. ) ;
#148993 = CARTESIAN_POINT ( 'NONE',  ( -1.364683531250000748, 0.5718750003414208027, 0.000000000000000000 ) ) ;
#148992 = CARTESIAN_POINT ( 'NONE',  ( 2.173718093399327422, 1.413494431062709333, 1.804626757829434380 ) ) ;
#148994 = CARTESIAN_POINT ( 'NONE',  ( 2.835626683552519012, 6.459981564119914310, 0.000000000000000000 ) ) ;
#148995 = CARTESIAN_POINT ( 'NONE',  ( 6.193377243344257543, 6.120028293523423812, -0.7998128361456281477 ) ) ;
#148996 = CARTESIAN_POINT ( 'NONE',  ( 4.741020875331694029, 2.125508857184394973, 0.6453399526389347329 ) ) ;
#148997 = CARTESIAN_POINT ( 'NONE',  ( -6.670248388243482651, 9.765411638717282017, 1.082531754730548412 ) ) ;
#148998 = CARTESIAN_POINT ( 'NONE',  ( -4.900932632813380184E-15, -5.758458176070767820, -10.93186801223269811 ) ) ;
#148999 = CARTESIAN_POINT ( 'NONE',  ( 4.514501963670558560, 8.210743357683563559, 1.040834085586084257E-14 ) ) ;
#149000 = CARTESIAN_POINT ( 'NONE',  ( -6.168596704093453731, 10.14052055484361325, 0.7216878364870458196 ) ) ;
#149001 = CIRCLE ( 'NONE', #173304, 0.08000000000000040412 ) ;
#149002 = CARTESIAN_POINT ( 'NONE',  ( 4.963693636378940788, 5.923969009597785274, -1.082531754730548412 ) ) ;
#149003 = ORIENTED_EDGE ( 'NONE', *, *, #88556, .F. ) ;
#149004 = CARTESIAN_POINT ( 'NONE',  ( 2.725232599228684993, 2.001511357256777313, 0.2440295182731533341 ) ) ;
#149006 = CARTESIAN_POINT ( 'NONE',  ( 1.463816541924748638, -0.5049463793320208005, 1.999668334691290683 ) ) ;
#149005 = CARTESIAN_POINT ( 'NONE',  ( 7.623762449586013901, 7.788811034138823253, 1.040834085586084257E-14 ) ) ;
#149007 = CARTESIAN_POINT ( 'NONE',  ( 4.657519343637313902, 4.904169560260807970, 0.6806404322877991353 ) ) ;
#149008 = CARTESIAN_POINT ( 'NONE',  ( 5.844973620822844218, 5.991759777147701804, 0.7216878364870328300 ) ) ;
#149009 = CYLINDRICAL_SURFACE ( 'NONE', #112881, 10.99999999999999112 ) ;
#149010 = CARTESIAN_POINT ( 'NONE',  ( 1.364683531249988535, 3.113541667008083991, 0.7879004041258500513 ) ) ;
#149011 = CARTESIAN_POINT ( 'NONE',  ( 4.066501749483540706, -2.044453849244652233, -0.7895499924894524568 ) ) ;
#149012 = CARTESIAN_POINT ( 'NONE',  ( 1.072888940501380839, -0.9041080511620370741, 1.802418165037560138 ) ) ;
#149013 = CARTESIAN_POINT ( 'NONE',  ( 0.8195642880178370948, 1.096917009463085790, -1.478703137254427924 ) ) ;
#149014 = CARTESIAN_POINT ( 'NONE',  ( 4.505690185649424251, -0.7896136771840707169, -1.663358820747300237 ) ) ;
#149015 = EDGE_CURVE ( 'NONE', #123589, #138847, #27899, .T. ) ;
#149016 = CARTESIAN_POINT ( 'NONE',  ( 6.611572464958476836, 10.86525164242692298, 0.7998128361456462443 ) ) ;
#149017 = SURFACE_STYLE_FILL_AREA ( #16863 ) ;
#149018 = CARTESIAN_POINT ( 'NONE',  ( 5.684540951402929920, -1.781552174421060064, -0.3977488440568625605 ) ) ;
#149019 = CARTESIAN_POINT ( 'NONE',  ( 6.504528880466823537, -1.955196382115764964, 0.4926337920100053447 ) ) ;
#149020 = CARTESIAN_POINT ( 'NONE',  ( -9.013473194986783454, 9.410140237106395134, -0.7998128361456291469 ) ) ;
#149022 = CARTESIAN_POINT ( 'NONE',  ( -7.144220599758281054, 7.299621885998258897, 0.7998128361456341429 ) ) ;
#149021 = CARTESIAN_POINT ( 'NONE',  ( 4.645576076348203465, -1.746196445045271606, -1.438666788099978389 ) ) ;
#149023 = CARTESIAN_POINT ( 'NONE',  ( 0.3113324583694621617, 1.833617258854224552, 1.035894449818143270 ) ) ;
#149024 = CARTESIAN_POINT ( 'NONE',  ( -0.4000000000000348277, 3.251480759208456917, 0.4649507210924809786 ) ) ;
#149025 = CARTESIAN_POINT ( 'NONE',  ( 4.686024408448190570, -1.271122505372159539, -1.634150330299996012 ) ) ;
#149026 = CARTESIAN_POINT ( 'NONE',  ( 9.348510611822643313, 10.86534945433664134, 1.199719254218453823 ) ) ;
#149027 = APPLICATION_PROTOCOL_DEFINITION ( 'draft international standard', 'automotive_design', 1998, #49107 ) ;
#149028 = CARTESIAN_POINT ( 'NONE',  ( -9.013473194986783454, 9.410140237106395134, -0.7998128361456291469 ) ) ;
#149029 = UNCERTAINTY_MEASURE_WITH_UNIT (LENGTH_MEASURE( 1.000000000000000082E-05 ), #134807, 'distance_accuracy_value', 'NONE');
#149030 = CARTESIAN_POINT ( 'NONE',  ( 6.016786309414542622, 10.24161080428416426, 0.7998128361456341429 ) ) ;
#149031 = CARTESIAN_POINT ( 'NONE',  ( 4.597200498174307981, 6.922409349013787683, -1.201048452015600843 ) ) ;
#149032 = CARTESIAN_POINT ( 'NONE',  ( -4.464712657601869417, 4.103252943490596216, 0.7998128361456341429 ) ) ;
#149034 = CARTESIAN_POINT ( 'NONE',  ( 1.424421946217780732, -2.203867130488819548, 0.2783968414596868501 ) ) ;
#149033 = CARTESIAN_POINT ( 'NONE',  ( 1.107859837811319581, 1.609452232531217275, 1.380942675281403353 ) ) ;
#149035 = CARTESIAN_POINT ( 'NONE',  ( 3.856552995061765632, 0.7561154531541111057, 1.965730562608114740 ) ) ;
#149037 = CARTESIAN_POINT ( 'NONE',  ( -6.774234028683526532, 7.932303117332766718, 1.199719254218452047 ) ) ;
#149036 =( GEOMETRIC_REPRESENTATION_CONTEXT ( 3 ) GLOBAL_UNCERTAINTY_ASSIGNED_CONTEXT ( ( #85149 ) ) GLOBAL_UNIT_ASSIGNED_CONTEXT ( ( #23410, #89521, #155574 ) ) REPRESENTATION_CONTEXT ( 'NONE', 'WORKASPACE' ) );
#149038 = CARTESIAN_POINT ( 'NONE',  ( 4.964256800898067645, 8.943383367689749619, 0.7998128361456462443 ) ) ;
#149039 = CARTESIAN_POINT ( 'NONE',  ( 3.350005920730843911, -0.7974703105717847462, 1.792663495558038056 ) ) ;
#149040 = CARTESIAN_POINT ( 'NONE',  ( 5.823390672269506574, 6.752709524857930745, -1.199719254218446718 ) ) ;
#149041 = CARTESIAN_POINT ( 'NONE',  ( -4.029167574269930441, 7.605081013511371779, 0.2528308249854539502 ) ) ;
#149042 = CARTESIAN_POINT ( 'NONE',  ( 3.822509244049070887, 6.547012320444182798, -1.199719254218452047 ) ) ;
#149043 = CARTESIAN_POINT ( 'NONE',  ( -4.665414256878287702, 8.457084043084382330, -0.7216878364870338292 ) ) ;
#149044 = CARTESIAN_POINT ( 'NONE',  ( -6.371969008742801144, 10.37778824360119145, 0.7216878364870458196 ) ) ;
#149045 = CARTESIAN_POINT ( 'NONE',  ( 2.443736651115399283, -1.977012053918187906, 0.7674769708189137507 ) ) ;
#149046 = CARTESIAN_POINT ( 'NONE',  ( -6.180537922983287302, 8.303989891604203422, -1.599625672291271394 ) ) ;
#149047 = CARTESIAN_POINT ( 'NONE',  ( 3.912515228517557286, 0.7039278570535618673, 1.831416474553926310 ) ) ;
#149048 = CARTESIAN_POINT ( 'NONE',  ( 2.747127081003514881, -1.797865629537301668, 1.199965651887124896 ) ) ;
#149049 = CARTESIAN_POINT ( 'NONE',  ( 2.964219115174483665, -1.702287218311925532, -0.7022057971969236645 ) ) ;
#149050 = CARTESIAN_POINT ( 'NONE',  ( -4.373759202716216876, 7.180157790548314267, -1.044885312346154782 ) ) ;
#149051 = CARTESIAN_POINT ( 'NONE',  ( -0.6823417656250003738, -0.7197916663252492686, -1.181850606188749264 ) ) ;
#149052 = CARTESIAN_POINT ( 'NONE',  ( 4.382551862494687533, 1.553031517084975555, -0.7855321229453329224 ) ) ;
#149053 = CARTESIAN_POINT ( 'NONE',  ( -6.671583288097857611, 16.00000000000178701, -9.747470831326625174 ) ) ;
#149054 = CARTESIAN_POINT ( 'NONE',  ( 4.365362273920244007, 6.116008624372160973, 1.443375672974062551 ) ) ;
#149055 = CARTESIAN_POINT ( 'NONE',  ( -1.138412281109779656E-15, -9.181223591647238891, 10.14523337821910864 ) ) ;
#149056 = CIRCLE ( 'NONE', #17463, 12.00000000000000178 ) ;
#149057 = CARTESIAN_POINT ( 'NONE',  ( 2.254944280175336324, -1.671361177491991201, 1.370965666894090385 ) ) ;
#149058 = EDGE_CURVE ( 'NONE', #171990, #57016, #72493, .T. ) ;
#149059 = CARTESIAN_POINT ( 'NONE',  ( 4.130232389481975908, 0.2495678132241747338, -2.000550906993769473 ) ) ;
#149060 = CARTESIAN_POINT ( 'NONE',  ( -9.070041577417988776, 12.56517035942090388, 1.082531754730558626 ) ) ;
#149061 = CARTESIAN_POINT ( 'NONE',  ( 1.147603855448702248, -1.704515299458901012, -1.329379018566230641 ) ) ;
#149062 = CARTESIAN_POINT ( 'NONE',  ( 3.502765367584356859, 1.555092314170872347, -1.211676150289840992 ) ) ;
#149063 = CARTESIAN_POINT ( 'NONE',  ( 2.460178626894731213, 0.8396039701564265156, 1.783738064433965986 ) ) ;
#149064 = CARTESIAN_POINT ( 'NONE',  ( 6.508999999999979025, 4.693190036150777011, 2.662629399390674667 ) ) ;
#149065 = CARTESIAN_POINT ( 'NONE',  ( 2.858853853349733409, 0.2825237051190258031, -1.921275437378862305 ) ) ;
#149068 = EDGE_LOOP ( 'NONE', ( #82755, #53168, #130093, #152991 ) ) ;
#149067 = CARTESIAN_POINT ( 'NONE',  ( -4.990809943606294929, 4.995235487061662205, -0.7216878364870338292 ) ) ;
#149066 = CARTESIAN_POINT ( 'NONE',  ( -10.11401940567025548, 10.90203684947788076, 1.040834085586084257E-14 ) ) ;
#149069 = CARTESIAN_POINT ( 'NONE',  ( -4.217995187182965289, 6.014356699837137832, 1.443375672974065660 ) ) ;
#149070 = CARTESIAN_POINT ( 'NONE',  ( 4.061549535745618833, 6.896169004081968090, -1.199719254218452047 ) ) ;
#149072 = EDGE_LOOP ( 'NONE', ( #170566, #177858, #204102, #133754 ) ) ;
#149071 = CARTESIAN_POINT ( 'NONE',  ( -5.119085517611572378, 8.129960982925583224, 1.199719254218452935 ) ) ;
#149073 = CARTESIAN_POINT ( 'NONE',  ( -9.964879715919934711, 10.72804054476916313, 0.7216878364870438212 ) ) ;
#149074 = CARTESIAN_POINT ( 'NONE',  ( 1.009129827085092135, 1.670030910484705755, -1.442630471070925458 ) ) ;
#149075 = CARTESIAN_POINT ( 'NONE',  ( -3.285556943750000514, -3.288541666188709023, -1.896917185911906500 ) ) ;
#149076 = CARTESIAN_POINT ( 'NONE',  ( 5.032062496497622384, 1.126290172248314292, 1.606047186625796819 ) ) ;
#149077 = VERTEX_POINT ( 'NONE', #191448 ) ;
#149078 = CARTESIAN_POINT ( 'NONE',  ( 3.608711286396129481, 2.011918449240827744, 0.6600949426460513969 ) ) ;
#149079 = CARTESIAN_POINT ( 'NONE',  ( 1.499999999999987121, 3.077083334016149863, -0.8660254037844262731 ) ) ;
#149081 = CARTESIAN_POINT ( 'NONE',  ( -5.018489415352746619, 9.006654751220198207, 0.7998128361456481317 ) ) ;
#149080 = CARTESIAN_POINT ( 'NONE',  ( 0.07479286986305369589, 0.004866263145587855152, -1.855573292446037970 ) ) ;
#149082 = CARTESIAN_POINT ( 'NONE',  ( 3.767381502543519112, 1.024135474229198151, 1.529801857347697025 ) ) ;
#149083 = ORIENTED_EDGE ( 'NONE', *, *, #181903, .F. ) ;
#149084 = CARTESIAN_POINT ( 'NONE',  ( -9.182950115157607840, 9.607863310639020327, 0.7998128361456462443 ) ) ;
#149085 = CARTESIAN_POINT ( 'NONE',  ( 5.660427296577901224, 2.118236611397010805, 0.1021076702828054988 ) ) ;
#149086 = DIRECTION ( 'NONE',  ( -0.000000000000000000, 1.000000000000000000, -0.000000000000000000 ) ) ;
#149087 = CARTESIAN_POINT ( 'NONE',  ( 6.796715079152391148, 6.823922435299587974, 0.7998128361456341429 ) ) ;
#149088 = EDGE_CURVE ( 'NONE', #25476, #63977, #181614, .T. ) ;
#149089 = CARTESIAN_POINT ( 'NONE',  ( 5.729779026133646092, -1.304086877343976880, -1.595700086769378023 ) ) ;
#149091 = CARTESIAN_POINT ( 'NONE',  ( 3.034521004542716227, -1.622529355458858236, 0.8704296449140033198 ) ) ;
#149090 = CARTESIAN_POINT ( 'NONE',  ( 0.5548465212725885998, 1.550470960922016861, -1.029025501433494583 ) ) ;
#149092 = CARTESIAN_POINT ( 'NONE',  ( 9.121938423896107651, 9.536683004167278099, -0.7998128361456221525 ) ) ;
#149093 = CARTESIAN_POINT ( 'NONE',  ( 0.4000000000000045186, 3.950000000000022826, -1.561251128379126385E-14 ) ) ;
#149094 = CARTESIAN_POINT ( 'NONE',  ( -5.908321080505254841, 10.11506803722328129, 0.7998128361456291469 ) ) ;
#149095 = DIRECTION ( 'NONE',  ( 0.000000000000000000, 0.000000000000000000, -1.000000000000000000 ) ) ;
#149096 = CIRCLE ( 'NONE', #45366, 0.7499999999999997780 ) ;
#149097 = CARTESIAN_POINT ( 'NONE',  ( 2.332911791115964473, 2.140974936812658935, 0.5348262304398290201 ) ) ;
#149098 = CARTESIAN_POINT ( 'NONE',  ( 4.675235532476687439, 0.006304645973906687281, -2.262578822721802219 ) ) ;
#149099 = CARTESIAN_POINT ( 'NONE',  ( 3.626185617424378282, 2.007256095728218614, 0.1928357053486499662 ) ) ;
#149100 = STYLED_ITEM ( 'NONE', ( #61449 ), #72370 ) ;
#149101 = CARTESIAN_POINT ( 'NONE',  ( -7.266807147244793263, 8.540658428949452485, 1.082531754730549967 ) ) ;
#149102 = CARTESIAN_POINT ( 'NONE',  ( 4.429823666617582312, -1.775263289385048848, 0.3600210208860327721 ) ) ;
#149103 = CARTESIAN_POINT ( 'NONE',  ( 5.823430154129352054, -1.392497453891910375, -1.315930268783272794 ) ) ;
#149104 = CARTESIAN_POINT ( 'NONE',  ( 6.827182134110172385, 0.001020705822878450282, 1.910856149448317165 ) ) ;
#149105 = CARTESIAN_POINT ( 'NONE',  ( 5.383624799460786647, 1.257121276536907750, 1.385457850027263182 ) ) ;
#149106 = CARTESIAN_POINT ( 'NONE',  ( 5.002340964340571183, 1.856068601349126324, 0.1372510170762584192 ) ) ;
#149107 = CARTESIAN_POINT ( 'NONE',  ( -1.364683531250012516, 4.988541667008084879, -0.7879004041258300672 ) ) ;
#149108 = CARTESIAN_POINT ( 'NONE',  ( 5.946140033727446372, 1.768047588762114986, 0.08285011829376774661 ) ) ;
#149109 = CARTESIAN_POINT ( 'NONE',  ( 0.4269707148552639997, -1.727061408318403712, 1.040797348915108111 ) ) ;
#149110 =( BOUNDED_CURVE ( )  B_SPLINE_CURVE ( 3, ( #44790, #75135, #7977, #27439 ),
 .UNSPECIFIED., .F., .T. ) 
 B_SPLINE_CURVE_WITH_KNOTS ( ( 4, 4 ),
 ( 0.000000000000000000, 0.5000000000000003331 ),
 .UNSPECIFIED. ) 
 CURVE ( )  GEOMETRIC_REPRESENTATION_ITEM ( )  RATIONAL_B_SPLINE_CURVE ( ( 1.000000000000000222, 0.3333333333333329818, 0.3333333333333334259, 1.000000000000000666 ) ) 
 REPRESENTATION_ITEM ( '' )  );
#149112 = CARTESIAN_POINT ( 'NONE',  ( 2.631583836753316863, -1.964825297316885155, 0.7587525405363388931 ) ) ;
#149111 = CARTESIAN_POINT ( 'NONE',  ( -4.433153041544240835, 4.274359424664112339, 0.7216878364870317197 ) ) ;
#149113 = CARTESIAN_POINT ( 'NONE',  ( 8.992082194361556091, 11.51384853155376220, 1.599625672291279388 ) ) ;
#149114 = CARTESIAN_POINT ( 'NONE',  ( -9.317477881089553549, 11.89347683273641820, 1.599625672291281386 ) ) ;
#149115 = DIRECTION ( 'NONE',  ( 0.000000000000000000, 1.000000000000000000, 0.000000000000000000 ) ) ;
#149116 = CARTESIAN_POINT ( 'NONE',  ( 2.408468576312505771, -2.014670991514801113, -0.1442217307643048063 ) ) ;
#149117 = CARTESIAN_POINT ( 'NONE',  ( 0.6823417656249899377, 2.342708333674753618, 1.181850606188767472 ) ) ;
#149118 = CARTESIAN_POINT ( 'NONE',  ( 3.497113557321089861, 6.167384019261527683, -1.199719254218446718 ) ) ;
#149119 = VERTEX_POINT ( 'NONE', #28971 ) ;
#149120 = EDGE_CURVE ( 'NONE', #26075, #41882, #95551, .T. ) ;
#149121 = CARTESIAN_POINT ( 'NONE',  ( 1.897963814661303150, -0.7301937759345776824, 2.034636513274298064 ) ) ;
#149122 = CARTESIAN_POINT ( 'NONE',  ( 6.889999999999970370, 7.053389210336755255, 2.318152334880723142 ) ) ;
#149125 = DIRECTION ( 'NONE',  ( 0.000000000000000000, 0.000000000000000000, -1.000000000000000000 ) ) ;
#149124 = CARTESIAN_POINT ( 'NONE',  ( -4.183485216215313329, 3.563207579971348515, -2.499999999999995115 ) ) ;
#149123 = CARTESIAN_POINT ( 'NONE',  ( 3.790386463472274148, 6.579812086429759788, 1.199719254218452047 ) ) ;
#149126 = CARTESIAN_POINT ( 'NONE',  ( 9.042925270190622200, 12.53353466765568669, 1.082531754730546636 ) ) ;
#149127 = CARTESIAN_POINT ( 'NONE',  ( -7.721398836998370818, -6.134628647623487474, 7.721398836998398352 ) ) ;
#149128 =( BOUNDED_CURVE ( )  B_SPLINE_CURVE ( 2, ( #175884, #28552, #112009, #78358, #210485, #173760, #61048, #126131, #94641 ),
 .UNSPECIFIED., .F., .T. ) 
 B_SPLINE_CURVE_WITH_KNOTS ( ( 3, 2, 2, 2, 3 ),
 ( 0.1718749999999998335, 0.1770833333333333426, 0.1875000000000000000, 0.1979166666666666574, 0.2031250000000002220 ),
 .UNSPECIFIED. ) 
 CURVE ( )  GEOMETRIC_REPRESENTATION_ITEM ( )  RATIONAL_B_SPLINE_CURVE ( ( 0.9330127018922194093, 0.9330127018922171889, 1.000000000000000000, 0.8660254037844387076, 1.000000000000000000, 0.8660254037844387076, 1.000000000000000000, 0.9330127018922165227, 0.9330127018922194093 ) ) 
 REPRESENTATION_ITEM ( '' )  );
#149129 = CARTESIAN_POINT ( 'NONE',  ( -8.080296364064746939, 9.489729181906076505, 1.082531754730558626 ) ) ;
#149130 = CARTESIAN_POINT ( 'NONE',  ( 0.5916818631664167993, -0.7834642122952638621, 2.046923429677327100 ) ) ;
#149131 = CARTESIAN_POINT ( 'NONE',  ( -7.721398836998405457, -6.134628647623499909, -7.721398836998363713 ) ) ;
#149132 = CARTESIAN_POINT ( 'NONE',  ( 1.973834762636607509, 2.164947816325224039, -0.6572921511966890451 ) ) ;
#149133 = CARTESIAN_POINT ( 'NONE',  ( -9.169391961543940539, 9.592045464756413509, 1.040834085586084257E-14 ) ) ;
#149134 = CARTESIAN_POINT ( 'NONE',  ( -3.741687207247254676, 7.309126141856352454, 1.040834085586084257E-14 ) ) ;
#149135 = CARTESIAN_POINT ( 'NONE',  ( 0.6823417656249899377, 3.488541667008085323, -1.181850606188754593 ) ) ;
#149136 = CARTESIAN_POINT ( 'NONE',  ( 4.594924845400013780, 8.373833185659544043, 0.04553248676899754321 ) ) ;
#149137 = CARTESIAN_POINT ( 'NONE',  ( -6.009258394948636914E-15, 11.43749999999999822, -1.732050807568875195 ) ) ;
#149138 = CARTESIAN_POINT ( 'NONE',  ( 3.230585741806197841, 6.991043475407723307, 0.7998128361456271485 ) ) ;
#149139 =( BOUNDED_CURVE ( )  B_SPLINE_CURVE ( 2, ( #33293, #180612, #1839, #17026, #200052, #181666, #149183 ),
 .UNSPECIFIED., .F., .T. ) 
 B_SPLINE_CURVE_WITH_KNOTS ( ( 3, 2, 2, 3 ),
 ( 0.4316551096257628672, 0.4345238095238095344, 0.4404761904761904656, 0.4428956208513696868 ),
 .UNSPECIFIED. ) 
 CURVE ( )  GEOMETRIC_REPRESENTATION_ITEM ( )  RATIONAL_B_SPLINE_CURVE ( ( 0.9331000818465632340, 0.9354320710352570512, 1.000000000000000000, 0.8660254037844387076, 1.000000000000000000, 0.9455441091255019082, 0.9353569697113766068 ) ) 
 REPRESENTATION_ITEM ( '' )  );
#149140 = EDGE_CURVE ( 'NONE', #65271, #11614, #76641, .T. ) ;
#149141 = CARTESIAN_POINT ( 'NONE',  ( 2.829092851278795617, -1.652813950429321999, 0.6331040572071617856 ) ) ;
#149142 = CARTESIAN_POINT ( 'NONE',  ( 6.159228477734898455, -1.889628185881117695, -1.139594184263223120 ) ) ;
#149143 = CARTESIAN_POINT ( 'NONE',  ( 1.364683531250000303, 14.56770833367473372, -0.7879004041258355073 ) ) ;
#149144 = ORIENTED_EDGE ( 'NONE', *, *, #153343, .F. ) ;
#149145 = CARTESIAN_POINT ( 'NONE',  ( -6.099189001301292379, 8.209082816308541197, 1.599625672291263179 ) ) ;
#149146 = CARTESIAN_POINT ( 'NONE',  ( 5.255482535091188012, 1.942537579172060047, -0.5405093616211650298 ) ) ;
#149147 = VERTEX_POINT ( 'NONE', #13764 ) ;
#149148 = CARTESIAN_POINT ( 'NONE',  ( 2.465516990510143280, 1.834972510290140191, -0.3627323784974947340 ) ) ;
#149149 = CARTESIAN_POINT ( 'NONE',  ( 2.852461952307944415, -2.064405766265942521, -0.1567919417525542591 ) ) ;
#149150 = TOROIDAL_SURFACE ( 'NONE', #204486, 3.399419719642636561, 0.1000000000000000056 ) ;
#149151 = CARTESIAN_POINT ( 'NONE',  ( -2.277406616971334508, 5.600798786534425311, 1.040834085586084257E-14 ) ) ;
#149152 = CARTESIAN_POINT ( 'NONE',  ( 2.443496805918866865, -1.782974011999260977, 0.6919810379762069141 ) ) ;
#149153 = CARTESIAN_POINT ( 'NONE',  ( -5.518377602441839613, 7.280004618224392487, 1.249996204172974190 ) ) ;
#149154 = CARTESIAN_POINT ( 'NONE',  ( -10.77321989194975416, 5.423924896255240213, -6.620653902763565135 ) ) ;
#149155 = LINE ( 'NONE', #137199, #52257 ) ;
#149156 = ADVANCED_FACE ( 'NONE', ( #192514 ), #133918, .F. ) ;
#149157 = CARTESIAN_POINT ( 'NONE',  ( -1.201851678989727383E-14, 4.009375000341416140, -1.575800808251660134 ) ) ;
#149158 = CARTESIAN_POINT ( 'NONE',  ( 0.7735182334044669039, 0.3705173918269571431, -1.875978362188876813 ) ) ;
#149159 = CARTESIAN_POINT ( 'NONE',  ( 6.048345925472183637, 8.149765894507963182, 1.443375672974065660 ) ) ;
#149160 = CARTESIAN_POINT ( 'NONE',  ( 2.928120951529111338, 1.047165451586975049, 1.658829547137883775 ) ) ;
#149161 = EDGE_CURVE ( 'NONE', #63704, #49215, #3196, .T. ) ;
#149162 = CARTESIAN_POINT ( 'NONE',  ( -5.974410882859528371, 4.760127796209656204, -2.438793965253434060 ) ) ;
#149163 = CARTESIAN_POINT ( 'NONE',  ( -3.447516199624892419, 7.244129009529488350, 0.7998128361456352531 ) ) ;
#149164 = CARTESIAN_POINT ( 'NONE',  ( 5.115537534566191091, 1.735013203181461350, 1.219038288318145646 ) ) ;
#149166 = SURFACE_STYLE_FILL_AREA ( #64712 ) ;
#149165 = CARTESIAN_POINT ( 'NONE',  ( 9.921869487102386032, 10.46993591124128997, 0.000000000000000000 ) ) ;
#149167 = CARTESIAN_POINT ( 'NONE',  ( 6.151636724293027214, 0.5744773170833740172, -1.885769548957224817 ) ) ;
#149168 = CARTESIAN_POINT ( 'NONE',  ( 0.6823417656249882723, 2.676041667008084879, -1.181850606188749264 ) ) ;
#149169 = CARTESIAN_POINT ( 'NONE',  ( 2.461191956773252087, -1.671442449460639468, 1.121892926246186306 ) ) ;
#149171 = CARTESIAN_POINT ( 'NONE',  ( 0.6150561885070615631, 0.1604698007556179251, 2.111222410368835067 ) ) ;
#149170 = CARTESIAN_POINT ( 'NONE',  ( -7.537970219518091319, 7.896646132300314314, -0.7216878364870278340 ) ) ;
#149172 = CARTESIAN_POINT ( 'NONE',  ( 1.499999999999823475, 7.438721522839173872, 4.195160983902624707 ) ) ;
#149173 = CARTESIAN_POINT ( 'NONE',  ( 2.471216696211364638, 1.848302923701108158, 0.9330170062570308787 ) ) ;
#149174 = CARTESIAN_POINT ( 'NONE',  ( 5.239300017038202917, 5.077214539491492928, 0.000000000000000000 ) ) ;
#149175 = CARTESIAN_POINT ( 'NONE',  ( 3.790386463472274148, 6.579812086429759788, 1.199719254218452047 ) ) ;
#149177 = ORIENTED_EDGE ( 'NONE', *, *, #56964, .T. ) ;
#149176 = B_SPLINE_CURVE_WITH_KNOTS ( 'NONE', 3,
 ( #53064, #98635, #134360, #52013 ),
 .UNSPECIFIED., .F., .F.,
 ( 4, 4 ),
 ( 0.000000000000000000, 3.548791410035703395E-05 ),
 .UNSPECIFIED. ) ;
#149179 = CARTESIAN_POINT ( 'NONE',  ( 4.599240423533799138, 6.388866465587984322, 1.599625672291267398 ) ) ;
#149178 = CARTESIAN_POINT ( 'NONE',  ( 5.578101482107681974, -2.039469400243614672, -0.4589526871568836430 ) ) ;
#149181 = EDGE_LOOP ( 'NONE', ( #56484, #115939, #145396, #20038 ) ) ;
#149180 = CARTESIAN_POINT ( 'NONE',  ( 4.366094929315432083, 0.8608494910617261464, 1.609850404305966265 ) ) ;
#149182 = CARTESIAN_POINT ( 'NONE',  ( 8.757677159423465696, 12.30470822171437284, 1.199719254218450271 ) ) ;
#149183 = CARTESIAN_POINT ( 'NONE',  ( 1.217526595471194906, 2.800000000000017586, -0.8761443883974121549 ) ) ;
#149184 = CARTESIAN_POINT ( 'NONE',  ( 9.377738819465895048, 12.64169150452043766, -6.543016420796631039 ) ) ;
#149185 = AXIS2_PLACEMENT_3D ( 'NONE', #204023, #42656, #158519 ) ;
#149186 = CARTESIAN_POINT ( 'NONE',  ( 5.192482782645277517, -2.189556457885518892, -0.2746672974567528347 ) ) ;
#149187 = CARTESIAN_POINT ( 'NONE',  ( -0.6823417656250039265, 10.38020833367472839, -1.181850606188755259 ) ) ;
#149188 = ORIENTED_EDGE ( 'NONE', *, *, #76938, .T. ) ;
#149189 = CARTESIAN_POINT ( 'NONE',  ( 4.424404876070213710, -0.8207606565990737124, -1.727334472114170794 ) ) ;
#149190 = CARTESIAN_POINT ( 'NONE',  ( -4.295235737431041478, 3.905529869957963029, -0.7998128361456221525 ) ) ;
#149191 =( BOUNDED_CURVE ( )  B_SPLINE_CURVE ( 2, ( #113308, #179314, #81794, #80738, #212846, #196617, #48256 ),
 .UNSPECIFIED., .F., .T. ) 
 B_SPLINE_CURVE_WITH_KNOTS ( ( 3, 2, 2, 3 ),
 ( 0.1785714285714287142, 0.1845238095238095899, 0.1904761904761904656, 0.1964285714285713413 ),
 .UNSPECIFIED. ) 
 CURVE ( )  GEOMETRIC_REPRESENTATION_ITEM ( )  RATIONAL_B_SPLINE_CURVE ( ( 0.9999999999999968914, 0.8660254037844418162, 1.000000000000000000, 0.8660254037844387076, 1.000000000000000000, 0.8660254037844405950, 0.9999999999999981126 ) ) 
 REPRESENTATION_ITEM ( '' )  );
#149192 = CARTESIAN_POINT ( 'NONE',  ( 7.904567251967224095, 9.180748867838630645, 1.199719254218462483 ) ) ;
#149193 = CARTESIAN_POINT ( 'NONE',  ( -1.360316468750026653, 2.192708333674788346, 0.7853790794158680422 ) ) ;
#149194 = CARTESIAN_POINT ( 'NONE',  ( 4.704316113817540668, 5.551085556617666228, -1.082531754730548412 ) ) ;
#149195 = CARTESIAN_POINT ( 'NONE',  ( 7.015401035077362124, 6.062865449010541141, -2.437084766375293921 ) ) ;
#149196 = CARTESIAN_POINT ( 'NONE',  ( 8.776573235218652513, 13.27486625357121852, -8.183627694784506801 ) ) ;
#149197 = CARTESIAN_POINT ( 'NONE',  ( -0.07694640568740516995, -1.131669979810394633, -1.452919414246391261 ) ) ;
#149198 = AXIS2_PLACEMENT_3D ( 'NONE', #13051, #196095, #178786 ) ;
#149199 = CARTESIAN_POINT ( 'NONE',  ( -11.92619526913699524, 12.57219975838509463, -1.328859060402685976 ) ) ;
#149200 = CARTESIAN_POINT ( 'NONE',  ( 5.184763189090160651, -0.2277032997176874074, -1.856539885857370953 ) ) ;
#149201 = CARTESIAN_POINT ( 'NONE',  ( 5.657495238652423097, 9.822437888394988548, 0.000000000000000000 ) ) ;
#149202 = DIRECTION ( 'NONE',  ( 1.276756478318932585E-15, -1.000000000000000000, 1.665334536937738262E-16 ) ) ;
#149203 = CARTESIAN_POINT ( 'NONE',  ( -5.585596099150174965, 9.460353182409786399, -0.7216878364870207285 ) ) ;
#149204 = CARTESIAN_POINT ( 'NONE',  ( 5.657830175604453338, 5.495223381160312393, 0.7998128361456341429 ) ) ;
#149205 = CARTESIAN_POINT ( 'NONE',  ( 1.692182146996668912, 0.9751594699732427651, -1.711024247558447842 ) ) ;
#149206 = CARTESIAN_POINT ( 'NONE',  ( 2.548454031204652637, -1.388473193742698619, 1.462459214312331168 ) ) ;
#149207 = CARTESIAN_POINT ( 'NONE',  ( -9.020252271793614440, 9.418049160047695878, 0.7998128361456462443 ) ) ;
#149208 = CARTESIAN_POINT ( 'NONE',  ( 6.180537922983273091, 8.303989891604203422, -1.599625672291281386 ) ) ;
#149209 = DIRECTION ( 'NONE',  ( -0.9982742078614211811, 0.000000000000000000, -0.05872483221476467591 ) ) ;
#149210 = CARTESIAN_POINT ( 'NONE',  ( 2.748186945943337012, 0.7392028471469233031, 2.063141171074922120 ) ) ;
#149211 = CARTESIAN_POINT ( 'NONE',  ( 6.516225534515442952, -0.8655890497146904172, -1.607451055071248636 ) ) ;
#149212 = CARTESIAN_POINT ( 'NONE',  ( -3.216308754939891212, 4.775446185561722956, -1.599625672291262513 ) ) ;
#149213 = CARTESIAN_POINT ( 'NONE',  ( 6.825078400183556049, 7.053092130845653784, 2.453807127456457238 ) ) ;
#149214 = CARTESIAN_POINT ( 'NONE',  ( -11.55950211276791428, 13.88000000000000078, -3.221476510067114329 ) ) ;
#149215 = CARTESIAN_POINT ( 'NONE',  ( 4.258669648468278446, 7.022179452304728287, 1.082531754730549078 ) ) ;
#149216 = CARTESIAN_POINT ( 'NONE',  ( 7.099665995050449041, 11.43469409420089455, 0.7998128361456462443 ) ) ;
#149217 = CARTESIAN_POINT ( 'NONE',  ( 3.728655938958122196, 4.308852335994623139, -1.199719254218446718 ) ) ;
#149218 = CARTESIAN_POINT ( 'NONE',  ( 5.695833931516881776, 9.659240330162777610, -0.7216878364870458196 ) ) ;
#149219 = ORIENTED_EDGE ( 'NONE', *, *, #42175, .F. ) ;
#149221 = CARTESIAN_POINT ( 'NONE',  ( 0.6100213217023927603, -0.7224815109628316412, 1.879156614266486391 ) ) ;
#149220 = CARTESIAN_POINT ( 'NONE',  ( 4.915489835137424102, -0.9894786724786635013, -1.552603174752004600 ) ) ;
#149222 = CARTESIAN_POINT ( 'NONE',  ( 3.075839645193487293, 1.666627022722726670, -1.582919517265988674 ) ) ;
#149224 = CARTESIAN_POINT ( 'NONE',  ( 0.8482322855925720217, -1.845984902429298025, -0.2351823381797259749 ) ) ;
#149223 = DIRECTION ( 'NONE',  ( 1.000000000000000000, -7.387867266669436732E-31, 0.000000000000000000 ) ) ;
#149225 = CARTESIAN_POINT ( 'NONE',  ( -3.475000000000000533, -0.02916666666666653876, -2.006292185433948827 ) ) ;
#149226 = CARTESIAN_POINT ( 'NONE',  ( -2.605138072120212200, 6.191078184115536232, -0.7998128361456281477 ) ) ;
#149227 = SURFACE_STYLE_USAGE ( .BOTH. , #20280 ) ;
#149228 = CARTESIAN_POINT ( 'NONE',  ( 3.955252344019274169, -1.661368509396843995, 0.9470704235666274062 ) ) ;
#149229 = CARTESIAN_POINT ( 'NONE',  ( -9.155833807930273238, 9.576227618873799585, -0.7998128361456291469 ) ) ;
#149230 = CARTESIAN_POINT ( 'NONE',  ( -6.956742217587851052, 7.288823140040177506, 0.000000000000000000 ) ) ;
#149233 = CARTESIAN_POINT ( 'NONE',  ( 2.131529507118444133, -1.219933349377068099, -1.418231869465089057 ) ) ;
#149232 = CARTESIAN_POINT ( 'NONE',  ( 3.526972370393847811, -1.930915134098612373, 0.8022322841883463562 ) ) ;
#149231 = B_SPLINE_CURVE_WITH_KNOTS ( 'NONE', 3,
 ( #158120, #193788, #125686, #142959, #177560, #62721, #27019 ),
 .UNSPECIFIED., .F., .F.,
 ( 4, 3, 4 ),
 ( 8.673617379884018139E-19, 0.0008000000000005095049, 0.002977368225425563401 ),
 .UNSPECIFIED. ) ;
#149234 = CARTESIAN_POINT ( 'NONE',  ( 6.643132081016105417, 10.69414516125339887, 0.7216878364870438212 ) ) ;
#149235 = CARTESIAN_POINT ( 'NONE',  ( -1.364683531250010740, 5.301041667008085767, -0.7879004041258300672 ) ) ;
#149236 = CARTESIAN_POINT ( 'NONE',  ( 5.688959394570705541, 1.398425918548395153, 1.197878823674280779 ) ) ;
#149237 = CARTESIAN_POINT ( 'NONE',  ( 2.846322183865124700, 5.408127416896231665, -1.199719254218446718 ) ) ;
#149238 = DIRECTION ( 'NONE',  ( -0.000000000000000000, -0.000000000000000000, 1.000000000000000000 ) ) ;
#149239 = CARTESIAN_POINT ( 'NONE',  ( 5.197747934024010696, -0.6158827634895787106, 1.611369335837910644 ) ) ;
#149240 = CARTESIAN_POINT ( 'NONE',  ( -6.201965203247477909, 9.323044272842313518, 1.199719254218452047 ) ) ;
#149241 = CARTESIAN_POINT ( 'NONE',  ( 0.8438932004057161373, 0.3398822538093429491, -1.700291973301551129 ) ) ;
#149242 = CARTESIAN_POINT ( 'NONE',  ( 6.463508838306311510, 0.3818026259072569983, -2.173449913608487716 ) ) ;
#149244 = EDGE_CURVE ( 'NONE', #113025, #111140, #27920, .T. ) ;
#149243 = CARTESIAN_POINT ( 'NONE',  ( 11.06299035296667732, 11.25683704376094418, -0.9087041361035911313 ) ) ;
#149245 = CIRCLE ( 'NONE', #59264, 11.09999999999999964 ) ;
#149246 = CARTESIAN_POINT ( 'NONE',  ( -1.225000000000016298, 0.8333333340161279690, 0.7072540797572858251 ) ) ;
#149247 = CARTESIAN_POINT ( 'NONE',  ( 4.487298306821032590, 0.1004956810540975631, 2.168842786202809680 ) ) ;
#149248 = CARTESIAN_POINT ( 'NONE',  ( 2.877373901574116211, 1.733520850877915187, -0.5729475677913041798 ) ) ;
#149249 = CARTESIAN_POINT ( 'NONE',  ( 0.9890223832832998330, 0.1386981244183866369, 1.956888703154149534 ) ) ;
#149250 = CARTESIAN_POINT ( 'NONE',  ( 5.296159404803077564, -0.9547103268642830320, -1.889991272064439176 ) ) ;
#149251 = AXIS2_PLACEMENT_3D ( 'NONE', #40510, #71897, #205104 ) ;
#149252 = EDGE_LOOP ( 'NONE', ( #212039, #5418, #197123, #47865 ) ) ;
#149254 = CARTESIAN_POINT ( 'NONE',  ( -1.364683531250012516, 4.051041667008088432, -0.7879004041258300672 ) ) ;
#149253 = CARTESIAN_POINT ( 'NONE',  ( 6.339416484298314280, 0.8816828672218860463, -2.116228320707528976 ) ) ;
#149255 = CARTESIAN_POINT ( 'NONE',  ( 8.432281472695482449, 11.92507992053172572, 1.199719254218450271 ) ) ;
#149256 = CARTESIAN_POINT ( 'NONE',  ( 1.981254353800803836, -1.939921095825656305, -0.8566514584813913480 ) ) ;
#149257 = CARTESIAN_POINT ( 'NONE',  ( -6.087247782855839340, 6.204136622861004646, 0.000000000000000000 ) ) ;
#149258 = CARTESIAN_POINT ( 'NONE',  ( -5.056828107772872727, 5.001980335264194721, -0.7216878364870197293 ) ) ;
#149259 = CARTESIAN_POINT ( 'NONE',  ( 6.192256317468841864, 1.077302059837774273, -1.884901478735945046 ) ) ;
#149261 = CARTESIAN_POINT ( 'NONE',  ( -0.7500000000000006661, 12.73958333401613352, -1.299038105676657340 ) ) ;
#149260 = CARTESIAN_POINT ( 'NONE',  ( 6.983263157960365675, 7.052158404629149224, 2.651961988451009944 ) ) ;
#149263 = VERTEX_POINT ( 'NONE', #97189 ) ;
#149262 = CARTESIAN_POINT ( 'NONE',  ( 2.245073739244434208, 2.155446677131687139, 0.5364521487482876161 ) ) ;
#149264 = CARTESIAN_POINT ( 'NONE',  ( 6.328750030911493241, 0.7691242348151774433, -1.864167186630163009 ) ) ;
#149266 = CARTESIAN_POINT ( 'NONE',  ( 4.838768981748684972, -1.999376597400838174, -0.5061158833775216692 ) ) ;
#149265 = CARTESIAN_POINT ( 'NONE',  ( 5.169736645512481132, 4.925780929386339935, 0.7998128361456341429 ) ) ;
#149268 = CARTESIAN_POINT ( 'NONE',  ( 3.475000000000000533, -3.704166666666666163, 2.006292185433948827 ) ) ;
#149267 = CARTESIAN_POINT ( 'NONE',  ( 5.318541398310776103, 9.426991741329731056, -0.7998128361456481317 ) ) ;
#149269 = CARTESIAN_POINT ( 'NONE',  ( 4.875038752565570732, 7.845239757038595663, -1.199719254218452047 ) ) ;
#149270 = CARTESIAN_POINT ( 'NONE',  ( 1.642778471875001811, -2.880208332855377584, 2.845375778867859751 ) ) ;
#149271 = SURFACE_STYLE_USAGE ( .BOTH. , #99461 ) ;
#149272 = CARTESIAN_POINT ( 'NONE',  ( 0.9200049341780929257, 1.243975779098299927, -1.680105788963416780 ) ) ;
#149273 = CARTESIAN_POINT ( 'NONE',  ( 4.282634502089007533, 1.642705626968201216, -0.8318752211165170163 ) ) ;
#149274 = CARTESIAN_POINT ( 'NONE',  ( 4.330940004561544043, 7.140181541042074365, -1.199719254218452047 ) ) ;
#149275 = CARTESIAN_POINT ( 'NONE',  ( 1.289626238417174831, -0.7804147442260088718, 1.538193839892360471 ) ) ;
#149276 = CARTESIAN_POINT ( 'NONE',  ( 0.3918150239524306189, -2.006371095615328226, 0.2024682584410575914 ) ) ;
#149277 = CARTESIAN_POINT ( 'NONE',  ( 1.881834863725037277, -0.6175646290925532744, -2.214118314682656852 ) ) ;
#149278 = CARTESIAN_POINT ( 'NONE',  ( -4.577849422908604637, 8.492574760035358494, -0.7998128361456281477 ) ) ;
#149279 = CARTESIAN_POINT ( 'NONE',  ( 1.247787707462020723, -1.783668181329477465, -1.391623327695093115 ) ) ;
#149280 = CARTESIAN_POINT ( 'NONE',  ( 3.826872495277617414, 1.999758222635793947, 0.6608955202877621060 ) ) ;
#149281 = CARTESIAN_POINT ( 'NONE',  ( -5.469788628470539926, 5.346117919495872783, -0.7998128361456362523 ) ) ;
#149282 = CARTESIAN_POINT ( 'NONE',  ( 4.937140493670735708, 8.911747675924535983, -0.7998128361456281477 ) ) ;
#149283 = CARTESIAN_POINT ( 'NONE',  ( 5.695833931072550094, 5.817763472438987726, 0.000000000000000000 ) ) ;
#149284 = CARTESIAN_POINT ( 'NONE',  ( 6.656247777566118629, -1.895918425136842833, 0.7852924748303453661 ) ) ;
#149285 = CARTESIAN_POINT ( 'NONE',  ( -4.740547266272593596, 8.682388910626682943, -0.7998128361456281477 ) ) ;
#149286 = UNCERTAINTY_MEASURE_WITH_UNIT (LENGTH_MEASURE( 1.000000000000000082E-05 ), #76691, 'distance_accuracy_value', 'NONE');
#149287 = CARTESIAN_POINT ( 'NONE',  ( 1.499999999999987121, 2.004166666666684637, 0.8660254037844524744 ) ) ;
#149288 = ADVANCED_FACE ( 'NONE', ( #181593 ), #132891, .T. ) ;
#149289 = CARTESIAN_POINT ( 'NONE',  ( -3.113568832632681360, 6.784247404713427798, -0.7998128361456281477 ) ) ;
#149290 = CARTESIAN_POINT ( 'NONE',  ( 5.291355414077095531, -0.05489642510923819357, -2.220905102120291019 ) ) ;
#149291 = CARTESIAN_POINT ( 'NONE',  ( 3.609492757825348175, -2.159078094573213757, 0.3743817768235499499 ) ) ;
#149292 = CARTESIAN_POINT ( 'NONE',  ( -5.922214171070950606, 5.803671375871217286, -0.7998128361456291469 ) ) ;
#149293 = CARTESIAN_POINT ( 'NONE',  ( -3.135678666510573365, 6.880318554229450712, 0.000000000000000000 ) ) ;
#149294 = CARTESIAN_POINT ( 'NONE',  ( 5.320985837513584116, 1.605487267134264595, -1.385306402853322405 ) ) ;
#149295 = CARTESIAN_POINT ( 'NONE',  ( -0.6823417656250003738, 2.967708333674754062, -1.181850606188749264 ) ) ;
#149296 = CARTESIAN_POINT ( 'NONE',  ( 6.889999999999965041, 7.051532193125384040, 2.878152852197481071 ) ) ;
#149297 = CARTESIAN_POINT ( 'NONE',  ( -6.100805936469506641, 6.219954468743612352, 0.7216878364870317197 ) ) ;
#149298 = CARTESIAN_POINT ( 'NONE',  ( 5.853796514643677007, -1.537196951383312804, -1.461068456062891041 ) ) ;
#149299 = CARTESIAN_POINT ( 'NONE',  ( -6.455090533882201775, 8.624301270986276080, -1.443375672974066548 ) ) ;
#149300 = ORIENTED_EDGE ( 'NONE', *, *, #183636, .F. ) ;
#149302 = CARTESIAN_POINT ( 'NONE',  ( 6.702040708066513197, -2.161345696851162845, 0.04751196314212167288 ) ) ;
#149301 = CARTESIAN_POINT ( 'NONE',  ( -3.512971199716682591, 7.112567143062499930, 0.000000000000000000 ) ) ;
#149303 = CARTESIAN_POINT ( 'NONE',  ( 3.655894977179307226, 7.416961240017848844, -0.7998128361456291469 ) ) ;
#149304 = CARTESIAN_POINT ( 'NONE',  ( 6.233933901472759942, 1.822226914158030286, 0.2631550708301691466 ) ) ;
#149305 = CARTESIAN_POINT ( 'NONE',  ( 0.6124999999999759526, 0.8958333340161606095, 1.060881119635896264 ) ) ;
#149306 = CARTESIAN_POINT ( 'NONE',  ( 1.364683531249986537, 2.217708333674751398, -0.7879004041258239610 ) ) ;
#149307 = CARTESIAN_POINT ( 'NONE',  ( 0.8897394992621279197, -0.4213058873485018840, -1.688518545418623340 ) ) ;
#149308 = CARTESIAN_POINT ( 'NONE',  ( 2.683624340501134853, 5.218313266304903664, -1.199719254218446718 ) ) ;
#149310 = ADVANCED_FACE ( 'NONE', ( #65691 ), #195553, .F. ) ;
#149309 = DIRECTION ( 'NONE',  ( 0.000000000000000000, 0.000000000000000000, -1.000000000000000000 ) ) ;
#149311 = CARTESIAN_POINT ( 'NONE',  ( -1.364683531250000748, -0.6781249996585803075, 0.000000000000000000 ) ) ;
#149312 = CARTESIAN_POINT ( 'NONE',  ( 1.419999999999989049, 6.200000000000045475, -2.899999999999995470 ) ) ;
#149313 = CARTESIAN_POINT ( 'NONE',  ( 5.172814640947125397, -2.034155943344346795, -0.7319064324283753864 ) ) ;
#149314 = EDGE_CURVE ( 'NONE', #66325, #94850, #44063, .T. ) ;
#149315 = CARTESIAN_POINT ( 'NONE',  ( -4.457933580795036654, 4.095344020549286590, -0.7998128361456221525 ) ) ;
#149316 = CARTESIAN_POINT ( 'NONE',  ( -6.900736999231456004, 8.113576589600553390, 1.082531754730549967 ) ) ;
#149317 = CARTESIAN_POINT ( 'NONE',  ( 4.592742373648754040, -0.4705147408641910944, -2.109722102427157964 ) ) ;
#149319 = ORIENTED_EDGE ( 'NONE', *, *, #211516, .T. ) ;
#149318 = CARTESIAN_POINT ( 'NONE',  ( -5.008811405605897882, 4.808311159487113073, 0.7998128361456281477 ) ) ;
#149320 = CARTESIAN_POINT ( 'NONE',  ( 1.364683531249990311, 2.634375000341422801, 1.214306433183764966E-14 ) ) ;
#149321 = CARTESIAN_POINT ( 'NONE',  ( 6.503199639966785739, 1.637674054957323433, 1.097108698291071827 ) ) ;
#149322 = CARTESIAN_POINT ( 'NONE',  ( 5.606719662199564524, 0.7002562906495370942, -1.586348028144116462 ) ) ;
#149324 = CARTESIAN_POINT ( 'NONE',  ( 1.734175692058033347, 2.168326105380265378, 0.3173973903456903112 ) ) ;
#149323 = CARTESIAN_POINT ( 'NONE',  ( 0.6801582343749865700, -1.026041666325229418, 1.178068619123805227 ) ) ;
#149325 = CARTESIAN_POINT ( 'NONE',  ( 2.397911878029312494, 1.783863880296262305, 1.463803424465635272 ) ) ;
#149326 = CARTESIAN_POINT ( 'NONE',  ( 5.343066995996487378, -1.769704953023493399, 1.055641863377870138 ) ) ;
#149327 = CARTESIAN_POINT ( 'NONE',  ( 6.427294056597427918, -1.271908742016104821, -1.467670737461545860 ) ) ;
#149328 = CARTESIAN_POINT ( 'NONE',  ( -6.358410854684783509, 9.401601182898824405, -1.082531754730537976 ) ) ;
#149329 = CARTESIAN_POINT ( 'NONE',  ( -2.993318053567081360, 6.714231172462041819, 0.000000000000000000 ) ) ;
#149330 = CARTESIAN_POINT ( 'NONE',  ( -11.86145016429273014, 13.40000000000000036, 1.179999999999997051 ) ) ;
#149331 = CARTESIAN_POINT ( 'NONE',  ( 3.305043459179863419, -0.4174351347619070229, -2.078937965663613774 ) ) ;
#149332 = CARTESIAN_POINT ( 'NONE',  ( 4.929342268689171469, 7.989555622611471897, -1.003472558803005565 ) ) ;
#149333 = CARTESIAN_POINT ( 'NONE',  ( 1.635388916632842360, 0.6352005984417673501, 1.913803229121699534 ) ) ;
#149334 = CARTESIAN_POINT ( 'NONE',  ( -5.205967797523171292, 9.017453497178271604, 0.000000000000000000 ) ) ;
#149335 = CARTESIAN_POINT ( 'NONE',  ( 5.034293675167554660, 1.138177661764948834, -1.890478833441497031 ) ) ;
#149336 = CARTESIAN_POINT ( 'NONE',  ( 3.285556943749998737, -1.392708332855375764, -1.896917185911906500 ) ) ;
#149337 = CARTESIAN_POINT ( 'NONE',  ( 2.149040161283378936, 1.622117262959487549, -0.9118680782764712056 ) ) ;
#149338 = CARTESIAN_POINT ( 'NONE',  ( 0.1399997263886024468, 7.629137130509076492, -2.599723212958489516 ) ) ;
#149339 = FACE_OUTER_BOUND ( 'NONE', #29385, .T. ) ;
#149340 = CARTESIAN_POINT ( 'NONE',  ( 4.021723392342543058, 3.853860420242510632, -2.500000000000000444 ) ) ;
#149342 = CARTESIAN_POINT ( 'NONE',  ( 6.825078400183546279, 2.419143596098617621, 2.525240329153962904 ) ) ;
#149341 = CARTESIAN_POINT ( 'NONE',  ( -5.730308518391983519, 7.387375129167091714, -1.324551712912255486 ) ) ;
#149343 =( LENGTH_UNIT ( ) NAMED_UNIT ( * ) SI_UNIT ( .MILLI., .METRE. ) );
#149344 = ORIENTED_EDGE ( 'NONE', *, *, #95824, .T. ) ;
#149345 = CARTESIAN_POINT ( 'NONE',  ( 3.731368383135937883, -1.904846641313600708, 0.7871492865094924518 ) ) ;
#149346 = CARTESIAN_POINT ( 'NONE',  ( -1.360316468750056851, 2.119791667008092517, -0.7853790794159082322 ) ) ;
#149347 = CARTESIAN_POINT ( 'NONE',  ( -5.422371370461663176, 8.413518134592214537, -1.199719254218446718 ) ) ;
#149348 = CARTESIAN_POINT ( 'NONE',  ( 3.809243936906735239, 1.705047127353828351, -1.082240749027115978 ) ) ;
#149349 = CARTESIAN_POINT ( 'NONE',  ( 1.499999999999985123, -0.4541666666666469010, -0.8660254037844323793 ) ) ;
#149350 = CARTESIAN_POINT ( 'NONE',  ( 4.518945272056516416, 4.166524327021037699, 0.7998128361456341429 ) ) ;
#149351 = AXIS2_PLACEMENT_3D ( 'NONE', #100364, #101430, #15896 ) ;
#149352 = CARTESIAN_POINT ( 'NONE',  ( 1.393510596882661989, 1.559873972335079184, 1.346953478171313057 ) ) ;
#149354 = CARTESIAN_POINT ( 'NONE',  ( -1.364683531250014514, 13.08854166700806410, -0.7879004041258335089 ) ) ;
#149353 = DIRECTION ( 'NONE',  ( 1.000000000000000000, 0.000000000000000000, 0.000000000000000000 ) ) ;
#149355 = CARTESIAN_POINT ( 'NONE',  ( 4.873266149108180123, 7.772895376346490970, 1.199719254218462483 ) ) ;
#149356 = CARTESIAN_POINT ( 'NONE',  ( -0.2408018239684278916, 2.008845716682732263, -2.515352618630611659 ) ) ;
#149357 = CARTESIAN_POINT ( 'NONE',  ( 1.411775340717499994, 1.237668241052336970, -1.363247244775968259 ) ) ;
#149358 = CARTESIAN_POINT ( 'NONE',  ( 6.481111342790009999, -0.1036386110354891726, -2.204582208980155222 ) ) ;
#149359 = CARTESIAN_POINT ( 'NONE',  ( 5.550083779947807550, 7.568460058062819407, -1.599625672291283607 ) ) ;
#149360 = CARTESIAN_POINT ( 'NONE',  ( 1.019082891775088484, 1.996809913787592095, 0.8282600050937348746 ) ) ;
#149361 = CARTESIAN_POINT ( 'NONE',  ( -4.799223189557577207, 4.701441264013013210, 0.7216878364870317197 ) ) ;
#149362 = CARTESIAN_POINT ( 'NONE',  ( 2.430875351317234756, -1.673853735218135741, 1.124246214196801485 ) ) ;
#149363 = CARTESIAN_POINT ( 'NONE',  ( 0.1399997263886024468, 7.629137130509076492, -2.599723212958489516 ) ) ;
#149364 = FACE_OUTER_BOUND ( 'NONE', #181040, .T. ) ;
#149365 = CARTESIAN_POINT ( 'NONE',  ( 2.969872605471105764, 6.605953636083951253, 0.1972538285620730192 ) ) ;
#149366 = CARTESIAN_POINT ( 'NONE',  ( 4.241065053910620719, -1.715758787085974957, 0.9708604712577516560 ) ) ;
#149367 = CARTESIAN_POINT ( 'NONE',  ( 3.028530041973789722, 0.4946322284519070189, 1.954779462066410733 ) ) ;
#149369 = CARTESIAN_POINT ( 'NONE',  ( 8.527715432871318058, 12.89282573841782664, -0.7216878364870338292 ) ) ;
#149368 = CARTESIAN_POINT ( 'NONE',  ( 1.364683531249986537, 2.155208333674751398, -0.7879004041258239610 ) ) ;
#149371 = CARTESIAN_POINT ( 'NONE',  ( 5.971333374016301043, 0.1563851966441217600, -2.100315135224324337 ) ) ;
#149370 = CARTESIAN_POINT ( 'NONE',  ( -6.191269702934848240, 10.37489842006599616, 0.000000000000000000 ) ) ;
#149372 = CARTESIAN_POINT ( 'NONE',  ( 5.107906530550561541, 0.6527686194882609261, -1.964817160181751010 ) ) ;
#149373 = CARTESIAN_POINT ( 'NONE',  ( 6.388916700537700777, 8.476822122092563916, 1.599625672291281386 ) ) ;
#149374 = CARTESIAN_POINT ( 'NONE',  ( -6.418895661066105873, 9.576129806964074120, -1.199719254218440723 ) ) ;
#149375 = CARTESIAN_POINT ( 'NONE',  ( 6.639320575229256782, 3.693993153770461113, 2.517469677323687538 ) ) ;
#149376 = CARTESIAN_POINT ( 'NONE',  ( 4.869401706892690029, -1.708532917064720991, -1.076912495999365449 ) ) ;
#149377 = CARTESIAN_POINT ( 'NONE',  ( 0.7499999999999885647, -0.4854166659838468623, 1.299038105676657340 ) ) ;
#149378 = CARTESIAN_POINT ( 'NONE',  ( 3.370030522709596355, 2.251568201494443588, -0.5052104078027676026 ) ) ;
#149379 = CARTESIAN_POINT ( 'NONE',  ( 1.006769942787159033, 0.5948965838462864086, 1.974949077847313328 ) ) ;
#149380 = CARTESIAN_POINT ( 'NONE',  ( 9.259855728453651125, 9.905512559391842942, 1.040834085586084257E-14 ) ) ;
#149381 = ADVANCED_FACE ( 'NONE', ( #20399 ), #87555, .F. ) ;
#149382 = CARTESIAN_POINT ( 'NONE',  ( 6.017840079619279692, 8.114175741012878973, -1.599625672291281386 ) ) ;
#149383 = CARTESIAN_POINT ( 'NONE',  ( 6.059568310664962709, 6.034194215389424798, 0.7998128361456352531 ) ) ;
#149384 = CARTESIAN_POINT ( 'NONE',  ( 1.364683531249988757, 1.196875000341421469, 0.000000000000000000 ) ) ;
#149385 = CARTESIAN_POINT ( 'NONE',  ( 5.065906673361608270, 5.939254536123854677, -1.199719254218450271 ) ) ;
#149386 = CARTESIAN_POINT ( 'NONE',  ( 6.114364089638782751, 9.116879957011832403, 1.082531754730558626 ) ) ;
#149388 = SURFACE_SIDE_STYLE ('',( #34561 ) ) ;
#149387 = CARTESIAN_POINT ( 'NONE',  ( 3.613895077877467443, 0.5305607931336644434, -2.105228361949755378 ) ) ;
#149389 = CARTESIAN_POINT ( 'NONE',  ( 4.067155351693835485E-15, 1.250000000682825130, -1.225000000000013411 ) ) ;
#149391 = CARTESIAN_POINT ( 'NONE',  ( 3.034521004542716227, -1.622529355458858236, 0.8704296449140033198 ) ) ;
#149390 = CARTESIAN_POINT ( 'NONE',  ( -4.365362273920257330, 6.116008624372160973, 1.443375672974064550 ) ) ;
#149392 = CARTESIAN_POINT ( 'NONE',  ( 0.6823417656249917140, 5.092708333674749177, 1.181850606188765695 ) ) ;
#149393 = CARTESIAN_POINT ( 'NONE',  ( 4.054362073078698891, -1.623213109359676443, 1.472610181411204922 ) ) ;
#149394 = CARTESIAN_POINT ( 'NONE',  ( -2.494940289813118994, 3.447199233515649386, 11.73777120880565583 ) ) ;
#149395 = CARTESIAN_POINT ( 'NONE',  ( 4.979486748501788185, 2.112903116282875082, -0.8095491994110515233 ) ) ;
#149396 = DIRECTION ( 'NONE',  ( 0.000000000000000000, 0.000000000000000000, -1.000000000000000000 ) ) ;
#149397 = CARTESIAN_POINT ( 'NONE',  ( 5.772745519453025054, 7.247817053759448847, -1.191736586928717978 ) ) ;
#149398 = CARTESIAN_POINT ( 'NONE',  ( -5.844973620822877969, 7.912498205750389424, 1.443375672974058777 ) ) ;
#149399 = CARTESIAN_POINT ( 'NONE',  ( 5.126391479742934187, 6.113783160189109722, -1.082531754730548412 ) ) ;
#149400 = CARTESIAN_POINT ( 'NONE',  ( 6.028513167084792457, 1.705988696259161719, 0.4703064415670314413 ) ) ;
#149401 = VECTOR ( 'NONE', #207893, 1000.000000000000000 ) ;
#149402 = CARTESIAN_POINT ( 'NONE',  ( 4.160795161724285762, 0.5389290103979550439, 1.939535095694967959 ) ) ;
#149403 = CARTESIAN_POINT ( 'NONE',  ( 7.121056995675668411, 9.330985799753529264, -1.599625672291262513 ) ) ;
#149404 = CARTESIAN_POINT ( 'NONE',  ( 3.276497419027382563, -1.255868110884267530, 1.690353172608966448 ) ) ;
#149405 = CARTESIAN_POINT ( 'NONE',  ( 0.7201576878450620667, 1.887430420354209160, 0.3262839321072578125 ) ) ;
#149406 = COLOUR_RGB ( '', 0.40784314, 0.44705882, 0.49803922) ;
#149408 = CARTESIAN_POINT ( 'NONE',  ( 3.388648328411762556, 6.040841252200647382, 1.199719254218462483 ) ) ;
#149407 = CARTESIAN_POINT ( 'NONE',  ( -0.6823417656250039265, 12.31770833367473017, -1.181850606188755259 ) ) ;
#149409 = CARTESIAN_POINT ( 'NONE',  ( 2.137097444212227693, -0.09349721708603592196, -1.967446466973846952 ) ) ;
#149410 = CARTESIAN_POINT ( 'NONE',  ( 0.9185735243398345240, 1.726912363944958617, 0.7195956246372691156 ) ) ;
#149411 = CARTESIAN_POINT ( 'NONE',  ( 0.5726126529861442771, 1.355618539282506640, -1.418395753018865113 ) ) ;
#149413 = ORIENTED_EDGE ( 'NONE', *, *, #176059, .F. ) ;
#149412 = CARTESIAN_POINT ( 'NONE',  ( -0.05268457437105152075, -1.747710896673961622, 0.7768168958157274373 ) ) ;
#149414 = CARTESIAN_POINT ( 'NONE',  ( 5.558479791922850133, 6.547609847740540445, -1.082531754730542195 ) ) ;
#149415 = CARTESIAN_POINT ( 'NONE',  ( 0.6823417656249899377, 1.155208333674752286, 1.181850606188755259 ) ) ;
#149416 = CARTESIAN_POINT ( 'NONE',  ( 6.227412191919261986, -1.760757567598171480, 0.6321290105378990498 ) ) ;
#149417 = CARTESIAN_POINT ( 'NONE',  ( 0.000000000000000000, 1.899999999999999023, 0.000000000000000000 ) ) ;
#149418 = CARTESIAN_POINT ( 'NONE',  ( 6.192251260771239885, 1.025525066348543568, -1.798363755310352419 ) ) ;
#149419 = CARTESIAN_POINT ( 'NONE',  ( 0.000000000000000000, 3.079999999999999183, -6.329999999999995630 ) ) ;
#149420 = CARTESIAN_POINT ( 'NONE',  ( 0.4321921490204432281, 1.190796696626210682, 1.693455153822187587 ) ) ;
#149421 = CARTESIAN_POINT ( 'NONE',  ( -1.500000000000013101, -0.07916666666664513852, 0.8660254037844403729 ) ) ;
#149422 = CARTESIAN_POINT ( 'NONE',  ( 6.938021921891177612, 9.117444880338284818, -1.599625672291262513 ) ) ;
#149423 = CARTESIAN_POINT ( 'NONE',  ( -6.679363233026820446, 10.94434087183997129, 0.000000000000000000 ) ) ;
#149424 = CARTESIAN_POINT ( 'NONE',  ( 6.042093733545556233, 7.078139439671806699, -1.199719254218452047 ) ) ;
#149425 = CARTESIAN_POINT ( 'NONE',  ( 4.061549535745618833, 6.896169004081968090, -1.199719254218452047 ) ) ;
#149426 = EDGE_CURVE ( 'NONE', #87946, #58569, #40951, .T. ) ;
#149427 = CARTESIAN_POINT ( 'NONE',  ( -0.6823417656250003738, 1.717708333674752730, -1.181850606188749264 ) ) ;
#149428 = CARTESIAN_POINT ( 'NONE',  ( 0.7499999999999902300, 2.233333333333351156, 1.299038105676669330 ) ) ;
#149430 = CARTESIAN_POINT ( 'NONE',  ( 5.183294799126148433, 4.941598775268944976, 1.040834085586084257E-14 ) ) ;
#149429 = CARTESIAN_POINT ( 'NONE',  ( 5.810985101215744741, -1.547553103248515027, 1.205733875218002238 ) ) ;
#149431 = ADVANCED_FACE ( 'NONE', ( #24665 ), #95870, .T. ) ;
#149432 = CARTESIAN_POINT ( 'NONE',  ( 3.725935337077026510, -1.776739457207517248, -0.9528653653038119398 ) ) ;
#149433 = CARTESIAN_POINT ( 'NONE',  ( 3.186650014752292925, 1.506923149468800682, -1.182699731353755501 ) ) ;
#149434 = CARTESIAN_POINT ( 'NONE',  ( -1.913843809498090520, 3.268536626279805013, -0.4294081188993455478 ) ) ;
#149435 = CARTESIAN_POINT ( 'NONE',  ( 1.031118135130421498, -1.979082047791239418, 0.9416876394413643547 ) ) ;
#149436 = CARTESIAN_POINT ( 'NONE',  ( 0.1331715793776860612, 5.723291439345874920, -2.547624684121822636 ) ) ;
#149437 = CARTESIAN_POINT ( 'NONE',  ( 3.022558680773678397, 1.760047114015901526, 0.6337009143728977723 ) ) ;
#149438 = CARTESIAN_POINT ( 'NONE',  ( 1.499999999999987121, -0.4645833326505149907, 0.8660254037844524744 ) ) ;
#149439 = CARTESIAN_POINT ( 'NONE',  ( -8.193204901359996128, 8.453160561208463264, 1.040834085586084257E-14 ) ) ;
#149441 = CARTESIAN_POINT ( 'NONE',  ( 4.569977310993092345, -0.9968198436792906625, 1.867865768302608531 ) ) ;
#149440 = CARTESIAN_POINT ( 'NONE',  ( -3.904385051055635270, 6.538571078664754843, 1.082531754730560403 ) ) ;
#149442 = CARTESIAN_POINT ( 'NONE',  ( -1.416502993825243362, 13.32998166073656066, -0.1108442676237804125 ) ) ;
#149443 = CARTESIAN_POINT ( 'NONE',  ( 6.004363041306050697, 2.067815565686380364, 0.1054426792976848049 ) ) ;
#149445 = CARTESIAN_POINT ( 'NONE',  ( -1.821370322827221777, -3.469446951953614189E-15, -0.2913868168252300994 ) ) ;
#149444 = CARTESIAN_POINT ( 'NONE',  ( 2.384421550557855429, -0.3601958963256215451, -2.059324561056875336 ) ) ;
#149447 = EDGE_LOOP ( 'NONE', ( #166843, #105972, #76761, #156661 ) ) ;
#149446 = CARTESIAN_POINT ( 'NONE',  ( 0.2347969022384633897, -1.580228140511737100, 0.6916409326972148275 ) ) ;
#149448 = CARTESIAN_POINT ( 'NONE',  ( 7.070740804726770357, 8.207951346058097286, 1.199719254218462483 ) ) ;
#149449 = CARTESIAN_POINT ( 'NONE',  ( 6.925078400183550364, -0.007619068086212391067, 2.144148427808051594 ) ) ;
#149451 = PRESENTATION_LAYER_ASSIGNMENT (  '', '', ( #28391 ) ) ;
#149450 = DIRECTION ( 'NONE',  ( -0.000000000000000000, -1.000000000000000000, -0.000000000000000000 ) ) ;
#149452 = CARTESIAN_POINT ( 'NONE',  ( -10.24086661081948435, 5.004020940043352184, 7.476643068812830251 ) ) ;
#149453 = CARTESIAN_POINT ( 'NONE',  ( 7.931156673870037643, 8.355363662377600420, -0.7216878364870267237 ) ) ;
#149454 = CARTESIAN_POINT ( 'NONE',  ( 1.419999999999989049, 6.280000000000035776, 2.775557561562891351E-14 ) ) ;
#149456 = CARTESIAN_POINT ( 'NONE',  ( 1.049118701917159946, -1.638035101892039602, 0.7738018112423280526 ) ) ;
#149455 = CARTESIAN_POINT ( 'NONE',  ( 6.156284269057003655, 9.340026192945279249, -1.199719254218452047 ) ) ;
#149457 = CARTESIAN_POINT ( 'NONE',  ( -7.182068686937172153, 9.402166106225269715, 1.599625672291283607 ) ) ;
#149458 = CARTESIAN_POINT ( 'NONE',  ( 3.032219910950674890, 6.689340329417765574, 0.7998128361456321445 ) ) ;
#149459 = CARTESIAN_POINT ( 'NONE',  ( -5.819752210671484960, 7.227523004248635807, 1.175121323085267289 ) ) ;
#149460 = CARTESIAN_POINT ( 'NONE',  ( 6.119526231721748033, 8.232809585132461194, 1.599625672291269396 ) ) ;
#149461 = DIRECTION ( 'NONE',  ( 5.551115123125764829E-17, 0.000000000000000000, -1.000000000000000000 ) ) ;
#149462 = CARTESIAN_POINT ( 'NONE',  ( 1.499999999999993117, 9.104166666666666075, 0.8660254037844408170 ) ) ;
#149463 = CARTESIAN_POINT ( 'NONE',  ( -11.35569630219380777, 11.11268439291364452, 3.554478010595060411 ) ) ;
#149464 = CARTESIAN_POINT ( 'NONE',  ( 8.866669273657322492, 12.32790267170016207, -1.082531754730543083 ) ) ;
#149465 = EDGE_LOOP ( 'NONE', ( #10508, #90591, #147782, #192892 ) ) ;
#149466 = CARTESIAN_POINT ( 'NONE',  ( 3.226847753617521963, -1.718569378881330989, -0.7146659259855172586 ) ) ;
#149467 = CARTESIAN_POINT ( 'NONE',  ( 0.9310837752575386039, -1.510843254991366402, -1.177573636344444896 ) ) ;
#149468 = CARTESIAN_POINT ( 'NONE',  ( 6.334985678650366658, 0.1896739171414266178, 1.917017188598265420 ) ) ;
#149469 = CARTESIAN_POINT ( 'NONE',  ( -1.432719062495390716, -3.042800438942089514, 3.165902886691621010 ) ) ;
#149471 = ADVANCED_FACE ( 'NONE', ( #187173 ), #88631, .T. ) ;
#149470 = AXIS2_PLACEMENT_3D ( 'NONE', #80632, #146724, #66466 ) ;
#149472 = DIRECTION ( 'NONE',  ( 0.000000000000000000, 0.000000000000000000, 1.000000000000000000 ) ) ;
#149473 = CARTESIAN_POINT ( 'NONE',  ( -1.579999999999998073, 8.674529973577531194, -2.499999999999990230 ) ) ;
#149474 = CARTESIAN_POINT ( 'NONE',  ( -4.961921032921567054, 4.891255414604337659, 0.7216878364870317197 ) ) ;
#149475 = CARTESIAN_POINT ( 'NONE',  ( 8.215877900201359552, 11.56864606933486606, -1.082531754730543083 ) ) ;
#149476 = CARTESIAN_POINT ( 'NONE',  ( 4.856285946018928712, -1.968934436971051305, -0.05237921274019693985 ) ) ;
#149477 = CARTESIAN_POINT ( 'NONE',  ( 1.119968162728638417, -0.5116716972351254000, 2.057716464106795318 ) ) ;
#149478 = CARTESIAN_POINT ( 'NONE',  ( -6.067437437315529536, 7.037430750744921859, 1.199719254218450271 ) ) ;
#149479 = DIRECTION ( 'NONE',  ( -1.000000000000000000, 5.578564026256490882E-16, 2.058387550816952846E-48 ) ) ;
#149480 = DIRECTION ( 'NONE',  ( 0.7592566023653005702, 0.6507913734559639396, 0.000000000000000000 ) ) ;
#149481 = CARTESIAN_POINT ( 'NONE',  ( 5.824229312739954700, 2.111140916326431416, 0.5876101183235474812 ) ) ;
#149482 = CARTESIAN_POINT ( 'NONE',  ( -1.250000000000035749, 8.500000000000000000, -9.921567416492205638 ) ) ;
#149483 = CARTESIAN_POINT ( 'NONE',  ( 4.541967935523826938, 0.8243062533531859692, -1.741262965308258970 ) ) ;
#149484 = CARTESIAN_POINT ( 'NONE',  ( -5.845536785786364931, 9.971543350059432598, 0.000000000000000000 ) ) ;
#149485 = CARTESIAN_POINT ( 'NONE',  ( 0.5690311950540331010, 0.1842100624489529381, -1.816270042949569730 ) ) ;
#149486 = CARTESIAN_POINT ( 'NONE',  ( 1.506762622594171930, -0.7967928049063889295, -2.058199171410409978 ) ) ;
#149487 = CARTESIAN_POINT ( 'NONE',  ( -0.1399574524686796051, 8.210952333604124576, 2.038660652713628618 ) ) ;
#149488 = ORIENTED_EDGE ( 'NONE', *, *, #2982, .T. ) ;
#149489 = DIRECTION ( 'NONE',  ( -0.6507913734559642727, -0.7592566023653003482, -2.775557561562895049E-17 ) ) ;
#149490 = ORIENTED_EDGE ( 'NONE', *, *, #44167, .F. ) ;
#149491 = CARTESIAN_POINT ( 'NONE',  ( 6.016450702237627901, 0.7947307017554460229, 1.802146183335861629 ) ) ;
#149492 = CARTESIAN_POINT ( 'NONE',  ( 1.540467339043756434, -1.639628711884850265, 1.040515435762645380 ) ) ;
#149493 = CARTESIAN_POINT ( 'NONE',  ( 6.890000000000009450, -0.01081285896028030651, 2.279840171838908525 ) ) ;
#149495 = CARTESIAN_POINT ( 'NONE',  ( 4.645250437676715194, 1.663689067502411412, -0.8338919413633429922 ) ) ;
#149494 = CARTESIAN_POINT ( 'NONE',  ( -5.610041701004606196, 9.767075427805856691, -0.7998128361456362523 ) ) ;
#149496 = CARTESIAN_POINT ( 'NONE',  ( 7.537407054554579489, 7.758339416593960536, 0.000000000000000000 ) ) ;
#149497 = CARTESIAN_POINT ( 'NONE',  ( 9.858406733136186526E-16, 7.849261790823902629, -8.049999999999993605 ) ) ;
#149498 = CARTESIAN_POINT ( 'NONE',  ( 0.000000000000000000, 10.00000000000000888, 0.000000000000000000 ) ) ;
#149499 = CARTESIAN_POINT ( 'NONE',  ( -5.530836599371015794, 8.540060901653093950, 1.199719254218452047 ) ) ;
#149500 = CARTESIAN_POINT ( 'NONE',  ( -6.064239847062411926, 10.29697326487330500, 0.000000000000000000 ) ) ;
#149501 = CARTESIAN_POINT ( 'NONE',  ( 0.2928600448571066495, 1.818678932476354149, -1.222557900829209121 ) ) ;
#149502 = CARTESIAN_POINT ( 'NONE',  ( 5.368665641331531013, 5.365790791082654998, -0.7216878364870207285 ) ) ;
#149503 = CIRCLE ( 'NONE', #69992, 4.000000000000000000 ) ;
#149504 = DIRECTION ( 'NONE',  ( 0.000000000000000000, 1.000000000000000000, 0.000000000000000000 ) ) ;
#149505 = DIRECTION ( 'NONE',  ( 0.9510565162951521989, 0.000000000000000000, -0.3090169943749515591 ) ) ;
#149506 = CARTESIAN_POINT ( 'NONE',  ( 1.084280211047653264, -1.780658692889337091, -0.4022698149812459212 ) ) ;
#149507 = CARTESIAN_POINT ( 'NONE',  ( -2.774614992291035698, 6.388801257648172971, 1.040834085586084257E-14 ) ) ;
#149508 = B_SPLINE_CURVE_WITH_KNOTS ( 'NONE', 3,
 ( #119607, #37221, #103295, #169356, #20942, #5751 ),
 .UNSPECIFIED., .F., .F.,
 ( 4, 2, 4 ),
 ( 0.0007479271397814149687, 0.001059363759668584780, 0.001370800379555754591 ),
 .UNSPECIFIED. ) ;
#149509 = CARTESIAN_POINT ( 'NONE',  ( 3.410549273128512304, -1.036309148604511288, -1.390238610006881981 ) ) ;
#149510 = CARTESIAN_POINT ( 'NONE',  ( -6.285146472706256482, 6.979120928820362835, -0.9578508296879204575 ) ) ;
#149511 = CARTESIAN_POINT ( 'NONE',  ( 0.6311622855796339415, 3.299999999999983391, 0.3999999999999593880 ) ) ;
#149512 = CARTESIAN_POINT ( 'NONE',  ( 1.271070482941954571, 8.436788551174016604, -10.93994114196923029 ) ) ;
#149513 = CARTESIAN_POINT ( 'NONE',  ( 6.147073579019600054, -1.539581890156189292, 0.9809480439507823890 ) ) ;
#149514 = CARTESIAN_POINT ( 'NONE',  ( 4.873855640358407904, -1.924671727690111966, 0.3787619532854279436 ) ) ;
#149515 = CARTESIAN_POINT ( 'NONE',  ( -8.148614017013223076, 9.465470093725620870, -1.199719254218446718 ) ) ;
#149516 = CARTESIAN_POINT ( 'NONE',  ( 5.341022448779654930, 8.318611059296550536, 1.199719254218462483 ) ) ;
#149517 = CARTESIAN_POINT ( 'NONE',  ( 4.248766647586673884, 2.079802475202694900, 0.4125236972643344102 ) ) ;
#149518 = CARTESIAN_POINT ( 'NONE',  ( 1.459778984583645340E-15, 18.91999999999999815, -11.92000000000000171 ) ) ;
#149519 = CARTESIAN_POINT ( 'NONE',  ( -9.169391961543940539, 9.592045464756413509, 1.040834085586084257E-14 ) ) ;
#149520 = CARTESIAN_POINT ( 'NONE',  ( 5.465584804120450002, 6.402597129658848196, -1.225016630617669744 ) ) ;
#149521 = CARTESIAN_POINT ( 'NONE',  ( 2.360293207207576849, -2.069885933316969240, 0.04650197241463926989 ) ) ;
#149523 = CARTESIAN_POINT ( 'NONE',  ( -0.6823417656250246877, 0.6135416670080897639, 1.181850606188755259 ) ) ;
#149522 = CARTESIAN_POINT ( 'NONE',  ( 3.332481584934672281, 7.719208080883574574, -2.450691333334232613 ) ) ;
#149524 = VERTEX_POINT ( 'NONE', #190365 ) ;
#149525 = CARTESIAN_POINT ( 'NONE',  ( 2.409158461118418693, -1.326566255432750197, -1.877132621748223373 ) ) ;
#149526 = CARTESIAN_POINT ( 'NONE',  ( 8.920901888112002354, 9.510066412326583674, 0.7216878364870438212 ) ) ;
#149528 = CARTESIAN_POINT ( 'NONE',  ( -3.285556943750000514, -3.288541666188709023, -1.896917185911906500 ) ) ;
#149527 = CARTESIAN_POINT ( 'NONE',  ( 6.861835142292143530, 8.138467433163244280, 1.082531754730549967 ) ) ;
#149529 = FACE_OUTER_BOUND ( 'NONE', #8377, .T. ) ;
#149530 = FACE_OUTER_BOUND ( 'NONE', #120038, .T. ) ;
#149531 = ORIENTED_EDGE ( 'NONE', *, *, #64709, .T. ) ;
#149532 = CARTESIAN_POINT ( 'NONE',  ( 4.779848517908583894, 4.883929213520019630, -0.7538207499340529028 ) ) ;
#149533 = CARTESIAN_POINT ( 'NONE',  ( 3.779479514802902340, 0.2291398179169491789, -1.898525689255560422 ) ) ;
#149534 = CARTESIAN_POINT ( 'NONE',  ( 0.08113548435146850091, 6.430127061359857343, -3.206836081813071004 ) ) ;
#149535 = CARTESIAN_POINT ( 'NONE',  ( 5.332891432879703686, 0.1301960547291525494, 1.719897333435776776 ) ) ;
#149536 = CARTESIAN_POINT ( 'NONE',  ( 3.415250174187448362, -1.861344788686780438, 0.7762291900053899241 ) ) ;
#149537 = CARTESIAN_POINT ( 'NONE',  ( 4.834794202738506463, 0.7220915915403209873, -2.182417960738481710 ) ) ;
#149538 = CARTESIAN_POINT ( 'NONE',  ( 11.48788097203293823, 11.33043054397688465, 3.469500700354830158 ) ) ;
#149539 = CARTESIAN_POINT ( 'NONE',  ( 1.032169062358662348, -1.402649970393770484, -1.703791656331831605 ) ) ;
#149540 = CARTESIAN_POINT ( 'NONE',  ( -3.838366886444665393, 7.492195444245147939, 0.000000000000000000 ) ) ;
#149541 = CARTESIAN_POINT ( 'NONE',  ( 6.204346024843479412, -0.6390883176130756071, -1.650510209504873593 ) ) ;
#149543 = CARTESIAN_POINT ( 'NONE',  ( 2.203457528917366570, -0.4999491416500188579, 2.236933425931705521 ) ) ;
#149542 = CARTESIAN_POINT ( 'NONE',  ( 7.049313524462606395, 7.188896964819984525, 0.000000000000000000 ) ) ;
#149544 = CARTESIAN_POINT ( 'NONE',  ( 0.2337849711155593480, 0.2922425735506446465, 1.715447441342861534 ) ) ;
#149545 = CARTESIAN_POINT ( 'NONE',  ( -7.445362632559989535, 8.715286488521982733, 1.199719254218452047 ) ) ;
#149546 = CARTESIAN_POINT ( 'NONE',  ( 6.404242042726283834, 1.626525233829802408, -1.468802942141099077 ) ) ;
#149547 = CARTESIAN_POINT ( 'NONE',  ( -3.305155586681401303, 7.078041627762083898, 0.7998128361456352531 ) ) ;
#149548 = DIRECTION ( 'NONE',  ( 0.000000000000000000, 1.804652791718263484E-16, -1.000000000000000000 ) ) ;
#149549 = CARTESIAN_POINT ( 'NONE',  ( -8.800111196542582448, 15.51845924339754390, 8.208664638256164992 ) ) ;
#149550 = CARTESIAN_POINT ( 'NONE',  ( 6.514133371570012265, 2.065101995627930620, -0.1482383472809906122 ) ) ;
#149551 = CARTESIAN_POINT ( 'NONE',  ( 1.569546381206438967, 1.394087592100446971, 1.457234012747665508 ) ) ;
#149552 = CIRCLE ( 'NONE', #211847, 10.91999999999999105 ) ;
#149553 = CARTESIAN_POINT ( 'NONE',  ( 1.499999999999987121, 0.07708333401615156955, -0.8660254037844323793 ) ) ;
#149554 = CARTESIAN_POINT ( 'NONE',  ( 5.145112535762402572, -1.651256390841379762, 0.9921342509419928124 ) ) ;
#149555 = CARTESIAN_POINT ( 'NONE',  ( 1.364683531250000303, 12.00520833367473195, -0.7879004041258355073 ) ) ;
#149556 = CARTESIAN_POINT ( 'NONE',  ( 2.566880079249767022, 0.7526719050801253807, 2.090118821510750458 ) ) ;
#149557 = ORIENTED_EDGE ( 'NONE', *, *, #176737, .F. ) ;
#149559 = AXIS2_PLACEMENT_3D ( 'NONE', #172952, #90639, #156699 ) ;
#149558 = CARTESIAN_POINT ( 'NONE',  ( -6.385527162356468445, 10.39360608948380538, 1.040834085586084257E-14 ) ) ;
#149560 = CARTESIAN_POINT ( 'NONE',  ( 0.000000000000000000, -1.500000000000001332, 0.000000000000000000 ) ) ;
#149561 = CARTESIAN_POINT ( 'NONE',  ( 10.21336978979620191, 10.81001959771741205, 0.7998128361456462443 ) ) ;
#149562 = CARTESIAN_POINT ( 'NONE',  ( 0.000000000000000000, 5.999999999999998224, 0.000000000000000000 ) ) ;
#149563 = CARTESIAN_POINT ( 'NONE',  ( 3.799227641567938019, 7.351783938512805427, -0.4255155205789330486 ) ) ;
#149564 = CARTESIAN_POINT ( 'NONE',  ( 3.966134247641060817, -1.625707123410979449, -0.6219663355369866586 ) ) ;
#149566 = ADVANCED_FACE ( 'NONE', ( #6272 ), #34858, .T. ) ;
#149565 = CARTESIAN_POINT ( 'NONE',  ( 3.754310534785664899, -1.959519245081872585, -0.09869234604030494018 ) ) ;
#149568 = CARTESIAN_POINT ( 'NONE',  ( -5.910991785878158211, 9.839981483592442402, -0.7216878364870278340 ) ) ;
#149567 = CARTESIAN_POINT ( 'NONE',  ( 4.467575310902914154, 5.170924936596891008, 1.199719254218464037 ) ) ;
#149569 = CARTESIAN_POINT ( 'NONE',  ( -5.811497925844209433, 6.060560459143458978, 0.5261113891226586459 ) ) ;
#149570 = CARTESIAN_POINT ( 'NONE',  ( 8.380911511541880188, 12.92948053010758258, 0.7998128361456462443 ) ) ;
#149571 = CARTESIAN_POINT ( 'NONE',  ( 0.8716181059342765769, -0.3045769538833371648, 2.039966307373513033 ) ) ;
#149572 = CARTESIAN_POINT ( 'NONE',  ( -6.482770005628665011, 10.71498210654212002, 0.7998128361456481317 ) ) ;
#149573 = CARTESIAN_POINT ( 'NONE',  ( -3.077337680177623103, 6.534051693608437184, 0.7216878364870317197 ) ) ;
#149574 = CARTESIAN_POINT ( 'NONE',  ( 1.587200854914575077, -0.3333832325802545404, -2.237697771577638051 ) ) ;
#149575 = ORIENTED_EDGE ( 'NONE', *, *, #179256, .F. ) ;
#149576 = CARTESIAN_POINT ( 'NONE',  ( -1.402160292154681736E-14, 0.1187500006828157706, -1.732050807568870754 ) ) ;
#149577 = CARTESIAN_POINT ( 'NONE',  ( 2.284254421533092216, -1.833544361078912388, -0.3693468884775341077 ) ) ;
#149578 = CARTESIAN_POINT ( 'NONE',  ( 1.353744004007218615, 0.1277301157788513497, -1.729473920685227428 ) ) ;
#149579 = CARTESIAN_POINT ( 'NONE',  ( 5.073855206572205567, -1.217758175834412260, 1.821886007100224969 ) ) ;
#149580 = CARTESIAN_POINT ( 'NONE',  ( 6.176872536373793743, -2.188556106905717780, -0.7317919303653409591 ) ) ;
#149581 = CARTESIAN_POINT ( 'NONE',  ( 1.481398948507294477, 1.904550386266171902, -0.7878645111692607061 ) ) ;
#149582 = CARTESIAN_POINT ( 'NONE',  ( 3.574105527548767647, -1.871835235816914578, -0.5168888941823551741 ) ) ;
#149583 = CARTESIAN_POINT ( 'NONE',  ( -3.077337680177623103, 6.534051693608437184, 0.7216878364870317197 ) ) ;
#149584 = CARTESIAN_POINT ( 'NONE',  ( 5.747288119592351308, -1.474170506619469023, -1.151262835514428540 ) ) ;
#149585 = CARTESIAN_POINT ( 'NONE',  ( 1.343750000000001110, 1.895863743164117654, 0.7852924748299160429 ) ) ;
#149586 = CARTESIAN_POINT ( 'NONE',  ( 4.000938479675252069, 7.594566414207783112, 0.1672846332331431873 ) ) ;
#149587 = CARTESIAN_POINT ( 'NONE',  ( 6.274767501101933043, -2.001204493855372579, 0.2439949869823473949 ) ) ;
#149589 = EDGE_CURVE ( 'NONE', #30492, #160543, #62507, .T. ) ;
#149588 = CARTESIAN_POINT ( 'NONE',  ( 3.445180431648323882, 6.073108699348104267, 1.082531754730549078 ) ) ;
#149590 = CARTESIAN_POINT ( 'NONE',  ( -0.6801582343750213200, 1.348958333674710186, -1.178068619123886718 ) ) ;
#149591 = CARTESIAN_POINT ( 'NONE',  ( 4.553361389630797618, -1.314998166741452090, 1.528740011303417745 ) ) ;
#149592 = CARTESIAN_POINT ( 'NONE',  ( -3.701012746406287413, 6.301303389907177532, 1.082531754730560403 ) ) ;
#149593 = CARTESIAN_POINT ( 'NONE',  ( 9.908311333488716954, 10.45411806535867782, 0.7998128361456462443 ) ) ;
#149594 = CARTESIAN_POINT ( 'NONE',  ( 5.564695703766185275, 5.456842840674144490, 0.000000000000000000 ) ) ;
#149595 = CARTESIAN_POINT ( 'NONE',  ( 2.244514701088017539, 0.3993153960501935051, 1.781317584591130432 ) ) ;
#149596 = CARTESIAN_POINT ( 'NONE',  ( -1.225000000000044276, 1.791666667349484321, -0.7072540797573277915 ) ) ;
#149597 = VERTEX_POINT ( 'NONE', #11617 ) ;
#149598 = CARTESIAN_POINT ( 'NONE',  ( -5.763624699140882157, 7.817591130454727200, -1.443375672974066548 ) ) ;
#149599 = CARTESIAN_POINT ( 'NONE',  ( -2.656508033273816238, 5.186677574539687363, -1.199719254218446718 ) ) ;
#149601 = CARTESIAN_POINT ( 'NONE',  ( -7.296259222448620463, 11.66405285949874759, 0.7998128361456481317 ) ) ;
#149600 = B_SPLINE_CURVE_WITH_KNOTS ( 'NONE', 3,
 ( #57552, #89000, #138813, #122645 ),
 .UNSPECIFIED., .F., .F.,
 ( 4, 4 ),
 ( 0.0005671806269306093424, 0.0008743016172331036749 ),
 .UNSPECIFIED. ) ;
#149602 = CARTESIAN_POINT ( 'NONE',  ( 6.604167511870285168, -0.8622997358492515696, 1.824817093501039267 ) ) ;
#149604 = ORIENTED_EDGE ( 'NONE', *, *, #42311, .T. ) ;
#149603 = CARTESIAN_POINT ( 'NONE',  ( -0.02259406399240069044, -1.896172633340575064, -0.9493637518730788649 ) ) ;
#149605 = EDGE_LOOP ( 'NONE', ( #193715, #7601, #138857, #70561 ) ) ;
#149606 = CARTESIAN_POINT ( 'NONE',  ( -7.208094944320834863, 8.438474185576302133, -1.199719254218452047 ) ) ;
#149607 = CIRCLE ( 'NONE', #83878, 0.7500000000000011102 ) ;
#149608 = CARTESIAN_POINT ( 'NONE',  ( 4.171104814498611368, 8.018039383557042044, 0.7998128361456321445 ) ) ;
#149609 = CARTESIAN_POINT ( 'NONE',  ( 5.963760128287220574, 2.030816783491296906, -0.3497918165830601334 ) ) ;
#149610 = CARTESIAN_POINT ( 'NONE',  ( 5.537732479266092689, -1.587839044716709669, 1.242724925242834066 ) ) ;
#149611 = VERTEX_POINT ( 'NONE', #158954 ) ;
#149612 = ORIENTED_EDGE ( 'NONE', *, *, #80870, .T. ) ;
#149613 = CARTESIAN_POINT ( 'NONE',  ( 2.876381804795541619, 6.437993120328354024, 0.3511878651327338674 ) ) ;
#149614 = DIRECTION ( 'NONE',  ( 0.7592566023653005702, 0.6507913734559639396, 0.000000000000000000 ) ) ;
#149617 = ORIENTED_EDGE ( 'NONE', *, *, #196844, .F. ) ;
#149616 = DIRECTION ( 'NONE',  ( 0.000000000000000000, -1.000000000000000000, 0.000000000000000000 ) ) ;
#149615 = CARTESIAN_POINT ( 'NONE',  ( -6.631873415740034083, 7.766215735565355160, 1.199719254218452047 ) ) ;
#149618 = CARTESIAN_POINT ( 'NONE',  ( 4.831949485534527966, 8.212610664285437068, 0.9193987405316924599 ) ) ;
#149619 = CARTESIAN_POINT ( 'NONE',  ( 5.431017465639029318, 0.9912489969874547224, 1.755499476546865445 ) ) ;
#149620 = CARTESIAN_POINT ( 'NONE',  ( 4.786955173189685553, 1.366302399619228947, 1.234289508136581892 ) ) ;
#149621 = CYLINDRICAL_SURFACE ( 'NONE', #160648, 11.00000000000000000 ) ;
#149622 = CARTESIAN_POINT ( 'NONE',  ( 3.704037377190313673, -0.6708616879335957961, 2.208036538417802230 ) ) ;
#149623 = CARTESIAN_POINT ( 'NONE',  ( 8.018721507839716267, 8.319872945426633137, -0.7998128361456341429 ) ) ;
#149624 = CARTESIAN_POINT ( 'NONE',  ( 5.343121995983710626, -1.856993961526328007, 1.106124453333141577 ) ) ;
#149625 = CARTESIAN_POINT ( 'NONE',  ( 6.435316467980822353, 10.65961964595298817, 1.040834085586084257E-14 ) ) ;
#149626 = CARTESIAN_POINT ( 'NONE',  ( 0.4330194205178988232, -1.374205638499223614, -1.372529395279479703 ) ) ;
#149627 = CARTESIAN_POINT ( 'NONE',  ( -3.425406365747000859, 7.148057860013469877, 1.040834085586084257E-14 ) ) ;
#149628 = CARTESIAN_POINT ( 'NONE',  ( -9.367496997601234554, 15.46908218389367029, -7.499999999995462296 ) ) ;
#149629 = CARTESIAN_POINT ( 'NONE',  ( -3.969505113751027547, 7.853116076009993840, 1.214306433183764966E-14 ) ) ;
#149630 = AXIS2_PLACEMENT_3D ( 'NONE', #43431, #201873, #88162 ) ;
#149631 = CARTESIAN_POINT ( 'NONE',  ( 3.326877442632663939, 0.04465521416292458912, 1.870282673472216439 ) ) ;
#149632 = CIRCLE ( 'NONE', #204951, 0.08000000000000020983 ) ;
#149635 = CARTESIAN_POINT ( 'NONE',  ( -5.088052786878465739, 9.158088361325352977, 0.000000000000000000 ) ) ;
#149634 = CARTESIAN_POINT ( 'NONE',  ( -1.500000000000015099, -1.047916665983845919, 0.8660254037844403729 ) ) ;
#149633 = CARTESIAN_POINT ( 'NONE',  ( 0.8438408207818194340, -1.215224102361469161, -1.476598726422105656 ) ) ;
#149636 = CARTESIAN_POINT ( 'NONE',  ( 3.000804911251079510, -0.6410980074830170405, -2.111705341948390657 ) ) ;
#149637 = CARTESIAN_POINT ( 'NONE',  ( 3.903950209304066998, 8.999999999999998224, -0.7749999999999996891 ) ) ;
#149638 = CARTESIAN_POINT ( 'NONE',  ( 4.436542580169809291, 6.199052314996659874, 1.599625672291267398 ) ) ;
#149639 = CARTESIAN_POINT ( 'NONE',  ( 1.217526595471194906, 2.800000000000017586, -0.8761443883974120439 ) ) ;
#149640 = CARTESIAN_POINT ( 'NONE',  ( -3.972702704004144714, 4.593573561881607148, 1.199719254218462483 ) ) ;
#149641 = CARTESIAN_POINT ( 'NONE',  ( -6.739811759324828344, 8.956476034002674780, -1.443375672974066548 ) ) ;
#149642 = CARTESIAN_POINT ( 'NONE',  ( 0.8078137629249462215, -1.962250697097242869, 0.1890654564427676487 ) ) ;
#149643 = CARTESIAN_POINT ( 'NONE',  ( 0.1480895125635858234, -1.786911571543071675, -1.459641600669525197 ) ) ;
#149644 = CARTESIAN_POINT ( 'NONE',  ( 1.451531895509536874, 1.483362660712842063, 1.284035263222626844 ) ) ;
#149645 = CARTESIAN_POINT ( 'NONE',  ( 4.364169495198770399, -2.057374995403418172, 0.1468088122822813202 ) ) ;
#149646 = CARTESIAN_POINT ( 'NONE',  ( 4.202664430556241726, 7.846932902383524144, 0.7216878364870298324 ) ) ;
#149647 = ADVANCED_FACE ( 'NONE', ( #30021 ), #57010, .T. ) ;
#149648 = CARTESIAN_POINT ( 'NONE',  ( 7.042534447655770080, 7.180988041878682004, -0.7998128361456341429 ) ) ;
#149649 = EDGE_LOOP ( 'NONE', ( #113912, #114344, #54328, #105383 ) ) ;
#149650 = CARTESIAN_POINT ( 'NONE',  ( 6.588899466117086767, 10.63087377720454363, 1.040834085586084257E-14 ) ) ;
#149651 = CARTESIAN_POINT ( 'NONE',  ( 1.364683531249988535, 4.426041667008082214, 0.7879004041258500513 ) ) ;
#149652 = CARTESIAN_POINT ( 'NONE',  ( -10.91033749632887151, 4.885617943545217834, -4.996452313011736202 ) ) ;
#149653 = CARTESIAN_POINT ( 'NONE',  ( 2.670593071767634719, 6.059516317130127838, -0.7216878364870267237 ) ) ;
#149654 = CARTESIAN_POINT ( 'NONE',  ( 1.270657207514551246, -0.9741964446108697384, -1.940257991389877201 ) ) ;
#149656 = CARTESIAN_POINT ( 'NONE',  ( 5.759284750224211713, 1.812880138157666465, -0.3211251414683007899 ) ) ;
#149655 = CARTESIAN_POINT ( 'NONE',  ( 9.493819324367764878, -9.279866070759380747, -0.3645580569637754120 ) ) ;
#149657 = CARTESIAN_POINT ( 'NONE',  ( 5.620091457764528897, 6.146229702208615642, -0.8320832460304794509 ) ) ;
#149659 = CARTESIAN_POINT ( 'NONE',  ( -11.86239285000045918, 12.29999999999999716, -1.812080536912752837 ) ) ;
#149658 = B_SPLINE_CURVE_WITH_KNOTS ( 'NONE', 3,
 ( #180624, #85257, #80996, #164383, #66836, #130881, #148144, #67909, #184880, #35436 ),
 .UNSPECIFIED., .F., .F.,
 ( 4, 2, 2, 2, 4 ),
 ( 0.000000000000000000, 0.0002598598948551708457, 0.0005197197897103416914, 0.0007795796845655125372, 0.001039439579420683383 ),
 .UNSPECIFIED. ) ;
#149660 = CARTESIAN_POINT ( 'NONE',  ( 1.124039026005444475, 1.118881483734196935, -1.498852260102357725 ) ) ;
#149662 = CARTESIAN_POINT ( 'NONE',  ( -5.891600325674557048, 6.152103933748189313, 0.8728944348482190474 ) ) ;
#149661 = AXIS2_PLACEMENT_3D ( 'NONE', #44816, #43747, #127199 ) ;
#149663 = CARTESIAN_POINT ( 'NONE',  ( 0.07735805125223899070, 0.2300150639059690694, -2.122327182112139443 ) ) ;
#149664 = CARTESIAN_POINT ( 'NONE',  ( 5.662876554447811017, 7.443216037249618999, -1.326882488215734845 ) ) ;
#149665 = CARTESIAN_POINT ( 'NONE',  ( -0.6823417656250212460, 5.613541667008087543, 1.181850606188767472 ) ) ;
#149666 = CARTESIAN_POINT ( 'NONE',  ( 0.7328884408557727603, 1.767063509844998492, 0.7314339715377634610 ) ) ;
#149667 = CARTESIAN_POINT ( 'NONE',  ( 2.482954129442132452, 1.619277697627572676, -0.7147633530761726695 ) ) ;
#149668 = CARTESIAN_POINT ( 'NONE',  ( 0.6625817696367036769, 0.5554855734208345996, 1.829800363923417716 ) ) ;
#149670 = CARTESIAN_POINT ( 'NONE',  ( 4.499565103457034532, -1.877818951341524878, 0.3776799693050793549 ) ) ;
#149669 = CARTESIAN_POINT ( 'NONE',  ( 2.655622817947407732, -3.216694470489968705, 1.969572979196722473 ) ) ;
#149671 = CARTESIAN_POINT ( 'NONE',  ( 0.7499999999999867883, -0.9333333333333138082, -1.299038105676652011 ) ) ;
#149672 = CARTESIAN_POINT ( 'NONE',  ( 5.459413677600381654, 1.609035625656387802, 1.135536449648701041 ) ) ;
#149673 = CARTESIAN_POINT ( 'NONE',  ( 1.424255164902767934, -2.103954720533041556, 0.2648648325892372646 ) ) ;
#149674 = CARTESIAN_POINT ( 'NONE',  ( -5.249999999999987566, 0.000000000000000000, 1.599999999999997202 ) ) ;
#149675 = CARTESIAN_POINT ( 'NONE',  ( 3.467518583331068438, 1.825290416974333807, -0.4087457676540603990 ) ) ;
#149677 = ORIENTED_EDGE ( 'NONE', *, *, #92035, .F. ) ;
#149676 = CARTESIAN_POINT ( 'NONE',  ( 0.2404813148422607627, 0.3085585699703840556, 1.799268721412583316 ) ) ;
#149679 = CARTESIAN_POINT ( 'NONE',  ( -4.123088111887291518, 7.824370207261548416, 0.000000000000000000 ) ) ;
#149678 = CARTESIAN_POINT ( 'NONE',  ( 3.862124860921032354, 2.190326239153097543, -0.2693113811002012525 ) ) ;
#149680 = CARTESIAN_POINT ( 'NONE',  ( 0.6823417656249917140, 4.655208333674755394, 1.181850606188765695 ) ) ;
#149681 = CARTESIAN_POINT ( 'NONE',  ( 2.049356628244120682, 1.795697342706262578, -1.014786283375568976 ) ) ;
#149682 = CARTESIAN_POINT ( 'NONE',  ( 4.476163270806094552, 8.373940915915776273, 0.7998128361456462443 ) ) ;
#149683 = CARTESIAN_POINT ( 'NONE',  ( -9.677822722056413696, 10.18521468535430685, 1.040834085586084257E-14 ) ) ;
#149684 = CARTESIAN_POINT ( 'NONE',  ( 3.719872605471109761, 6.605953636083950364, -2.420000000000002149 ) ) ;
#149685 = DIRECTION ( 'NONE',  ( 0.000000000000000000, 0.000000000000000000, 1.000000000000000000 ) ) ;
#149686 = CARTESIAN_POINT ( 'NONE',  ( -1.499999999999946709, 7.750000000000000000, 15.75000000000000711 ) ) ;
#149687 = ORIENTED_EDGE ( 'NONE', *, *, #62182, .T. ) ;
#149688 = CARTESIAN_POINT ( 'NONE',  ( 4.703616579153604427, -1.598285800263723910, -1.315984976451072930 ) ) ;
#149689 = CARTESIAN_POINT ( 'NONE',  ( -0.6823417656250003738, -0.7197916663252492686, -1.181850606188749264 ) ) ;
#149690 = CARTESIAN_POINT ( 'NONE',  ( 1.897963814661303150, -0.7301937759345775714, 2.034636513274298064 ) ) ;
#149691 = CARTESIAN_POINT ( 'NONE',  ( -5.872679487624441030, 7.188158700483015195, -1.149102218512105145 ) ) ;
#149692 = CARTESIAN_POINT ( 'NONE',  ( 1.576825605243727502, -1.426663165427190405, 1.429853764617691647 ) ) ;
#149693 = DIRECTION ( 'NONE',  ( 0.000000000000000000, 0.000000000000000000, 1.000000000000000000 ) ) ;
#149694 = EDGE_CURVE ( 'NONE', #133393, #56668, #121710, .T. ) ;
#149695 = VERTEX_POINT ( 'NONE', #209509 ) ;
#149697 = CARTESIAN_POINT ( 'NONE',  ( 8.107412671292035355, 10.48173408797264194, 1.443375672974076540 ) ) ;
#149696 = CARTESIAN_POINT ( 'NONE',  ( 3.475000000000000533, -3.354166666666667851, 2.006292185433948827 ) ) ;
#149698 = CARTESIAN_POINT ( 'NONE',  ( 6.485703859413265882, 1.880147802650249611, 0.7282652505391642439 ) ) ;
#149699 = CARTESIAN_POINT ( 'NONE',  ( 0.3215004009857677092, -1.429452135790244549, -1.422604240635255479 ) ) ;
#149700 = CARTESIAN_POINT ( 'NONE',  ( 6.639320575229258559, 7.052241914652472410, 2.701414248926166994 ) ) ;
#149701 = CARTESIAN_POINT ( 'NONE',  ( 4.985950990042907094, -2.174969566330759996, -0.2684501861200879747 ) ) ;
#149702 = CARTESIAN_POINT ( 'NONE',  ( -1.499999999999997780, 3.431250000682818602, 1.214306433183764966E-14 ) ) ;
#149703 = CARTESIAN_POINT ( 'NONE',  ( 3.990413957267644474, -1.096855775730350757, 1.566394476586838502 ) ) ;
#149704 = CARTESIAN_POINT ( 'NONE',  ( -5.739179097286464248, 5.590130456455974617, -0.7998128361456221525 ) ) ;
#149705 = EDGE_CURVE ( 'NONE', #23400, #121694, #49116, .T. ) ;
#149706 = CARTESIAN_POINT ( 'NONE',  ( 4.839897649954202130, 4.748894801142428790, -0.7216878364870197293 ) ) ;
#149708 = CARTESIAN_POINT ( 'NONE',  ( 2.372672929649359386, -0.3474902101525711440, -1.986097784353996643 ) ) ;
#149707 = FACE_OUTER_BOUND ( 'NONE', #116280, .T. ) ;
#149709 = CARTESIAN_POINT ( 'NONE',  ( -0.6823417656250039265, 11.88020833367473017, -1.181850606188755259 ) ) ;
#149711 = CARTESIAN_POINT ( 'NONE',  ( -4.736594563127865420, 6.619389305106191834, -1.599625672291271394 ) ) ;
#149710 = CARTESIAN_POINT ( 'NONE',  ( 0.2051334325893399424, 1.998568519175287328, 1.122693669494337909 ) ) ;
#149712 = CARTESIAN_POINT ( 'NONE',  ( 4.295721138614797319, -0.6590762262537721572, 1.594082981517078945 ) ) ;
#149713 = CARTESIAN_POINT ( 'NONE',  ( 0.1399997263886038068, 6.947785072119228467, -2.594798351071639253 ) ) ;
#149714 = CARTESIAN_POINT ( 'NONE',  ( 4.684505768721569652, 5.424010470718658716, -1.199719254218452047 ) ) ;
#149715 = CARTESIAN_POINT ( 'NONE',  ( -11.41176686791169104, 12.34049196513146107, -3.404018756831829418 ) ) ;
#149716 = CARTESIAN_POINT ( 'NONE',  ( 1.504273306027693602, 1.959471947749168663, 0.09963418240711149898 ) ) ;
#149717 = FACE_OUTER_BOUND ( 'NONE', #213623, .T. ) ;
#149718 = CARTESIAN_POINT ( 'NONE',  ( 3.845709127770629010, 7.638411082374393146, 0.7998128361456321445 ) ) ;
#149719 = CARTESIAN_POINT ( 'NONE',  ( 0.1753634416057497647, 0.0001173177735149660568, -2.144164757042036573 ) ) ;
#149720 = ORIENTED_EDGE ( 'NONE', *, *, #143030, .F. ) ;
#149722 = STYLED_ITEM ( 'NONE', ( #58430 ), #65706 ) ;
#149721 = CARTESIAN_POINT ( 'NONE',  ( 0.3036855567021545244, -1.598042064648269811, -1.315789336611736138 ) ) ;
#149723 = EDGE_LOOP ( 'NONE', ( #3160, #34775, #156820, #76278 ) ) ;
#149724 = CARTESIAN_POINT ( 'NONE',  ( 3.967288593341521175, -1.508176260789632739, -1.003069782103764185 ) ) ;
#149725 = EDGE_LOOP ( 'NONE', ( #139997, #163207, #39722, #146052 ) ) ;
#149726 = CARTESIAN_POINT ( 'NONE',  ( 7.354371980770088690, 7.544798497178720531, 0.000000000000000000 ) ) ;
#149727 = CARTESIAN_POINT ( 'NONE',  ( 9.579603127937247109, 7.849261790823902629, -0.08720040834114990702 ) ) ;
#149728 = CARTESIAN_POINT ( 'NONE',  ( 4.705596528438695358, 1.345619282010660500, 1.212945642518966416 ) ) ;
#149729 = CARTESIAN_POINT ( 'NONE',  ( 7.038091138825468107, 8.344099429118761790, -1.082531754730548412 ) ) ;
#149730 = CARTESIAN_POINT ( 'NONE',  ( -1.420000000000001039, 2.244000000000016648, -2.508000000000002228 ) ) ;
#149731 = CARTESIAN_POINT ( 'NONE',  ( 5.373129273518238769, 6.310201232541126970, -1.074510414011679016 ) ) ;
#149733 = CARTESIAN_POINT ( 'NONE',  ( 8.380911511541880188, 12.92948053010758258, 0.7998128361456462443 ) ) ;
#149732 = CARTESIAN_POINT ( 'NONE',  ( 6.057066403244290242, 1.520950583283819935, -1.072200347198979831 ) ) ;
#149734 = CARTESIAN_POINT ( 'NONE',  ( 3.849167162397474140, 0.2308054593076276639, -1.901561516516042660 ) ) ;
#149735 = CARTESIAN_POINT ( 'NONE',  ( -6.764644832400126262, -7.632775601084264672, -6.764644832402675334 ) ) ;
#149736 = CARTESIAN_POINT ( 'NONE',  ( -11.36822525729066413, 5.406166865499119289, 5.610767994321700591 ) ) ;
#149738 = EDGE_CURVE ( 'NONE', #79131, #49812, #28659, .T. ) ;
#149737 = SHAPE_REPRESENTATION ( 'coil', ( #200407 ), #124915 ) ;
#149739 = CARTESIAN_POINT ( 'NONE',  ( 9.499610831742323569, -9.904389604292740401, -0.08598863555141049442 ) ) ;
#149740 = CARTESIAN_POINT ( 'NONE',  ( 0.6823417656249882723, -0.9072916663252494907, 1.181850606188755259 ) ) ;
#149741 = CARTESIAN_POINT ( 'NONE',  ( 7.293923454472091450, 7.611924906413328529, 0.7216878364870317197 ) ) ;
#149742 = B_SPLINE_CURVE_WITH_KNOTS ( 'NONE', 3,
 ( #142800, #61505, #178468, #208805, #94037, #193632, #91907, #59373, #95099, #160076, #11678, #143874, #209867, #207747, #127671, #26865, #10608, #78808, #191489, #157964, #92969, #159014, #161147, #77753, #60434, #43158, #126594, #25798, #192555, #111395, #144932, #45274, #109270, #112456, #190427, #175278, #44210, #176335, #110332, #177399, #194699, #12734, #27942, #210938, #46341, #108199, #96169, #174223, #162220, #13807, #79878, #145989, #2868, #132931, #131879, #34323, #150232, #32204, #14864, #18059, #33262, #1803, #181633, #129796, #195775, #182704, #84146, #51666, #148100, #213067, #15927, #50582, #151297, #47414, #99345, #100397, #65732, #196834, #149146, #117789, #85211, #113528, #130841, #116704, #67860, #180583, #726, #183778, #197888, #98280, #165394, #82010, #66792, #35389, #214103, #16990, #198937, #31154, #64696, #166466, #83068, #200015, #49517, #134009, #164339, #167536, #115637, #101465, #19134, #147044, #179535, #97227, #163280, #80953, #48475, #114592, #70002, #37533, #168597, #156639, #172891, #203211, #89511, #73219, #68938, #20197, #86286, #139325, #152357, #71072, #137189, #6076, #54857, #53792, #122079, #103610, #105781, #22320, #136116, #201072, #3932, #189123, #202131, #188041, #135060, #102535, #90579, #7147, #52714, #38607, #88433, #106864, #39670, #87358, #205356, #72146, #171806, #154497, #121008, #138256, #24466, #204268, #56990, #153426, #186975, #55921, #184829, #119923, #23398, #104685, #170734, #155565, #123163, #185898, #40758, #169666, #21251, #118847, #4995, #36459, #125276, #191238, #61257, #127415, #210697, #94846, #126342, #207497, #209615, #8231, #142543, #28762, #12493, #74314, #173972, #107946, #78566, #25546, #10358, #76435, #159822, #208549, #190180, #206429, #11425, #77501, #110077, #58053, #41835, #62327, #128486, #91654, #193387, #140411, #157707, #29837, #160897, #95921, #192302, #143620, #45031, #42901, #111145, #177145, #176089, #9304, #144686, #124218, #75377, #26616, #60183, #43961, #194452, #46097, #27687, #141491, #112213, #59119, #93786, #178222, #109010, #175029, #92717, #158763, #161975, #35133, #165152, #164101, #66544, #182451, #64459, #47169, #50338, #65492, #148904, #34079, #213869, #13565, #79637, #478, #116458, #195530, #131639, #63394, #15684, #199765, #82828, #96988, #196592, #98048, #197642, #145756, #67611, #129548, #16743, #51410, #117530, #81771, #132687, #211756, #48234, #113283, #166212, #179289, #147851, #49287, #99099, #115405, #146805, #198694, #130603, #100148, #181398, #163039, #30913, #14619, #80715, #212823, #114347, #180344, #31965, #183524, #17804, #33022, #83888, #149979, #1550, #133756, #119663, #53529, #170473, #118592, #185649, #137997, #37280, #169415, #200816, #104426, #22059, #20999, #4740, #188862, #55661, #102275, #70815, #87096, #101205, #153166, #103351, #168353, #136930, #6887, #19945, #152106, #202958, #135859, #154240, #54600, #120748, #39416, #204015, #187787, #186722, #167291, #18878, #5812, #121819, #23136, #38349, #184581, #201880, #88170, #122904, #84962, #71888, #105510, #171543, #86032, #89253, #155305, #56736, #139070, #72965, #205095, #151051, #2618, #68689, #134811, #52467, #36200, #3676, #69755, #125023, #26354, #176891, #107688, #190981, #74055, #92470, #142288, #106604, #208299, #59930, #140147, #126085, #91393, #75123 ),
 .UNSPECIFIED., .F., .F.,
 ( 4, 1, 1, 1, 1, 1, 1, 1, 1, 1, 1, 1, 1, 1, 1, 1, 1, 1, 1, 1, 1, 1, 1, 1, 1, 1, 1, 1, 1, 1, 1, 1, 1, 1, 1, 1, 1, 1, 1, 1, 1, 1, 1, 1, 1, 1, 1, 1, 1, 1, 1, 1, 1, 1, 1, 1, 1, 1, 1, 1, 1, 1, 1, 1, 1, 1, 1, 1, 1, 1, 1, 1, 1, 1, 1, 1, 1, 1, 1, 1, 1, 1, 1, 1, 1, 1, 1, 1, 1, 1, 1, 1, 1, 1, 1, 1, 1, 1, 1, 1, 1, 1, 1, 1, 1, 1, 1, 1, 1, 1, 1, 1, 1, 1, 1, 1, 1, 1, 1, 1, 1, 1, 1, 1, 1, 1, 1, 1, 1, 1, 1, 1, 1, 1, 1, 1, 1, 1, 1, 1, 1, 1, 1, 1, 1, 1, 1, 1, 1, 1, 1, 1, 1, 1, 1, 1, 1, 1, 1, 1, 1, 1, 1, 1, 1, 1, 1, 1, 1, 1, 1, 1, 1, 1, 1, 1, 1, 1, 1, 1, 1, 1, 1, 1, 1, 1, 1, 1, 1, 1, 1, 1, 1, 1, 1, 1, 1, 1, 1, 1, 1, 1, 1, 1, 1, 1, 1, 1, 1, 1, 1, 1, 1, 1, 1, 1, 1, 1, 1, 1, 1, 1, 1, 1, 1, 1, 1, 1, 1, 1, 1, 1, 1, 1, 1, 1, 1, 1, 1, 1, 1, 1, 1, 1, 1, 1, 1, 1, 1, 1, 1, 1, 1, 1, 1, 1, 1, 1, 1, 1, 1, 1, 1, 1, 1, 1, 1, 1, 1, 1, 1, 1, 1, 1, 1, 1, 1, 1, 1, 1, 1, 1, 1, 1, 1, 1, 1, 1, 1, 1, 1, 1, 1, 1, 1, 1, 1, 1, 1, 1, 1, 1, 1, 1, 1, 1, 1, 1, 1, 1, 1, 1, 1, 1, 1, 1, 1, 1, 1, 1, 1, 1, 1, 1, 1, 1, 1, 1, 1, 1, 1, 1, 1, 1, 1, 1, 1, 1, 1, 1, 1, 1, 1, 1, 1, 1, 1, 1, 1, 1, 1, 1, 1, 1, 1, 1, 1, 1, 1, 1, 1, 1, 1, 1, 1, 1, 1, 1, 1, 1, 1, 1, 1, 1, 1, 1, 1, 1, 1, 1, 1, 1, 1, 1, 4 ),
 ( 0.000000000000000000, 0.002600034503794030130, 0.005208798665460326327, 0.007813183304800875098, 0.01041632952039499814, 0.01302078637366306003, 0.01562487905948694092, 0.01822913957756216313, 0.02083328395591756144, 0.02343739818322774712, 0.02604168118785421884, 0.02864568517727394958, 0.03125004130332968699, 0.03385401862675675722, 0.03645834363201481965, 0.03906241290072134942, 0.04166661303991354287, 0.04427083116291704451, 0.04687488238457573897, 0.04947921467585455341, 0.05208318889621989245, 0.05468754274347345512, 0.05729155431138267807, 0.05989582568988525285, 0.06249996760622017478, 0.06510408932096034551, 0.06770837349117478365, 0.07031237295078232585, 0.07291672927807971161, 0.07552070761765239393, 0.07812503204114096267, 0.08072910085791458468, 0.08333330089851145872, 0.08593751883178461781, 0.08854156980611090078, 0.09114590188302622298, 0.09374987588873062716, 0.09635422952249227124, 0.09895824087764454324, 0.1015625120427016276, 0.1041666537503683765, 0.1067707752516706410, 0.1093750592157429480, 0.1119790584643299974, 0.1145834145867499904, 0.1171873927198607973, 0.1197917169388799108, 0.1223957855539345302, 0.1249999853896588409, 0.1276042031245507580, 0.1302082538950744550, 0.1328125857752754935, 0.1354165595809520839, 0.1380209130188291833, 0.1406249241787864424, 0.1432291951479887082, 0.1458333366646657747, 0.1484374579699756502, 0.1510417417453218114, 0.1536457408005802994, 0.1562500967354857329, 0.1588540746797905134, 0.1614583987117299280, 0.1640624671426803571, 0.1666666667910262079, 0.1692708843450304312, 0.1718749349293641482, 0.1744792666302357464, 0.1770832402535473249, 0.1796875935129024493, 0.1822916044953091785, 0.1848958752860835608, 0.1875000166293293857, 0.1901041377562054102, 0.1927084213602507368, 0.1953124202398235920, 0.1979167760045740521, 0.2005207537777317084, 0.2031250776399721736, 0.2057291459044250093, 0.2083333453828807025, 0.2109375627734847158, 0.2135416131892344249, 0.2161459447281551538, 0.2187499181867580689, 0.2213542712849473904, 0.2239582821074418695, 0.2265625527372090720, 0.2291666939245756707, 0.2317708148905701926, 0.2343750983407339450, 0.2369790970622578097, 0.2395834526742069426, 0.2421874302938704648, 0.2447917540037867212, 0.2473958221193426621, 0.2500000214453905190, 0.2526042386900758108, 0.2552082889548416555, 0.2578126203491843960, 0.2604165936607292231, 0.2630209466151033904, 0.2656249572953180982, 0.2682292277814931625, 0.2708333688305272213, 0.2734374896531870935, 0.2760417729668830367, 0.2786457715479891406, 0.2812501270244852081, 0.2838541045083020076, 0.2864584280832634389, 0.2890624960675178268, 0.2916666952586349781, 0.2942709123748779576, 0.2968749625062547248, 0.2994792937733871119, 0.3020832669555192918, 0.3046876197834237909, 0.3072916303389863768, 0.3098959006989794318, 0.3125000416272227799, 0.3151041623240899980, 0.3177084455187270673, 0.3203124439770417831, 0.3229167993354283839, 0.3255207767010412923, 0.3281251001584127303, 0.3307291680289564662, 0.3333333671026155187, 0.3359375841078879321, 0.3385416341234662174, 0.3411459652807516951, 0.3437499383511121720, 0.3463542910698884647, 0.3489583015184220538, 0.3515625717696388985, 0.3541667125946290073, 0.3567708331832410984, 0.3593751162762241491, 0.3619791146293697692, 0.3645834698869864221, 0.3671874471520340522, 0.3697917705091763874, 0.3723958382835964032, 0.3750000372572658280, 0.3776042541690359799, 0.3802083040864021046, 0.3828126351512001757, 0.3854166081274262856, 0.3880209607544118922, 0.3906249711135359459, 0.3932292412733790488, 0.3958333820126498370, 0.3984375025105409418, 0.4010417855192715542, 0.4036457837848667074, 0.4062501389590495449, 0.4088541161411674008, 0.4114584394154381930, 0.4140625071113177014, 0.4166667060024629166, 0.4192709228381954478, 0.4218749726749327911, 0.4244793036646000717, 0.4270832765643259310, 0.4296876291168554296, 0.4322916394041865784, 0.4348959094900549660, 0.4375000501611374104, 0.4401041705858387276, 0.4427084535277153732, 0.4453124517233759683, 0.4479168068314584583, 0.4505207839482789911, 0.4531251071570330247, 0.4557291747919532399, 0.4583333736180368323, 0.4609375903951940523, 0.4635416401688834398, 0.4661459711007739370, 0.4687499439416310532, 0.4713542964370365795, 0.4739583066701890113, 0.4765625766994796009, 0.4791667173199026797, 0.4817708376889431876, 0.4843751205813623395, 0.4869791187247021202, 0.4895834737840155659, 0.4921874508531692838, 0.4947917740137594000, 0.4973958416052992049, 0.5000000403837819851, 0.5026042571198243714, 0.5052083068480445194, 0.5078126377395105751, 0.5104166105391289010, 0.5130209629947408700, 0.5156249731913270518, 0.5182292431814352618, 0.5208333837687260104, 0.5234375040996330775, 0.5260417869599895990, 0.5286457850686206994, 0.5312501400964950715, 0.5338541171356111503, 0.5364584402653888029, 0.5390625078311259699, 0.5416667065794673608, 0.5442709232918542250, 0.5468749729921829061, 0.5494793038605755298, 0.5520832766365837418, 0.5546876290697317913, 0.5572916392473630243, 0.5598959092156829964, 0.5625000497873680061, 0.5651041700976676685, 0.5677084529433557014, 0.5703124510348895893, 0.5729168060486536929, 0.5755207830753605869, 0.5781251061916765632, 0.5807291737491879768, 0.5833333724848467350, 0.5859375891910368894, 0.5885416388810509325, 0.5911459697437208005, 0.5937499425137473530, 0.5963542949417601768, 0.5989583051180477069, 0.6015625750819736384, 0.6041667156555785567, 0.6067708359627971282, 0.6093751188112106476, 0.6119791169032582356, 0.6145834719202413199, 0.6171874489521673723, 0.6197917720723722379, 0.6223958396392350600, 0.6250000383796699976, 0.6276042550971219214, 0.6302083047943985994, 0.6328126356686964993, 0.6354166084503697354, 0.6380209608905765828, 0.6406249710831318778, 0.6432292410600577437, 0.6458333816531092175, 0.6484375019747732338, 0.6510417848433065480, 0.6536457829534795261, 0.6562501379910111732, 0.6588541150457848383, 0.6614584381872300467, 0.6640625057810221055, 0.6666667045436925898, 0.6692709212898660942, 0.6718749710119833463, 0.6744793019152608426, 0.6770832747262099938, 0.6796876271959411131, 0.6822916374223763070, 0.6848959074296973037, 0.6875000480597228680, 0.6901041684133596421, 0.6927084513194080584, 0.6953124494653194487, 0.6979168045407300180, 0.7005207816359816375, 0.7031251048160196415, 0.7057291724543196532, 0.7083333712566866058, 0.7109375880490425015, 0.7135416378135795989, 0.7161459687631898108, 0.7187499416210458847, 0.7213542941376326345, 0.7239583044155618596, 0.7265625744706748490, 0.7291667151552034820, 0.7317708355583423252, 0.7343751185193033715, 0.7369791167185673064, 0.7395834718491895998, 0.7421874490025512916, 0.7447917722385364314, 0.7473958399389256657, 0.7500000387984516736, 0.7526042556544531026, 0.7552083054789914263, 0.7578126364922896929, 0.7604166094146853627, 0.7630209619954617661, 0.7656249723425013753, 0.7682292424628052174, 0.7708333832193684509, 0.7734375036895410060, 0.7760417867228139865, 0.7786457849930478181, 0.7812501401962168579, 0.7838541174253229604, 0.7864584407346123518, 0.7890625085146746320, 0.7916667074488250577, 0.7942709243859374935, 0.7968749742880611997, 0.7994793053824050810, 0.8020832783869765725, 0.8046876310492792062, 0.8072916414830481058, 0.8098959116859448804, 0.8125000525320774658, 0.8151041730868179291, 0.8177084562098055898, 0.8203124545686294455, 0.8229168098616829186, 0.8255207871841712119, 0.8281251105841250792, 0.8307291784614470043, 0.8333333774876906519, 0.8359375945233833427, 0.8385416445206798075, 0.8411459757134309712, 0.8437499488178175078, 0.8463543015789862789, 0.8489583121171074831, 0.8515625824200027116, 0.8541667233732427311, 0.8567708440300897399, 0.8593751272601987123, 0.8619791257252362726, 0.8645834811255164176, 0.8671874585590289009, 0.8697917820670107991, 0.8723958500591838527, 0.8750000491949933012, 0.8776042663467393812, 0.8802083164568000884, 0.8828126477653241988, 0.8854166209871692228, 0.8880209738645485906, 0.8906249845246493324, 0.8932292549449527552, 0.8958333960228427317, 0.8984375167993386979, 0.9010418001539796107, 0.9036457987428592187, 0.9062501542677121602, 0.9088541318298947180, 0.9114584554632734203, 0.9140625235878931942, 0.9166667228507454634, 0.9192709401360219523, 0.9218749903764450471, 0.9244793218181143191, 0.9270832951750564987, 0.9296876481859919217, 0.9322916589857459524, 0.9348959295408556525, 0.9375000707608250883, 0.9401041916746273319, 0.9427084751713679101, 0.9453124739016935951, 0.9479168295687272483, 0.9505208072738278169, 0.9531251310501845930, 0.9557291993520028450, 0.9583333987332913750, 0.9609376160454207172, 0.9635416666839513589, 0.9661459986354887786, 0.9687499708159389433, 0.9713543235632202677, 0.9739583390673558494, 0.9765626083347638264, 0.9791667417950460361, 0.9817708662416058107, 0.9843751381318576188, 0.9869792129215403387, 0.9895836736503123010, 0.9921868305638316121, 0.9947912020913856068, 0.9973999845648282569, 1.000000000000000000 ),
 .UNSPECIFIED. ) ;
#149744 = CARTESIAN_POINT ( 'NONE',  ( 5.876184115051023227, -2.107333617329323783, -0.2052446207758129582 ) ) ;
#149743 = CARTESIAN_POINT ( 'NONE',  ( -10.30383355670593737, 11.12348669235284504, -0.7216878364870267237 ) ) ;
#149745 = CARTESIAN_POINT ( 'NONE',  ( 0.6554165194554737450, -1.826866057147133349, -1.155366728873077564 ) ) ;
#149746 = CARTESIAN_POINT ( 'NONE',  ( -4.586401103172829785, 8.572828063668767484, 0.7998128361456281477 ) ) ;
#149747 = CARTESIAN_POINT ( 'NONE',  ( 4.692003678781083487, 7.631698837623355658, -1.199719254218450271 ) ) ;
#149748 = CARTESIAN_POINT ( 'NONE',  ( 0.8854529848611718545, 1.222500307375608886, 1.355994775097228766 ) ) ;
#149749 = CARTESIAN_POINT ( 'NONE',  ( -4.090809663021341969, 5.795697244990093644, 1.599625672291267398 ) ) ;
#149750 = CARTESIAN_POINT ( 'NONE',  ( 3.909063277197013520, 1.565549990038747952, 0.9388121169797561949 ) ) ;
#149751 = CARTESIAN_POINT ( 'NONE',  ( 12.00693267275518572, 8.237831693621128437, -3.583085096157309302 ) ) ;
#149752 = CARTESIAN_POINT ( 'NONE',  ( 1.793074957647671663, -0.09724762972821224261, -1.910064080951429100 ) ) ;
#149753 = ORIENTED_EDGE ( 'NONE', *, *, #190504, .F. ) ;
#149754 = CARTESIAN_POINT ( 'NONE',  ( 3.086336304319175383, 1.096367280595906601, -1.635968976963786847 ) ) ;
#149755 = CARTESIAN_POINT ( 'NONE',  ( 4.335450565170337001, 0.8274041267214229389, -1.757107282799404091 ) ) ;
#149756 = CARTESIAN_POINT ( 'NONE',  ( -6.454563648557663846, 9.688018802362710957, -1.199719254218452047 ) ) ;
#149758 = CARTESIAN_POINT ( 'NONE',  ( 4.676102344489991403, 2.097148071331572439, -0.3138259731317455392 ) ) ;
#149757 = CARTESIAN_POINT ( 'NONE',  ( 5.657495238652423097, 9.822437888394988548, 0.000000000000000000 ) ) ;
#149759 = CARTESIAN_POINT ( 'NONE',  ( -6.966220764712169000, 6.002124920821316323, -2.500000000000000444 ) ) ;
#149760 = CARTESIAN_POINT ( 'NONE',  ( 3.000541214264150547, -1.884352459892328024, -0.3246530749497905655 ) ) ;
#149761 = CARTESIAN_POINT ( 'NONE',  ( 6.058883744127357751, 6.050764970021646150, 0.4299300578466564993 ) ) ;
#149762 = CARTESIAN_POINT ( 'NONE',  ( -1.249999999999964695, 8.500000000000000000, 10.97907099895069294 ) ) ;
#149763 = LINE ( 'NONE', #1340, #125833 ) ;
#149764 = CARTESIAN_POINT ( 'NONE',  ( 4.903208829997618423, 5.749440385532527564, -1.199719254218450271 ) ) ;
#149765 = COLOUR_RGB ( '', 0.09019608, 0.27058824, 0.51372549) ;
#149766 = DIRECTION ( 'NONE',  ( 0.000000000000000000, -1.000000000000000000, -1.804652791718263484E-16 ) ) ;
#149768 = CARTESIAN_POINT ( 'NONE',  ( 6.175017591530616023, 1.752142144017948100, -0.9981200475188132248 ) ) ;
#149767 = CARTESIAN_POINT ( 'NONE',  ( 4.494645072041675071, -0.4025399330690944133, -1.780595394402582077 ) ) ;
#149769 = CARTESIAN_POINT ( 'NONE',  ( -1.886825320689270225, 2.480000000000016858, -2.459652456995881753 ) ) ;
#149770 = CARTESIAN_POINT ( 'NONE',  ( -7.863365906246048809, 12.11775129068834289, -0.7216878364870267237 ) ) ;
#149771 = CARTESIAN_POINT ( 'NONE',  ( -5.823544721894389653, 7.314923355733134791, 1.295626528688619272 ) ) ;
#149772 = CARTESIAN_POINT ( 'NONE',  ( 11.44789321844504215, 11.29999999999999716, -3.303298730975399167 ) ) ;
#149773 = CARTESIAN_POINT ( 'NONE',  ( 6.034044788248046132, 0.9204803733943857091, -1.628451883209979689 ) ) ;
#149774 = CARTESIAN_POINT ( 'NONE',  ( 8.450809820019639318, 8.753699632978056755, -0.7998128361456291469 ) ) ;
#149775 = CARTESIAN_POINT ( 'NONE',  ( -5.935772324684618795, 5.819489221753827657, 0.000000000000000000 ) ) ;
#149776 = CARTESIAN_POINT ( 'NONE',  ( 3.842846474469570062, 6.570739089268092137, -1.199719254218452047 ) ) ;
#149777 = CARTESIAN_POINT ( 'NONE',  ( -1.364683531250014514, 9.901041667008064096, -0.7879004041258335089 ) ) ;
#149778 = CARTESIAN_POINT ( 'NONE',  ( -4.577849422908604637, 8.492574760035358494, -0.7998128361456281477 ) ) ;
#149779 = CARTESIAN_POINT ( 'NONE',  ( 4.356247428692526569, 3.976710176429713250, 0.7998128361456341429 ) ) ;
#149780 = CARTESIAN_POINT ( 'NONE',  ( -5.921879234118920365, 10.13088588310589699, 0.000000000000000000 ) ) ;
#149781 = CARTESIAN_POINT ( 'NONE',  ( -5.229694566569281555, 7.124396299129368337, 1.599625672291267398 ) ) ;
#149782 =( GEOMETRIC_REPRESENTATION_CONTEXT ( 3 ) GLOBAL_UNCERTAINTY_ASSIGNED_CONTEXT ( ( #131282 ) ) GLOBAL_UNIT_ASSIGNED_CONTEXT ( ( #177501, #127778, #147143 ) ) REPRESENTATION_CONTEXT ( 'NONE', 'WORKASPACE' ) );
#149783 = CARTESIAN_POINT ( 'NONE',  ( 0.2392000317489213768, -0.1454578200970526591, -2.037356452166842580 ) ) ;
#149784 = CARTESIAN_POINT ( 'NONE',  ( 1.124788838837559535, 0.4171406989393853793, 2.075574515046583191 ) ) ;
#149785 = CARTESIAN_POINT ( 'NONE',  ( 7.781490099239519509, 11.16582331816642260, 1.199719254218460707 ) ) ;
#149786 = CARTESIAN_POINT ( 'NONE',  ( -2.281615103654124344, 2.664038801896170483, 2.456549816139032227 ) ) ;
#149787 = CARTESIAN_POINT ( 'NONE',  ( 5.735237735067806319, -0.04509738862551111033, -2.069921269439451539 ) ) ;
#149789 = CARTESIAN_POINT ( 'NONE',  ( 4.022946295931974170, 7.796337852756115794, -0.3444838504574644356 ) ) ;
#149788 = CARTESIAN_POINT ( 'NONE',  ( 2.102840161960460197, -0.4018910908503615653, 1.796694178532439956 ) ) ;
#149790 = CARTESIAN_POINT ( 'NONE',  ( 5.178851490740196795, 7.065079377328788546, 1.443375672974062551 ) ) ;
#149792 = CARTESIAN_POINT ( 'NONE',  ( 0.1054570145121072472, 2.614151819895196738, -2.076146791065091701 ) ) ;
#149791 = CARTESIAN_POINT ( 'NONE',  ( -3.475000000000000533, -3.499999999999999556, 0.000000000000000000 ) ) ;
#149793 = CARTESIAN_POINT ( 'NONE',  ( 1.271856881794002136, 1.368814058113819732, 1.838566387026792093 ) ) ;
#149795 = DIRECTION ( 'NONE',  ( -5.578564026256490882E-16, -1.000000000000000000, -9.066213480720158442E-32 ) ) ;
#149794 = CARTESIAN_POINT ( 'NONE',  ( -9.499640643549723151, -8.037485387949200089, 0.09382487309180524704 ) ) ;
#149796 = CARTESIAN_POINT ( 'NONE',  ( 2.232540727315056373, 1.246330492051262784, -1.450604739030990187 ) ) ;
#149797 = ORIENTED_EDGE ( 'NONE', *, *, #150358, .F. ) ;
#149798 = CARTESIAN_POINT ( 'NONE',  ( 6.914295152845067349, 11.01050207838719075, 1.040834085586084257E-14 ) ) ;
#149799 = VECTOR ( 'NONE', #164049, 1000.000000000000000 ) ;
#149800 = CARTESIAN_POINT ( 'NONE',  ( 1.037359019205979171, -0.04529029187893931357, 2.012842730658084278 ) ) ;
#149801 = CARTESIAN_POINT ( 'NONE',  ( 0.6550357524967264089, 1.634203043994170157, -1.084997510809107446 ) ) ;
#149802 = CARTESIAN_POINT ( 'NONE',  ( -10.08065090696061716, 11.71951313199760136, -1.199719254218441611 ) ) ;
#149804 = DIRECTION ( 'NONE',  ( -0.6507913734559640506, -0.7592566023653003482, 0.000000000000000000 ) ) ;
#149803 = CARTESIAN_POINT ( 'NONE',  ( -7.666245793523398078, 11.03137162816423356, 1.199719254218453823 ) ) ;
#149805 = CARTESIAN_POINT ( 'NONE',  ( -3.285556943750000070, -0.1968749995220411830, 0.000000000000000000 ) ) ;
#149807 = CARTESIAN_POINT ( 'NONE',  ( 2.553260254243350680, 0.4745879851475919842, -1.704939281604215706 ) ) ;
#149806 = CARTESIAN_POINT ( 'NONE',  ( 4.294928614669782263, 1.678954898789623673, 1.245530301124315953 ) ) ;
#149808 = CARTESIAN_POINT ( 'NONE',  ( 1.500000000000001332, 12.12499999999999645, 0.000000000000000000 ) ) ;
#149810 = CARTESIAN_POINT ( 'NONE',  ( 5.753944192167276483, 0.9242165444633635429, 2.097870995526931015 ) ) ;
#149809 = CARTESIAN_POINT ( 'NONE',  ( -11.68285187161687233, 7.296907067810727732, 2.749671221570443080 ) ) ;
#149811 = CARTESIAN_POINT ( 'NONE',  ( 2.888294976258547475, 1.492474662269949182, -0.8948698564717886272 ) ) ;
#149812 = AXIS2_PLACEMENT_3D ( 'NONE', #108631, #89135, #207122 ) ;
#149813 = CARTESIAN_POINT ( 'NONE',  ( 10.37606763316019531, 10.99983374830873650, 0.7998128361456462443 ) ) ;
#149814 = CARTESIAN_POINT ( 'NONE',  ( 4.098537063712264228, 7.253343185014818673, 1.055677455976588686 ) ) ;
#149815 = CARTESIAN_POINT ( 'NONE',  ( 3.268574299048069953, -1.732005324549376279, 0.08218708453346619536 ) ) ;
#149816 =( BOUNDED_CURVE ( )  B_SPLINE_CURVE ( 2, ( #205620, #109280, #175289, #26875, #10617 ),
 .UNSPECIFIED., .F., .T. ) 
 B_SPLINE_CURVE_WITH_KNOTS ( ( 3, 2, 3 ),
 ( 0.1312500000637054354, 0.1333333333333333592, 0.1375000000000000666 ),
 .UNSPECIFIED. ) 
 CURVE ( )  GEOMETRIC_REPRESENTATION_ITEM ( )  RATIONAL_B_SPLINE_CURVE ( ( 0.9330127018922194093, 0.9330127039405975431, 1.000000000000000000, 0.8660254037844369313, 1.000000000000001776 ) ) 
 REPRESENTATION_ITEM ( '' )  );
#149817 = CARTESIAN_POINT ( 'NONE',  ( 3.156845524303863559, -0.6275973837717390147, -2.078511276010074127 ) ) ;
#149818 = CARTESIAN_POINT ( 'NONE',  ( 3.659811400685081040, 6.357198169852855685, -1.199719254218446718 ) ) ;
#149819 = CARTESIAN_POINT ( 'NONE',  ( 5.612517632836664383, 1.944729323200470095, 0.5331731267440716904 ) ) ;
#149820 = CARTESIAN_POINT ( 'NONE',  ( 0.6562500000000004441, -1.895863743164078130, 0.7852924748300215141 ) ) ;
#149821 = B_SPLINE_CURVE_WITH_KNOTS ( 'NONE', 3,
 ( #55771, #121928, #34183, #84000, #1661, #67717, #208409, #124071, #76292, #8082 ),
 .UNSPECIFIED., .F., .F.,
 ( 4, 3, 3, 4 ),
 ( 0.000000000000000000, 3.125173617800492537E-05, 5.893797102792729749E-05, 8.663451821266118878E-05 ),
 .UNSPECIFIED. ) ;
#149822 = CARTESIAN_POINT ( 'NONE',  ( -0.7499999999999972244, 4.639583334016150751, -1.299038105676652899 ) ) ;
#149823 = CARTESIAN_POINT ( 'NONE',  ( 2.116120358982703120, -0.9062717621706478655, -1.699889088518308222 ) ) ;
#149824 = CARTESIAN_POINT ( 'NONE',  ( 1.499999999999993117, 8.385416667349465669, 0.8660254037844409281 ) ) ;
#149825 = CARTESIAN_POINT ( 'NONE',  ( 5.871364357536254630, -1.904906058150414472, -1.142540087918672898 ) ) ;
#149826 = ORIENTED_EDGE ( 'NONE', *, *, #32673, .F. ) ;
#149827 = CARTESIAN_POINT ( 'NONE',  ( -0.1106856583841086261, 2.025759259886884323, -2.413105898545636840 ) ) ;
#149828 = CARTESIAN_POINT ( 'NONE',  ( -0.7500000000000215383, 2.191666666666689078, 1.299038105676671107 ) ) ;
#149829 = CARTESIAN_POINT ( 'NONE',  ( 5.425234023762710578, 9.481190127698507553, -0.7998128361456291469 ) ) ;
#149830 = CARTESIAN_POINT ( 'NONE',  ( 4.161989969270895706, 5.878740935614591656, 1.443375672974062551 ) ) ;
#149831 = CARTESIAN_POINT ( 'NONE',  ( -3.285556943749998737, -1.830208332855373987, 1.896917185911908721 ) ) ;
#149832 = CARTESIAN_POINT ( 'NONE',  ( 1.664984172775041182, 0.7006824767318786673, 2.107951039278654015 ) ) ;
#149834 = EDGE_CURVE ( 'NONE', #195016, #104013, #203748, .T. ) ;
#149833 = CARTESIAN_POINT ( 'NONE',  ( 10.39230484541318589, 3.038454817776199857, -6.000000000000105693 ) ) ;
#149835 = CARTESIAN_POINT ( 'NONE',  ( 9.408995418203975447, 10.07950886410055524, 0.7216878364870438212 ) ) ;
#149836 = SURFACE_SIDE_STYLE ('',( #50192 ) ) ;
#149837 = CARTESIAN_POINT ( 'NONE',  ( 0.2632415847364302786, -1.930764589519979424, -0.9721467891136772455 ) ) ;
#149838 = CARTESIAN_POINT ( 'NONE',  ( 3.881377115262159894, 7.750300077773022878, 0.7998128361456271485 ) ) ;
#149839 = CARTESIAN_POINT ( 'NONE',  ( -4.841670253855968831, 4.821239182352949904, 0.000000000000000000 ) ) ;
#149840 = CARTESIAN_POINT ( 'NONE',  ( 4.615719743604500103, 0.4549637584481819319, -2.011722621177906678 ) ) ;
#149841 = CARTESIAN_POINT ( 'NONE',  ( -4.717347382551060342, 7.590990148696470818, 1.199719254218464037 ) ) ;
#149842 = CARTESIAN_POINT ( 'NONE',  ( -1.201851678989727383E-14, 4.618750000682821266, -1.732050807568863648 ) ) ;
#149843 = CARTESIAN_POINT ( 'NONE',  ( 0.6823417656249864960, -0.5739583329919112353, -1.181850606188749264 ) ) ;
#149845 = B_SPLINE_CURVE_WITH_KNOTS ( 'NONE', 3,
 ( #122320, #71307, #169894, #91888, #58292, #40992, #124448, #21483 ),
 .UNSPECIFIED., .F., .F.,
 ( 4, 2, 2, 4 ),
 ( 0.000000000000000000, 0.001499836411158095902, 0.002999672822316190503, 0.005999345644632378405 ),
 .UNSPECIFIED. ) ;
#149844 = CARTESIAN_POINT ( 'NONE',  ( 5.448468942325162878, 0.5420331153751513087, 1.790312535500695024 ) ) ;
#149846 = CARTESIAN_POINT ( 'NONE',  ( 4.975145882941295561, -1.721944285756441984, -0.2046304421847028043 ) ) ;
#149847 = CARTESIAN_POINT ( 'NONE',  ( 4.335344899790516848, 0.7389749068974335033, -1.575905762629246309 ) ) ;
#149848 = CARTESIAN_POINT ( 'NONE',  ( 4.630273154266905777, 5.360739087188218122, 1.199719254218464037 ) ) ;
#149849 = CARTESIAN_POINT ( 'NONE',  ( 2.050677904428706455, -1.769283327057631805, 1.457584778241685974 ) ) ;
#149850 = CARTESIAN_POINT ( 'NONE',  ( 1.364683531249990311, 4.946875000341417916, 1.214306433183764966E-14 ) ) ;
#149851 = CARTESIAN_POINT ( 'NONE',  ( 5.864805775728457071, 0.1527762835577218814, -2.085202849681159876 ) ) ;
#149852 = CARTESIAN_POINT ( 'NONE',  ( 0.4625323210639306071, 0.1833022542275381250, -1.831979997761295165 ) ) ;
#149853 = CARTESIAN_POINT ( 'NONE',  ( 0.4294077647110511320, -6.532648833121157850, 9.469892045836672878 ) ) ;
#149854 = FILL_AREA_STYLE ('',( #118471 ) ) ;
#149855 = CARTESIAN_POINT ( 'NONE',  ( 1.213517774399593740, 1.944071949784083264, 0.5350861613380719639 ) ) ;
#149856 = CARTESIAN_POINT ( 'NONE',  ( -3.741687207247254676, 7.309126141856352454, 1.040834085586084257E-14 ) ) ;
#149857 = CARTESIAN_POINT ( 'NONE',  ( 9.645118626927368766, 13.59280469987849216, -8.209452448563446580 ) ) ;
#149858 = CARTESIAN_POINT ( 'NONE',  ( -8.389798128758148010, 8.682519326506312751, 0.7998128361456462443 ) ) ;
#149859 = CARTESIAN_POINT ( 'NONE',  ( 6.169123589417988995, 7.156064594864501416, -1.199719254218445830 ) ) ;
#149860 = CARTESIAN_POINT ( 'NONE',  ( -1.360316468749990459, 1.890625000341386475, -2.428612866367529932E-14 ) ) ;
#149861 = CARTESIAN_POINT ( 'NONE',  ( 4.002672028760116518, -2.097606743168555443, -0.3097674545872728946 ) ) ;
#149862 = CARTESIAN_POINT ( 'NONE',  ( -1.364683531250014514, -0.5114583329919092369, -0.7879004041258359514 ) ) ;
#149863 = CARTESIAN_POINT ( 'NONE',  ( 5.443921307256319508, 0.7362202147598860824, -1.670853202368662860 ) ) ;
#149864 = VERTEX_POINT ( 'NONE', #105 ) ;
#149865 = CARTESIAN_POINT ( 'NONE',  ( -6.631873415740034083, 7.766215735565355160, 1.199719254218452047 ) ) ;
#149866 = SURFACE_SIDE_STYLE ('',( #134699 ) ) ;
#149867 = CARTESIAN_POINT ( 'NONE',  ( -3.475000000000000533, -2.085416665710750905, -2.006292185433948827 ) ) ;
#149868 = CARTESIAN_POINT ( 'NONE',  ( -7.054319997812058318, 7.124461507069184130, 1.040834085586084257E-14 ) ) ;
#149869 = CARTESIAN_POINT ( 'NONE',  ( 2.988540512386147707, -1.199814222051265311, 1.624667845120256748 ) ) ;
#149870 = CARTESIAN_POINT ( 'NONE',  ( 0.1828346100962909559, -2.042824957133956953, -0.5113311198858895290 ) ) ;
#149871 = CARTESIAN_POINT ( 'NONE',  ( 8.703444544968814256, 12.24143683818393313, -1.199719254218446718 ) ) ;
#149872 = CARTESIAN_POINT ( 'NONE',  ( 3.924516644892431572, -1.252765583397809079, 1.376256255023865283 ) ) ;
#149873 = CARTESIAN_POINT ( 'NONE',  ( 10.21336978979620191, 10.81001959771741205, 0.7998128361456462443 ) ) ;
#149874 = DIRECTION ( 'NONE',  ( 0.000000000000000000, 1.000000000000000000, 0.000000000000000000 ) ) ;
#149875 = ORIENTED_EDGE ( 'NONE', *, *, #125621, .F. ) ;
#149876 = CARTESIAN_POINT ( 'NONE',  ( -4.115063316947640715, 4.759660943649018705, 1.199719254218462483 ) ) ;
#149877 = AXIS2_PLACEMENT_3D ( 'NONE', #159670, #78414, #25394 ) ;
#149878 = CARTESIAN_POINT ( 'NONE',  ( -8.342344591110322227, 8.627156865917170236, -0.7998128361456291469 ) ) ;
#149879 = CARTESIAN_POINT ( 'NONE',  ( 6.368051766976638994, 1.057089778920755840, 1.768976859881221442 ) ) ;
#149880 = AXIS2_PLACEMENT_3D ( 'NONE', #166404, #149086, #101403 ) ;
#149882 = CARTESIAN_POINT ( 'NONE',  ( -4.695247098932518348, 7.056227087241170537, 1.405392365797274445 ) ) ;
#149881 = CARTESIAN_POINT ( 'NONE',  ( -5.725286006720766707, 9.901527117808042178, 0.7998128361456291469 ) ) ;
#149883 = CARTESIAN_POINT ( 'NONE',  ( 5.364607279338250656, 7.693244595681929532, -1.319704323257679057 ) ) ;
#149884 = CARTESIAN_POINT ( 'NONE',  ( 1.141452232654313059, -0.03515412242651934360, -1.733669386235114906 ) ) ;
#149885 = CARTESIAN_POINT ( 'NONE',  ( 1.728031430807571267, 0.1683455491279534644, 1.732166925338991303 ) ) ;
#149887 = CARTESIAN_POINT ( 'NONE',  ( 8.609064354997688184, 9.146255957026539818, 1.040834085586084257E-14 ) ) ;
#149886 = CARTESIAN_POINT ( 'NONE',  ( 6.182281242350501138, -1.240197753460486663, 1.945954285860839850 ) ) ;
#149888 = CARTESIAN_POINT ( 'NONE',  ( 5.063044020060520900, 4.871582543017558109, 0.7998128361456352531 ) ) ;
#149889 = CARTESIAN_POINT ( 'NONE',  ( 1.388040899126226302, -0.9290452130323262336, 1.839580399304826752 ) ) ;
#149890 = CARTESIAN_POINT ( 'NONE',  ( 6.608760977740426590, 0.8891218545476579083, -2.119637956729656381 ) ) ;
#149891 = CARTESIAN_POINT ( 'NONE',  ( 0.9311234436981489226, -1.646869630441518240, 3.475000000000000533 ) ) ;
#149892 = CARTESIAN_POINT ( 'NONE',  ( -3.962726036944197894, 7.845207153068690431, -0.7998128361456481317 ) ) ;
#149893 = CARTESIAN_POINT ( 'NONE',  ( 6.297708355432167338, -0.6282832542035889922, 1.762108908958268216 ) ) ;
#149895 = CARTESIAN_POINT ( 'NONE',  ( -5.641601317062233001, 9.595968946632336127, -0.7216878364870338292 ) ) ;
#149894 = CARTESIAN_POINT ( 'NONE',  ( 4.394721148579957770, -1.856311205515799312, -0.4593126252911489127 ) ) ;
#149896 = CARTESIAN_POINT ( 'NONE',  ( 6.322910218073367616, 2.057572540570989261, 0.7984293639632376038 ) ) ;
#149897 = CARTESIAN_POINT ( 'NONE',  ( -8.054952659850432184, 8.570068656013202002, 0.000000000000000000 ) ) ;
#149898 = CARTESIAN_POINT ( 'NONE',  ( 3.051993976407674225, 6.574760382535328240, -0.7216878364870338292 ) ) ;
#149899 = CARTESIAN_POINT ( 'NONE',  ( -4.841670253411603397, 5.781608396135871075, 1.082531754730549078 ) ) ;
#149900 = CARTESIAN_POINT ( 'NONE',  ( 0.08268334464456467137, -1.317614589208983444, 1.530782303595918714 ) ) ;
#149901 = VERTEX_POINT ( 'NONE', #66171 ) ;
#149902 = CARTESIAN_POINT ( 'NONE',  ( 3.346982425237558179, 0.5585957852003355928, 2.238849765380794832 ) ) ;
#149903 = CARTESIAN_POINT ( 'NONE',  ( 5.213317179658601752, -1.656387821537348426, -1.051046178410528942 ) ) ;
#149904 = CARTESIAN_POINT ( 'NONE',  ( 2.254674508890702089, -0.5182927192734412269, -1.892014123021222627 ) ) ;
#149905 = DIRECTION ( 'NONE',  ( -1.000000000000000000, 0.000000000000000000, 0.000000000000000000 ) ) ;
#149906 = CARTESIAN_POINT ( 'NONE',  ( -9.383881589012478486, 15.40581400629704945, 7.387911201601294664 ) ) ;
#149907 = ORIENTED_EDGE ( 'NONE', *, *, #111061, .T. ) ;
#149908 = CARTESIAN_POINT ( 'NONE',  ( -0.1001773172763717329, -2.075113514603315945, 0.4199855073994100407 ) ) ;
#149910 = CARTESIAN_POINT ( 'NONE',  ( -6.984421689334302741, 11.30024240419870374, 0.000000000000000000 ) ) ;
#149909 = CARTESIAN_POINT ( 'NONE',  ( -3.737243898861318137, 7.511868315313511069, 0.7998128361456341429 ) ) ;
#149911 = CARTESIAN_POINT ( 'NONE',  ( -0.02900071798685524560, -0.004641455105012376459, -2.173770343569726649 ) ) ;
#149912 = CARTESIAN_POINT ( 'NONE',  ( 3.942362285364631624, -1.074967207919340861, 1.886227828529878803 ) ) ;
#149913 = CARTESIAN_POINT ( 'NONE',  ( 10.65566590394000634, 9.862353226835116615, -5.420130399562989254 ) ) ;
#149914 = CARTESIAN_POINT ( 'NONE',  ( 1.898838059644195386, -2.080654286433290867, -0.4088066060855889972 ) ) ;
#149915 = CARTESIAN_POINT ( 'NONE',  ( -0.7500000000000006661, 2.889583334016148974, -1.299038105676652011 ) ) ;
#149916 = CARTESIAN_POINT ( 'NONE',  ( 9.901532256681887745, 10.44620914241737530, 0.000000000000000000 ) ) ;
#149917 = CARTESIAN_POINT ( 'NONE',  ( -4.909967638851771454, 4.671257834700952571, -0.2941531795261614346 ) ) ;
#149918 = CARTESIAN_POINT ( 'NONE',  ( 6.546060204425600659, 6.805396270974036987, -0.4351356575816138772 ) ) ;
#149919 = CARTESIAN_POINT ( 'NONE',  ( 1.968112693492467979, 1.056634718301739717, 1.769108711375965148 ) ) ;
#149920 = CARTESIAN_POINT ( 'NONE',  ( -8.045874094706015001, 11.47427131287732927, -1.199719254218446718 ) ) ;
#149921 = CARTESIAN_POINT ( 'NONE',  ( 0.6823417656249882723, 2.676041667008084879, -1.181850606188749264 ) ) ;
#149922 = CARTESIAN_POINT ( 'NONE',  ( -0.02264175331117417728, 6.946776101658422853, -2.684156320254589279 ) ) ;
#149923 = CARTESIAN_POINT ( 'NONE',  ( -2.449742653233043743, 3.299999999999976730, -0.4000000000000339950 ) ) ;
#149924 = VERTEX_POINT ( 'NONE', #117155 ) ;
#149925 = CARTESIAN_POINT ( 'NONE',  ( 4.582611755193141789, -1.246403352314252810, 1.450376384258989182 ) ) ;
#149926 = CARTESIAN_POINT ( 'NONE',  ( 11.92619526913699701, 12.69999999999999929, -1.328859060402686199 ) ) ;
#149927 = CARTESIAN_POINT ( 'NONE',  ( 1.071959817704574602, 2.180298862187507680, -0.6038346756046736319 ) ) ;
#149928 = CARTESIAN_POINT ( 'NONE',  ( -8.663296969452339624, 13.05100419776235299, 1.040834085586084257E-14 ) ) ;
#149929 = CARTESIAN_POINT ( 'NONE',  ( 1.300706311995255771, -0.2675212335121620599, -1.791602419159578519 ) ) ;
#149930 = CARTESIAN_POINT ( 'NONE',  ( 2.501083532561697798, -0.1830384092258540707, 1.906917772027187929 ) ) ;
#149931 = CARTESIAN_POINT ( 'NONE',  ( 2.857943571468853250, -0.6518772230660694333, 1.965110387975615991 ) ) ;
#149932 = CARTESIAN_POINT ( 'NONE',  ( 1.364683531249988535, 2.176041667008087543, 0.7879004041258500513 ) ) ;
#149933 = CARTESIAN_POINT ( 'NONE',  ( 0.4792893823705188794, 1.840408107720743924, -0.7072656782263522235 ) ) ;
#149934 = CARTESIAN_POINT ( 'NONE',  ( 5.619733630554700099, -1.879067156935828820, 0.4242066570522682878 ) ) ;
#149936 = CARTESIAN_POINT ( 'NONE',  ( 5.504185490526544378, 7.460110003252303557, -1.249659907641489820 ) ) ;
#149935 = CARTESIAN_POINT ( 'NONE',  ( -0.01646294620048001714, -0.1635519927996042511, -2.271437254364586877 ) ) ;
#149937 = CARTESIAN_POINT ( 'NONE',  ( -1.364683531250012516, 2.280208333674751842, 0.7879004041258379498 ) ) ;
#149938 = CARTESIAN_POINT ( 'NONE',  ( 4.826661651916083429, -1.349687995210807401, 1.559865583710306147 ) ) ;
#149939 = MECHANICAL_DESIGN_GEOMETRIC_PRESENTATION_REPRESENTATION (  '', ( #187945 ), #200917 ) ;
#149940 = CARTESIAN_POINT ( 'NONE',  ( -5.442708600882160574, 8.437244903416123876, -1.199719254218446718 ) ) ;
#149941 = CARTESIAN_POINT ( 'NONE',  ( 8.749089199520284410, 9.101692242395490240, 0.7998128361456481317 ) ) ;
#149942 = CARTESIAN_POINT ( 'NONE',  ( 0.000000000000000000, 5.868705557303649734, -4.125226524755057689 ) ) ;
#149944 = CARTESIAN_POINT ( 'NONE',  ( -1.500000000000011324, 3.420833333333355597, 0.8660254037844403729 ) ) ;
#149943 = CARTESIAN_POINT ( 'NONE',  ( 4.770599357992978184, -1.377743202910805875, 1.592837501749831519 ) ) ;
#149945 = CARTESIAN_POINT ( 'NONE',  ( 1.100314673101766338, 0.8801652113111978482, -1.984954624234806175 ) ) ;
#149947 = CARTESIAN_POINT ( 'NONE',  ( -0.6823417656250212460, 3.363541667008085323, 1.181850606188767472 ) ) ;
#149946 = AXIS2_PLACEMENT_3D ( 'NONE', #145372, #80317, #65111 ) ;
#149948 = CARTESIAN_POINT ( 'NONE',  ( 5.360679719606757487, -1.569739296358707570, 1.486333574453831519 ) ) ;
#149949 = CARTESIAN_POINT ( 'NONE',  ( 5.549475203002828927, -1.825015992387307273, 0.8654263401719575199 ) ) ;
#149950 = CARTESIAN_POINT ( 'NONE',  ( -0.1399997263889611598, 6.947783040739049731, -2.595329734540325006 ) ) ;
#149951 = CIRCLE ( 'NONE', #143031, 0.08000000000000020983 ) ;
#149954 = CARTESIAN_POINT ( 'NONE',  ( 5.504247177468179153, 7.444707678511436555, 1.443375672974062551 ) ) ;
#149953 = CARTESIAN_POINT ( 'NONE',  ( 1.642778471875000035, -2.676041666188708756, -2.845375778867859751 ) ) ;
#149952 = CARTESIAN_POINT ( 'NONE',  ( -9.053429965380070499, 14.55305227869001783, -7.821648902489916289 ) ) ;
#149955 = CARTESIAN_POINT ( 'NONE',  ( -5.550083779947821760, 7.568460058062819407, -1.599625672291271394 ) ) ;
#149956 = CARTESIAN_POINT ( 'NONE',  ( 3.837125247982266174, -1.679222704393277921, -1.116210984008485507 ) ) ;
#149957 = CARTESIAN_POINT ( 'NONE',  ( -7.330154606482786050, 11.70359747420527619, 0.000000000000000000 ) ) ;
#149959 = CARTESIAN_POINT ( 'NONE',  ( -10.97093617010560429, -5.223179855899848789, 0.3663205537282924751 ) ) ;
#149958 = CARTESIAN_POINT ( 'NONE',  ( -2.927671105547157371, 5.503034492191895666, 1.199719254218462483 ) ) ;
#149960 = CARTESIAN_POINT ( 'NONE',  ( 0.6823417656249917140, 4.092708333674755394, 1.181850606188765695 ) ) ;
#149962 = CARTESIAN_POINT ( 'NONE',  ( -11.96212011828583677, 12.27187554950063308, -0.9569185076418453839 ) ) ;
#149961 = CARTESIAN_POINT ( 'NONE',  ( 4.856408821558930278, 0.8241108818672329139, 1.998647875481096126 ) ) ;
#149963 = DIRECTION ( 'NONE',  ( -5.578564026256490882E-16, -1.000000000000000000, -9.066213480720158442E-32 ) ) ;
#149964 = EDGE_CURVE ( 'NONE', #11599, #8789, #80175, .T. ) ;
#149966 = CARTESIAN_POINT ( 'NONE',  ( 5.202749988929913805, 1.864175517894875789, 0.7691070904374335271 ) ) ;
#149965 = CARTESIAN_POINT ( 'NONE',  ( -5.843201017365469596, 9.760892253660966134, 0.7216878364870458196 ) ) ;
#149967 = CARTESIAN_POINT ( 'NONE',  ( -1.500000000000011324, 4.629166666666689522, -0.8660254037844313801 ) ) ;
#149968 = CARTESIAN_POINT ( 'NONE',  ( 0.09967489844521590370, -1.724374414367945141, -0.04833993824084405894 ) ) ;
#149969 = CARTESIAN_POINT ( 'NONE',  ( 5.357406976055401948, 6.279338222599979424, 1.199719254218452935 ) ) ;
#149971 = CARTESIAN_POINT ( 'NONE',  ( 7.666209513884374438, 7.908608952478760834, 0.7998128361456281477 ) ) ;
#149970 = CARTESIAN_POINT ( 'NONE',  ( 7.700668062882064291, 10.00719871149432549, -1.443375672974057666 ) ) ;
#149972 = CARTESIAN_POINT ( 'NONE',  ( 5.940666398231567058, 0.3644617591120716260, 1.834516074763043347 ) ) ;
#149973 = CARTESIAN_POINT ( 'NONE',  ( 5.871345457035325843, -1.728819661934883678, -1.031334786431532313 ) ) ;
#149974 = CARTESIAN_POINT ( 'NONE',  ( 6.539320575229228716, 1.281788455817688188, 2.013036689384885225 ) ) ;
#149975 = CARTESIAN_POINT ( 'NONE',  ( 3.023105065722954787, 5.510411095776657220, 1.082531754730546636 ) ) ;
#149976 = CARTESIAN_POINT ( 'NONE',  ( -5.763624699140868834, 9.738329559057408602, -0.7216878364870338292 ) ) ;
#149977 = ORIENTED_EDGE ( 'NONE', *, *, #41144, .F. ) ;
#149979 = CARTESIAN_POINT ( 'NONE',  ( 1.265250157614560056, 1.862010354082011876, -0.7743342583275417690 ) ) ;
#149978 = CARTESIAN_POINT ( 'NONE',  ( 2.543736517606724146, -1.977637755382474438, 0.7655657148115800892 ) ) ;
#149980 = CARTESIAN_POINT ( 'NONE',  ( 2.583996913715621790, 0.9723193252555061283, 1.528341728153536305 ) ) ;
#149981 = CARTESIAN_POINT ( 'NONE',  ( 7.713663051532233972, 7.963971413067895355, -0.7998128361456341429 ) ) ;
#149982 = CARTESIAN_POINT ( 'NONE',  ( 6.631704542599726082, -1.407888343591977121, -1.640466528430361670 ) ) ;
#149983 = CARTESIAN_POINT ( 'NONE',  ( 7.233438648090761980, 8.397765496649418182, 1.199719254218462483 ) ) ;
#149985 = CARTESIAN_POINT ( 'NONE',  ( 0.05764063133973944958, 1.105241252117078909, 1.564514492536345891 ) ) ;
#149984 = CARTESIAN_POINT ( 'NONE',  ( -6.254388934605767503, 6.191208599995166040, 0.7998128361456341429 ) ) ;
#149986 = CARTESIAN_POINT ( 'NONE',  ( 1.930226670627029684, 8.999999999999998224, 0.7750000000000004663 ) ) ;
#149987 = SURFACE_STYLE_FILL_AREA ( #148912 ) ;
#149988 = EDGE_CURVE ( 'NONE', #74967, #184212, #160368, .T. ) ;
#149989 = CARTESIAN_POINT ( 'NONE',  ( 4.799223189113185128, 8.542918120699967588, 1.040834085586084257E-14 ) ) ;
#149990 = CARTESIAN_POINT ( 'NONE',  ( 0.6823417656249899377, 0.9052083336747520637, 1.181850606188755259 ) ) ;
#149991 = DIRECTION ( 'NONE',  ( -0.000000000000000000, 1.000000000000000000, -0.000000000000000000 ) ) ;
#149992 = CARTESIAN_POINT ( 'NONE',  ( -2.137381772448751605, 5.645362501165475777, -0.7998128361456281477 ) ) ;
#149993 = CARTESIAN_POINT ( 'NONE',  ( 3.836934241894359054, 0.3148432204054998351, 2.138525872868973998 ) ) ;
#149994 = CARTESIAN_POINT ( 'NONE',  ( -4.977251789992602760, 8.820894498384422633, 0.000000000000000000 ) ) ;
#149995 = CARTESIAN_POINT ( 'NONE',  ( 4.746763178560254204, 6.631252689777363152, 1.443375672974065660 ) ) ;
#149996 = CARTESIAN_POINT ( 'NONE',  ( 2.285534418239892229, 0.09939759515392716793, -2.118372479656557061 ) ) ;
#149997 = CARTESIAN_POINT ( 'NONE',  ( 6.633835642106551411, -1.195214757176918496, -1.380038946949893486 ) ) ;
#149998 =( BOUNDED_CURVE ( )  B_SPLINE_CURVE ( 3, ( #92766, #175077, #77549, #163088 ),
 .UNSPECIFIED., .F., .T. ) 
 B_SPLINE_CURVE_WITH_KNOTS ( ( 4, 4 ),
 ( 0.000000000000000000, 0.5000000000000017764 ),
 .UNSPECIFIED. ) 
 CURVE ( )  GEOMETRIC_REPRESENTATION_ITEM ( )  RATIONAL_B_SPLINE_CURVE ( ( 1.000000000000000000, 0.3333333333333309834, 0.3333333333333333703, 1.000000000000002442 ) ) 
 REPRESENTATION_ITEM ( '' )  );
#149999 = CARTESIAN_POINT ( 'NONE',  ( 3.251204012874517879, -1.609649185575717123, -1.137836448096725794 ) ) ;
#150000 = CARTESIAN_POINT ( 'NONE',  ( 5.818603510220927255, -0.6945032022064903110, -1.782003016414166474 ) ) ;
#150001 = EDGE_LOOP ( 'NONE', ( #140413, #140175, #72793, #152833, #19833, #170749, #207888, #64527, #43963, #211633, #55952, #182858, #10974, #59213, #43457, #124903, #91388, #38710, #63429, #39986, #159383, #22883, #164633, #147486, #87906 ) ) ;
#150002 = CARTESIAN_POINT ( 'NONE',  ( 9.481437597266046069, -6.708819892820501174, -0.4299312922663391379 ) ) ;
#150003 = CARTESIAN_POINT ( 'NONE',  ( 5.529738209476210642, 1.898601866877418942, -0.5236614360015124925 ) ) ;
#150004 = CARTESIAN_POINT ( 'NONE',  ( 1.447104159573095572, 0.5638456037007446575, -1.858296221435972617 ) ) ;
#150005 = ORIENTED_EDGE ( 'NONE', *, *, #141317, .T. ) ;
#150006 = CARTESIAN_POINT ( 'NONE',  ( -3.797165540279144214, 6.587721009371067638, 1.199719254218452935 ) ) ;
#150008 = CARTESIAN_POINT ( 'NONE',  ( 1.838377265450863440, 2.505607861886320897, -2.496072963307877313 ) ) ;
#150007 = CARTESIAN_POINT ( 'NONE',  ( -5.777182853198894463, 9.754147405458438058, 0.7216878364870267237 ) ) ;
#150009 = CARTESIAN_POINT ( 'NONE',  ( 5.608269097547198712, 9.694731047113750222, -0.7998128361456281477 ) ) ;
#150011 = CARTESIAN_POINT ( 'NONE',  ( 4.055297343818923039, 7.745280977848496562, 0.7216878364870257245 ) ) ;
#150010 = CARTESIAN_POINT ( 'NONE',  ( 7.955937213120826357, 8.176348258262782664, 0.7998128361456481317 ) ) ;
#150013 = ORIENTED_EDGE ( 'NONE', *, *, #7856, .T. ) ;
#150012 = CARTESIAN_POINT ( 'NONE',  ( 6.569012486276131213, -1.474873517498687558, 1.216900358440069052 ) ) ;
#150014 = CARTESIAN_POINT ( 'NONE',  ( 3.528125218122651230, -1.314342534882004809, -1.772652456903674567 ) ) ;
#150015 = CARTESIAN_POINT ( 'NONE',  ( 1.835297179245497068, 0.2165863673247066801, 2.196102686035047213 ) ) ;
#150016 = FACE_OUTER_BOUND ( 'NONE', #14329, .T. ) ;
#150017 = CARTESIAN_POINT ( 'NONE',  ( 0.4867802866235851345, -1.800715477623024086, -0.6440170976053718466 ) ) ;
#150018 = LINE ( 'NONE', #1588, #66189 ) ;
#150019 = CARTESIAN_POINT ( 'NONE',  ( -0.1263102688159843667, 6.363441598446241798, 3.117922131261609664 ) ) ;
#150020 = CARTESIAN_POINT ( 'NONE',  ( 3.455589482447297911, 1.630370400113917873, 1.275915752658785873 ) ) ;
#150021 = CARTESIAN_POINT ( 'NONE',  ( -4.238895582566952314, 8.097128612970093897, 1.040834085586084257E-14 ) ) ;
#150022 = CARTESIAN_POINT ( 'NONE',  ( -6.197060558222979409, 6.958367536249086882, 0.8797177744420351386 ) ) ;
#150023 = AXIS2_PLACEMENT_3D ( 'NONE', #173661, #25234, #58811 ) ;
#150025 = CARTESIAN_POINT ( 'NONE',  ( 1.446389902895691693, 2.159248346720197276, 0.1057134262518744372 ) ) ;
#150024 = CARTESIAN_POINT ( 'NONE',  ( -3.469997250093771246, 6.135748327496311383, -1.199719254218452935 ) ) ;
#150026 = CARTESIAN_POINT ( 'NONE',  ( 3.404031855413204966, -0.8899279105200922357, -2.002928011436304612 ) ) ;
#150027 = CARTESIAN_POINT ( 'NONE',  ( 6.938893903907228378E-15, 10.64264068711930733, 1.214306433183764966E-14 ) ) ;
#150028 = CARTESIAN_POINT ( 'NONE',  ( 4.095971805104288599, 5.871996087412059140, 1.443375672974058777 ) ) ;
#150029 = CARTESIAN_POINT ( 'NONE',  ( -0.07933194154488912297, -7.246166700194011767, 9.499668754385634628 ) ) ;
#150030 = CARTESIAN_POINT ( 'NONE',  ( -8.012344526598182026E-15, 14.85937500034139980, -1.575800808251669460 ) ) ;
#150031 = CARTESIAN_POINT ( 'NONE',  ( -4.847922445338252118, 7.813604065273374921, -1.199719254218453823 ) ) ;
#150032 = UNCERTAINTY_MEASURE_WITH_UNIT (LENGTH_MEASURE( 1.000000000000000082E-05 ), #177834, 'distance_accuracy_value', 'NONE');
#150033 = CARTESIAN_POINT ( 'NONE',  ( 6.328739007766592373, 0.6541968508507016722, -1.606262126034884608 ) ) ;
#150034 = CARTESIAN_POINT ( 'NONE',  ( -2.656508033273816238, 5.186677574539687363, -1.199719254218446718 ) ) ;
#150035 = CARTESIAN_POINT ( 'NONE',  ( 3.907136544319700810, -1.695332804699274387, 1.187946514627869821 ) ) ;
#150036 = CARTESIAN_POINT ( 'NONE',  ( 5.765271170472290763, 1.955999355395316996, -0.8108409051663100220 ) ) ;
#150037 = CARTESIAN_POINT ( 'NONE',  ( 7.135668919494039031, 7.219368582364847242, 1.040834085586084257E-14 ) ) ;
#150038 = CARTESIAN_POINT ( 'NONE',  ( 0.6823417656249899377, 5.176041667008086655, -1.181850606188754593 ) ) ;
#150039 = CARTESIAN_POINT ( 'NONE',  ( 2.834760172256750810, -1.883157219239324887, -0.5764521555583942414 ) ) ;
#150040 = CARTESIAN_POINT ( 'NONE',  ( 1.406358598101828283, -1.903450966454448334, -0.1843715739238485363 ) ) ;
#150041 = CARTESIAN_POINT ( 'NONE',  ( 6.210887435761151210, -0.2868632742878024500, 2.274177813689901573 ) ) ;
#150042 = CARTESIAN_POINT ( 'NONE',  ( 3.369579884941567016, 1.780956498284639533, -0.4009276245297774266 ) ) ;
#150043 = CARTESIAN_POINT ( 'NONE',  ( 5.388439706788500594, 5.251210844200210559, 0.7998128361456352531 ) ) ;
#150044 = CARTESIAN_POINT ( 'NONE',  ( 3.985733972293228344, 7.593847367743336463, 1.040834085586084257E-14 ) ) ;
#150045 = CARTESIAN_POINT ( 'NONE',  ( -6.856673000209188906, 9.022537805042615489, 1.599625672291283607 ) ) ;
#150046 = ORIENTED_EDGE ( 'NONE', *, *, #176483, .F. ) ;
#150047 = ORIENTED_EDGE ( 'NONE', *, *, #57277, .T. ) ;
#150048 = CARTESIAN_POINT ( 'NONE',  ( 3.551042609437846220, 0.2996916850201857829, 1.990680017358969600 ) ) ;
#150049 = CARTESIAN_POINT ( 'NONE',  ( 4.117980938109369937, 1.947433809354440326, -0.2358448244534834815 ) ) ;
#150050 = CARTESIAN_POINT ( 'NONE',  ( -8.128276786592724790, 9.441743324901704426, -1.199719254218446718 ) ) ;
#150051 = CARTESIAN_POINT ( 'NONE',  ( -6.573005544526917099, 6.562927978236513304, -0.7998128361456291469 ) ) ;
#150052 = CARTESIAN_POINT ( 'NONE',  ( 0.1753634416057497925, 7.629137130509101361, -2.744001747789548418 ) ) ;
#150054 = CARTESIAN_POINT ( 'NONE',  ( 5.242920984569427567, -1.516648554753729616, 0.9119251698698880304 ) ) ;
#150053 = CARTESIAN_POINT ( 'NONE',  ( 0.3981334665579424059, -0.7082897861981848342, -1.967241634975321452 ) ) ;
#150055 = CARTESIAN_POINT ( 'NONE',  ( -11.86239285000045918, 12.22000000000000064, -1.812080536912752837 ) ) ;
#150056 = CARTESIAN_POINT ( 'NONE',  ( 1.746283639092637729, 0.6896231194409886411, 2.080178558289603963 ) ) ;
#150057 = CARTESIAN_POINT ( 'NONE',  ( 0.08108764725259924588, -0.8233000410203991093, 1.533359828670758374 ) ) ;
#150058 = CARTESIAN_POINT ( 'NONE',  ( 7.721532178182734185, 8.967207948423393304, 1.199719254218462483 ) ) ;
#150059 = CARTESIAN_POINT ( 'NONE',  ( 0.2335667940003049725, 0.6933325534057503958, -2.235178663643789143 ) ) ;
#150060 = CARTESIAN_POINT ( 'NONE',  ( 0.2754634098539961440, 0.9884889332615778290, 1.413329177942000303 ) ) ;
#150061 = CARTESIAN_POINT ( 'NONE',  ( 0.9138903340461038693, 0.6688396875448484602, 2.198942881657910853 ) ) ;
#150062 = CARTESIAN_POINT ( 'NONE',  ( 0.8025787753177977546, 1.655945718051672566, -1.435626523826734280 ) ) ;
#150063 = CARTESIAN_POINT ( 'NONE',  ( 6.151638658550825589, -0.2577636348817541334, -1.714396880517143451 ) ) ;
#150064 = CARTESIAN_POINT ( 'NONE',  ( 2.719571217284349363, -0.2154062111461417517, 2.196339928330424129 ) ) ;
#150065 = CARTESIAN_POINT ( 'NONE',  ( 0.6378409936122396706, 2.026330576540099404, -0.7799181171992456418 ) ) ;
#150066 = CARTESIAN_POINT ( 'NONE',  ( -9.499606442108964544, -9.746166700193986898, 0.08647222121513538362 ) ) ;
#150067 = CARTESIAN_POINT ( 'NONE',  ( 1.798220840057991543, -1.003180963283013982, -1.864648404631663148 ) ) ;
#150068 = CARTESIAN_POINT ( 'NONE',  ( 6.727182134110234024, 7.051482179251418181, 2.887205776801844426 ) ) ;
#150069 = CARTESIAN_POINT ( 'NONE',  ( 5.315425438393720725, -0.2827910679824903184, 1.905415604636887750 ) ) ;
#150070 = EDGE_LOOP ( 'NONE', ( #77673, #72408, #75486, #149319 ) ) ;
#150072 = CARTESIAN_POINT ( 'NONE',  ( -1.500000000000011324, 5.879166666666686858, -0.8660254037844313801 ) ) ;
#150071 = CARTESIAN_POINT ( 'NONE',  ( 2.296762559223310074, 1.838876890742843884, -1.368561501106011713 ) ) ;
#150073 = CARTESIAN_POINT ( 'NONE',  ( 4.857899112398166075, 4.561970474086296079, 1.040834085586084257E-14 ) ) ;
#150074 = CARTESIAN_POINT ( 'NONE',  ( 5.301401758143367893, 6.143722458377430584, 1.199719254218462483 ) ) ;
#150075 = CARTESIAN_POINT ( 'NONE',  ( 4.459788417035775332, -1.717034742021033455, -1.409269467666877995 ) ) ;
#150076 = CARTESIAN_POINT ( 'NONE',  ( -6.073689629242151611, 10.02979563418376685, -0.7216878364870278340 ) ) ;
#150077 = ADVANCED_FACE ( 'NONE', ( #166920 ), #205024, .T. ) ;
#150078 = CARTESIAN_POINT ( 'NONE',  ( 6.968527767744109980, 7.232296605230681408, 0.7216878364870317197 ) ) ;
#150079 = B_SPLINE_CURVE_WITH_KNOTS ( 'NONE', 3,
 ( #44772, #176885, #211497, #95664, #31711, #78305 ),
 .UNSPECIFIED., .F., .F.,
 ( 4, 2, 4 ),
 ( 0.000000000000000000, 0.0003767011250903909642, 0.0007534022501807819284 ),
 .UNSPECIFIED. ) ;
#150080 = CARTESIAN_POINT ( 'NONE',  ( -8.392133896734675247, 10.81390885098904420, 1.443375672974064550 ) ) ;
#150081 = CIRCLE ( 'NONE', #46345, 4.583333333333340143 ) ;
#150082 = CARTESIAN_POINT ( 'NONE',  ( 5.722950238744209273, 6.809768379023969587, 1.082531754730549967 ) ) ;
#150083 = ORIENTED_EDGE ( 'NONE', *, *, #201840, .F. ) ;
#150084 = CARTESIAN_POINT ( 'NONE',  ( 3.410779880581996437, -1.203353552534730309, -1.617818353255597863 ) ) ;
#150086 = CARTESIAN_POINT ( 'NONE',  ( 0.5673240888519160974, 1.792687530798135143, 1.019967006830464706 ) ) ;
#150085 = CARTESIAN_POINT ( 'NONE',  ( 7.233438648090761980, 8.397765496649418182, 1.199719254218462483 ) ) ;
#150087 = DIRECTION ( 'NONE',  ( 0.000000000000000000, -0.000000000000000000, 1.000000000000000000 ) ) ;
#150088 = CARTESIAN_POINT ( 'NONE',  ( 5.167065940139554669, 9.042344340222555843, -0.7216878364870458196 ) ) ;
#150089 = STYLED_ITEM ( 'NONE', ( #208312 ), #185816 ) ;
#150090 = PLANE ( 'NONE',  #71494 ) ;
#150091 = CARTESIAN_POINT ( 'NONE',  ( -1.364683531250012516, 3.988541667008088876, -0.7879004041258300672 ) ) ;
#150092 = CARTESIAN_POINT ( 'NONE',  ( 4.347736757272718577, 2.190986304709115373, -0.05254992341368477232 ) ) ;
#150093 = CARTESIAN_POINT ( 'NONE',  ( 1.248672897702383988, 1.986100274556975354, -0.3474695496914689818 ) ) ;
#150094 = CARTESIAN_POINT ( 'NONE',  ( 0.6965153189463432204, 1.505040478001760107, 1.060415605250275339 ) ) ;
#150095 = CARTESIAN_POINT ( 'NONE',  ( 5.056304237002312796, -1.661761009075436002, 1.579303468685322009 ) ) ;
#150096 = CARTESIAN_POINT ( 'NONE',  ( 3.978315823851843014, -0.1823813840945518738, -1.832081410093854501 ) ) ;
#150097 = ADVANCED_FACE ( 'NONE', ( #10788 ), #68130, .T. ) ;
#150098 = CARTESIAN_POINT ( 'NONE',  ( 7.741869408603235136, 8.990934717247309749, 1.199719254218462483 ) ) ;
#150099 = CARTESIAN_POINT ( 'NONE',  ( 3.926616521958687045, 1.733384925006593136, 0.5729815612169064654 ) ) ;
#150100 = CARTESIAN_POINT ( 'NONE',  ( 4.676407821165474488, 1.496050514612049742, 1.352155788975975437 ) ) ;
#150101 = CARTESIAN_POINT ( 'NONE',  ( -7.503547950159405566, 10.84155747757291266, 1.199719254218453823 ) ) ;
#150103 = CARTESIAN_POINT ( 'NONE',  ( -6.071018923869249129, 10.30488218781460574, 0.7998128361456291469 ) ) ;
#150102 = CARTESIAN_POINT ( 'NONE',  ( 4.803764043965432329, -0.6079002506334645339, 2.179255796609281148 ) ) ;
#150104 = CARTESIAN_POINT ( 'NONE',  ( 6.686557493494803772, -2.064527365108769885, -0.4147649638114383475 ) ) ;
#150105 = CARTESIAN_POINT ( 'NONE',  ( -7.587723245503481095, 8.881373870289390737, 1.199719254218452047 ) ) ;
#150106 = CARTESIAN_POINT ( 'NONE',  ( 4.791501694037465953, -1.894250426384593844, 0.8359921707915063394 ) ) ;
#150107 = CARTESIAN_POINT ( 'NONE',  ( 8.594979316059474073, 12.11489407112305372, 1.199719254218450271 ) ) ;
#150108 = CARTESIAN_POINT ( 'NONE',  ( -3.555477883677943599E-14, 2.484375000341469963, 1.570758158831768281 ) ) ;
#150109 = PRODUCT_CONTEXT ( 'NONE', #82292, 'mechanical' ) ;
#150111 = CARTESIAN_POINT ( 'NONE',  ( 2.244641533702110614, 0.4219287677580378926, 1.879577339372063838 ) ) ;
#150110 = CARTESIAN_POINT ( 'NONE',  ( -8.474009703741204547, 9.845098394908269768, -1.199719254218446718 ) ) ;
#150112 = CARTESIAN_POINT ( 'NONE',  ( -3.923105346307911745, 5.670318552149568703, -1.599625672291283607 ) ) ;
#150113 = CARTESIAN_POINT ( 'NONE',  ( 6.491062224718945117, 0.1893930596480186412, 1.960278089617428554 ) ) ;
#150114 = CARTESIAN_POINT ( 'NONE',  ( 5.058600711230250013, 5.074324715956299414, -0.7216878364870458196 ) ) ;
#150115 = CARTESIAN_POINT ( 'NONE',  ( 5.320181785876097358, 6.346852008952179602, 1.110229221197155169 ) ) ;
#150116 = CARTESIAN_POINT ( 'NONE',  ( -4.223528545856940042, 4.886203710709899006, -1.199719254218446718 ) ) ;
#150118 = CARTESIAN_POINT ( 'NONE',  ( 2.180208177693909288, 2.177553952664741388, -0.4384792121874846460 ) ) ;
#150117 = CARTESIAN_POINT ( 'NONE',  ( 0.3168469074051638024, -0.7203255543706194031, -1.994627023381766673 ) ) ;
#150119 = CARTESIAN_POINT ( 'NONE',  ( 3.768672590584824178, -1.415924365303207644, 1.559078948506262385 ) ) ;
#150120 = CARTESIAN_POINT ( 'NONE',  ( -6.129167961829681488, 9.308390501180058507, -1.199719254218452047 ) ) ;
#150121 = CARTESIAN_POINT ( 'NONE',  ( 7.613066949273408213, 8.840665181362512115, -1.199719254218441611 ) ) ;
#150122 = CARTESIAN_POINT ( 'NONE',  ( 0.3790724793553065797, -0.09720884262147008736, 1.858658634516747510 ) ) ;
#150123 = CARTESIAN_POINT ( 'NONE',  ( 6.745345117998789775, 7.828323044875442172, 1.199719254218462483 ) ) ;
#150124 = CARTESIAN_POINT ( 'NONE',  ( -4.218308198147158627, 7.356310275799033960, -0.8477421400144637964 ) ) ;
#150125 = CARTESIAN_POINT ( 'NONE',  ( 4.822949958159288286, 6.649860922651058992, -1.599625672291256295 ) ) ;
#150126 = CARTESIAN_POINT ( 'NONE',  ( -4.773879485787619892, 7.623257595843924150, 1.082531754730549967 ) ) ;
#150127 = CARTESIAN_POINT ( 'NONE',  ( -8.378575743565381373, 8.877352577022161739, 0.7216878364870438212 ) ) ;
#150128 = CARTESIAN_POINT ( 'NONE',  ( 0.9496594531581278309, -1.914679731917130479, 0.9119059213342151082 ) ) ;
#150129 = CARTESIAN_POINT ( 'NONE',  ( -5.855142236255304944, 7.924361590421551860, -1.599625672291271394 ) ) ;
#150131 = CARTESIAN_POINT ( 'NONE',  ( 4.738696794244872557, -1.902450960283699199, -0.4786090228221794307 ) ) ;
#150130 = CARTESIAN_POINT ( 'NONE',  ( 1.225000000000001199, 0.6458333333333310389, -0.7072540797572937077 ) ) ;
#150132 = CARTESIAN_POINT ( 'NONE',  ( 3.397504326804317909, 1.702965868850464082, 1.331369057855802174 ) ) ;
#150133 = CARTESIAN_POINT ( 'NONE',  ( 1.540310226958538475, -1.555040833713853710, 0.9856339240054690087 ) ) ;
#150134 = CARTESIAN_POINT ( 'NONE',  ( -4.026842413655439046, 7.608452276161581374, 0.2328349793435397497 ) ) ;
#150135 = ADVANCED_FACE ( 'NONE', ( #208982 ), #43332, .F. ) ;
#150136 = CARTESIAN_POINT ( 'NONE',  ( -0.6823417656250246877, -1.136458332991911790, 1.181850606188755259 ) ) ;
#150137 = CARTESIAN_POINT ( 'NONE',  ( 4.505614311517684101, -0.7474637548481823934, -1.571778613660354207 ) ) ;
#150138 = CARTESIAN_POINT ( 'NONE',  ( -1.724555757183582561, 15.99999999999538858, -11.68000002332616205 ) ) ;
#150139 = CARTESIAN_POINT ( 'NONE',  ( 4.961921032921539521, 7.772363057508363759, -1.082531754730549078 ) ) ;
#150140 = CARTESIAN_POINT ( 'NONE',  ( -10.45142907045522129, 5.144535043903895932, -5.216774619840575333 ) ) ;
#150141 = CARTESIAN_POINT ( 'NONE',  ( 1.551884642779034262, 0.6273040060550126862, -2.068667048528524344 ) ) ;
#150142 = CARTESIAN_POINT ( 'NONE',  ( 3.638045922354939954, 0.05228986736816390590, -2.015604357568132166 ) ) ;
#150143 = CARTESIAN_POINT ( 'NONE',  ( -9.286972035236626510, 11.85788667924133399, -1.443375672974058777 ) ) ;
#150144 = CARTESIAN_POINT ( 'NONE',  ( 1.323354039402934390, -0.05256100377049736927, 2.161234000603563299 ) ) ;
#150145 = CARTESIAN_POINT ( 'NONE',  ( 3.959811223838666905, 1.956698650606549350, -0.2402693447622703815 ) ) ;
#150146 = AXIS2_PLACEMENT_3D ( 'NONE', #34242, #211923, #33184 ) ;
#150147 = EDGE_CURVE ( 'NONE', #22322, #204026, #186039, .T. ) ;
#150148 = CARTESIAN_POINT ( 'NONE',  ( 6.509000000000051855, 1.248119779622055336, 2.213941609938009591 ) ) ;
#150149 = CARTESIAN_POINT ( 'NONE',  ( 3.140110198738320424, 0.4743784485543530716, 1.883105278476588706 ) ) ;
#150152 = ORIENTED_EDGE ( 'NONE', *, *, #932, .F. ) ;
#150151 = CARTESIAN_POINT ( 'NONE',  ( -4.828112100242303306, 4.805421336470338645, -0.7216878364870338292 ) ) ;
#150150 = CARTESIAN_POINT ( 'NONE',  ( -8.636180661780658241, 12.05899929117736846, -1.082531754730543083 ) ) ;
#150154 = EDGE_CURVE ( 'NONE', #26009, #28024, #116618, .T. ) ;
#150153 = CARTESIAN_POINT ( 'NONE',  ( -5.921879234118920365, 10.13088588310589699, 0.000000000000000000 ) ) ;
#150155 = CARTESIAN_POINT ( 'NONE',  ( 4.947799714344386146, 4.737130853015369958, -0.7998128361456481317 ) ) ;
#150156 = CARTESIAN_POINT ( 'NONE',  ( -3.332271893908731464, 7.109677319527304640, -0.7998128361456481317 ) ) ;
#150158 = ORIENTED_EDGE ( 'NONE', *, *, #185760, .T. ) ;
#150157 = CARTESIAN_POINT ( 'NONE',  ( -6.252245114557387851, 7.323316050852266557, -1.199719254218453823 ) ) ;
#150159 = CARTESIAN_POINT ( 'NONE',  ( -8.283668667825340393, 12.60810451253083997, 0.7216878364870458196 ) ) ;
#150160 = CARTESIAN_POINT ( 'NONE',  ( 6.317414003067519879, -0.2912348092876380079, 2.289091032272353221 ) ) ;
#150161 = CARTESIAN_POINT ( 'NONE',  ( 1.642778471875001811, -3.492708332855375630, 2.845375778867859751 ) ) ;
#150162 = CARTESIAN_POINT ( 'NONE',  ( 5.418788444413384475, -1.423528547644649755, 1.350099487149841071 ) ) ;
#150163 = CARTESIAN_POINT ( 'NONE',  ( 1.494767762416523871, -2.000856930885573259, 0.2496086726550551527 ) ) ;
#150164 = VERTEX_POINT ( 'NONE', #175457 ) ;
#150165 = CARTESIAN_POINT ( 'NONE',  ( 3.485668972010677269, -0.6104075878305641467, 2.027481811383638810 ) ) ;
#150166 = CARTESIAN_POINT ( 'NONE',  ( 0.7499999999999902300, 3.514583334016149863, 1.299038105676669330 ) ) ;
#150168 = CARTESIAN_POINT ( 'NONE',  ( -4.543954038874438162, 8.453030145328826350, 1.040834085586084257E-14 ) ) ;
#150167 = CARTESIAN_POINT ( 'NONE',  ( 0.000000000000000000, 0.5000000000000004441, 0.000000000000000000 ) ) ;
#150169 = CARTESIAN_POINT ( 'NONE',  ( 3.978315823851843014, -0.1823813840945518738, -1.832081410093854501 ) ) ;
#150170 = ORIENTED_EDGE ( 'NONE', *, *, #60919, .T. ) ;
#150171 = UNCERTAINTY_MEASURE_WITH_UNIT (LENGTH_MEASURE( 1.000000000000000082E-05 ), #7069, 'distance_accuracy_value', 'NONE');
#150172 = CARTESIAN_POINT ( 'NONE',  ( -6.970863535720637216, 11.28442455831609337, 0.7998128361456481317 ) ) ;
#150173 = DIRECTION ( 'NONE',  ( 0.000000000000000000, 1.000000000000000000, 0.000000000000000000 ) ) ;
#150174 = CARTESIAN_POINT ( 'NONE',  ( 5.449516625918088053, -1.916229881892789866, 0.9086369058012438993 ) ) ;
#150175 = DIRECTION ( 'NONE',  ( 0.000000000000000000, 1.000000000000000000, 0.000000000000000000 ) ) ;
#150176 = CARTESIAN_POINT ( 'NONE',  ( 5.262536180398716290, 9.291375977107183104, -0.7998128361456291469 ) ) ;
#150177 = CARTESIAN_POINT ( 'NONE',  ( 5.905559377550752664, -0.5051061836833131702, 1.997775138168448761 ) ) ;
#150180 = CARTESIAN_POINT ( 'NONE',  ( 2.261056740009634414, 1.805359621025553363, -0.3608742708730780513 ) ) ;
#150179 = CARTESIAN_POINT ( 'NONE',  ( 1.011883965753940018, 1.859189825682316277, -0.08597224477241424689 ) ) ;
#150178 = DIRECTION ( 'NONE',  ( 0.000000000000000000, 0.000000000000000000, 1.000000000000000000 ) ) ;
#150181 = CARTESIAN_POINT ( 'NONE',  ( 9.610031953988080744, 10.10612545594124967, -0.7998128361456281477 ) ) ;
#150182 = CARTESIAN_POINT ( 'NONE',  ( 4.875256056531546811, 6.897355949014277954, -1.450507286032868270 ) ) ;
#150183 = CARTESIAN_POINT ( 'NONE',  ( -5.921879234118920365, 10.13088588310589699, 0.000000000000000000 ) ) ;
#150184 = CARTESIAN_POINT ( 'NONE',  ( 1.224999999999951017, 2.166666667349502085, 0.7072540797572777205 ) ) ;
#150185 = CARTESIAN_POINT ( 'NONE',  ( 1.928631425534212074, 1.268998755960360603, -1.805353087401928569 ) ) ;
#150186 = CARTESIAN_POINT ( 'NONE',  ( 5.097078980560620920, 1.884938936817718069, -1.250935519564094767 ) ) ;
#150187 = CARTESIAN_POINT ( 'NONE',  ( -8.188761592974058701, 8.655902734665618325, -0.7216878364870278340 ) ) ;
#150188 = CARTESIAN_POINT ( 'NONE',  ( 5.150580392983738598, 1.786086171955153068, 0.3018458199737662495 ) ) ;
#150189 = CARTESIAN_POINT ( 'NONE',  ( 5.331221607142452967, -1.514317160175217447, -1.173313937468897672 ) ) ;
#150190 = CARTESIAN_POINT ( 'NONE',  ( -1.364683531249997417, 5.071875000341417916, 1.214306433183764966E-14 ) ) ;
#150191 = CARTESIAN_POINT ( 'NONE',  ( 4.346526858336821952, 0.5246154692373095063, 1.900329053005628044 ) ) ;
#150192 = CARTESIAN_POINT ( 'NONE',  ( 5.594569530875262764, -0.4557361262383100020, -1.814172972432124720 ) ) ;
#150193 = CARTESIAN_POINT ( 'NONE',  ( 5.037489322368606359, 1.736649509538616964, -0.6695082933049227858 ) ) ;
#150194 = CARTESIAN_POINT ( 'NONE',  ( -0.6823417656249969321, 5.717708333674756283, -1.181850606188749264 ) ) ;
#150195 = CARTESIAN_POINT ( 'NONE',  ( 5.032005376881601322, 0.9078957314892305286, -1.519088338465144128 ) ) ;
#150196 = DIRECTION ( 'NONE',  ( 0.000000000000000000, 1.000000000000000000, -8.546850786086437571E-32 ) ) ;
#150198 = CARTESIAN_POINT ( 'NONE',  ( 2.139418596640904280, -1.880839966478216052, 0.9477614987608102837 ) ) ;
#150197 = CARTESIAN_POINT ( 'NONE',  ( -3.917943204224928699, 4.633650495426258509, -1.082531754730548412 ) ) ;
#150199 = CARTESIAN_POINT ( 'NONE',  ( 8.886479618753304166, 12.45497775759917758, -1.199719254218446718 ) ) ;
#150201 = CARTESIAN_POINT ( 'NONE',  ( -1.180180411290526976, 2.825872823607642914, -0.7749999999999979128 ) ) ;
#150200 = CARTESIAN_POINT ( 'NONE',  ( 1.426546532658254263, 7.396047039057247474, -4.272878514717298515 ) ) ;
#150202 = CARTESIAN_POINT ( 'NONE',  ( 3.603867943843573673, 1.538443694073919898, 1.459757404076333698 ) ) ;
#150203 = CARTESIAN_POINT ( 'NONE',  ( 1.933859055862125809, -1.958050917679872160, 0.4949566823095867263 ) ) ;
#150204 = CARTESIAN_POINT ( 'NONE',  ( 1.364683531249988535, 1.613541667008084879, 0.7879004041258500513 ) ) ;
#150205 = CARTESIAN_POINT ( 'NONE',  ( 6.720655732516688019, 6.039915720534646759, 2.321169117395345705 ) ) ;
#150206 = CARTESIAN_POINT ( 'NONE',  ( 3.876741858503734761, 6.610283703974623393, 1.199719254218462483 ) ) ;
#150207 = ORIENTED_EDGE ( 'NONE', *, *, #68027, .F. ) ;
#150208 = CARTESIAN_POINT ( 'NONE',  ( 2.319794969891198821, -2.097318901067245722, 0.5227781780692899449 ) ) ;
#150209 = DIRECTION ( 'NONE',  ( 1.544526636936600361E-14, -1.000000000000000000, 1.522060196430166414E-14 ) ) ;
#150212 = CARTESIAN_POINT ( 'NONE',  ( -3.939566984407580907, 8.987080315575658673, -0.7749999999999979128 ) ) ;
#150211 = CARTESIAN_POINT ( 'NONE',  ( 11.94105722165070560, 10.07417237917041142, -1.187919369849492757 ) ) ;
#150210 = CARTESIAN_POINT ( 'NONE',  ( 4.655245641445829641, 6.524482229810530498, 1.599625672291269396 ) ) ;
#150213 = CARTESIAN_POINT ( 'NONE',  ( 0.000000000000000000, 2.000000000000001776, 10.25000000000000000 ) ) ;
#150214 = CARTESIAN_POINT ( 'NONE',  ( -7.886602582589937960, -6.765616048178459963, 7.668547801473422965 ) ) ;
#150215 = CARTESIAN_POINT ( 'NONE',  ( -7.592202833972775622, 8.920286730132099606, 1.082531754730558626 ) ) ;
#150216 = CARTESIAN_POINT ( 'NONE',  ( 0.9783777488623355278, -2.139296967303818686, -0.4750931833387496694 ) ) ;
#150217 = CARTESIAN_POINT ( 'NONE',  ( 0.2089193878861559939, 7.199905994521539121, 1.991006660531130512 ) ) ;
#150219 = CARTESIAN_POINT ( 'NONE',  ( -1.364683531250014514, 12.33854166700805877, -0.7879004041258335089 ) ) ;
#150218 = CARTESIAN_POINT ( 'NONE',  ( 1.850798253084064537, 0.7104643512030085484, 2.148151574381700790 ) ) ;
#150220 = CARTESIAN_POINT ( 'NONE',  ( -7.974166903131914452, 12.45494515362926435, -0.7998128361456281477 ) ) ;
#150221 = EDGE_CURVE ( 'NONE', #33663, #105242, #23141, .T. ) ;
#150222 = CARTESIAN_POINT ( 'NONE',  ( 4.434779938697545276, -1.616694733667634942, 1.205040202231235869 ) ) ;
#150223 = CARTESIAN_POINT ( 'NONE',  ( -5.409340101728186134, 5.413244328212063472, 0.7216878364870317197 ) ) ;
#150224 = CARTESIAN_POINT ( 'NONE',  ( 0.6823417656249882723, 2.738541667008084879, -1.181850606188749264 ) ) ;
#150225 = CARTESIAN_POINT ( 'NONE',  ( 4.637820276784100137, 8.319831082953612622, -0.4078742439591088731 ) ) ;
#150226 = CARTESIAN_POINT ( 'NONE',  ( 0.7500000000000006661, 10.91666666666666430, -1.299038105676657340 ) ) ;
#150227 = CARTESIAN_POINT ( 'NONE',  ( 8.014278199453778839, 8.522615118883788199, 0.000000000000000000 ) ) ;
#150228 = CARTESIAN_POINT ( 'NONE',  ( 3.180641231044952555, -0.1265111898236283006, -1.765250312072360162 ) ) ;
#150229 = CARTESIAN_POINT ( 'NONE',  ( 6.510767885691055135, 1.639592601025055885, -1.477219212978691409 ) ) ;
#150230 = ORIENTED_EDGE ( 'NONE', *, *, #49562, .F. ) ;
#150231 = CARTESIAN_POINT ( 'NONE',  ( -5.855142236255304944, 7.924361590421551860, -1.599625672291271394 ) ) ;
#150232 = CARTESIAN_POINT ( 'NONE',  ( 5.642203898613793456, 0.8197873783117490820, 1.842442240159094080 ) ) ;
#150233 = ORIENTED_EDGE ( 'NONE', *, *, #191848, .F. ) ;
#150234 = CARTESIAN_POINT ( 'NONE',  ( 2.922558825391399662, 1.760836971185793187, 0.6318509464167121337 ) ) ;
#150235 = EDGE_CURVE ( 'NONE', #10132, #54906, #23388, .T. ) ;
#150236 = CARTESIAN_POINT ( 'NONE',  ( 2.237250781069185734, -0.09733102107959035187, -2.068066387140480522 ) ) ;
#150237 = CIRCLE ( 'NONE', #70575, 0.07999999999999994615 ) ;
#150238 = CARTESIAN_POINT ( 'NONE',  ( -6.495764994278840021, 8.671754808115688107, 1.443375672974064550 ) ) ;
#150239 = CARTESIAN_POINT ( 'NONE',  ( 1.968876373762207255, -1.476028252698018628, 1.215921256797661609 ) ) ;
#150240 = CARTESIAN_POINT ( 'NONE',  ( 1.500000000000001332, 9.625000000000001776, 0.000000000000000000 ) ) ;
#150241 = CARTESIAN_POINT ( 'NONE',  ( -10.39336823037077195, 4.932734307774878424, -5.330979603150785451 ) ) ;
#150242 = DIRECTION ( 'NONE',  ( 0.000000000000000000, 1.000000000000000000, 0.000000000000000000 ) ) ;
#150243 = B_SPLINE_CURVE_WITH_KNOTS ( 'NONE', 3,
 ( #122018, #154438, #71014, #105715 ),
 .UNSPECIFIED., .F., .F.,
 ( 4, 4 ),
 ( 0.000000000000000000, 1.000000000000000000 ),
 .UNSPECIFIED. ) ;
#150244 = CARTESIAN_POINT ( 'NONE',  ( -0.6823417656250212460, 4.113541667008085767, 1.181850606188767472 ) ) ;
#150245 = CARTESIAN_POINT ( 'NONE',  ( 0.6328886395040033142, 1.767934563615305654, 0.7296191750566642931 ) ) ;
#150246 = CARTESIAN_POINT ( 'NONE',  ( 5.722950238744200391, 7.770137593325314285, 1.443375672974065660 ) ) ;
#150247 = CARTESIAN_POINT ( 'NONE',  ( 1.697631272820496307, -1.418720726069604865, -1.355276769646639901 ) ) ;
#150248 = EDGE_CURVE ( 'NONE', #87431, #12920, #101273, .T. ) ;
#150249 = CARTESIAN_POINT ( 'NONE',  ( 0.2454708137151571101, -1.954895187565863779, -0.4925657318226167591 ) ) ;
#150250 = CARTESIAN_POINT ( 'NONE',  ( -5.743814354044916470, 6.730146830254374990, -1.199719254218453823 ) ) ;
#150251 = CARTESIAN_POINT ( 'NONE',  ( 4.957343421279005291, -1.817532610912236724, 1.092287347377165707 ) ) ;
#150253 = CARTESIAN_POINT ( 'NONE',  ( -11.52114515671133610, 8.081606464056415362, 2.192706985476595261 ) ) ;
#150252 = CARTESIAN_POINT ( 'NONE',  ( 9.610031953988080744, 10.10612545594124967, -0.7998128361456281477 ) ) ;
#150254 = CARTESIAN_POINT ( 'NONE',  ( 6.204366038997092936, -0.7071694579776456324, -1.840334891991159738 ) ) ;
#150255 = CARTESIAN_POINT ( 'NONE',  ( -1.364683531250012516, 2.238541667008087988, -0.7879004041258289570 ) ) ;
#150256 = CARTESIAN_POINT ( 'NONE',  ( 1.476815932985692026, -1.420704281710112316, 1.426639689446000281 ) ) ;
#150257 = EDGE_LOOP ( 'NONE', ( #108385, #209610, #180067, #3390, #141415 ) ) ;
#150259 = CARTESIAN_POINT ( 'NONE',  ( 1.406030203601447592, -1.179493747730875342, -1.758069577626440116 ) ) ;
#150258 = CARTESIAN_POINT ( 'NONE',  ( -7.212574532790102744, 8.477387045419011002, -1.082531754730550855 ) ) ;
#150260 = CARTESIAN_POINT ( 'NONE',  ( 11.40211703457567971, 7.516167754840261672, -3.765886988443341021 ) ) ;
#150261 = CARTESIAN_POINT ( 'NONE',  ( 2.822784111170244525, -1.429543836668966561, 1.497820115680066344 ) ) ;
#150262 = CARTESIAN_POINT ( 'NONE',  ( 5.337069745634900997, 6.255611453776062980, 1.199719254218452047 ) ) ;
#150263 = CARTESIAN_POINT ( 'NONE',  ( 5.923986774528332333, 5.876015756563318426, -0.7998128361456481317 ) ) ;
#150264 = VERTEX_POINT ( 'NONE', #180768 ) ;
#150266 = CARTESIAN_POINT ( 'NONE',  ( 4.650610384687404952, 5.384465856012134566, 1.199719254218462483 ) ) ;
#150265 = CARTESIAN_POINT ( 'NONE',  ( 4.294928614669782263, 1.678954898789623673, 1.245530301124315953 ) ) ;
#150269 = ORIENTED_EDGE ( 'NONE', *, *, #127920, .T. ) ;
#150268 = CARTESIAN_POINT ( 'NONE',  ( 2.420317109208899531, -0.6946167411978272366, -1.673203699974361580 ) ) ;
#150267 = CARTESIAN_POINT ( 'NONE',  ( 3.891465932158610030, 1.322013910284997262, 1.259209046625270556 ) ) ;
#150270 = CARTESIAN_POINT ( 'NONE',  ( 6.410767893487317792, 1.638320036227768783, -1.478771730184471611 ) ) ;
#150271 = CARTESIAN_POINT ( 'NONE',  ( 9.802633114045661955, 10.59323031708064455, 5.525202073719254869 ) ) ;
#150272 = CARTESIAN_POINT ( 'NONE',  ( 5.368293279414073638, 1.083412401764087374, 1.922438065789177308 ) ) ;
#150273 = CARTESIAN_POINT ( 'NONE',  ( -1.364683531250000748, 8.921875000341403350, 0.000000000000000000 ) ) ;
#150274 = CARTESIAN_POINT ( 'NONE',  ( 4.195896582043898704, 1.251535281948525036, 1.445917311372606262 ) ) ;
#150275 = CARTESIAN_POINT ( 'NONE',  ( -2.937312835655025101, 6.578615408239493867, 1.040834085586084257E-14 ) ) ;
#150276 = CARTESIAN_POINT ( 'NONE',  ( 6.283314124929436417, 9.417951348137970413, -1.199719254218440723 ) ) ;
#150277 = CARTESIAN_POINT ( 'NONE',  ( -4.957638175832625493E-14, 0.8593750003414141192, -1.570758158831808249 ) ) ;
#150278 = CARTESIAN_POINT ( 'NONE',  ( 5.463572716182834910, 5.476515711742504067, 0.7216878364870317197 ) ) ;
#150279 = CARTESIAN_POINT ( 'NONE',  ( -11.86145016429273724, 12.59412591486745114, 1.099999999999996980 ) ) ;
#150280 = CARTESIAN_POINT ( 'NONE',  ( 8.762672035042523788, 13.53725231859170997, -8.198939407311630845 ) ) ;
#150281 = CARTESIAN_POINT ( 'NONE',  ( 11.07790593930098311, 11.29999999999999893, -0.7000000000000009548 ) ) ;
#150282 = EDGE_LOOP ( 'NONE', ( #211758, #76502, #205403, #104717 ) ) ;
#150283 = ORIENTED_EDGE ( 'NONE', *, *, #80621, .T. ) ;
#150284 = DIRECTION ( 'NONE',  ( 0.000000000000000000, 0.000000000000000000, 1.000000000000000000 ) ) ;
#150285 = ADVANCED_FACE ( 'NONE', ( #84337 ), #109832, .T. ) ;
#150286 = CARTESIAN_POINT ( 'NONE',  ( 3.919104170388473030, -0.1403237101727794756, 1.865361397874479632 ) ) ;
#150287 = CARTESIAN_POINT ( 'NONE',  ( 7.452141709366786770, 8.723195411463290583, 1.199719254218452047 ) ) ;
#150288 = DIRECTION ( 'NONE',  ( -1.000000000000000000, 0.000000000000000000, 0.000000000000000000 ) ) ;
#150290 = CARTESIAN_POINT ( 'NONE',  ( -6.670248388243482651, 9.765411638717282017, 1.082531754730548412 ) ) ;
#150289 = CIRCLE ( 'NONE', #101734, 0.08000000000000020983 ) ;
#150291 = CARTESIAN_POINT ( 'NONE',  ( 5.660692828905515839, 6.562895374266609849, -1.199719254218445830 ) ) ;
#150292 = CARTESIAN_POINT ( 'NONE',  ( 0.4089589639980686919, -1.585120765669449261, 1.168626392425928584 ) ) ;
#150293 = CARTESIAN_POINT ( 'NONE',  ( 2.776970437579088014, 1.727991955821889025, -1.039012595151635354 ) ) ;
#150294 = CARTESIAN_POINT ( 'NONE',  ( -9.657485491635913633, 10.16148791653038330, 1.040834085586084257E-14 ) ) ;
#150295 = CARTESIAN_POINT ( 'NONE',  ( 5.773793314573267388, 7.829454515125894964, 1.599625672291268286 ) ) ;
#150296 = SURFACE_STYLE_FILL_AREA ( #38670 ) ;
#150297 = CARTESIAN_POINT ( 'NONE',  ( 2.642740014504705748, -1.821389600533462216, 1.218302608185666491 ) ) ;
#150298 = CARTESIAN_POINT ( 'NONE',  ( 6.147073579019600054, -1.539581890156189292, 0.9809480439507823890 ) ) ;
#150299 = CARTESIAN_POINT ( 'NONE',  ( -3.436101866059630527, 6.096203712789787232, 1.199719254218462483 ) ) ;
#150300 = AXIS2_PLACEMENT_3D ( 'NONE', #65504, #143635, #210711 ) ;
#150301 = CARTESIAN_POINT ( 'NONE',  ( 3.919715808126649659, 7.587102519540811940, 0.000000000000000000 ) ) ;
#150302 = CARTESIAN_POINT ( 'NONE',  ( 7.639129486296027061, 10.99973593639901814, 1.199719254218460707 ) ) ;
#150303 = CARTESIAN_POINT ( 'NONE',  ( 4.864678189204997949, 4.569879397027603929, 0.7998128361456341429 ) ) ;
#150304 = CARTESIAN_POINT ( 'NONE',  ( 5.831415467653547680, 8.857049574687536619, -1.082531754730548412 ) ) ;
#150305 = EDGE_LOOP ( 'NONE', ( #120378, #111802, #87614 ) ) ;
#150307 = CARTESIAN_POINT ( 'NONE',  ( 0.2584475630193752149, 2.007833436562710183, 0.1460894178599257687 ) ) ;
#150306 = CARTESIAN_POINT ( 'NONE',  ( 3.983814121021773680, -1.821778379405362136, -0.2661574599523569007 ) ) ;
#150308 = CARTESIAN_POINT ( 'NONE',  ( 3.005512134316370432, 2.280722703800378337, 0.2841129622813722277 ) ) ;
#150310 = CARTESIAN_POINT ( 'NONE',  ( 0.8833916088089890373, -1.769421289247067097, 0.5767519331581376640 ) ) ;
#150309 = CARTESIAN_POINT ( 'NONE',  ( 0.000000000000000000, -0.5000000000000004441, 0.000000000000000000 ) ) ;
#150311 = CARTESIAN_POINT ( 'NONE',  ( 3.475000000000000533, -0.5250000000000011324, 0.000000000000000000 ) ) ;
#150312 = CARTESIAN_POINT ( 'NONE',  ( -4.416205349749324327, 6.175325546172740765, 1.599625672291267398 ) ) ;
#150313 = DIRECTION ( 'NONE',  ( 0.000000000000000000, 0.000000000000000000, 1.000000000000000000 ) ) ;
#150314 = CARTESIAN_POINT ( 'NONE',  ( 4.570513122935188299, 0.7371126809179430195, 1.764830652192488580 ) ) ;
#150315 = CARTESIAN_POINT ( 'NONE',  ( -9.508345801885592863, 9.987491611821676329, 0.7998128361456462443 ) ) ;
#150316 = CARTESIAN_POINT ( 'NONE',  ( 6.326190869690321961, 6.855918622363850190, 0.6739092513716876676 ) ) ;
#150317 = CARTESIAN_POINT ( 'NONE',  ( -5.153507786970262572, 9.026526494858359229, -0.7216878364870338292 ) ) ;
#150319 = CARTESIAN_POINT ( 'NONE',  ( 2.289737743334671283, -0.8020533187339595749, 1.690132462187944107 ) ) ;
#150318 = CARTESIAN_POINT ( 'NONE',  ( 3.737900851971903915, 2.080878125540788215, 0.2026709130291924343 ) ) ;
#150320 = CARTESIAN_POINT ( 'NONE',  ( 6.466876084038451822, 10.48851316477946582, 1.040834085586084257E-14 ) ) ;
#150321 = CARTESIAN_POINT ( 'NONE',  ( -1.201851678989727383E-14, 5.759375000341417028, -1.575800808251661023 ) ) ;
#150322 = CARTESIAN_POINT ( 'NONE',  ( 5.425302022954732628, -1.172690680311109901, -1.419496581506813904 ) ) ;
#150323 = CARTESIAN_POINT ( 'NONE',  ( 5.332434488876471868, 5.115595079977664383, 0.7998128361456341429 ) ) ;
#150324 = CARTESIAN_POINT ( 'NONE',  ( 11.86145016429272836, 19.00000000000000000, -1.180000000000002158 ) ) ;
#150325 = CARTESIAN_POINT ( 'NONE',  ( 4.213312296666638979, -0.2916954692788272796, 1.699858598931931919 ) ) ;
#150326 = CARTESIAN_POINT ( 'NONE',  ( -5.364222332501225488, 9.410009821226765325, 0.7998128361456481317 ) ) ;
#150327 = CARTESIAN_POINT ( 'NONE',  ( 6.568967528192747096, -2.015767819289843388, -0.8987472251835016968 ) ) ;
#150328 = CARTESIAN_POINT ( 'NONE',  ( 6.983263157960370116, 1.251666756963093041, 2.167287073222202931 ) ) ;
#150329 = SURFACE_SIDE_STYLE ('',( #1896 ) ) ;
#150330 = CARTESIAN_POINT ( 'NONE',  ( 5.155217109558853039, 1.808899791667990753, -1.200326510068568497 ) ) ;
#150331 = CARTESIAN_POINT ( 'NONE',  ( 2.807047293222181494, 1.542382716246639474, 0.9765254425028799812 ) ) ;
#150333 = CARTESIAN_POINT ( 'NONE',  ( 6.122275928298587466, 2.094602363090028785, 0.3085360351358697462 ) ) ;
#150332 = B_SPLINE_CURVE_WITH_KNOTS ( 'NONE', 3,
 ( #125775, #112706, #59619, #110576, #11928, #210117, #113775, #79061 ),
 .UNSPECIFIED., .F., .F.,
 ( 4, 2, 2, 4 ),
 ( 0.000000000000000000, 0.0002889198933005425896, 0.0005778397866010851792, 0.001155679573202170358 ),
 .UNSPECIFIED. ) ;
#150334 = ORIENTED_EDGE ( 'NONE', *, *, #164392, .F. ) ;
#150336 = CARTESIAN_POINT ( 'NONE',  ( -1.364683531249997417, 2.571875000341422357, 1.214306433183764966E-14 ) ) ;
#150335 = CARTESIAN_POINT ( 'NONE',  ( 6.075753635015332499, -1.229876075327457130, 1.934346496684937966 ) ) ;
#150337 = CARTESIAN_POINT ( 'NONE',  ( 7.404724451357931336, 11.79059562655963056, 0.7998128361456462443 ) ) ;
#150338 = CARTESIAN_POINT ( 'NONE',  ( 1.119968162728638417, -0.5116716972351254000, 2.057716464106795318 ) ) ;
#150339 = CARTESIAN_POINT ( 'NONE',  ( -4.121315508874262790, 6.791656612786516334, -1.082531754730549967 ) ) ;
#150340 = DIRECTION ( 'NONE',  ( -1.224646799147353207E-16, 0.000000000000000000, -1.000000000000000000 ) ) ;
#150341 = CARTESIAN_POINT ( 'NONE',  ( -6.087247782411500552, 7.164505836643929371, 1.082531754730549967 ) ) ;
#150342 = CARTESIAN_POINT ( 'NONE',  ( 6.262575984712966282, -0.7736541179628317888, -2.028742479192620518 ) ) ;
#150344 = CARTESIAN_POINT ( 'NONE',  ( -1.500000000000008216, 12.53125000068279427, 3.469446951953614189E-15 ) ) ;
#150343 = DIRECTION ( 'NONE',  ( 0.000000000000000000, 0.000000000000000000, -1.000000000000000000 ) ) ;
#150346 = EDGE_LOOP ( 'NONE', ( #191597, #119676, #154087, #56108 ) ) ;
#150345 = CARTESIAN_POINT ( 'NONE',  ( 1.489269531296941507, -2.110695925841240772, -0.6924467157797905559 ) ) ;
#150347 = CARTESIAN_POINT ( 'NONE',  ( 5.942029771888944545, -1.730864577151491890, -1.034168155301495862 ) ) ;
#150349 = CARTESIAN_POINT ( 'NONE',  ( 4.030177592043080459, 1.141696479982070578, 1.717582018908659025 ) ) ;
#150348 = CARTESIAN_POINT ( 'NONE',  ( 4.039439701867726384, 6.800097854565950506, 1.199719254218462483 ) ) ;
#150351 = CARTESIAN_POINT ( 'NONE',  ( -3.474999999999998312, -3.820833333333332416, 2.006292185433951047 ) ) ;
#150350 = CARTESIAN_POINT ( 'NONE',  ( 7.679767667498067496, 7.924426798361372093, 0.000000000000000000 ) ) ;
#150352 = CARTESIAN_POINT ( 'NONE',  ( 6.363572996767764778, 8.517530811019446091, -1.599625672291283607 ) ) ;
#150353 = CARTESIAN_POINT ( 'NONE',  ( -3.285556943749998737, -3.667708332855377673, 1.896917185911908499 ) ) ;
#150354 = CARTESIAN_POINT ( 'NONE',  ( -0.4019237886466871523, 12.69866454968462754, -1.499999999999998668 ) ) ;
#150355 = CARTESIAN_POINT ( 'NONE',  ( 0.3575176574102476579, 2.067590324638542310, -0.3087094068163088179 ) ) ;
#150356 = CARTESIAN_POINT ( 'NONE',  ( 4.483046177357690176, -2.016033783801042034, -0.04667830911464498911 ) ) ;
#150357 = CARTESIAN_POINT ( 'NONE',  ( 4.669393045487420402, 1.064170941109745305, 1.502380130741477693 ) ) ;
#150358 = EDGE_CURVE ( 'NONE', #140091, #97721, #157693, .T. ) ;
#150359 = CARTESIAN_POINT ( 'NONE',  ( 3.669453130792974971, 7.432779085900453886, 1.040834085586084257E-14 ) ) ;
#150360 = CARTESIAN_POINT ( 'NONE',  ( 0.9028307623185973796, 1.406233313734496448, 0.9983791803314099322 ) ) ;
#150361 = DIRECTION ( 'NONE',  ( -0.000000000000000000, -1.000000000000000000, -0.000000000000000000 ) ) ;
#150362 = CARTESIAN_POINT ( 'NONE',  ( 0.3878286276588240877, -0.7819352795844608517, -2.161732420081037720 ) ) ;
#150363 = CARTESIAN_POINT ( 'NONE',  ( -4.954615070790188369, 7.867802451642154082, -1.199719254218452047 ) ) ;
#150364 = CARTESIAN_POINT ( 'NONE',  ( 1.388340239569575640, -1.017395381511316810, 2.020837998375684563 ) ) ;
#150365 = CARTESIAN_POINT ( 'NONE',  ( 2.473383067358714715, 0.1024098097114657241, -2.103702895048992882 ) ) ;
#150366 = CARTESIAN_POINT ( 'NONE',  ( -4.664887371553763096, 7.600063145858131364, -1.199719254218453823 ) ) ;
#150367 = CARTESIAN_POINT ( 'NONE',  ( 6.449928391799196525, 8.548002428564306143, -1.599625672291262513 ) ) ;
#150368 = CARTESIAN_POINT ( 'NONE',  ( 6.007671464186834065, 7.141943142040370063, 1.082531754730549967 ) ) ;
#150369 = CARTESIAN_POINT ( 'NONE',  ( 6.406249999940950346, 1.895863741710943406, -0.7852924748303196090 ) ) ;
#150370 = CARTESIAN_POINT ( 'NONE',  ( -6.898401231254901234, 6.942556279419168419, -0.7998128361456291469 ) ) ;
#150371 = CARTESIAN_POINT ( 'NONE',  ( -1.500000000000013101, 2.420833333333359150, 0.8660254037844403729 ) ) ;
#150372 = CARTESIAN_POINT ( 'NONE',  ( -5.135841261478327979, 4.886236314679810455, 0.7998128361456341429 ) ) ;
#150373 = CARTESIAN_POINT ( 'NONE',  ( 5.308899460236623291, -0.5399372957704140497, -2.154654435841397930 ) ) ;
#150374 = CARTESIAN_POINT ( 'NONE',  ( 3.433693710695666201, 0.9853049363134911420, -1.957518807868402044 ) ) ;
#150375 = CARTESIAN_POINT ( 'NONE',  ( -5.331380718671772101, 7.243030143248949670, -1.599625672291256295 ) ) ;
#150376 = CARTESIAN_POINT ( 'NONE',  ( -3.902768115887413014, 5.646591783325653147, -1.599625672291283607 ) ) ;
#150377 = CARTESIAN_POINT ( 'NONE',  ( 0.6823417656249899377, 3.926041667008085767, -1.181850606188754593 ) ) ;
#150378 = CARTESIAN_POINT ( 'NONE',  ( 6.890000000000009450, -0.01081285896028030651, 2.279840171838913854 ) ) ;
#150379 = CARTESIAN_POINT ( 'NONE',  ( -5.178851490740209229, 7.065079377328788546, 1.443375672974064550 ) ) ;
#150380 = CARTESIAN_POINT ( 'NONE',  ( 5.959260761812961604, -1.790568634313693730, 1.135864312162476297 ) ) ;
#150381 = CARTESIAN_POINT ( 'NONE',  ( -7.268579750702160780, 8.613002809641560731, -1.082531754730549967 ) ) ;
#150382 = ORIENTED_EDGE ( 'NONE', *, *, #58928, .T. ) ;
#150384 = CARTESIAN_POINT ( 'NONE',  ( 6.139563164240942506, -1.562336469324271837, -1.494251390645913613 ) ) ;
#150383 = CARTESIAN_POINT ( 'NONE',  ( -4.638297949650955765, 8.425448351319163365, 0.7216878364870267237 ) ) ;
#150385 = CARTESIAN_POINT ( 'NONE',  ( 5.854423403002611437, 5.724582146458163656, 1.040834085586084257E-14 ) ) ;
#150386 = CARTESIAN_POINT ( 'NONE',  ( 6.181194517112824194, 1.274813594131599226, 1.328792456347933637 ) ) ;
#150387 = UNCERTAINTY_MEASURE_WITH_UNIT (LENGTH_MEASURE( 1.000000000000000082E-05 ), #171936, 'distance_accuracy_value', 'NONE');
#150388 = CARTESIAN_POINT ( 'NONE',  ( 1.224999999999990985, 0.9166666673494643369, 0.7072540797572697269 ) ) ;
#150389 = CARTESIAN_POINT ( 'NONE',  ( 0.6823417656249899377, 3.155208333674754062, 1.181850606188765695 ) ) ;
#150390 = CARTESIAN_POINT ( 'NONE',  ( 1.118268200169919568, -0.04383651085794643132, 1.740047355671838547 ) ) ;
#150391 = FACE_OUTER_BOUND ( 'NONE', #77139, .T. ) ;
#150392 = CARTESIAN_POINT ( 'NONE',  ( -0.1501718367240184870, 8.265200931437576060, 1.995665264648829096 ) ) ;
#150393 = CARTESIAN_POINT ( 'NONE',  ( 10.37617649292455724, 9.136187099972529424, -6.038418756994051506 ) ) ;
#150394 = CARTESIAN_POINT ( 'NONE',  ( 5.805597153138060129, -0.5296426447994294628, 2.095691122003799478 ) ) ;
#150395 = CIRCLE ( 'NONE', #60393, 2.025000000000006573 ) ;
#150396 = CARTESIAN_POINT ( 'NONE',  ( -3.867100128395853709, 5.534702787927018974, -1.599625672291256295 ) ) ;
#150397 = CARTESIAN_POINT ( 'NONE',  ( -8.337901282280023807, 8.829899038855916871, 0.7216878364870438212 ) ) ;
#150398 = CARTESIAN_POINT ( 'NONE',  ( 4.329101982860062314, 0.1031891237209987822, 2.159356164053369387 ) ) ;
#150399 = CARTESIAN_POINT ( 'NONE',  ( 1.364683531249988535, 3.655208333674750509, -0.7879004041258239610 ) ) ;
#150400 = CARTESIAN_POINT ( 'NONE',  ( 6.309841845984305309, -1.956726702252456596, 0.2390368442499128110 ) ) ;
#150401 = CARTESIAN_POINT ( 'NONE',  ( 5.026542006541363961, 1.714758565716298477, -0.2553409819617598053 ) ) ;
#150402 = EDGE_CURVE ( 'NONE', #159873, #125532, #85472, .T. ) ;
#150404 = CARTESIAN_POINT ( 'NONE',  ( 1.646283778714407342, 0.6915601415973006150, 2.079641132013386517 ) ) ;
#150403 = CARTESIAN_POINT ( 'NONE',  ( -0.6801582343750022241, -0.1510416663252633906, -1.178068619123841643 ) ) ;
#150405 = CARTESIAN_POINT ( 'NONE',  ( 2.011159220144568938, 1.709348158914993254, -1.550378056569144958 ) ) ;
#150406 = CARTESIAN_POINT ( 'NONE',  ( 4.604794268142059721, 1.595455460008918580, -1.304385708662815002 ) ) ;
#150407 = CARTESIAN_POINT ( 'NONE',  ( 6.603083112279575673, -0.4245024861969335928, 1.902271653767301007 ) ) ;
#150408 = CARTESIAN_POINT ( 'NONE',  ( -6.019457014343129408, 9.966524250134902729, 0.000000000000000000 ) ) ;
#150410 = ADVANCED_FACE ( 'NONE', ( #65921 ), #1990, .F. ) ;
#150409 = CARTESIAN_POINT ( 'NONE',  ( -4.142898457427624415, 6.991076079377632091, 1.199719254218452935 ) ) ;
#150411 = CARTESIAN_POINT ( 'NONE',  ( 4.720248583150478794, 5.235598830736874376, 1.011424349686943280 ) ) ;
#150412 = FILL_AREA_STYLE ('',( #84326 ) ) ;
#150413 = CARTESIAN_POINT ( 'NONE',  ( 1.055314813143366726, -1.277040974352643854, 1.560502084637045650 ) ) ;
#150414 = CARTESIAN_POINT ( 'NONE',  ( -6.358410854684783509, 9.401601182898824405, -1.082531754730537976 ) ) ;
#150415 = CARTESIAN_POINT ( 'NONE',  ( 4.155453238874762256, -1.833011353516471154, -1.228491751752130545 ) ) ;
#150416 = CARTESIAN_POINT ( 'NONE',  ( 1.001543065824772753E-15, -1.509374999522041794, 3.793834371823811669 ) ) ;
#150417 = CARTESIAN_POINT ( 'NONE',  ( 1.410758858885716061, -1.471193852737593843, 1.139540799010074323 ) ) ;
#150418 =( BOUNDED_SURFACE ( )  B_SPLINE_SURFACE ( 3, 3, ( 
 ( #65932, #49718, #167738, #133140, #17194, #16125, #198091, #113730, #147240, #85417 ),
 ( #199140, #33465, #82209, #31353, #149356, #84350, #97428, #197032, #166676, #19338 ),
 ( #18267, #163482, #181832, #117987, #48668, #132081, #183980, #195984, #116912, #151501 ),
 ( #115846, #150439, #148302, #67003, #937, #50784, #182912, #34529, #2002, #15065 ),
 ( #100600, #114785, #101669, #68067, #214301, #64896, #69141, #3070, #131042, #180783 ),
 ( #134204, #99541, #47618, #179736, #200213, #51866, #35590, #32408, #165604, #83268 ),
 ( #7349, #188243, #40959, #119049, #90779, #87562, #123355, #107067, #4139, #39883 ) ),
 .UNSPECIFIED., .T., .F., .F. ) 
 B_SPLINE_SURFACE_WITH_KNOTS ( ( 4, 3, 4 ),
 ( 4, 1, 1, 1, 1, 1, 1, 4 ),
 ( 0.000000000000000000, 0.5000000000000000000, 1.000000000000000000 ),
 ( 0.000000000000000000, 0.09489293188423997272, 0.1878783894049059211, 0.2584743716234961797, 0.3617987437640678983, 0.5212292184658617877, 0.7337638816394396191, 1.000000000000000000 ),
 .UNSPECIFIED. ) 
 GEOMETRIC_REPRESENTATION_ITEM ( )  RATIONAL_B_SPLINE_SURFACE ( (
 ( 1.000000000000000222, 1.000000000000000222, 1.000000000000000000, 1.000000000000000000, 1.000000000000000000, 1.000000000000000000, 1.000000000000000000, 0.9999999999999997780, 1.000000000000000000, 1.000000000000000000),
 ( 0.3333333333333334259, 0.3333333333333333703, 0.3333333333333334259, 0.3333333333333334259, 0.3333333333333333703, 0.3333333333333333703, 0.3333333333333333703, 0.3333333333333332038, 0.3333333333333333703, 0.3333333333333333703),
 ( 0.3333333333333334259, 0.3333333333333333703, 0.3333333333333334259, 0.3333333333333334259, 0.3333333333333333703, 0.3333333333333333703, 0.3333333333333333703, 0.3333333333333332038, 0.3333333333333333703, 0.3333333333333333703),
 ( 1.000000000000000222, 1.000000000000000222, 1.000000000000000000, 1.000000000000000000, 1.000000000000000000, 1.000000000000000000, 1.000000000000000000, 0.9999999999999997780, 1.000000000000000000, 1.000000000000000000),
 ( 0.3333333333333334259, 0.3333333333333333703, 0.3333333333333334259, 0.3333333333333334259, 0.3333333333333333703, 0.3333333333333333703, 0.3333333333333333703, 0.3333333333333332038, 0.3333333333333333703, 0.3333333333333333703),
 ( 0.3333333333333334259, 0.3333333333333333703, 0.3333333333333334259, 0.3333333333333334259, 0.3333333333333333703, 0.3333333333333333703, 0.3333333333333333703, 0.3333333333333332038, 0.3333333333333333703, 0.3333333333333333703),
 ( 1.000000000000000222, 1.000000000000000222, 1.000000000000000000, 1.000000000000000000, 1.000000000000000000, 1.000000000000000000, 1.000000000000000000, 0.9999999999999997780, 1.000000000000000000, 1.000000000000000000) ) ) 
 REPRESENTATION_ITEM ( '' )  SURFACE ( )  );
#150419 = VECTOR ( 'NONE', #172156, 1000.000000000000000 ) ;
#150420 = CARTESIAN_POINT ( 'NONE',  ( 0.9311234436981489226, -1.953119629485602804, 3.475000000000000533 ) ) ;
#150421 = PLANE ( 'NONE',  #107890 ) ;
#150422 = CARTESIAN_POINT ( 'NONE',  ( -1.432341765625004593, 8.460937500170699010, 8.673617379884035472E-16 ) ) ;
#150424 = CARTESIAN_POINT ( 'NONE',  ( 6.925078400183550364, -0.007619068086212391067, 2.144148427808051594 ) ) ;
#150423 = CARTESIAN_POINT ( 'NONE',  ( -5.297016005617503076, 7.750740434075895635, -1.313619143682826396 ) ) ;
#150425 = CARTESIAN_POINT ( 'NONE',  ( 10.95308175811721085, 12.30000000000000071, -1.800000000000001155 ) ) ;
#150426 = VERTEX_POINT ( 'NONE', #183966 ) ;
#150427 = CARTESIAN_POINT ( 'NONE',  ( 3.608323775901512764, -0.8336323056173270407, -1.884943839506166174 ) ) ;
#150428 = CARTESIAN_POINT ( 'NONE',  ( -1.360316468750026875, 2.140625000341400685, -4.857225732735059864E-14 ) ) ;
#150429 = CARTESIAN_POINT ( 'NONE',  ( -5.018489415352746619, 9.006654751220198207, 0.7998128361456481317 ) ) ;
#150430 = CARTESIAN_POINT ( 'NONE',  ( 2.262373273732374290, 2.019286824851754591, 0.04726863806006965929 ) ) ;
#150431 = CARTESIAN_POINT ( 'NONE',  ( -0.7500000000000249800, -1.058333333333314030, 1.299038105676659116 ) ) ;
#150432 = CARTESIAN_POINT ( 'NONE',  ( 2.510230996824538430, 6.080353262937265413, 0.000000000000000000 ) ) ;
#150433 = CARTESIAN_POINT ( 'NONE',  ( 2.184514296101589537, -2.020881322650217360, -0.4031914428916544280 ) ) ;
#150434 =( BOUNDED_CURVE ( )  B_SPLINE_CURVE ( 2, ( #27420, #212566, #213610, #176884, #64205, #179028, #130346 ),
 .UNSPECIFIED., .F., .T. ) 
 B_SPLINE_CURVE_WITH_KNOTS ( ( 3, 2, 2, 3 ),
 ( 0.2500000000000002220, 0.2559523809523810978, 0.2619047619047619735, 0.2678571428571428492 ),
 .UNSPECIFIED. ) 
 CURVE ( )  GEOMETRIC_REPRESENTATION_ITEM ( )  RATIONAL_B_SPLINE_CURVE ( ( 0.9999999999999950040, 0.8660254037844437036, 1.000000000000000000, 0.8660254037844387076, 1.000000000000000000, 0.8660254037844387076, 1.000000000000000000 ) ) 
 REPRESENTATION_ITEM ( '' )  );
#150436 = CARTESIAN_POINT ( 'NONE',  ( -0.6823417656250039265, 13.56770833367473195, -1.181850606188755259 ) ) ;
#150435 = CARTESIAN_POINT ( 'NONE',  ( -3.267151830768976417, 6.755501535964965498, -0.7216878364870478180 ) ) ;
#150437 = EDGE_CURVE ( 'NONE', #196229, #78732, #105921, .T. ) ;
#150438 = CARTESIAN_POINT ( 'NONE',  ( 6.657217119509961201, 7.725507046638470321, -1.199719254218446718 ) ) ;
#150439 = CARTESIAN_POINT ( 'NONE',  ( -0.1409997244345879697, 0.2375178066936211585, -2.034344168881811132 ) ) ;
#150441 = PRESENTATION_LAYER_ASSIGNMENT (  '', '', ( #181629 ) ) ;
#150440 = CARTESIAN_POINT ( 'NONE',  ( 0.3394786764520755784, 1.835982197492795898, 0.1384515631646099088 ) ) ;
#150442 = CARTESIAN_POINT ( 'NONE',  ( 5.233140740401229785, 0.1595256157847015632, 2.201181388321731269 ) ) ;
#150443 = CARTESIAN_POINT ( 'NONE',  ( 5.189738938980948291, 9.276722205444929870, 0.000000000000000000 ) ) ;
#150444 = CARTESIAN_POINT ( 'NONE',  ( 1.423353863051743273, -0.05456730952056210171, 2.161080666180377197 ) ) ;
#150445 = CARTESIAN_POINT ( 'NONE',  ( -3.470524135418294520, 6.992769224722559684, -0.7216878364870267237 ) ) ;
#150446 = CARTESIAN_POINT ( 'NONE',  ( 1.868375392651611122, -1.978555653031977446, -0.3886301775877995524 ) ) ;
#150447 = CARTESIAN_POINT ( 'NONE',  ( 2.355183240404590705, -0.9839461204387394133, 2.077256468512170162 ) ) ;
#150448 = DIRECTION ( 'NONE',  ( 1.276756478318932585E-15, -1.000000000000000000, 1.665334536937738262E-16 ) ) ;
#150449 = CARTESIAN_POINT ( 'NONE',  ( 0.6197280442463182215, -0.9970892369244135356, -1.582582228963416160 ) ) ;
#150450 = CARTESIAN_POINT ( 'NONE',  ( 4.012542200100970291, 1.395003824703803685, -1.393317042198267020 ) ) ;
#150451 = AXIS2_PLACEMENT_3D ( 'NONE', #129970, #126768, #112635 ) ;
#150452 = CARTESIAN_POINT ( 'NONE',  ( 3.819546216251490822, -1.394084564108012403, -1.457236891723237449 ) ) ;
#150454 = CARTESIAN_POINT ( 'NONE',  ( 9.693716643646595799, 11.37205284141829686, 1.082531754730548412 ) ) ;
#150453 = CARTESIAN_POINT ( 'NONE',  ( 0.6823417656249899377, 1.592708333674752730, 1.181850606188755259 ) ) ;
#150456 = CARTESIAN_POINT ( 'NONE',  ( 5.233084072137057063, 0.1537158111805384808, 2.100522205955375199 ) ) ;
#150455 = CARTESIAN_POINT ( 'NONE',  ( -7.527801604085656351, 9.805521176231838609, 1.599625672291295375 ) ) ;
#150457 = CARTESIAN_POINT ( 'NONE',  ( 5.441872305809390298, 1.387781221417656141, 1.536568222347669987 ) ) ;
#150458 = CARTESIAN_POINT ( 'NONE',  ( 5.608269097547198712, 9.694731047113750222, -0.7998128361456281477 ) ) ;
#150459 = CARTESIAN_POINT ( 'NONE',  ( -6.340409392685171674, 10.54889472477470846, 0.7998128361456481317 ) ) ;
#150460 = CARTESIAN_POINT ( 'NONE',  ( 1.919771823249041720, 3.227545531266407419, -0.4000000000000275002 ) ) ;
#150461 = CARTESIAN_POINT ( 'NONE',  ( 5.572523036771587890, 0.8223149429010238043, 1.845017218462653208 ) ) ;
#150462 = CARTESIAN_POINT ( 'NONE',  ( 1.499999999999985123, -1.172916665983846363, -0.8660254037844323793 ) ) ;
#150463 = CARTESIAN_POINT ( 'NONE',  ( 0.8134211793521692879, -1.740389775365951186, -1.106656028277221537 ) ) ;
#150464 = CARTESIAN_POINT ( 'NONE',  ( 7.456621297836067086, 10.68284669990868174, 1.082531754730558626 ) ) ;
#150465 = CARTESIAN_POINT ( 'NONE',  ( 6.879836604291781121, 6.991173891287354003, -0.7998128361456341429 ) ) ;
#150466 = CARTESIAN_POINT ( 'NONE',  ( 4.376249722160992839, 8.327651452488305850, 0.000000000000000000 ) ) ;
#150467 = CARTESIAN_POINT ( 'NONE',  ( 1.364683531249986537, 0.4677083336747514530, -0.7879004041258309554 ) ) ;
#150469 = CARTESIAN_POINT ( 'NONE',  ( 9.452953409716815969, 4.518459255873298552, -7.393264975473035072 ) ) ;
#150468 = CARTESIAN_POINT ( 'NONE',  ( 4.193214648376505593, 8.114110533073061404, 0.000000000000000000 ) ) ;
#150470 = CARTESIAN_POINT ( 'NONE',  ( 6.765155463094751909, 8.915767345075790828, 1.443375672974076540 ) ) ;
#150472 = CARTESIAN_POINT ( 'NONE',  ( -6.135297098026184948, 5.374196335731616259, -2.500000000000000444 ) ) ;
#150471 = CARTESIAN_POINT ( 'NONE',  ( 3.227178390111482553, -2.005013095889785824, -0.8334813368568798619 ) ) ;
#150474 = CARTESIAN_POINT ( 'NONE',  ( 2.489598673502769977, -1.836455140896048999, -0.1334285330320400531 ) ) ;
#150473 = CARTESIAN_POINT ( 'NONE',  ( -5.775410249741523394, 5.840326167560965231, 0.7216878364870317197 ) ) ;
#150475 = CARTESIAN_POINT ( 'NONE',  ( 1.364683531249990311, 3.384375000341416140, 1.214306433183764966E-14 ) ) ;
#150476 = CARTESIAN_POINT ( 'NONE',  ( 4.195009555701286530, 1.760677850468267414, 1.304791629949946019 ) ) ;
#150477 = CARTESIAN_POINT ( 'NONE',  ( 8.382543407088986598, 14.06748126314016289, 8.587517679487557842 ) ) ;
#150478 = CARTESIAN_POINT ( 'NONE',  ( 4.961948105735218384, 2.238643107264228327, -0.3270478844536877649 ) ) ;
#150479 = CARTESIAN_POINT ( 'NONE',  ( -5.362413449404877852, 6.214902764849178141, -1.199719254218446718 ) ) ;
#150480 = CARTESIAN_POINT ( 'NONE',  ( -5.094707486240121597, 6.719114383638050469, -1.440239009331502062 ) ) ;
#150481 = CARTESIAN_POINT ( 'NONE',  ( 4.868750418105482147, 8.172599172502351905, -0.9747704861028365642 ) ) ;
#150482 = CARTESIAN_POINT ( 'NONE',  ( -5.844973620822877969, 7.912498205750389424, 1.443375672974058777 ) ) ;
#150483 = CARTESIAN_POINT ( 'NONE',  ( 4.909461021924244051, 6.821066840368686712, 1.443375672974065660 ) ) ;
#150484 = CARTESIAN_POINT ( 'NONE',  ( 6.907488038778298645, -0.3811802009726448226, 1.734239976993730670 ) ) ;
#150485 =( BOUNDED_CURVE ( )  B_SPLINE_CURVE ( 2, ( #69003, #55987, #88497, #187038, #35449 ),
 .UNSPECIFIED., .F., .T. ) 
 B_SPLINE_CURVE_WITH_KNOTS ( ( 3, 2, 3 ),
 ( 0.01079486483480429637, 0.01250000000000000069, 0.01382216642637607365 ),
 .UNSPECIFIED. ) 
 CURVE ( )  GEOMETRIC_REPRESENTATION_ITEM ( )  RATIONAL_B_SPLINE_CURVE ( ( 0.9352202683046948462, 0.9451732491399882363, 1.000000000000000000, 0.9574871888551585997, 0.9419547032718735835 ) ) 
 REPRESENTATION_ITEM ( '' )  );
#150486 = CARTESIAN_POINT ( 'NONE',  ( 4.301435403400270197, 1.797132274555211184, -0.9072848608384380675 ) ) ;
#150487 = CARTESIAN_POINT ( 'NONE',  ( 6.283314124929436417, 9.417951348137970413, -1.199719254218440723 ) ) ;
#150488 = CARTESIAN_POINT ( 'NONE',  ( 3.311648941680225722, -0.4124737740866398217, 2.064988983437756165 ) ) ;
#150489 = CARTESIAN_POINT ( 'NONE',  ( 1.388148191917773611, -0.6910900405009687830, -1.786773533054702545 ) ) ;
#150491 = CARTESIAN_POINT ( 'NONE',  ( 1.499999999999987121, 2.795833333333352488, -0.8660254037844262731 ) ) ;
#150490 = CARTESIAN_POINT ( 'NONE',  ( 0.6823417656249934904, 12.19270833367473017, 1.181850606188764807 ) ) ;
#150492 = CARTESIAN_POINT ( 'NONE',  ( 2.471101528187972463, 1.758070753236480988, 0.8880565435460830992 ) ) ;
#150493 = CARTESIAN_POINT ( 'NONE',  ( 0.08069323953814251660, -0.1329233695197447052, -1.840450602299897431 ) ) ;
#150494 = CARTESIAN_POINT ( 'NONE',  ( 1.293326634533353170, -1.775083115552608559, 0.8357255594537355003 ) ) ;
#150496 = ORIENTED_EDGE ( 'NONE', *, *, #189724, .F. ) ;
#150495 = CARTESIAN_POINT ( 'NONE',  ( 6.416260824072121061, -1.810972107014690913, 0.05430519662179972284 ) ) ;
#150497 = CARTESIAN_POINT ( 'NONE',  ( 5.341549334104184865, 8.215262742221458581, 1.082531754730558626 ) ) ;
#150498 = CARTESIAN_POINT ( 'NONE',  ( 1.364683531249986537, 0.4260416670080872659, 0.7879004041258500513 ) ) ;
#150499 = CARTESIAN_POINT ( 'NONE',  ( 6.069203928793593050, 0.1358119448514639727, -1.865795782587629681 ) ) ;
#150500 = CARTESIAN_POINT ( 'NONE',  ( 8.516493047678546091, 13.08765898893368629, -0.7998128361456352531 ) ) ;
#150501 = LINE ( 'NONE', #83331, #145031 ) ;
#150502 = B_SPLINE_CURVE_WITH_KNOTS ( 'NONE', 3,
 ( #58330, #59391, #111409, #44226, #30092, #177413 ),
 .UNSPECIFIED., .F., .F.,
 ( 4, 2, 4 ),
 ( 0.4261085947076337921, 0.4631192677600871610, 0.5001299408125404744 ),
 .UNSPECIFIED. ) ;
#150503 = CARTESIAN_POINT ( 'NONE',  ( 5.330949937734919430, -1.947458545883517189, -0.7027056652011903770 ) ) ;
#150504 = CARTESIAN_POINT ( 'NONE',  ( 1.224999999999943023, 2.645833333333332593, -0.7072540797573158011 ) ) ;
#150505 = CARTESIAN_POINT ( 'NONE',  ( -4.678972410047611774, 5.591794245544547515, 1.082531754730549078 ) ) ;
#150506 = SURFACE_STYLE_FILL_AREA ( #18336 ) ;
#150507 = CARTESIAN_POINT ( 'NONE',  ( -0.7500000000000215383, 0.1916666666666871910, 1.299038105676659116 ) ) ;
#150508 = CARTESIAN_POINT ( 'NONE',  ( 7.772902139336337335, 7.962807338847539107, 0.7998128361456341429 ) ) ;
#150509 = CARTESIAN_POINT ( 'NONE',  ( -7.178152263431422320, 10.46192917639026554, 1.199719254218453823 ) ) ;
#150510 = CARTESIAN_POINT ( 'NONE',  ( 6.099189001301251523, 8.209082816308541197, 1.599625672291268286 ) ) ;
#150511 = CARTESIAN_POINT ( 'NONE',  ( -1.402160292154681736E-14, 1.696875000341421469, -1.575800808251659024 ) ) ;
#150512 = CARTESIAN_POINT ( 'NONE',  ( -0.7500000000000215383, 3.191666666666689967, 1.299038105676671107 ) ) ;
#150514 = CARTESIAN_POINT ( 'NONE',  ( 5.508690485854129903, 5.321227076451600091, 1.040834085586084257E-14 ) ) ;
#150513 = CARTESIAN_POINT ( 'NONE',  ( 4.791432466842788784, -1.794507165602466037, 0.7932701521168731285 ) ) ;
#150515 = CARTESIAN_POINT ( 'NONE',  ( 3.514999820297697308, 2.016288306963448296, 0.002811503506894295987 ) ) ;
#150516 = CARTESIAN_POINT ( 'NONE',  ( 2.254979328032254760, 0.08947561643129221809, -1.913730806789506245 ) ) ;
#150517 = CARTESIAN_POINT ( 'NONE',  ( -1.889772045536145306, 3.296949564223910834, -0.4024211290685451581 ) ) ;
#150518 = CARTESIAN_POINT ( 'NONE',  ( 0.4159077360078728969, -1.177411712353953588, -1.848246096435968600 ) ) ;
#150519 = CARTESIAN_POINT ( 'NONE',  ( 0.2333690889706959148, 4.088440985731725874, -2.608190362703251441 ) ) ;
#150520 = CARTESIAN_POINT ( 'NONE',  ( 3.585083614955933307, 1.692364770286663322, -0.7970176776704935850 ) ) ;
#150521 = CARTESIAN_POINT ( 'NONE',  ( -0.7500000000000249800, -1.277083332650516656, 1.299038105676659116 ) ) ;
#150522 = CARTESIAN_POINT ( 'NONE',  ( -8.030507057996002729, 8.263346410617135263, 1.040834085586084257E-14 ) ) ;
#150524 = CARTESIAN_POINT ( 'NONE',  ( 4.552435263133931542, -1.381712717965150938, 1.604331009294196031 ) ) ;
#150523 = CARTESIAN_POINT ( 'NONE',  ( -4.663641653420935285, 5.503632019488245319, 1.082531754730560403 ) ) ;
#150525 = CARTESIAN_POINT ( 'NONE',  ( -6.189669738297100210, 5.317594965474102153, -2.438128856460784366 ) ) ;
#150526 = CARTESIAN_POINT ( 'NONE',  ( 6.355931484454268698, -0.7012994977402075003, 1.948090369817329526 ) ) ;
#150528 = CARTESIAN_POINT ( 'NONE',  ( 4.006649928318074316, 7.586413011018040997, -0.2369455770718699450 ) ) ;
#150527 = CARTESIAN_POINT ( 'NONE',  ( 2.437156881564545685, -1.551092155746801815, -1.402114238623404896 ) ) ;
#150530 = ORIENTED_EDGE ( 'NONE', *, *, #97346, .F. ) ;
#150529 = CARTESIAN_POINT ( 'NONE',  ( 0.8852880119799062530, 1.153610147808200370, 1.282378885572494465 ) ) ;
#150531 = CARTESIAN_POINT ( 'NONE',  ( 5.425234023762710578, 9.481190127698507553, -0.7998128361456291469 ) ) ;
#150532 = CARTESIAN_POINT ( 'NONE',  ( 7.217903723666667659, 15.51194592830137786, 9.588197132884870300 ) ) ;
#150533 = CARTESIAN_POINT ( 'NONE',  ( -0.09770433987277686583, -9.919999999999998153, -9.499497670693795470 ) ) ;
#150534 = CARTESIAN_POINT ( 'NONE',  ( 7.144783764277405247, 8.398297815487545392, -1.082531754730543971 ) ) ;
#150535 = CARTESIAN_POINT ( 'NONE',  ( -1.500000000000015099, 9.479166666666669627, -0.8660254037844309360 ) ) ;
#150537 = CARTESIAN_POINT ( 'NONE',  ( 0.7503001202024300875, 1.784421795204504946, 0.3107989935832651818 ) ) ;
#150536 = CARTESIAN_POINT ( 'NONE',  ( 5.668190738965027897, 8.770583741171307679, -1.199719254218452047 ) ) ;
#150538 = CARTESIAN_POINT ( 'NONE',  ( -8.369460898337653276, 8.658792557682392754, 0.7998128361456462443 ) ) ;
#150539 = CARTESIAN_POINT ( 'NONE',  ( 3.506755287428983792, 7.242964935309132990, 1.040834085586084257E-14 ) ) ;
#150540 = CARTESIAN_POINT ( 'NONE',  ( -5.258916259484140099, 7.686978671390940043, 1.214082833407425621 ) ) ;
#150541 = CARTESIAN_POINT ( 'NONE',  ( 7.309781096423290769, 8.557108029695882578, 1.199719254218452935 ) ) ;
#150542 = CARTESIAN_POINT ( 'NONE',  ( 3.834746474454188013E-15, 9.062500000000001776, 1.500000000000001554 ) ) ;
#150543 = CARTESIAN_POINT ( 'NONE',  ( 0.07999999999998980149, -9.999999999999994671, -10.91970695577493977 ) ) ;
#150544 = CARTESIAN_POINT ( 'NONE',  ( 9.910647101909615841, 10.66476916175714607, 0.000000000000000000 ) ) ;
#150545 = ORIENTED_EDGE ( 'NONE', *, *, #96134, .T. ) ;
#150546 = EDGE_CURVE ( 'NONE', #113379, #109831, #192601, .T. ) ;
#150547 = ADVANCED_FACE ( 'NONE', ( #922 ), #49706, .F. ) ;
#150548 = CARTESIAN_POINT ( 'NONE',  ( 0.6674275129862971001, 1.287417287929611076, 1.418633514309353583 ) ) ;
#150549 = CARTESIAN_POINT ( 'NONE',  ( 0.1883438084668061507, 1.224518555304452416, 1.730999496979759522 ) ) ;
#150550 = MECHANICAL_DESIGN_GEOMETRIC_PRESENTATION_REPRESENTATION (  '', ( #12153 ), #188568 ) ;
#150551 = DIRECTION ( 'NONE',  ( 0.7592566023653005702, 0.6507913734559639396, 0.000000000000000000 ) ) ;
#150552 = FACE_OUTER_BOUND ( 'NONE', #123608, .T. ) ;
#150553 = CARTESIAN_POINT ( 'NONE',  ( -1.567642296063691987, 8.684662666223690763, -2.500960217906271321 ) ) ;
#150554 = CARTESIAN_POINT ( 'NONE',  ( -3.741687207691642314, 6.348756928073427730, 1.082531754730560403 ) ) ;
#150555 =( GEOMETRIC_REPRESENTATION_CONTEXT ( 3 ) GLOBAL_UNCERTAINTY_ASSIGNED_CONTEXT ( ( #44356 ) ) GLOBAL_UNIT_ASSIGNED_CONTEXT ( ( #30136, #212057, #179590 ) ) REPRESENTATION_CONTEXT ( 'NONE', 'WORKASPACE' ) );
#150556 = CARTESIAN_POINT ( 'NONE',  ( 7.944714827928033962, 12.21265836598400689, 0.7216878364870438212 ) ) ;
#150557 = CARTESIAN_POINT ( 'NONE',  ( 3.660960169446208390, 1.555274301336776022, -1.208163239264722133 ) ) ;
#150558 = CARTESIAN_POINT ( 'NONE',  ( 1.366058183223411771, 0.6122477967837879342, -2.030190212274018524 ) ) ;
#150559 = CARTESIAN_POINT ( 'NONE',  ( -6.728924311084075960, 6.744833205886536120, 1.040834085586084257E-14 ) ) ;
#150560 = CARTESIAN_POINT ( 'NONE',  ( -11.13163773270227530, 7.261023013786968683, 4.365999805656710642 ) ) ;
#150561 = CARTESIAN_POINT ( 'NONE',  ( 6.017560223340764125, -1.214513600917455083, -1.823921334435735231 ) ) ;
#150562 = CARTESIAN_POINT ( 'NONE',  ( 0.000000000000000000, 6.999999999999999112, 0.000000000000000000 ) ) ;
#150563 = CARTESIAN_POINT ( 'NONE',  ( 4.471652382922743030, 1.868735325311605688, -0.4673391499005700722 ) ) ;
#150564 = CARTESIAN_POINT ( 'NONE',  ( -8.843996274815957293, 9.212417163573759282, 1.040834085586084257E-14 ) ) ;
#150565 = CARTESIAN_POINT ( 'NONE',  ( 0.1998643617870856648, -1.825052844667142349, -0.05062755788937112200 ) ) ;
#150566 = CARTESIAN_POINT ( 'NONE',  ( 0.7334016978863611147, 0.1661181961954381059, 2.200687262777756725 ) ) ;
#150567 = DIRECTION ( 'NONE',  ( -5.578564026256490882E-16, -1.000000000000000000, -9.066213480720158442E-32 ) ) ;
#150568 = ORIENTED_EDGE ( 'NONE', *, *, #155760, .F. ) ;
#150569 = CARTESIAN_POINT ( 'NONE',  ( 4.421367491832282504, 5.291255174293369556, 1.082531754730549078 ) ) ;
#150570 = CARTESIAN_POINT ( 'NONE',  ( 5.928554213991230171, -1.252361881311152558, 1.519918492727867054 ) ) ;
#150571 = CARTESIAN_POINT ( 'NONE',  ( -0.05917297228825654093, -1.501800262597710267, -1.231000148999121357 ) ) ;
#150572 = CARTESIAN_POINT ( 'NONE',  ( 6.274848118712046841, -2.282167594539401101, 0.2721878479114477334 ) ) ;
#150574 = CARTESIAN_POINT ( 'NONE',  ( 4.487043221128726778, 0.08799343497551150028, 1.858965402599630723 ) ) ;
#150573 = CARTESIAN_POINT ( 'NONE',  ( -6.095272577795516789, 9.268845886473535245, 1.199719254218452047 ) ) ;
#150575 = CARTESIAN_POINT ( 'NONE',  ( 6.821687566331318564, 7.987665577921906568, 1.199719254218452935 ) ) ;
#150576 = FACE_OUTER_BOUND ( 'NONE', #189050, .T. ) ;
#150577 = CARTESIAN_POINT ( 'NONE',  ( -5.249999999999987566, 1.374772708486751593, 1.000000000000000888 ) ) ;
#150578 = CARTESIAN_POINT ( 'NONE',  ( -6.501298352952815662, 7.543601818988450169, -1.199719254218446718 ) ) ;
#150579 = CARTESIAN_POINT ( 'NONE',  ( -3.263163593824906172, -0.8930720647284263736, 0.4328774883419782005 ) ) ;
#150580 = CARTESIAN_POINT ( 'NONE',  ( 0.8201894534925309177, 1.301127354658284663, -1.763390660798454634 ) ) ;
#150581 = CARTESIAN_POINT ( 'NONE',  ( 4.690757960648231695, 5.535267711253469614, 1.082531754730560403 ) ) ;
#150582 = EDGE_LOOP ( 'NONE', ( #17451, #15426, #174173, #144251 ) ) ;
#150583 = CARTESIAN_POINT ( 'NONE',  ( 4.907894938888484937, 6.474487383728033230, 2.499999999999998668 ) ) ;
#150584 = CARTESIAN_POINT ( 'NONE',  ( 3.404766800216717737, 6.348112014766642552, 1.069586989871921467 ) ) ;
#150585 = CARTESIAN_POINT ( 'NONE',  ( 0.6799654140086827114, -1.016662149479659494, 1.516215539243186639 ) ) ;
#150586 = CARTESIAN_POINT ( 'NONE',  ( -4.029797971759847997, 5.724516938518342535, -1.599625672291256295 ) ) ;
#150587 = CARTESIAN_POINT ( 'NONE',  ( 3.726996057929339745, 1.726255173046949309, 0.1649803145151728934 ) ) ;
#150588 = CARTESIAN_POINT ( 'NONE',  ( -10.39230484541327826, 3.447199233515649386, -5.999999999999975131 ) ) ;
#150589 = CARTESIAN_POINT ( 'NONE',  ( -0.3282377607281322107, 2.698664549684628433, -1.225000000000014744 ) ) ;
#150590 = CARTESIAN_POINT ( 'NONE',  ( 1.250000000000037526, 8.500000000000000000, -10.97907099895068583 ) ) ;
#150591 = CARTESIAN_POINT ( 'NONE',  ( 6.551389018236878137, -1.469694460105780642, -1.082916835497591324 ) ) ;
#150592 = CARTESIAN_POINT ( 'NONE',  ( 4.451973756923766068, -0.7546651901383871763, 1.810992078419524365 ) ) ;
#150593 = CARTESIAN_POINT ( 'NONE',  ( -9.073431116043565225, 11.60875560684942265, -1.599625672291263179 ) ) ;
#150594 = CARTESIAN_POINT ( 'NONE',  ( 4.774442650306744085, 8.721933525333202653, -0.7998128361456281477 ) ) ;
#150595 = CARTESIAN_POINT ( 'NONE',  ( 4.740951199079581180, 2.029406658027664623, 0.6148427566107574904 ) ) ;
#150596 = CARTESIAN_POINT ( 'NONE',  ( 6.668631453075247073, 8.873432343378178544, -1.599625672291281386 ) ) ;
#150597 = CARTESIAN_POINT ( 'NONE',  ( -10.29471871147821282, 10.90492667301307605, -0.7998128361456291469 ) ) ;
#150598 = CIRCLE ( 'NONE', #8641, 4.500000000000000000 ) ;
#150599 = CARTESIAN_POINT ( 'NONE',  ( 4.202137545231717120, 6.989912005157271402, 1.199719254218462483 ) ) ;
#150600 = CARTESIAN_POINT ( 'NONE',  ( 3.309495622959734096, -1.689761761210720525, -1.195817184978978043 ) ) ;
#150602 = CARTESIAN_POINT ( 'NONE',  ( -1.364683531250000748, 0.07187500034142035865, 0.000000000000000000 ) ) ;
#150601 = CARTESIAN_POINT ( 'NONE',  ( 2.276625743944757474, 2.743370740431589017, 2.499999999999998668 ) ) ;
#150604 = ORIENTED_EDGE ( 'NONE', *, *, #196542, .F. ) ;
#150603 = CARTESIAN_POINT ( 'NONE',  ( 5.110122900737038343, -0.8006010496643833907, 2.072185752117897461 ) ) ;
#150605 = CARTESIAN_POINT ( 'NONE',  ( 3.200086968229500783, 2.078864265255635946, 0.9811947989078557697 ) ) ;
#150606 = CARTESIAN_POINT ( 'NONE',  ( 8.188761592974039161, 10.57664116326830595, -1.443375672974063439 ) ) ;
#150608 = CARTESIAN_POINT ( 'NONE',  ( 3.285556943750000514, -2.063541666188710266, 1.896917185911906500 ) ) ;
#150607 = CARTESIAN_POINT ( 'NONE',  ( 5.533136088152891929, 9.469426179571447832, -0.7216878364870458196 ) ) ;
#150609 = DIRECTION ( 'NONE',  ( 0.000000000000000000, 0.000000000000000000, 1.000000000000000000 ) ) ;
#150610 = ORIENTED_EDGE ( 'NONE', *, *, #36937, .F. ) ;
#150612 = CARTESIAN_POINT ( 'NONE',  ( 4.255647627037052709E-16, 0.5000000000000004441, 3.475000000000000089 ) ) ;
#150611 = AXIS2_PLACEMENT_3D ( 'NONE', #209694, #128560, #45112 ) ;
#150613 = EDGE_CURVE ( 'NONE', #54318, #125323, #10341, .T. ) ;
#150614 = CARTESIAN_POINT ( 'NONE',  ( 4.271672842113056312, 0.4137096367802223784, -1.866957553337177611 ) ) ;
#150615 = CARTESIAN_POINT ( 'NONE',  ( -0.2542610327306510931, 7.036558673036513056, -4.015411564048622317 ) ) ;
#150616 = CARTESIAN_POINT ( 'NONE',  ( 4.770341545797544214, -1.125046721222152213, 1.307389476665332895 ) ) ;
#150617 = CARTESIAN_POINT ( 'NONE',  ( 3.010954138651841916, 0.05432569772663428664, 2.015980714967258614 ) ) ;
#150618 = CARTESIAN_POINT ( 'NONE',  ( 5.502642741134641469, -2.243371634331346343, 0.5006679109763980673 ) ) ;
#150619 = CARTESIAN_POINT ( 'NONE',  ( -11.49978884755372555, 12.35729178837191888, -3.429452816445187402 ) ) ;
#150620 = CARTESIAN_POINT ( 'NONE',  ( 5.865875422609286183, 2.075172955015105014, -0.3584678469405917500 ) ) ;
#150621 = CARTESIAN_POINT ( 'NONE',  ( -4.638297949650955765, 8.425448351319163365, 0.7216878364870267237 ) ) ;
#150622 = EDGE_LOOP ( 'NONE', ( #158688, #111960, #24373, #55674 ) ) ;
#150623 = CARTESIAN_POINT ( 'NONE',  ( 5.905463120178883862, -0.4284811148945049109, 1.716917210449308673 ) ) ;
#150625 = CARTESIAN_POINT ( 'NONE',  ( 1.447684683128658278, 0.6615928844308440748, -2.194714443420691552 ) ) ;
#150624 = CARTESIAN_POINT ( 'NONE',  ( 4.929271367020211514, 7.908511140569038922, 1.199719254218452047 ) ) ;
#150626 = CARTESIAN_POINT ( 'NONE',  ( 0.4447213192238759771, 0.5506589691408066978, -1.650998906686143464 ) ) ;
#150627 = CARTESIAN_POINT ( 'NONE',  ( -3.755772246185468788, 4.340488027759846545, -1.199719254218452047 ) ) ;
#150628 = FILL_AREA_STYLE ('',( #183104 ) ) ;
#150629 = CARTESIAN_POINT ( 'NONE',  ( -5.327428015527048366, 5.180030537728460338, -0.7998128361456362523 ) ) ;
#150630 = CARTESIAN_POINT ( 'NONE',  ( -0.6801582343750229853, -0.8697916663252605041, -1.178068619123862515 ) ) ;
#150631 = EDGE_CURVE ( 'NONE', #82918, #80427, #4470, .T. ) ;
#150632 = CARTESIAN_POINT ( 'NONE',  ( 6.883263157960362477, -0.004191378316371896506, 2.053658919477070910 ) ) ;
#150633 = CARTESIAN_POINT ( 'NONE',  ( 1.270720652900014791, -0.3006520276036573902, -1.993892820393451615 ) ) ;
#150634 = CARTESIAN_POINT ( 'NONE',  ( 1.499999999999987121, -0.2145833326505137972, 0.8660254037844524744 ) ) ;
#150635 = CARTESIAN_POINT ( 'NONE',  ( 5.022062012317437762, -1.032219231902216761, -1.626458924502146797 ) ) ;
#150636 = CARTESIAN_POINT ( 'NONE',  ( -8.012344526598182026E-15, 12.04687500034140335, -1.575800808251669460 ) ) ;
#150637 = CARTESIAN_POINT ( 'NONE',  ( 2.549351761953377427, 0.2766319664159795355, 2.204086880180194274 ) ) ;
#150638 = VERTEX_POINT ( 'NONE', #21441 ) ;
#150640 = CARTESIAN_POINT ( 'NONE',  ( -7.013428937081412684, 5.939655416065874327, 2.436399677959149468 ) ) ;
#150639 = PRESENTATION_STYLE_ASSIGNMENT (( #151704 ) ) ;
#150641 = CARTESIAN_POINT ( 'NONE',  ( 3.733245760708456817, 7.355895828392214675, 0.2085371205484687906 ) ) ;
#150642 = CARTESIAN_POINT ( 'NONE',  ( 8.028399517586572998, 12.51821653715971472, -0.7998128361456352531 ) ) ;
#150643 = FACE_OUTER_BOUND ( 'NONE', #53794, .T. ) ;
#150644 =( NAMED_UNIT ( * ) SI_UNIT ( $, .STERADIAN. ) SOLID_ANGLE_UNIT ( ) );
#150645 = CARTESIAN_POINT ( 'NONE',  ( 4.282551955697760704, 1.552239185393188947, -0.7873791831930468943 ) ) ;
#150646 = CARTESIAN_POINT ( 'NONE',  ( 2.963279974173158138, 1.655882904019840840, 1.051842618152734499 ) ) ;
#150648 = CARTESIAN_POINT ( 'NONE',  ( -6.344852701515500293, 9.385783337534627790, 1.082531754730548412 ) ) ;
#150647 = CARTESIAN_POINT ( 'NONE',  ( 3.323720213644492993, 7.029424015893889433, 1.040834085586084257E-14 ) ) ;
#150649 = CARTESIAN_POINT ( 'NONE',  ( -5.910693218230258061, 6.000975156485434781, -0.07073762994192281384 ) ) ;
#150650 = CARTESIAN_POINT ( 'NONE',  ( 2.275435306267621804, 5.643409308550367598, 0.5316758947214432762 ) ) ;
#150651 = CARTESIAN_POINT ( 'NONE',  ( 0.9243725180730785196, 1.015136377070953388, 1.795498427122848017 ) ) ;
#150652 = CARTESIAN_POINT ( 'NONE',  ( -6.320072162264675164, 10.52516795595079557, 0.7998128361456481317 ) ) ;
#150653 = CARTESIAN_POINT ( 'NONE',  ( -5.558479791478509568, 5.587240632920778438, 0.000000000000000000 ) ) ;
#150654 = CARTESIAN_POINT ( 'NONE',  ( 1.622331739061450007, -1.257988004683800787, -1.880359251820800104 ) ) ;
#150655 = EDGE_LOOP ( 'NONE', ( #20758, #58750, #112097, #159497 ) ) ;
#150656 = CARTESIAN_POINT ( 'NONE',  ( -1.500000000000015099, -0.08958333265051321437, -0.8660254037844383745 ) ) ;
#150657 = CARTESIAN_POINT ( 'NONE',  ( 2.794054307841778328, -1.865266697571520194, -0.1415833504254116748 ) ) ;
#150658 = CARTESIAN_POINT ( 'NONE',  ( 0.8965906023701503136, -0.7780376274850349105, -1.549907966113317270 ) ) ;
#150659 = EDGE_CURVE ( 'NONE', #5754, #153475, #99259, .T. ) ;
#150660 = CARTESIAN_POINT ( 'NONE',  ( 5.636325218313963603, 0.4264374063192889475, 2.149501299143250055 ) ) ;
#150661 = CARTESIAN_POINT ( 'NONE',  ( 5.667085135620930636, -2.082984650255703230, -0.9933455750401504192 ) ) ;
#150662 = CARTESIAN_POINT ( 'NONE',  ( 1.622021928100621624, -1.144040325636319189, -1.713970819250490552 ) ) ;
#150663 = CARTESIAN_POINT ( 'NONE',  ( 3.029168698193057008, -1.304570280419844686, -1.438651077900707120 ) ) ;
#150664 = CARTESIAN_POINT ( 'NONE',  ( -3.253593677155282471, 6.739683690082376444, 1.040834085586084257E-14 ) ) ;
#150665 = CARTESIAN_POINT ( 'NONE',  ( 5.817618194842750334, -1.825074353437942332, 0.4092329068215995735 ) ) ;
#150666 = CARTESIAN_POINT ( 'NONE',  ( 1.906250000000001332, 1.895863743164044823, -0.7852924748300882385 ) ) ;
#150667 = EDGE_CURVE ( 'NONE', #202176, #167392, #90565, .T. ) ;
#150668 = CARTESIAN_POINT ( 'NONE',  ( 3.995705304526904200, 7.602062626508213405, -0.07732544726959944548 ) ) ;
#150669 = CARTESIAN_POINT ( 'NONE',  ( 0.2976278659034147789, -1.588993460933589841, 0.6942472086189295233 ) ) ;
#150670 = CARTESIAN_POINT ( 'NONE',  ( 4.340018570150304456, 6.156717313299049366, -1.443375672974068769 ) ) ;
#150671 = CARTESIAN_POINT ( 'NONE',  ( -1.953008978358306879E-14, 1.828125000341410678, -1.570758158831798257 ) ) ;
#150672 = CARTESIAN_POINT ( 'NONE',  ( 4.078750125433938223, -0.7691220382576718917, 1.864168106189521890 ) ) ;
#150673 = CARTESIAN_POINT ( 'NONE',  ( -4.161989969270909917, 5.878740935614591656, 1.443375672974064550 ) ) ;
#150674 = CARTESIAN_POINT ( 'NONE',  ( 7.910292558569346433, 11.31609285405122556, -1.199719254218446718 ) ) ;
#150675 = CARTESIAN_POINT ( 'NONE',  ( 3.705121118284530279, 7.544668081299086282, -1.734723475976807094E-15 ) ) ;
#150677 =( NAMED_UNIT ( * ) PLANE_ANGLE_UNIT ( ) SI_UNIT ( $, .RADIAN. ) );
#150676 = CARTESIAN_POINT ( 'NONE',  ( 1.805030607383810715, 1.517133602069477893, 1.015288170653723343 ) ) ;
#150678 = CARTESIAN_POINT ( 'NONE',  ( -3.786470039966538970, 7.639575156594750283, 0.000000000000000000 ) ) ;
#150679 = CARTESIAN_POINT ( 'NONE',  ( 11.38999389752405023, 1.405705671057797534, -3.777644806142902656 ) ) ;
#150680 = CARTESIAN_POINT ( 'NONE',  ( -10.30047605039691128, 4.688744718740807116, 5.507884344589919934 ) ) ;
#150681 = ORIENTED_EDGE ( 'NONE', *, *, #186335, .T. ) ;
#150682 = CARTESIAN_POINT ( 'NONE',  ( -6.265276382846530545, 6.482112999508623297, 0.000000000000000000 ) ) ;
#150683 = CARTESIAN_POINT ( 'NONE',  ( -2.764973262183167968, 5.313220341600567664, 1.199719254218462483 ) ) ;
#150684 = CARTESIAN_POINT ( 'NONE',  ( -7.960608749518247151, 12.43912730774665576, 0.000000000000000000 ) ) ;
#150685 = CARTESIAN_POINT ( 'NONE',  ( 5.567059059060062154, -1.590727130084067964, 1.244318111769521229 ) ) ;
#150687 = ORIENTED_EDGE ( 'NONE', *, *, #138823, .F. ) ;
#150686 = CARTESIAN_POINT ( 'NONE',  ( 0.1180496341894651385, -0.5612577129426484790, 2.044807062438446454 ) ) ;
#150688 = CARTESIAN_POINT ( 'NONE',  ( -5.562588163356775972, 9.711712967216715953, 0.7998128361456291469 ) ) ;
#150689 = CARTESIAN_POINT ( 'NONE',  ( 4.710568305744190276, 7.583081225755162968, 1.199719254218462483 ) ) ;
#150690 = CARTESIAN_POINT ( 'NONE',  ( 4.909085936489448798, 1.792118714629163057, 1.017505292531006189 ) ) ;
#150691 = CARTESIAN_POINT ( 'NONE',  ( 5.151017605526479137, 0.9962996879465220168, 1.753031629501592192 ) ) ;
#150692 = ORIENTED_EDGE ( 'NONE', *, *, #125292, .F. ) ;
#150693 = ORIENTED_EDGE ( 'NONE', *, *, #24957, .F. ) ;
#150694 = CARTESIAN_POINT ( 'NONE',  ( 0.000000000000000000, 4.999999999999997335, 0.000000000000000000 ) ) ;
#150695 = CARTESIAN_POINT ( 'NONE',  ( -0.2108831679770926115, 5.723481173670196043, -2.491210874135452613 ) ) ;
#150697 = VERTEX_POINT ( 'NONE', #185580 ) ;
#150696 = CARTESIAN_POINT ( 'NONE',  ( -7.293360289508603600, 7.473618190706972086, 0.000000000000000000 ) ) ;
#150698 = CARTESIAN_POINT ( 'NONE',  ( 5.084740326411086642, 7.951855545768795608, 1.193092838546747414 ) ) ;
#150699 = CARTESIAN_POINT ( 'NONE',  ( 5.589220178194088895, 1.203167956798111060, -1.617571559180859486 ) ) ;
#150700 = CARTESIAN_POINT ( 'NONE',  ( 4.400242069895500485, 1.421654421768648868, -1.169904355399861595 ) ) ;
#150701 = CARTESIAN_POINT ( 'NONE',  ( -0.02319159430947542386, 1.394398620246390275, -2.068318759734718792 ) ) ;
#150702 = CARTESIAN_POINT ( 'NONE',  ( 1.999037954658490213, -0.6180237258119178900, -2.223338030673171151 ) ) ;
#150703 = CARTESIAN_POINT ( 'NONE',  ( 7.530627977747744062, 7.750430493652658015, -0.7998128361456341429 ) ) ;
#150704 = CARTESIAN_POINT ( 'NONE',  ( 4.657600047955182454, 0.4785990281669267876, -2.107782517917502929 ) ) ;
#150705 = CARTESIAN_POINT ( 'NONE',  ( 6.123478934866503742, 10.29580919065294431, 0.7998128361456462443 ) ) ;
#150706 = CARTESIAN_POINT ( 'NONE',  ( 0.09902944379243035222, -0.5168498253214492966, 1.871975360678623579 ) ) ;
#150707 = CARTESIAN_POINT ( 'NONE',  ( -4.786191920824102830, 5.542644314838231168, 1.199719254218462483 ) ) ;
#150708 = CARTESIAN_POINT ( 'NONE',  ( 3.901994836520364718, 0.3331327188077978785, 2.274008445091058928 ) ) ;
#150709 = CARTESIAN_POINT ( 'NONE',  ( -9.490193176475230530, 15.20116513229150534, -7.238303200632643986 ) ) ;
#150711 = AXIS2_PLACEMENT_3D ( 'NONE', #201387, #33581, #36768 ) ;
#150710 = CARTESIAN_POINT ( 'NONE',  ( -4.197131071882288289, 7.054347462908075350, -1.199719254218455378 ) ) ;
#150712 = CARTESIAN_POINT ( 'NONE',  ( 3.801501934187266230, -0.5436965770258190833, 1.789884385262895616 ) ) ;
#150713 = VECTOR ( 'NONE', #197735, 1000.000000000000000 ) ;
#150716 = CARTESIAN_POINT ( 'NONE',  ( -5.478376588373717659, 8.549133898814758936, -1.199719254218452047 ) ) ;
#150715 = CARTESIAN_POINT ( 'NONE',  ( -0.7500000000000006661, -0.8604166659838472508, -1.299038105676652011 ) ) ;
#150714 = CARTESIAN_POINT ( 'NONE',  ( 0.6504702201592416078, 1.884490048413577368, 0.3244712162126031085 ) ) ;
#150717 = CARTESIAN_POINT ( 'NONE',  ( 2.737190076726934151, 0.2709513247245790013, 2.190122135706531914 ) ) ;
#150718 = DIRECTION ( 'NONE',  ( 1.000000000000000000, 0.000000000000000000, 1.224646799147353207E-16 ) ) ;
#150719 = CARTESIAN_POINT ( 'NONE',  ( 4.005544317833563461, 6.760553239859419250, -1.199719254218452047 ) ) ;
#150720 = DIRECTION ( 'NONE',  ( 0.6507913734559640506, -0.7592566023653004592, 0.000000000000000000 ) ) ;
#150721 = CARTESIAN_POINT ( 'NONE',  ( -3.425406365747000859, 7.148057860013469877, 1.040834085586084257E-14 ) ) ;
#150722 = CARTESIAN_POINT ( 'NONE',  ( -6.495764994278840021, 8.671754808115688107, 1.443375672974064550 ) ) ;
#150723 = CARTESIAN_POINT ( 'NONE',  ( 0.4914017305483203701, 1.457842971892213235, 1.327161884117057600 ) ) ;
#150724 = CARTESIAN_POINT ( 'NONE',  ( 6.498638929175646339, -0.6082784835782985011, -2.226023345802934372 ) ) ;
#150725 = CARTESIAN_POINT ( 'NONE',  ( 1.029656018189710309, 1.891699080040713410, -0.5197978237033785698 ) ) ;
#150726 = CARTESIAN_POINT ( 'NONE',  ( 3.836832695767174783, -1.986499165045521265, -0.5546697284559941599 ) ) ;
#150727 = CARTESIAN_POINT ( 'NONE',  ( 6.819388077993785657, 7.058300300521964665, 1.040834085586084257E-14 ) ) ;
#150728 = CARTESIAN_POINT ( 'NONE',  ( 6.475954649182838807, 7.584310507915338562, 1.199719254218452047 ) ) ;
#150729 = ORIENTED_EDGE ( 'NONE', *, *, #14091, .F. ) ;
#150730 = CARTESIAN_POINT ( 'NONE',  ( 8.066738210006686671, 9.473911335505048825, 1.082531754730558626 ) ) ;
#150731 = CARTESIAN_POINT ( 'NONE',  ( -0.6823417656250212460, 5.363541667008087543, 1.181850606188767472 ) ) ;
#150732 = FACE_OUTER_BOUND ( 'NONE', #71073, .T. ) ;
#150733 = CARTESIAN_POINT ( 'NONE',  ( 4.378920427089557421, 5.171457255435017331, -1.082531754730548412 ) ) ;
#150734 = CARTESIAN_POINT ( 'NONE',  ( 6.355955588539900170, -0.7375000094371157999, 2.042207395130499759 ) ) ;
#150736 = CARTESIAN_POINT ( 'NONE',  ( 6.614805131849967879, -0.1256686391097518729, 1.812046779126045726 ) ) ;
#150735 = CARTESIAN_POINT ( 'NONE',  ( 9.498763045328258769, -9.581505939640273084, -0.1791256580993725867 ) ) ;
#150737 = CARTESIAN_POINT ( 'NONE',  ( 5.445097452434600527, 6.261244994358417415, -1.018272717561970353 ) ) ;
#150738 = DIRECTION ( 'NONE',  ( 1.276756478318932585E-15, -1.000000000000000000, 1.665334536937738262E-16 ) ) ;
#150739 = CARTESIAN_POINT ( 'NONE',  ( 0.9658262494645246665, 0.9167188063998463754, 1.630421345857439475 ) ) ;
#150740 = CARTESIAN_POINT ( 'NONE',  ( -6.024621019446552594, 6.066914679173425640, 0.6088392743194663836 ) ) ;
#150741 = DIRECTION ( 'NONE',  ( -0.7613463080411786432, 0.000000000000000000, -0.6483454320283800199 ) ) ;
#150742 = CARTESIAN_POINT ( 'NONE',  ( 5.269423316188119877, 7.778230059001682406, -1.291559732514224068 ) ) ;
#150743 = CARTESIAN_POINT ( 'NONE',  ( -0.6823417656249969321, 5.530208333674756283, -1.181850606188749264 ) ) ;
#150744 = CARTESIAN_POINT ( 'NONE',  ( 0.8559432719405722922, 0.7744784914341161786, -1.748599447100062321 ) ) ;
#150745 = CARTESIAN_POINT ( 'NONE',  ( 2.904884094325186350, 1.494127413938572069, 0.9483235522904243098 ) ) ;
#150746 = AXIS2_PLACEMENT_3D ( 'NONE', #204007, #172624, #55655 ) ;
#150747 = CARTESIAN_POINT ( 'NONE',  ( 1.277824965264368728, 1.883817941867833134, -0.3277997056638781714 ) ) ;
#150749 = CARTESIAN_POINT ( 'NONE',  ( 4.323789496349770722, 0.8154102246901802076, -1.733521564635835732 ) ) ;
#150748 = CARTESIAN_POINT ( 'NONE',  ( -9.797921721691023933, 3.956598013261175772, -6.103348209225892163 ) ) ;
#150750 = CARTESIAN_POINT ( 'NONE',  ( -0.1409997244346088141, 4.088373444016307978, -2.555100908668860082 ) ) ;
#150751 = CARTESIAN_POINT ( 'NONE',  ( 5.494576857243831824, 1.940090112543988665, 0.3384423684570179724 ) ) ;
#150752 = CARTESIAN_POINT ( 'NONE',  ( 0.5980879788009090259, 1.428637019467562830, 1.567290143595565066 ) ) ;
#150753 = CARTESIAN_POINT ( 'NONE',  ( 0.2897211420239304558, -7.754973434576989177, -10.97056425546336023 ) ) ;
#150754 = CARTESIAN_POINT ( 'NONE',  ( 3.590566789841375339, -0.3639703897368729568, -1.834726254853453087 ) ) ;
#150756 = EDGE_LOOP ( 'NONE', ( #208049, #118117, #201112, #71556 ) ) ;
#150755 = CARTESIAN_POINT ( 'NONE',  ( 1.137010146156680834, -1.651496384925277283, 0.7785749969668461778 ) ) ;
#150758 = CARTESIAN_POINT ( 'NONE',  ( -1.992392395334928734, -0.1979219324388414303, 0.6149939648489994859 ) ) ;
#150757 = CARTESIAN_POINT ( 'NONE',  ( 3.071135375186518690, -2.039199700013223815, -0.8442704067812344393 ) ) ;
#150759 = CARTESIAN_POINT ( 'NONE',  ( 1.364683531249990311, 5.176041667008085767, 0.7879004041258500513 ) ) ;
#150760 = CARTESIAN_POINT ( 'NONE',  ( 1.223174996406689585, -1.863865272486511460, -0.8838528460363299644 ) ) ;
#150761 = CARTESIAN_POINT ( 'NONE',  ( 6.693975156845185737, 8.832723654451292816, 1.599625672291281386 ) ) ;
#150762 = CARTESIAN_POINT ( 'NONE',  ( -9.501566725078754772, 9.979582688880366703, -0.7998128361456291469 ) ) ;
#150763 = CARTESIAN_POINT ( 'NONE',  ( 4.421367491832268293, 7.211993602896056288, 1.082531754730549078 ) ) ;
#150764 = CARTESIAN_POINT ( 'NONE',  ( 11.95360554405576359, 11.10444996502598336, -1.059413164304676469 ) ) ;
#150765 = AXIS2_PLACEMENT_3D ( 'NONE', #195027, #206999, #43469 ) ;
#150766 = CARTESIAN_POINT ( 'NONE',  ( 6.469012471580376733, -1.473683540339595588, 1.218514635347216046 ) ) ;
#150767 = EDGE_LOOP ( 'NONE', ( #4920, #170807, #149188, #8936, #175075, #144344, #34769, #203125, #126980 ) ) ;
#150768 = CARTESIAN_POINT ( 'NONE',  ( 2.682155120989743402, -1.190029146579720587, -1.693995171316540427 ) ) ;
#150769 = CARTESIAN_POINT ( 'NONE',  ( -1.499999999999997780, 5.150000000000022560, 1.214306433183764966E-14 ) ) ;
#150770 = CARTESIAN_POINT ( 'NONE',  ( 1.423353863051743273, -0.05456730952056210171, 2.161080666180377197 ) ) ;
#150771 = CARTESIAN_POINT ( 'NONE',  ( -6.483603504774570148, 6.769331023298949646, -0.2299166613418425487 ) ) ;
#150772 = CARTESIAN_POINT ( 'NONE',  ( 1.242838512808578377, 1.947023393874779851, 0.5366068325038054754 ) ) ;
#150773 = DIRECTION ( 'NONE',  ( 0.000000000000000000, 1.000000000000000000, 0.000000000000000000 ) ) ;
#150774 = VERTEX_POINT ( 'NONE', #149911 ) ;
#150776 = CARTESIAN_POINT ( 'NONE',  ( 8.812436659202669276, 10.34389285956704363, -1.082531754730543083 ) ) ;
#150775 = CARTESIAN_POINT ( 'NONE',  ( 1.001543065824772753E-15, -2.362500000000001155, 4.012584370867899430 ) ) ;
#150777 = CARTESIAN_POINT ( 'NONE',  ( 2.000000000000011990, 2.453103989352373237E-14, 0.5999999999999970912 ) ) ;
#150778 = CARTESIAN_POINT ( 'NONE',  ( 0.5675926644314840397, 1.357872185771633156, 1.490966652548594285 ) ) ;
#150779 = CARTESIAN_POINT ( 'NONE',  ( 1.608462485350599769, 8.735270501766756013, -2.463594439587629914 ) ) ;
#150780 = CARTESIAN_POINT ( 'NONE',  ( 5.108995794240286159, -0.3219066699026683631, 2.167653318578148358 ) ) ;
#150781 = CARTESIAN_POINT ( 'NONE',  ( -1.500000000000013101, 2.910416667349485120, -0.8660254037844313801 ) ) ;
#150782 = CARTESIAN_POINT ( 'NONE',  ( 3.656429697474584462, 1.903630103707624865, 0.1825790434749063051 ) ) ;
#150783 = CARTESIAN_POINT ( 'NONE',  ( -4.497554271431319250, 6.270232621468402989, -1.599625672291256295 ) ) ;
#150784 = CARTESIAN_POINT ( 'NONE',  ( 4.324687812634887329, 6.068555086205916105, 1.443375672974062551 ) ) ;
#150786 = CARTESIAN_POINT ( 'NONE',  ( 1.581657880887325174, -0.6766953518495041342, 1.899626397962331126 ) ) ;
#150785 = CARTESIAN_POINT ( 'NONE',  ( 10.98997987423604172, -6.893137084989842123, -0.4694063952341842594 ) ) ;
#150787 = CARTESIAN_POINT ( 'NONE',  ( -1.364683531250014514, 10.40104166700806765, -0.7879004041258335089 ) ) ;
#150789 = CARTESIAN_POINT ( 'NONE',  ( -3.969505113751027547, 7.853116076009993840, 1.214306433183764966E-14 ) ) ;
#150788 = CARTESIAN_POINT ( 'NONE',  ( 0.6270410820986601630, 0.1761543355088228957, 2.285679397864130102 ) ) ;
#150790 = CARTESIAN_POINT ( 'NONE',  ( 3.645241786196154354, -1.305741510076625644, -1.126962775032739339 ) ) ;
#150791 = CARTESIAN_POINT ( 'NONE',  ( 0.1405533004714279166, 6.947787103499396544, -2.874819994463383654 ) ) ;
#150792 = CARTESIAN_POINT ( 'NONE',  ( 5.169736645512481132, 4.925780929386339935, 0.7998128361456341429 ) ) ;
#150793 = CARTESIAN_POINT ( 'NONE',  ( 3.947104627881218963, 8.980740528189222971, -0.7749999999999996891 ) ) ;
#150794 = CARTESIAN_POINT ( 'NONE',  ( 0.8538673084422104820, -0.7095216264049221122, 1.829241926910141203 ) ) ;
#150795 = DIRECTION ( 'NONE',  ( 5.578174157656880098E-15, 1.000000000000000000, -7.437565543542506798E-15 ) ) ;
#150796 = CARTESIAN_POINT ( 'NONE',  ( 4.385172619016207918, 7.203452924572514959, 1.199719254218462483 ) ) ;
#150797 = CARTESIAN_POINT ( 'NONE',  ( 0.1753634416057497647, 2.004068818557998011, -2.558292918872175914 ) ) ;
#150798 = VERTEX_POINT ( 'NONE', #203949 ) ;
#150799 = FILL_AREA_STYLE ('',( #130348 ) ) ;
#150800 = ORIENTED_EDGE ( 'NONE', *, *, #11172, .F. ) ;
#150801 = CARTESIAN_POINT ( 'NONE',  ( 3.475094438140493125, -1.599078698050887981, -0.8510578468755282122 ) ) ;
#150802 = ORIENTED_EDGE ( 'NONE', *, *, #133443, .F. ) ;
#150803 = CARTESIAN_POINT ( 'NONE',  ( 5.722423353419669567, 8.833855124701747386, 1.199719254218451159 ) ) ;
#150804 = CARTESIAN_POINT ( 'NONE',  ( 2.898410978271408922, 6.603506251283770112, -0.7998128361456362523 ) ) ;
#150805 = CARTESIAN_POINT ( 'NONE',  ( 5.074790875859057415, -1.308146702057958910, 1.253318493144810697 ) ) ;
#150806 = CARTESIAN_POINT ( 'NONE',  ( 7.010974831598141499, 7.352094523052197239, -0.7216878364870317197 ) ) ;
#150807 = CARTESIAN_POINT ( 'NONE',  ( 5.016205007133085481, 6.569753085731051989, -1.234251006731339917 ) ) ;
#150808 = ADVANCED_FACE ( 'NONE', ( #1478 ), #36131, .F. ) ;
#150810 = CARTESIAN_POINT ( 'NONE',  ( 8.041957671200231417, 12.53403438304231976, 1.040834085586084257E-14 ) ) ;
#150809 = CARTESIAN_POINT ( 'NONE',  ( 6.303157624210896870, -1.571610030290017557, 0.9964359807085266807 ) ) ;
#150811 = EDGE_CURVE ( 'NONE', #200044, #27064, #168505, .T. ) ;
#150812 = CARTESIAN_POINT ( 'NONE',  ( 3.304201903042072175, 1.212927065539553206, -1.482701048864635496 ) ) ;
#150813 = CARTESIAN_POINT ( 'NONE',  ( 4.367134877377630175, 7.148722219365612141, -1.082531754730548412 ) ) ;
#150814 = CARTESIAN_POINT ( 'NONE',  ( -11.88671056400589521, 6.998741290788587754, 4.405061004403326486 ) ) ;
#150815 = CARTESIAN_POINT ( 'NONE',  ( -5.000000000000024869, 0.2350621082554960051, 0.7750000000000117906 ) ) ;
#150816 = CARTESIAN_POINT ( 'NONE',  ( -1.364683531250000748, -1.240624999658580752, 0.000000000000000000 ) ) ;
#150817 =( BOUNDED_CURVE ( )  B_SPLINE_CURVE ( 3, ( #186057, #69092, #49669, #16072 ),
 .UNSPECIFIED., .F., .T. ) 
 B_SPLINE_CURVE_WITH_KNOTS ( ( 4, 4 ),
 ( 1.570796326794897224, 2.200856270442954621 ),
 .UNSPECIFIED. ) 
 CURVE ( )  GEOMETRIC_REPRESENTATION_ITEM ( )  RATIONAL_B_SPLINE_CURVE ( ( 1.000000000000000000, 0.9671913951481618810, 0.9671913951481618810, 1.000000000000000000 ) ) 
 REPRESENTATION_ITEM ( '' )  );
#150818 = CARTESIAN_POINT ( 'NONE',  ( 6.656690234629796699, 6.868486149930637552, 1.040834085586084257E-14 ) ) ;
#150819 = CARTESIAN_POINT ( 'NONE',  ( -2.252626078164912560, 5.779814191167667481, 0.7998128361456341429 ) ) ;
#150820 = CARTESIAN_POINT ( 'NONE',  ( 0.5499753625364013354, 0.6768306982547143136, -2.053065283773393368 ) ) ;
#150821 = CARTESIAN_POINT ( 'NONE',  ( -5.152980901645737077, 8.169505597632108262, -1.199719254218453823 ) ) ;
#150822 = CARTESIAN_POINT ( 'NONE',  ( 5.204350862799327793, 7.165104988056252289, -1.599625672291281386 ) ) ;
#150823 = CARTESIAN_POINT ( 'NONE',  ( 1.237009950130557812, -1.652246606862219025, 0.7767072072360350354 ) ) ;
#150824 = CARTESIAN_POINT ( 'NONE',  ( -4.497554271431319250, 6.270232621468402989, -1.599625672291256295 ) ) ;
#150825 = CARTESIAN_POINT ( 'NONE',  ( 3.293790705515726724, -0.7410340593078694749, 1.668602820345471027 ) ) ;
#150826 = EDGE_CURVE ( 'NONE', #116745, #73904, #9409, .T. ) ;
#150827 = CARTESIAN_POINT ( 'NONE',  ( 9.709990956404908502, 13.29774486163194958, 8.129890332494706939 ) ) ;
#150828 = ORIENTED_EDGE ( 'NONE', *, *, #158729, .F. ) ;
#150829 = CARTESIAN_POINT ( 'NONE',  ( 3.103910798422233608, 0.7114650421483189602, -1.836736179910645195 ) ) ;
#150830 = CARTESIAN_POINT ( 'NONE',  ( 3.878411472391342318, -0.1936643080829789088, -1.932398009575059472 ) ) ;
#150831 = CARTESIAN_POINT ( 'NONE',  ( -7.910256278930404505, 8.193330178365746619, -0.7998128361456362523 ) ) ;
#150833 = CARTESIAN_POINT ( 'NONE',  ( 4.588201236890728119, 1.223260742344203900, 1.732012071221388450 ) ) ;
#150832 = CARTESIAN_POINT ( 'NONE',  ( 6.749980374757213575, 8.968339418673846097, 1.599625672291268286 ) ) ;
#150834 = CARTESIAN_POINT ( 'NONE',  ( 0.06856108760741723429, -7.850763007174482055, 9.549252947205623343 ) ) ;
#150835 = CARTESIAN_POINT ( 'NONE',  ( 7.913155211870404493, 12.38376484715752213, 0.7998128361456462443 ) ) ;
#150836 = CARTESIAN_POINT ( 'NONE',  ( 5.624517712206933417, 6.335738387217328516, 1.153896037602806013 ) ) ;
#150837 = DIRECTION ( 'NONE',  ( 1.207943261119674327E-30, 2.168404344971008079E-15, -1.000000000000000000 ) ) ;
#150838 = CARTESIAN_POINT ( 'NONE',  ( -1.402160292154681736E-14, 12.92187500034139980, 1.575800808251682339 ) ) ;
#150839 = CARTESIAN_POINT ( 'NONE',  ( 5.359550796103802028, 5.147230771742885125, -0.7998128361456231517 ) ) ;
#150840 = CARTESIAN_POINT ( 'NONE',  ( 4.715203562502613188, 8.723097599553565118, 0.7998128361456341429 ) ) ;
#150841 = LINE ( 'NONE', #52259, #134152 ) ;
#150842 = CARTESIAN_POINT ( 'NONE',  ( 5.479063914364931343, -0.04889757770590653918, -1.825204647902956889 ) ) ;
#150843 = CARTESIAN_POINT ( 'NONE',  ( 10.99944587961300257, -9.906575223978485667, -0.1104109902703103996 ) ) ;
#150844 = CARTESIAN_POINT ( 'NONE',  ( -8.459924665247381625, 11.85336729522185806, 1.082531754730560403 ) ) ;
#150845 = CARTESIAN_POINT ( 'NONE',  ( -4.758546912290684716, 8.291040531757728260, 0.8107885835855069834 ) ) ;
#150846 = CARTESIAN_POINT ( 'NONE',  ( -1.922735082439551935, 0.6236244280033473864, -0.2879360613984097150 ) ) ;
#150847 = CARTESIAN_POINT ( 'NONE',  ( 6.104356062600288624, -0.6750377415852754082, -1.744797942764392928 ) ) ;
#150848 = CARTESIAN_POINT ( 'NONE',  ( 8.288111976655649471, 8.563885482386732306, -0.7998128361456291469 ) ) ;
#150849 = CARTESIAN_POINT ( 'NONE',  ( 3.809137074456845795, 1.652770800469059775, 0.9896037298236616264 ) ) ;
#150850 = CARTESIAN_POINT ( 'NONE',  ( 2.977454500823585093, 6.499579965040511276, -0.5808385047149626779 ) ) ;
#150851 = CARTESIAN_POINT ( 'NONE',  ( 3.571683402196252910, 6.254382171615883834, 1.199719254218462483 ) ) ;
#150852 = CARTESIAN_POINT ( 'NONE',  ( 0.6823417656249969321, 9.338541667008065872, -1.181850606188757036 ) ) ;
#150853 = CARTESIAN_POINT ( 'NONE',  ( -6.762819695118240659, 6.784377820593065600, 0.7998128361456341429 ) ) ;
#150854 =( NAMED_UNIT ( * ) SI_UNIT ( $, .STERADIAN. ) SOLID_ANGLE_UNIT ( ) );
#150855 = CARTESIAN_POINT ( 'NONE',  ( -6.084577077482911101, 10.32070003369722144, 0.000000000000000000 ) ) ;
#150856 = CIRCLE ( 'NONE', #202612, 0.08000000000000004330 ) ;
#150857 = CARTESIAN_POINT ( 'NONE',  ( 1.089646232962078853, -0.5102306600231114597, 2.054730298310704750 ) ) ;
#150858 = AXIS2_PLACEMENT_3D ( 'NONE', #112288, #178304, #162049 ) ;
#150859 = CARTESIAN_POINT ( 'NONE',  ( 9.565441069641300587, 11.11843498845840905, -1.199719254218440723 ) ) ;
#150860 = CARTESIAN_POINT ( 'NONE',  ( 0.5988494165465870767, 6.720065942961383598, 3.593421257281793402 ) ) ;
#150861 = CARTESIAN_POINT ( 'NONE',  ( 6.842638490404138629, -2.029097751484234546, -0.4099019697717393163 ) ) ;
#150863 = CARTESIAN_POINT ( 'NONE',  ( 4.009205846845453003, 7.815100513429686480, -0.2297154615349787654 ) ) ;
#150862 = CARTESIAN_POINT ( 'NONE',  ( 1.645803748337611783, 0.5784278848013635344, 1.748079663633335334 ) ) ;
#150864 = CARTESIAN_POINT ( 'NONE',  ( 6.155038550924150087, 7.243595066575396757, 1.082531754730558626 ) ) ;
#150866 = SURFACE_STYLE_USAGE ( .BOTH. , #33890 ) ;
#150865 = CARTESIAN_POINT ( 'NONE',  ( 3.268924434670684498, 6.827845917175511481, -1.734723475976807094E-15 ) ) ;
#150867 = CARTESIAN_POINT ( 'NONE',  ( 1.764052804016162268, 1.181211026566388211, 1.964360346841328209 ) ) ;
#150868 = CARTESIAN_POINT ( 'NONE',  ( -1.284945213870648306, 3.300000000000025135, -0.4778516606550328727 ) ) ;
#150869 = CARTESIAN_POINT ( 'NONE',  ( 5.964781414698055784, 0.1407378593174268555, -1.936906258807554071 ) ) ;
#150870 = VERTEX_POINT ( 'NONE', #67544 ) ;
#150871 = CARTESIAN_POINT ( 'NONE',  ( 7.985389288324691748, 10.33937347451072775, -1.443375672974058777 ) ) ;
#150872 = ADVANCED_FACE ( 'NONE', ( #133687 ), #71844, .F. ) ;
#150873 = CARTESIAN_POINT ( 'NONE',  ( 0.5979028997950117663, 1.355058449971069834, 1.489028425022032698 ) ) ;
#150874 = CARTESIAN_POINT ( 'NONE',  ( 0.5671465430379521999, 1.703994235754960451, 0.9719838849941149217 ) ) ;
#150875 = CARTESIAN_POINT ( 'NONE',  ( -11.86145016429273191, 10.90000000000000036, 1.099999999999996758 ) ) ;
#150877 = CARTESIAN_POINT ( 'NONE',  ( -9.670366421564544623, 3.035553407718987629, -6.557686755922881972 ) ) ;
#150876 = CARTESIAN_POINT ( 'NONE',  ( -7.069687034522070590, 10.33538640932937724, -1.199719254218440723 ) ) ;
#150878 = CARTESIAN_POINT ( 'NONE',  ( -10.30047605039691128, 4.688744718740807116, 5.507884344589919934 ) ) ;
#150880 = CARTESIAN_POINT ( 'NONE',  ( 2.623613022005319984, -1.017049183177589855, -1.448221827668960238 ) ) ;
#150879 = CARTESIAN_POINT ( 'NONE',  ( 4.453126923439646667, 0.4583234712903122565, -2.039610397757870341 ) ) ;
#150881 = CARTESIAN_POINT ( 'NONE',  ( 2.550000000000000266, 1.000000000000000888, -1.849324200890695824 ) ) ;
#150883 = CARTESIAN_POINT ( 'NONE',  ( 5.226663038502143088, 0.1645964690673335229, 2.286419844370500165 ) ) ;
#150882 = CARTESIAN_POINT ( 'NONE',  ( -11.96447454455668513, 7.947521973683856267, 1.052947412299385377 ) ) ;
#150884 = CARTESIAN_POINT ( 'NONE',  ( 2.817972641794503019, 1.638747005868109285, 0.5862587914967545277 ) ) ;
#150885 = CARTESIAN_POINT ( 'NONE',  ( 8.380911511541880188, 12.92948053010758258, 0.7998128361456462443 ) ) ;
#150886 = CARTESIAN_POINT ( 'NONE',  ( 4.213551878797002992, 8.137837301896977849, 0.000000000000000000 ) ) ;
#150887 = CARTESIAN_POINT ( 'NONE',  ( 3.743219424636199832, -1.670416500854546626, -0.4642454339297346078 ) ) ;
#150888 = CARTESIAN_POINT ( 'NONE',  ( 3.930270145471780996, 1.203169952209550919, 1.807132499170207351 ) ) ;
#150889 = CARTESIAN_POINT ( 'NONE',  ( 3.825371897350130723, 7.614684313550482031, 0.7998128361456321445 ) ) ;
#150890 = CARTESIAN_POINT ( 'NONE',  ( 4.891814693739657827, -2.006371927678828104, 0.2024599332275459629 ) ) ;
#150892 = AXIS2_PLACEMENT_3D ( 'NONE', #27164, #192852, #93269 ) ;
#150891 = CARTESIAN_POINT ( 'NONE',  ( 0.4374999999988640753, 1.451031289089056431, -1.451031289061139651 ) ) ;
#150893 = CARTESIAN_POINT ( 'NONE',  ( -1.500000000000011324, 3.952083334016153415, 0.8660254037844403729 ) ) ;
#150894 = CARTESIAN_POINT ( 'NONE',  ( 2.291906413246731944, -0.8257142216546548008, 1.740595036569925647 ) ) ;
#150895 = CARTESIAN_POINT ( 'NONE',  ( -8.012344526598182026E-15, 15.04687500034140157, -1.575800808251669460 ) ) ;
#150896 = CARTESIAN_POINT ( 'NONE',  ( 5.924141181918635368, -2.204746212865996480, 0.2713366554644781603 ) ) ;
#150897 = ORIENTED_EDGE ( 'NONE', *, *, #200985, .F. ) ;
#150898 = CARTESIAN_POINT ( 'NONE',  ( -0.1110810684432986112, 0.002541288824218449188, -1.796853612742685513 ) ) ;
#150899 = CARTESIAN_POINT ( 'NONE',  ( -1.500000000000013101, 1.129166666666688634, -0.8660254037844313801 ) ) ;
#150900 = CARTESIAN_POINT ( 'NONE',  ( 5.666418135507635512, 8.698239360479199433, 1.199719254218462483 ) ) ;
#150901 = CARTESIAN_POINT ( 'NONE',  ( 4.894130264408854458, 6.732904613275549899, -1.443375672974051449 ) ) ;
#150902 = CARTESIAN_POINT ( 'NONE',  ( 1.001543065824772753E-15, -2.121874999522043392, 3.793834371823810780 ) ) ;
#150903 = CARTESIAN_POINT ( 'NONE',  ( 0.8564553275840697255, 0.8952667643853294832, -2.033071718549640305 ) ) ;
#150904 = CARTESIAN_POINT ( 'NONE',  ( 5.705508943770692731, -1.545575431542939970, -1.208212526538715137 ) ) ;
#150905 = CARTESIAN_POINT ( 'NONE',  ( 9.571693261567965294, 10.26932301469188857, 0.7216878364870438212 ) ) ;
#150906 = CARTESIAN_POINT ( 'NONE',  ( 0.2344991881673083867, 3.432054146482980794, 1.989640237496114850 ) ) ;
#150907 = CARTESIAN_POINT ( 'NONE',  ( 0.3511320849261707622, -1.736299752564632204, 1.287366282644891724 ) ) ;
#150908 = CARTESIAN_POINT ( 'NONE',  ( 4.044074958626150185, 7.940114228364351767, 0.7998128361456271485 ) ) ;
#150909 = CARTESIAN_POINT ( 'NONE',  ( -5.370438244788932280, 6.398504386076097283, 1.082531754730549078 ) ) ;
#150910 = CARTESIAN_POINT ( 'NONE',  ( 4.826661651916083429, -1.349687995210807401, 1.559865583710306147 ) ) ;
#150911 = CARTESIAN_POINT ( 'NONE',  ( -5.901876940650454095, 5.779944607047298177, -0.7998128361456291469 ) ) ;
#150912 = B_SPLINE_CURVE_WITH_KNOTS ( 'NONE', 3,
 ( #98472, #165602, #17191, #82206, #199136, #83266, #116909, #182909, #34525, #166673 ),
 .UNSPECIFIED., .F., .F.,
 ( 4, 2, 2, 2, 4 ),
 ( 7.239403734759171957E-05, 0.0003307887970069800987, 0.0005891835566663685591, 0.0008475783163257569110, 0.001105973075985145371 ),
 .UNSPECIFIED. ) ;
#150913 = CARTESIAN_POINT ( 'NONE',  ( -0.7500000000000215383, 3.722916667349487785, 1.299038105676671107 ) ) ;
#150914 = CARTESIAN_POINT ( 'NONE',  ( -0.6823417656250246877, -0.4489583329919111243, 1.181850606188755259 ) ) ;
#150915 = CARTESIAN_POINT ( 'NONE',  ( 6.010993879215096314, 1.649516084216671397, 0.8821100558755521348 ) ) ;
#150916 = CARTESIAN_POINT ( 'NONE',  ( 4.922368227709418065, -1.231479607182428104, -1.221251793340462299 ) ) ;
#150917 = CARTESIAN_POINT ( 'NONE',  ( 4.546296192243603151, -1.394137154979861570, 1.041651924218311986 ) ) ;
#150918 = CARTESIAN_POINT ( 'NONE',  ( -2.373851744317279522, 1.000000000000000888, 11.76285798163022100 ) ) ;
#150919 = EDGE_CURVE ( 'NONE', #142577, #147150, #16499, .T. ) ;
#150920 = CARTESIAN_POINT ( 'NONE',  ( 2.156203017566417302, 0.9840264443441574249, 2.070573632387271434 ) ) ;
#150921 = CARTESIAN_POINT ( 'NONE',  ( 0.6823417656249899377, 3.988541667008085767, -1.181850606188754593 ) ) ;
#150922 = CARTESIAN_POINT ( 'NONE',  ( 5.478101502371197640, -2.040020603162643997, -0.4570242091310200427 ) ) ;
#150923 = CARTESIAN_POINT ( 'NONE',  ( 0.3746297210940018885, 1.718982886236510854, -0.6599183738737608440 ) ) ;
#150924 = AXIS2_PLACEMENT_3D ( 'NONE', #129660, #112323, #63506 ) ;
#150925 = DIRECTION ( 'NONE',  ( -0.6691306063588566833, 0.000000000000000000, 0.7431448254773955764 ) ) ;
#150926 = CARTESIAN_POINT ( 'NONE',  ( 2.004529941291322448, -1.955172360644286789, 0.4926429297785542283 ) ) ;
#150927 = CARTESIAN_POINT ( 'NONE',  ( 0.07648947921621782053, -2.126777779243053779, -0.5280787695999613618 ) ) ;
#150928 = CARTESIAN_POINT ( 'NONE',  ( 9.200879715223321043, 13.24877694306529641, -9.037004148943696080 ) ) ;
#150929 = CARTESIAN_POINT ( 'NONE',  ( -8.148614017013223076, 9.465470093725620870, -1.199719254218446718 ) ) ;
#150930 = CARTESIAN_POINT ( 'NONE',  ( 6.979750152936881058, 7.037463354714830643, 0.7998128361456341429 ) ) ;
#150931 = CARTESIAN_POINT ( 'NONE',  ( 2.332823983099761911, 1.383068002389773454, -1.607457772141835717 ) ) ;
#150932 = CARTESIAN_POINT ( 'NONE',  ( -0.6823417656250003738, -1.032291666325242607, -1.181850606188749264 ) ) ;
#150934 = EDGE_CURVE ( 'NONE', #45474, #48843, #103284, .T. ) ;
#150933 = CARTESIAN_POINT ( 'NONE',  ( 5.285714101943871590, 1.228958891529348785, 1.350286652578087665 ) ) ;
#150935 = ORIENTED_EDGE ( 'NONE', *, *, #59473, .F. ) ;
#150936 = CARTESIAN_POINT ( 'NONE',  ( -5.420227550413282636, 9.545625585449309725, 0.7998128361456291469 ) ) ;
#150937 = CARTESIAN_POINT ( 'NONE',  ( -0.003385325826195171531, 8.210945192570349604, -2.038658773260200174 ) ) ;
#150938 = CARTESIAN_POINT ( 'NONE',  ( -1.642778471874998480, -1.188541666188709600, 2.845375778867863303 ) ) ;
#150939 = CARTESIAN_POINT ( 'NONE',  ( -5.799137018343247796, 7.788745826199009237, -1.599625672291256295 ) ) ;
#150940 = CARTESIAN_POINT ( 'NONE',  ( 3.146744605306639908, 1.971464920705681800, 0.4384460897248109723 ) ) ;
#150941 = CARTESIAN_POINT ( 'NONE',  ( 0.2707219772894990384, -1.375384669632748524, 1.594866825539154043 ) ) ;
#150942 = CARTESIAN_POINT ( 'NONE',  ( -5.144392941742557568, 4.966489618313220333, -0.7998128361456362523 ) ) ;
#150943 = CARTESIAN_POINT ( 'NONE',  ( 3.608110912359719258, 1.861131631771815842, 0.004268880383616681894 ) ) ;
#150944 = CARTESIAN_POINT ( 'NONE',  ( 9.890836756369282057, 11.49806328964105617, -1.199719254218440723 ) ) ;
#150945 = CARTESIAN_POINT ( 'NONE',  ( 11.89321938400721379, 13.76255278360646983, -1.599605898944101323 ) ) ;
#150946 = CARTESIAN_POINT ( 'NONE',  ( -2.903417451620861289, 6.539070793532962611, 0.7998128361456341429 ) ) ;
#150947 = CARTESIAN_POINT ( 'NONE',  ( -6.723954117373590833, 9.932031339322813679, -1.199719254218440723 ) ) ;
#150949 = CARTESIAN_POINT ( 'NONE',  ( -4.474540158260005285, 7.266292661500576955, 1.287230779100386968 ) ) ;
#150948 = CARTESIAN_POINT ( 'NONE',  ( -6.074935347375019390, 9.245119117649618801, 1.199719254218452047 ) ) ;
#150950 = CARTESIAN_POINT ( 'NONE',  ( -1.402160292154681736E-14, -0.8031249996585825279, -1.575800808251665908 ) ) ;
#150951 = CARTESIAN_POINT ( 'NONE',  ( 1.985274739808037481, 1.615814429867837410, 0.6292545280836835397 ) ) ;
#150952 = CARTESIAN_POINT ( 'NONE',  ( 1.130330966444204277, -1.574854822160208556, 0.7409792249596267588 ) ) ;
#150954 = CARTESIAN_POINT ( 'NONE',  ( 7.619319141200057821, 10.87266085050000974, 1.082531754730557072 ) ) ;
#150953 = CARTESIAN_POINT ( 'NONE',  ( 6.568959576340373197, -2.106780069790818555, -0.9421804820441375128 ) ) ;
#150955 = CARTESIAN_POINT ( 'NONE',  ( 4.927462483923885195, 4.713404084191450849, -0.7998128361456481317 ) ) ;
#150956 = CARTESIAN_POINT ( 'NONE',  ( 1.282574848904423082, -2.009897191344016232, -0.4543217371432185514 ) ) ;
#150957 = CARTESIAN_POINT ( 'NONE',  ( 6.749376085230743172, -2.252018642839793472, -0.4587488502729390460 ) ) ;
#150958 = CARTESIAN_POINT ( 'NONE',  ( -11.33772463945036968, 10.19999999999999929, -3.600000000000000977 ) ) ;
#150959 = CARTESIAN_POINT ( 'NONE',  ( -6.147696309153835692, 6.137010213626392208, 0.7998128361456281477 ) ) ;
#150960 = EDGE_CURVE ( 'NONE', #16328, #4563, #135791, .T. ) ;
#150961 = CARTESIAN_POINT ( 'NONE',  ( 0.3738188115672124168, 1.133047686669987675, 1.613170723887060065 ) ) ;
#150963 = CARTESIAN_POINT ( 'NONE',  ( -7.282137904315833410, 7.668451441222825515, 0.000000000000000000 ) ) ;
#150962 = CARTESIAN_POINT ( 'NONE',  ( 4.816621285000030284, -0.6497861859515661198, -1.798733151862880186 ) ) ;
#150964 = CARTESIAN_POINT ( 'NONE',  ( 5.795608111622330583, 1.668732747960173235, 1.444295198399044855 ) ) ;
#150965 = CARTESIAN_POINT ( 'NONE',  ( -1.225000000000032285, 1.833333334016213012, 0.7072540797572777205 ) ) ;
#150966 = DIRECTION ( 'NONE',  ( 0.000000000000000000, 0.000000000000000000, -1.000000000000000000 ) ) ;
#150967 = CARTESIAN_POINT ( 'NONE',  ( 4.299344108864946890, 6.109263775132799168, -1.443375672974068769 ) ) ;
#150968 = CARTESIAN_POINT ( 'NONE',  ( -6.583366107887490770, 9.838288338247510367, 1.199719254218452935 ) ) ;
#150969 = CARTESIAN_POINT ( 'NONE',  ( -0.1106727585415967219, -0.002281114264979232885, -2.003378291782103471 ) ) ;
#150970 = CARTESIAN_POINT ( 'NONE',  ( 3.786388324757625323, -1.140120265720317327, 2.006200910446949592 ) ) ;
#150971 = CARTESIAN_POINT ( 'NONE',  ( 4.598074495912658044, 0.8407358649686399454, -1.772743347989129692 ) ) ;
#150972 = CARTESIAN_POINT ( 'NONE',  ( 0.7077677203753615087, 0.6208407433182620005, -1.860969989990405749 ) ) ;
#150973 = DIRECTION ( 'NONE',  ( -0.000000000000000000, 1.000000000000000000, -0.000000000000000000 ) ) ;
#150974 = CARTESIAN_POINT ( 'NONE',  ( 10.12374542407609290, -16.99999999999999645, -4.551898349974266011 ) ) ;
#150975 = ORIENTED_EDGE ( 'NONE', *, *, #59704, .T. ) ;
#150976 = CARTESIAN_POINT ( 'NONE',  ( 0.1810649180928698143, 1.756560269771380911, -1.181951075121101979 ) ) ;
#150978 = CARTESIAN_POINT ( 'NONE',  ( -8.670602931139386627, 10.07445716020612103, 1.199719254218462483 ) ) ;
#150977 = CARTESIAN_POINT ( 'NONE',  ( -5.773074481320628948, 5.629675071162500544, 0.000000000000000000 ) ) ;
#150979 = SURFACE_STYLE_FILL_AREA ( #84892 ) ;
#150981 = AXIS2_PLACEMENT_3D ( 'NONE', #147300, #48732, #180843 ) ;
#150980 = CARTESIAN_POINT ( 'NONE',  ( 2.747136105846450516, -0.3671824478193272956, -2.139636267262314373 ) ) ;
#150982 = CARTESIAN_POINT ( 'NONE',  ( -0.2036233647782254297, 2.640173713333016536, 2.069169101323902193 ) ) ;
#150983 = CARTESIAN_POINT ( 'NONE',  ( 0.1586465271753433603, 2.115359532055087310, 0.1496401998123952359 ) ) ;
#150984 = CARTESIAN_POINT ( 'NONE',  ( -0.7500000000000215383, 2.972916667349487341, 1.299038105676671107 ) ) ;
#150985 = CARTESIAN_POINT ( 'NONE',  ( 8.890396042259068210, 11.39521468743417998, -1.599625672291257406 ) ) ;
#150986 = CARTESIAN_POINT ( 'NONE',  ( 11.86145016429272836, 13.40000000000000036, -1.100000000000000533 ) ) ;
#150987 = CARTESIAN_POINT ( 'NONE',  ( 6.463557619869761517, 6.860074278669063830, -0.6545079704341187909 ) ) ;
#150988 = CARTESIAN_POINT ( 'NONE',  ( 2.618495166727810908, 1.348686541216067347, -1.558216953862724408 ) ) ;
#150990 = CARTESIAN_POINT ( 'NONE',  ( 7.106142513049811704, 14.54891773411305245, -9.615630241012095070 ) ) ;
#150989 = CARTESIAN_POINT ( 'NONE',  ( -8.503988664269602538, 10.94440607977979063, 1.599625672291269396 ) ) ;
#150991 = CARTESIAN_POINT ( 'NONE',  ( -0.6823417656250212460, 2.051041667008083991, 1.181850606188767472 ) ) ;
#150992 = CARTESIAN_POINT ( 'NONE',  ( 0.07755575628181492209, 4.082361791518872352, -2.743585103993382734 ) ) ;
#150993 = CARTESIAN_POINT ( 'NONE',  ( -4.952636518945644717, 6.537114055553945313, 2.442608363190701404 ) ) ;
#150994 = VERTEX_POINT ( 'NONE', #54532 ) ;
#150995 = CARTESIAN_POINT ( 'NONE',  ( 4.477155480220369910, -1.709698060584059043, -0.8567103784868702610 ) ) ;
#150996 = CARTESIAN_POINT ( 'NONE',  ( 1.220146605508150803E-14, 9.468750000682799595, -1.499999999999998446 ) ) ;
#150997 = CARTESIAN_POINT ( 'NONE',  ( 1.739923964384773258, -1.638176463808267647, -1.560613564838263523 ) ) ;
#150998 = CARTESIAN_POINT ( 'NONE',  ( -2.428882075142555497, 5.985446187641602300, 1.040834085586084257E-14 ) ) ;
#150999 = CARTESIAN_POINT ( 'NONE',  ( 1.828075118979434865, -0.8562131971674535880, -1.596496639089627578 ) ) ;
#151000 = CARTESIAN_POINT ( 'NONE',  ( 0.5849901852424718163, 1.567898511244028459, 1.100480585720535087 ) ) ;
#151001 = CARTESIAN_POINT ( 'NONE',  ( 1.504437137538238600, 2.067909592606699487, 0.1035681241481553605 ) ) ;
#151002 = CARTESIAN_POINT ( 'NONE',  ( 1.364683531249986537, 0.2177083336747502595, -0.7879004041258309554 ) ) ;
#151003 = CARTESIAN_POINT ( 'NONE',  ( 0.2683544108190681898, -1.289511475198481305, 1.491327623740832387 ) ) ;
#151004 = CARTESIAN_POINT ( 'NONE',  ( 6.059198490463121090, -1.653572398999035853, -0.9882694798356050914 ) ) ;
#151006 = CARTESIAN_POINT ( 'NONE',  ( 5.551963943121584144, 7.421064284658021037, -1.246246109899084020 ) ) ;
#151005 = CARTESIAN_POINT ( 'NONE',  ( 6.551417122825020201, -1.769646310455678995, -1.318412661681533260 ) ) ;
#151007 = CARTESIAN_POINT ( 'NONE',  ( -0.6823417656250212460, 1.801041667008083991, 1.181850606188755259 ) ) ;
#151008 = AXIS2_PLACEMENT_3D ( 'NONE', #105751, #171778, #136088 ) ;
#151009 = CARTESIAN_POINT ( 'NONE',  ( 4.650865732144216835, -0.4487226328800034691, -2.013136760839563166 ) ) ;
#151010 = CARTESIAN_POINT ( 'NONE',  ( -7.413611068574208041, 7.543634422958360730, 0.7998128361456341429 ) ) ;
#151011 = CARTESIAN_POINT ( 'NONE',  ( 8.599949509769960088, 8.927695937686774386, 1.040834085586084257E-14 ) ) ;
#151012 = CARTESIAN_POINT ( 'NONE',  ( -1.217358635584817383, 2.889784080462333371, 0.7750000000000083489 ) ) ;
#151013 =( BOUNDED_CURVE ( )  B_SPLINE_CURVE ( 3, ( #168969, #133313, #70376, #120301 ),
 .UNSPECIFIED., .F., .T. ) 
 B_SPLINE_CURVE_WITH_KNOTS ( ( 4, 4 ),
 ( 0.4999999999999988898, 1.000000000000000000 ),
 .UNSPECIFIED. ) 
 CURVE ( )  GEOMETRIC_REPRESENTATION_ITEM ( )  RATIONAL_B_SPLINE_CURVE ( ( 1.000000000000001554, 0.3333333333333333703, 0.3333333333333318715, 1.000000000000000000 ) ) 
 REPRESENTATION_ITEM ( '' )  );
#151014 = CARTESIAN_POINT ( 'NONE',  ( 3.994848817520957773, 7.812407387083109001, 1.040834085586084257E-14 ) ) ;
#151016 = CARTESIAN_POINT ( 'NONE',  ( -1.499999999999997780, 3.150000000000020783, 1.214306433183764966E-14 ) ) ;
#151015 = CARTESIAN_POINT ( 'NONE',  ( 5.069407556592405939, 0.2091588727727889396, -2.095552839448256766 ) ) ;
#151017 = MECHANICAL_DESIGN_GEOMETRIC_PRESENTATION_REPRESENTATION (  '', ( #178682 ), #57611 ) ;
#151018 = CARTESIAN_POINT ( 'NONE',  ( 0.8015275938294207370, -1.862055209299150249, 1.116337150347948892 ) ) ;
#151019 = CARTESIAN_POINT ( 'NONE',  ( 0.6823417656249899377, 0.9052083336747520637, 1.181850606188755259 ) ) ;
#151020 = CARTESIAN_POINT ( 'NONE',  ( 4.798204600472657511, -2.160985683756014630, -0.05834674948757002932 ) ) ;
#151021 = CARTESIAN_POINT ( 'NONE',  ( 5.637369771878480762, -0.04735730112789998669, 2.019284605405778255 ) ) ;
#151022 = CARTESIAN_POINT ( 'NONE',  ( -0.1399997263889819488, 4.088450529495776919, -2.555104583160577647 ) ) ;
#151025 = CARTESIAN_POINT ( 'NONE',  ( 5.992340707560160240, 7.053780915984068756, 1.082531754730558626 ) ) ;
#151024 = CARTESIAN_POINT ( 'NONE',  ( 3.285556943749998737, -2.355208332855375453, -1.896917185911906500 ) ) ;
#151023 = CARTESIAN_POINT ( 'NONE',  ( -8.120144897977780829, 14.55205941280230242, -8.786172316246053882 ) ) ;
#151026 = CARTESIAN_POINT ( 'NONE',  ( -5.956828388357799042, 8.042995434541133193, 1.599625672291263179 ) ) ;
#151027 = CARTESIAN_POINT ( 'NONE',  ( 3.714077560468319827, 1.074663192196689376, -1.706111893292367343 ) ) ;
#151028 = CARTESIAN_POINT ( 'NONE',  ( -7.479294296233107708, 11.87759377891399204, 0.7998128361456481317 ) ) ;
#151030 = DIRECTION ( 'NONE',  ( 0.000000000000000000, 0.000000000000000000, 1.000000000000000000 ) ) ;
#151029 = CARTESIAN_POINT ( 'NONE',  ( -4.939248034080176097, 4.656877549381960080, 1.214306433183764966E-14 ) ) ;
#151032 = CARTESIAN_POINT ( 'NONE',  ( -11.94651559118242901, 12.44869344121018173, -1.135242698369575587 ) ) ;
#151031 = CARTESIAN_POINT ( 'NONE',  ( 4.733375416736937069, -1.977748744329570263, 0.8730265686548792647 ) ) ;
#151033 =( LENGTH_UNIT ( ) NAMED_UNIT ( * ) SI_UNIT ( .MILLI., .METRE. ) );
#151034 = DIRECTION ( 'NONE',  ( 0.000000000000000000, 0.000000000000000000, 1.000000000000000000 ) ) ;
#151036 = CARTESIAN_POINT ( 'NONE',  ( 4.341422844945469706, 0.4390097190783425196, -1.967893369681630311 ) ) ;
#151035 = CARTESIAN_POINT ( 'NONE',  ( -7.334597914868735025, 9.580116872145431728, -1.443375672974058777 ) ) ;
#151037 = CARTESIAN_POINT ( 'NONE',  ( -0.7500000000000215383, 5.191666666666685082, 1.299038105676671107 ) ) ;
#151038 = CARTESIAN_POINT ( 'NONE',  ( 1.119288186499637794, -1.683610015651057168, 0.3742365367947718124 ) ) ;
#151039 = CARTESIAN_POINT ( 'NONE',  ( 5.682802662783380754, 6.658966523782627434, 1.199719254218452935 ) ) ;
#151041 = CARTESIAN_POINT ( 'NONE',  ( -11.89942855770813956, 9.719999999999998863, 0.6999999999999992895 ) ) ;
#151040 = CARTESIAN_POINT ( 'NONE',  ( 8.107412671292035355, 10.48173408797264194, 1.443375672974076540 ) ) ;
#151042 = CARTESIAN_POINT ( 'NONE',  ( -5.593777659986292505, 7.397990072842402398, -1.241664499109219166 ) ) ;
#151043 = CARTESIAN_POINT ( 'NONE',  ( 5.044154037833219029, 1.865456107639616556, 0.1390639465682907416 ) ) ;
#151044 = CARTESIAN_POINT ( 'NONE',  ( 6.064703285670603350, 0.6354670234634349768, 1.910320939954947228 ) ) ;
#151045 = DIRECTION ( 'NONE',  ( 0.000000000000000000, 0.000000000000000000, -1.000000000000000000 ) ) ;
#151046 = AXIS2_PLACEMENT_3D ( 'NONE', #192587, #42120, #45306 ) ;
#151047 = CARTESIAN_POINT ( 'NONE',  ( -6.916067756302494374, 7.241369601873926420, 0.000000000000000000 ) ) ;
#151048 = ORIENTED_EDGE ( 'NONE', *, *, #83695, .F. ) ;
#151049 = CARTESIAN_POINT ( 'NONE',  ( 9.151390499099949949, 12.66007743471656788, -1.082531754730543971 ) ) ;
#151051 = CARTESIAN_POINT ( 'NONE',  ( 0.2281389574181335589, 2.011207032379238591, 0.1455110067964115739 ) ) ;
#151050 = CARTESIAN_POINT ( 'NONE',  ( 1.840644454891388282, 1.218392294859267144, -1.735325642819862013 ) ) ;
#151052 = CARTESIAN_POINT ( 'NONE',  ( 1.599580717682536291, 1.250984903983554997, 1.310507481138773800 ) ) ;
#151053 = CARTESIAN_POINT ( 'NONE',  ( 8.011942431032855083, 8.311964022485323511, 0.7998128361456291469 ) ) ;
#151054 = CARTESIAN_POINT ( 'NONE',  ( 6.491117449447131982, 1.883434485765375310, -1.060826435891427666 ) ) ;
#151055 = ORIENTED_EDGE ( 'NONE', *, *, #150235, .T. ) ;
#151057 = EDGE_CURVE ( 'NONE', #74053, #14390, #92628, .T. ) ;
#151056 = TOROIDAL_SURFACE ( 'NONE', #182103, 1.600000000000000311, 0.1000000000000000056 ) ;
#151058 = PRODUCT_DEFINITION ( 'UNKNOWN', '', #131830, #132740 ) ;
#151059 = CARTESIAN_POINT ( 'NONE',  ( 6.103141704446003679, 10.27208242182903142, 0.7998128361456462443 ) ) ;
#151061 = CARTESIAN_POINT ( 'NONE',  ( 0.5674276921618210956, 1.288973137450568407, 1.417358193720698933 ) ) ;
#151060 = CARTESIAN_POINT ( 'NONE',  ( -6.091691091241777656, 6.001394449403842479, 0.7998128361456341429 ) ) ;
#151062 = CARTESIAN_POINT ( 'NONE',  ( 1.872340672757953906, 8.979957301293506333, 0.7750000000000004663 ) ) ;
#151063 = CARTESIAN_POINT ( 'NONE',  ( 0.000000000000000000, 8.999999999999998224, 0.000000000000000000 ) ) ;
#151064 = CARTESIAN_POINT ( 'NONE',  ( -0.6823417656250003738, -0.7197916663252492686, -1.181850606188749264 ) ) ;
#151065 = CARTESIAN_POINT ( 'NONE',  ( 4.229780737783593203, 4.037091736943370535, -0.7216878364870188411 ) ) ;
#151066 = CARTESIAN_POINT ( 'NONE',  ( -4.322352044658376968, 3.937165561723182883, 0.7998128361456341429 ) ) ;
#151067 = AXIS2_PLACEMENT_3D ( 'NONE', #22726, #201473, #167938 ) ;
#151068 = CARTESIAN_POINT ( 'NONE',  ( 4.047864428982482110, 0.7307185629543844207, -2.034579650689218866 ) ) ;
#151069 = CARTESIAN_POINT ( 'NONE',  ( -6.956742217587851052, 7.288823140040177506, 0.000000000000000000 ) ) ;
#151070 = CARTESIAN_POINT ( 'NONE',  ( 5.560252395380206103, 8.540692657035327429, 1.082531754730547524 ) ) ;
#151071 = CARTESIAN_POINT ( 'NONE',  ( 2.461320219219771843, -1.760565900816572826, 1.181798851529712646 ) ) ;
#151072 = CARTESIAN_POINT ( 'NONE',  ( 6.387720234973090605, 1.261301916940280154, 1.320039730931761524 ) ) ;
#151073 = CARTESIAN_POINT ( 'NONE',  ( 2.407442502341358814, -0.4355224260998523111, 1.922489325443673236 ) ) ;
#151074 = ORIENTED_EDGE ( 'NONE', *, *, #165074, .F. ) ;
#151075 = CYLINDRICAL_SURFACE ( 'NONE', #159965, 8.500000000000000000 ) ;
#151076 = CARTESIAN_POINT ( 'NONE',  ( 6.021921669442146907, 1.940670798679052123, -0.3350140356708011802 ) ) ;
#151077 = CARTESIAN_POINT ( 'NONE',  ( 1.148265734048327769, -1.531264750074516234, 1.194210492925862344 ) ) ;
#151078 = ORIENTED_EDGE ( 'NONE', *, *, #122616, .F. ) ;
#151079 = CARTESIAN_POINT ( 'NONE',  ( -5.795184315198522285, 5.725746220678519904, -0.7998128361456362523 ) ) ;
#151081 = CARTESIAN_POINT ( 'NONE',  ( 6.701130152864326561, -6.864242550357417372, -6.729185449012855535 ) ) ;
#151080 = CARTESIAN_POINT ( 'NONE',  ( -5.939880696562884310, 9.943961556049767836, 0.7216878364870267237 ) ) ;
#151083 = CARTESIAN_POINT ( 'NONE',  ( 6.346625304528514810, 6.577020074804287297, 0.000000000000000000 ) ) ;
#151082 = CARTESIAN_POINT ( 'NONE',  ( 7.579171565239241737, 8.801120566655981747, 1.199719254218462483 ) ) ;
#151085 = VERTEX_POINT ( 'NONE', #18806 ) ;
#151084 = CARTESIAN_POINT ( 'NONE',  ( 4.652931681422667332, 0.3304644650514582116, 1.883354098946861344 ) ) ;
#151086 = CARTESIAN_POINT ( 'NONE',  ( 3.756632125300945368, 0.7937082651479386852, 2.059386989456575279 ) ) ;
#151087 = CARTESIAN_POINT ( 'NONE',  ( 1.800138458411651765, -0.7431416638853624024, 2.077998897882806784 ) ) ;
#151088 = CARTESIAN_POINT ( 'NONE',  ( 0.3000000002818084543, 3.198312376128888079, -0.5146719259196330665 ) ) ;
#151089 = CARTESIAN_POINT ( 'NONE',  ( 1.031728963041964153, -1.865498905729731316, 0.4196304693004496156 ) ) ;
#151091 =( BOUNDED_CURVE ( )  B_SPLINE_CURVE ( 3, ( #70546, #123695, #55397, #151844 ),
 .UNSPECIFIED., .F., .T. ) 
 B_SPLINE_CURVE_WITH_KNOTS ( ( 4, 4 ),
 ( 0.001563600248854528623, 0.002072481089630083019 ),
 .UNSPECIFIED. ) 
 CURVE ( )  GEOMETRIC_REPRESENTATION_ITEM ( )  RATIONAL_B_SPLINE_CURVE ( ( 0.9992558763692048762, 0.7599451551847443698, 0.6066669034981619912, 0.5394211213094574076 ) ) 
 REPRESENTATION_ITEM ( '' )  );
#151090 = CARTESIAN_POINT ( 'NONE',  ( 0.07661050522430287724, 1.422454998960010153, -1.972067596371825715 ) ) ;
#151092 = CARTESIAN_POINT ( 'NONE',  ( 0.4294425147611369287, -9.006862915010142245, -9.490288674561773163 ) ) ;
#151093 = CARTESIAN_POINT ( 'NONE',  ( 6.845108005540235574, -7.986884274785875704, -6.643335646896346702 ) ) ;
#151094 = CARTESIAN_POINT ( 'NONE',  ( 2.963400493335893504, 1.747644659881589568, 1.109742091278065113 ) ) ;
#151095 = CARTESIAN_POINT ( 'NONE',  ( -4.550733115681270036, 8.460939068270139529, 0.7998128361456481317 ) ) ;
#151096 = CARTESIAN_POINT ( 'NONE',  ( -4.976059700032323896, 7.958698620104867061, 1.042642055368933285 ) ) ;
#151098 = CARTESIAN_POINT ( 'NONE',  ( 0.6554165194554737450, -1.826866057147133349, -1.155366728873077342 ) ) ;
#151097 = CARTESIAN_POINT ( 'NONE',  ( -4.765854690403601879, 5.518917546014321829, 1.199719254218462483 ) ) ;
#151099 = CARTESIAN_POINT ( 'NONE',  ( 3.685266855566126321, 1.588411730319793769, 1.510178839762461811 ) ) ;
#151100 = CARTESIAN_POINT ( 'NONE',  ( -0.4365480345679259022, -0.9795170267801369679, 3.437609648208244106 ) ) ;
#151101 = CARTESIAN_POINT ( 'NONE',  ( 3.092668437693027794, 6.622213920701574885, -0.7216878364870338292 ) ) ;
#151102 = FACE_OUTER_BOUND ( 'NONE', #163706, .T. ) ;
#151103 = CARTESIAN_POINT ( 'NONE',  ( 1.364683531249997417, 13.79687500034139980, 2.602085213965210642E-15 ) ) ;
#151104 = CARTESIAN_POINT ( 'NONE',  ( -6.466312919074983512, 6.508729591867735031, -0.7998128361456362523 ) ) ;
#151105 = CARTESIAN_POINT ( 'NONE',  ( 6.205661552121055635, 1.621658882679182456, 0.6149916719311411262 ) ) ;
#151106 = CARTESIAN_POINT ( 'NONE',  ( -9.408995418203979000, 12.00024729270324286, 1.443375672974076540 ) ) ;
#151107 = CARTESIAN_POINT ( 'NONE',  ( 3.889561532384704368, -1.914723906051108537, 0.7877538119766481772 ) ) ;
#151108 = CARTESIAN_POINT ( 'NONE',  ( 4.394233635046361108, -0.9068805580662200327, -1.913321081533605028 ) ) ;
#151109 = CARTESIAN_POINT ( 'NONE',  ( 6.368579470117202490, 8.453095353268645695, 1.599625672291281386 ) ) ;
#151110 = CARTESIAN_POINT ( 'NONE',  ( 0.6823417656249917140, 4.092708333674755394, 1.181850606188765695 ) ) ;
#151111 = CARTESIAN_POINT ( 'NONE',  ( 2.518351277774394159, 0.8375136450692384216, 1.782609909039992946 ) ) ;
#151112 = CARTESIAN_POINT ( 'NONE',  ( 0.2988868148526523938, -0.2362956723594503705, -1.897694653714178781 ) ) ;
#151113 = CARTESIAN_POINT ( 'NONE',  ( 4.699361189290715224, -0.6141998521675575695, 2.208390280175839049 ) ) ;
#151114 = CARTESIAN_POINT ( 'NONE',  ( 3.158640206316553289, -1.382037546686708973, 1.193037399656725395 ) ) ;
#151115 = CARTESIAN_POINT ( 'NONE',  ( 4.390861645979372341, 6.216034235099629157, -1.599625672291269396 ) ) ;
#151116 = CARTESIAN_POINT ( 'NONE',  ( 5.246642258364164313, 8.104537820524768676, -1.082531754730549078 ) ) ;
#151117 = CARTESIAN_POINT ( 'NONE',  ( -5.910464900553636269, 8.982960586366182554, -1.199719254218440723 ) ) ;
#151118 = ORIENTED_EDGE ( 'NONE', *, *, #78415, .F. ) ;
#151119 = CARTESIAN_POINT ( 'NONE',  ( 3.726818050638240898, 1.420666359685630598, -1.426677609031762994 ) ) ;
#151120 = CARTESIAN_POINT ( 'NONE',  ( 3.977359813172594905, -0.1486911861427446802, 1.956209631609528099 ) ) ;
#151121 = CARTESIAN_POINT ( 'NONE',  ( -6.347188469492005325, 10.55680364771601809, -0.7998128361456291469 ) ) ;
#151122 = B_SPLINE_CURVE_WITH_KNOTS ( 'NONE', 3,
 ( #16008, #65816, #50671, #53881, #37624, #82094, #148187 ),
 .UNSPECIFIED., .F., .F.,
 ( 4, 3, 4 ),
 ( 0.0001788552925466792450, 0.0009000000022260257627, 0.002103779968145169134 ),
 .UNSPECIFIED. ) ;
#151123 = CARTESIAN_POINT ( 'NONE',  ( -5.762378981008047241, 6.681529218386182301, 1.199719254218450271 ) ) ;
#151124 = CARTESIAN_POINT ( 'NONE',  ( 0.07536363704233395300, 5.720741966631408104, -2.738263776839637398 ) ) ;
#151126 = CARTESIAN_POINT ( 'NONE',  ( 5.524192064727496465, 1.051792464684684347, -1.423223091708211818 ) ) ;
#151125 = CARTESIAN_POINT ( 'NONE',  ( 0.01142647129402651375, -2.049560973810752085, 0.4120210816158270117 ) ) ;
#151127 = CARTESIAN_POINT ( 'NONE',  ( 2.097856687836355150, -2.190910012095201420, 0.05558666267656967030 ) ) ;
#151128 = CARTESIAN_POINT ( 'NONE',  ( 0.01074006189176902708, -1.707493591921129372, 0.3360247309564004525 ) ) ;
#151129 = CARTESIAN_POINT ( 'NONE',  ( 7.124973419181436007, 8.271222729588529887, -1.199719254218446718 ) ) ;
#151130 = CARTESIAN_POINT ( 'NONE',  ( 0.2335667940002476017, 0.2385907455819072931, -2.187945659632169804 ) ) ;
#151131 = CARTESIAN_POINT ( 'NONE',  ( 0.1524156081505250449, -1.388816673012055025, 1.022707173280016368 ) ) ;
#151132 = CARTESIAN_POINT ( 'NONE',  ( 0.7733716040702149908, -2.287020594544288521, 0.2280439049123609840 ) ) ;
#151133 = CARTESIAN_POINT ( 'NONE',  ( 1.013517375116283592, -2.137022957946862700, 0.4851717564131745597 ) ) ;
#151134 = CARTESIAN_POINT ( 'NONE',  ( 6.345060247669167097, -0.9239052495037097801, 1.466952517609141138 ) ) ;
#151135 = CARTESIAN_POINT ( 'NONE',  ( 2.895379187063460424, 1.892502543702856865, -1.135010264495312837 ) ) ;
#151136 = CARTESIAN_POINT ( 'NONE',  ( 6.531686450800388677, 2.079676181002787061, -0.6237389289161490158 ) ) ;
#151137 = CARTESIAN_POINT ( 'NONE',  ( 1.341172884435502866, -1.819006327537198153, -1.083427034744638862 ) ) ;
#151138 = CARTESIAN_POINT ( 'NONE',  ( 6.827182134110235445, 7.051404648315344303, 2.887205390314013354 ) ) ;
#151139 = CARTESIAN_POINT ( 'NONE',  ( 4.999011269523485623, 1.601735033023284904, -1.069960431631542752 ) ) ;
#151140 = ORIENTED_EDGE ( 'NONE', *, *, #16981, .F. ) ;
#151142 = CARTESIAN_POINT ( 'NONE',  ( 1.499999999999989120, 5.295833333333356485, -0.8660254037844323793 ) ) ;
#151141 = CARTESIAN_POINT ( 'NONE',  ( 1.417954980037740009, -1.278267931767061771, -1.902717450791486353 ) ) ;
#151143 = CARTESIAN_POINT ( 'NONE',  ( 4.630273154266905777, 5.360739087188218122, 1.199719254218464037 ) ) ;
#151144 = CARTESIAN_POINT ( 'NONE',  ( 6.114890974963323345, 7.092793211334054604, 1.199719254218462483 ) ) ;
#151145 = CARTESIAN_POINT ( 'NONE',  ( 5.197972062552532080, 1.490711083722006780, 1.646940351458234808 ) ) ;
#151146 = CARTESIAN_POINT ( 'NONE',  ( -7.212574532790092974, 10.39812547402169862, -1.082531754730543971 ) ) ;
#151147 = CARTESIAN_POINT ( 'NONE',  ( 4.961921032921539521, 7.772363057508363759, -1.082531754730549078 ) ) ;
#151148 = CARTESIAN_POINT ( 'NONE',  ( -8.636180661780672452, 9.177891648273343250, -0.7216878364870267237 ) ) ;
#151149 = CARTESIAN_POINT ( 'NONE',  ( 6.699137298928158124, 6.988284068270579574, 0.7216878364870328300 ) ) ;
#151150 =( GEOMETRIC_REPRESENTATION_CONTEXT ( 3 ) GLOBAL_UNCERTAINTY_ASSIGNED_CONTEXT ( ( #206582 ) ) GLOBAL_UNIT_ASSIGNED_CONTEXT ( ( #123017, #89362, #181252 ) ) REPRESENTATION_CONTEXT ( 'NONE', 'WORKASPACE' ) );
#151151 = CARTESIAN_POINT ( 'NONE',  ( 2.777970385693105726, 1.728001979019553325, -1.038993764437286416 ) ) ;
#151153 = CARTESIAN_POINT ( 'NONE',  ( 0.6903719162679988752, 1.063636609032023950, -1.767059929103020677 ) ) ;
#151152 = CARTESIAN_POINT ( 'NONE',  ( 7.182068686937156166, 9.402166106225269715, 1.599625672291281386 ) ) ;
#151154 = CARTESIAN_POINT ( 'NONE',  ( 4.892487020634524342, 4.880525410245029505, -1.277330582746047388E-09 ) ) ;
#151155 = CARTESIAN_POINT ( 'NONE',  ( 5.519577934094851202, 8.493239118869080784, 1.082531754730547524 ) ) ;
#151156 = DIRECTION ( 'NONE',  ( 0.000000000000000000, 8.546850786086437571E-32, 1.000000000000000000 ) ) ;
#151157 = CARTESIAN_POINT ( 'NONE',  ( 0.6823417656249899377, 3.092708333674754062, 1.181850606188765695 ) ) ;
#151158 = CARTESIAN_POINT ( 'NONE',  ( 4.488337453930180132, -0.4787454259813396229, -2.138356021698713416 ) ) ;
#151159 = CARTESIAN_POINT ( 'NONE',  ( 1.160779977835691312, 1.203355533934968635, 1.617816888933524710 ) ) ;
#151160 = CARTESIAN_POINT ( 'NONE',  ( 1.030510548812729965, -1.664561007783531332, 0.7873658874757857307 ) ) ;
#151161 = CARTESIAN_POINT ( 'NONE',  ( 5.390252792638895230, -0.5542908586613685129, -2.224220739628431254 ) ) ;
#151162 = CARTESIAN_POINT ( 'NONE',  ( 3.292734131499192252, 1.452021927685825275, 1.131891246899892289 ) ) ;
#151163 = CARTESIAN_POINT ( 'NONE',  ( 9.772729797352075920, 10.29593960653257234, -0.7998128361456281477 ) ) ;
#151164 = CARTESIAN_POINT ( 'NONE',  ( 3.698116152863577977, -1.823479002399010396, -0.09026698595545472326 ) ) ;
#151165 = CARTESIAN_POINT ( 'NONE',  ( 5.344375030997434273, 0.3906003880304632636, -1.978050218768567792 ) ) ;
#151166 = CARTESIAN_POINT ( 'NONE',  ( -9.528683032306089373, 10.01121838064558744, 0.7998128361456462443 ) ) ;
#151168 = CARTESIAN_POINT ( 'NONE',  ( -6.607619761813764647, 8.802252036906432764, 1.599625672291269396 ) ) ;
#151167 = CARTESIAN_POINT ( 'NONE',  ( 4.874029165478985348, 1.298689969358796770, 1.852503425883561095 ) ) ;
#151169 = CARTESIAN_POINT ( 'NONE',  ( 6.317421145955757211, -0.2613792861649695265, 2.089613723330654427 ) ) ;
#151170 = SURFACE_SIDE_STYLE ('',( #34198 ) ) ;
#151171 = CARTESIAN_POINT ( 'NONE',  ( 3.174344110969638866, -1.018096006688212096, -1.802650257252853772 ) ) ;
#151172 = CARTESIAN_POINT ( 'NONE',  ( 10.55232363013785246, 11.20546574478267132, 0.000000000000000000 ) ) ;
#151173 = CARTESIAN_POINT ( 'NONE',  ( 1.360316468749978469, 2.296875000341369599, -4.857225732735059864E-14 ) ) ;
#151174 = PRODUCT_CONTEXT ( 'NONE', #144661, 'mechanical' ) ;
#151177 = ADVANCED_FACE ( 'NONE', ( #20931 ), #87027, .F. ) ;
#151176 = CARTESIAN_POINT ( 'NONE',  ( 1.998540859798603408, -0.5134167636005394497, -1.856760371892735906 ) ) ;
#151175 = CARTESIAN_POINT ( 'NONE',  ( -8.799405390469187793, 10.22472669609091689, -1.199719254218446718 ) ) ;
#151178 = CARTESIAN_POINT ( 'NONE',  ( 4.858666941289190078, 5.005999693891180158, -0.7510321973731617362 ) ) ;
#151179 = CARTESIAN_POINT ( 'NONE',  ( 6.807475516257630588, -1.579661688080177262, -1.175915379947721773 ) ) ;
#151180 = CARTESIAN_POINT ( 'NONE',  ( 4.462041952228939401, 6.299077925724123617, -1.443375672974068769 ) ) ;
#151181 = CARTESIAN_POINT ( 'NONE',  ( 5.712091369430416066, 6.087825614771766425, 0.6924918054137980672 ) ) ;
#151182 = CARTESIAN_POINT ( 'NONE',  ( -4.274898507010545856, 3.881803101134051470, -0.7998128361456221525 ) ) ;
#151183 = CARTESIAN_POINT ( 'NONE',  ( 1.283751863706618535, 0.1568931172264090290, -2.215910488618375584 ) ) ;
#151184 = CARTESIAN_POINT ( 'NONE',  ( 3.188603428895543601, -2.074531711476882201, -0.3615289903074799249 ) ) ;
#151185 = CARTESIAN_POINT ( 'NONE',  ( -6.424584688029276514, 8.588711117491191871, 1.599625672291269396 ) ) ;
#151186 = CARTESIAN_POINT ( 'NONE',  ( 7.935599982700328958, 8.152621489438862667, 0.7998128361456481317 ) ) ;
#151187 = CARTESIAN_POINT ( 'NONE',  ( 6.977413160773116019, -0.1420559494431029579, 1.829748798152310174 ) ) ;
#151188 = CARTESIAN_POINT ( 'NONE',  ( 6.986529229743720926, 7.045372277656132276, -0.7998128361456281477 ) ) ;
#151189 = CARTESIAN_POINT ( 'NONE',  ( 4.955668840994886359, 5.740367388370866131, 1.199719254218462483 ) ) ;
#151190 = CARTESIAN_POINT ( 'NONE',  ( -5.804299160426242388, 6.904675454319632699, -1.082531754730549967 ) ) ;
#151192 = CARTESIAN_POINT ( 'NONE',  ( -8.527715433315703919, 9.051348881730875817, 1.040834085586084257E-14 ) ) ;
#151191 = AXIS2_PLACEMENT_3D ( 'NONE', #147479, #97669, #14233 ) ;
#151193 = CARTESIAN_POINT ( 'NONE',  ( 1.230900525853476868, 1.420129835883350955, -1.575055732827963295 ) ) ;
#151194 = CARTESIAN_POINT ( 'NONE',  ( -4.749098946536820520, 8.762642214260091933, 0.7998128361456281477 ) ) ;
#151196 = CARTESIAN_POINT ( 'NONE',  ( 4.844172697165038066, -0.9265620464425131653, 1.729294158640543699 ) ) ;
#151195 = CARTESIAN_POINT ( 'NONE',  ( 1.224999999999965006, 0.3541666666667217522, 0.7072540797572456350 ) ) ;
#151197 = CARTESIAN_POINT ( 'NONE',  ( 3.731458613173586514, -1.998165266068991253, 0.8252760040215676440 ) ) ;
#151198 = CARTESIAN_POINT ( 'NONE',  ( 1.856743374925871715, 0.3135980649527739250, -1.814175028193690808 ) ) ;
#151199 = CARTESIAN_POINT ( 'NONE',  ( -4.022721148277657477, 7.614442113290216696, -0.1953124528039917873 ) ) ;
#151200 = CARTESIAN_POINT ( 'NONE',  ( 4.264789376140788235, 7.497597942732838305, -1.024658161349981444 ) ) ;
#151201 = CARTESIAN_POINT ( 'NONE',  ( 4.892389968643020559, 1.444305832375993637, -0.9706037289107912747 ) ) ;
#151202 = FACE_OUTER_BOUND ( 'NONE', #175655, .T. ) ;
#151203 = CARTESIAN_POINT ( 'NONE',  ( 6.168596704537822717, 6.299043698156668647, 1.040834085586084257E-14 ) ) ;
#151204 = CARTESIAN_POINT ( 'NONE',  ( -11.69380381030441107, 8.410673437356566140, -1.083569014401829955 ) ) ;
#151205 = CARTESIAN_POINT ( 'NONE',  ( 7.750457368506414646, 12.19395069656619945, 0.7998128361456462443 ) ) ;
#151206 = CARTESIAN_POINT ( 'NONE',  ( 1.604591590977550108, -0.7782141685120853580, -2.016947388195994062 ) ) ;
#151207 = CARTESIAN_POINT ( 'NONE',  ( 3.514999820297697308, 2.016288306963448296, 0.002811503506894295987 ) ) ;
#151208 = CARTESIAN_POINT ( 'NONE',  ( -8.771762197917311710, 13.17754696430482042, 0.7216878364870317197 ) ) ;
#151209 = CARTESIAN_POINT ( 'NONE',  ( 1.587033755777764510, -0.3173376132806354222, -2.138153673666403964 ) ) ;
#151210 = EDGE_CURVE ( 'NONE', #66793, #180510, #10040, .T. ) ;
#151211 = CARTESIAN_POINT ( 'NONE',  ( 3.608241331778249350, -0.7978255515562487910, -1.802987302761626998 ) ) ;
#151212 = CARTESIAN_POINT ( 'NONE',  ( 6.609000000000019526, 4.695354556932705314, 2.562644781943986150 ) ) ;
#151213 = CARTESIAN_POINT ( 'NONE',  ( 3.157691648149099972, 0.8757969000599256093, 1.733462199761313993 ) ) ;
#151216 = ORIENTED_EDGE ( 'NONE', *, *, #85559, .T. ) ;
#151215 = CARTESIAN_POINT ( 'NONE',  ( -3.201133666602369310, 6.748756687762456963, -0.7216878364870458196 ) ) ;
#151214 = CYLINDRICAL_SURFACE ( 'NONE', #146404, 1.250000000000000000 ) ;
#151217 = CIRCLE ( 'NONE', #109839, 10.99999999999999112 ) ;
#151218 = CARTESIAN_POINT ( 'NONE',  ( -5.777182852754558340, 5.912670547734647286, 0.000000000000000000 ) ) ;
#151219 = CARTESIAN_POINT ( 'NONE',  ( -0.1106856583841242386, 7.629137130509040965, -2.596956429031356262 ) ) ;
#151220 = CARTESIAN_POINT ( 'NONE',  ( 5.194709132691408549, 6.089524072008651423, 1.199719254218452935 ) ) ;
#151221 = CARTESIAN_POINT ( 'NONE',  ( -5.679940009482361774, 5.591294530676332641, 0.7998128361456281477 ) ) ;
#151222 = CARTESIAN_POINT ( 'NONE',  ( -4.281342646865346602, 8.216926531310035031, 0.7998128361456352531 ) ) ;
#151223 = CARTESIAN_POINT ( 'NONE',  ( -9.286972035236630063, 10.89751746493999107, -1.082531754730537976 ) ) ;
#151224 = CARTESIAN_POINT ( 'NONE',  ( 6.809642309899604840, -0.5188996100353564511, 2.257106211077652969 ) ) ;
#151225 = CARTESIAN_POINT ( 'NONE',  ( -3.285556943750000070, -3.259374999522044014, 0.000000000000000000 ) ) ;
#151226 = CARTESIAN_POINT ( 'NONE',  ( 4.504711789546460565, 0.5192035298374733099, 1.891763301562799260 ) ) ;
#151227 = CARTESIAN_POINT ( 'NONE',  ( 1.248672897702383988, 1.986100274556975354, -0.3474695496914689818 ) ) ;
#151228 = VERTEX_POINT ( 'NONE', #105444 ) ;
#151229 = CARTESIAN_POINT ( 'NONE',  ( 3.538375268227810011, 0.7659831068804138221, 1.974087397274668643 ) ) ;
#151230 = CARTESIAN_POINT ( 'NONE',  ( 1.499999999999987121, 3.577083334016152527, -0.8660254037844262731 ) ) ;
#151232 = CARTESIAN_POINT ( 'NONE',  ( -6.742482464697739708, 6.760651051769146491, 0.7998128361456341429 ) ) ;
#151231 = CARTESIAN_POINT ( 'NONE',  ( 9.581975256308805200, -7.217880409008743392, 3.332261557277432708E-13 ) ) ;
#151233 = CARTESIAN_POINT ( 'NONE',  ( 2.642321604431462578, -1.530645349967133972, 1.022873098850234141 ) ) ;
#151234 = ORIENTED_EDGE ( 'NONE', *, *, #200488, .F. ) ;
#151235 = CARTESIAN_POINT ( 'NONE',  ( -9.321394304595349567, 10.83371376257142416, 1.199719254218462483 ) ) ;
#151236 = CARTESIAN_POINT ( 'NONE',  ( 0.006768871532346317291, 8.210909518262139883, 2.038649385027042626 ) ) ;
#151237 = CARTESIAN_POINT ( 'NONE',  ( 5.238584497427841491, 1.261362679698872169, -1.704546977916908457 ) ) ;
#151238 = CARTESIAN_POINT ( 'NONE',  ( 0.7499999999999902300, 4.347916667349481123, -1.299038105676658228 ) ) ;
#151239 = CARTESIAN_POINT ( 'NONE',  ( 5.774883364416965037, 8.824782127540085952, -1.199719254218440723 ) ) ;
#151240 = CARTESIAN_POINT ( 'NONE',  ( 5.923136198411797615, -0.05496255519776967885, 2.060232511946280098 ) ) ;
#151242 = CARTESIAN_POINT ( 'NONE',  ( 2.331387312403776946, 0.8663521307504215008, -1.624669977836174839 ) ) ;
#151241 = CARTESIAN_POINT ( 'NONE',  ( 0.3614606035443160836, -0.5022670859271642918, 1.791915111541013461 ) ) ;
#151243 = CARTESIAN_POINT ( 'NONE',  ( 10.08456733046637765, 10.65975006183261087, 0.000000000000000000 ) ) ;
#151244 =( NAMED_UNIT ( * ) PLANE_ANGLE_UNIT ( ) SI_UNIT ( $, .RADIAN. ) );
#151245 = CARTESIAN_POINT ( 'NONE',  ( -11.86145016429273724, 10.09412591486744404, 1.099999999999996980 ) ) ;
#151246 = CARTESIAN_POINT ( 'NONE',  ( 3.701012746850603996, 7.261672604726938651, 1.040834085586084257E-14 ) ) ;
#151247 = EDGE_CURVE ( 'NONE', #111149, #21772, #175637, .T. ) ;
#151248 = CARTESIAN_POINT ( 'NONE',  ( 2.034064749695370100, -1.442962035976073309, -1.669870808145665020 ) ) ;
#151249 = CARTESIAN_POINT ( 'NONE',  ( 4.938899882951366394, 0.3800905753248150498, 2.230106783295758177 ) ) ;
#151250 = CARTESIAN_POINT ( 'NONE',  ( -7.429504990608782222, 8.730472579540773381, 1.082531754730549967 ) ) ;
#151251 = CARTESIAN_POINT ( 'NONE',  ( 4.834136970758627250, -0.9753174380719393799, -1.526440946957215994 ) ) ;
#151252 = CARTESIAN_POINT ( 'NONE',  ( 4.469893758321111576, -0.8975064867107468425, 1.692437687186749917 ) ) ;
#151253 = CARTESIAN_POINT ( 'NONE',  ( -0.6823417656249969321, 5.030208333674755394, -1.181850606188749264 ) ) ;
#151254 = CARTESIAN_POINT ( 'NONE',  ( 4.082859939823464401, -0.1922352567787863620, -1.962060651276048118 ) ) ;
#151255 = CARTESIAN_POINT ( 'NONE',  ( 4.803500792215161574, -0.4985019455652460740, 1.802925825644098534 ) ) ;
#151256 = CARTESIAN_POINT ( 'NONE',  ( 5.301151097710674165, -1.596257866726397134, 0.9565186216247966167 ) ) ;
#151257 = CARTESIAN_POINT ( 'NONE',  ( -6.735605996566196296E-15, -9.900000000000005684, 9.579665964948942403 ) ) ;
#151258 = CARTESIAN_POINT ( 'NONE',  ( 0.1457207355009884908, 1.993892511249679034, -0.3006540981884687214 ) ) ;
#151260 = CARTESIAN_POINT ( 'NONE',  ( 2.297617436792959378, 1.628516202021938808, 1.335460665606647446 ) ) ;
#151259 = CARTESIAN_POINT ( 'NONE',  ( -2.941756144040970522, 5.415504020480993219, -1.082531754730543083 ) ) ;
#151261 = CARTESIAN_POINT ( 'NONE',  ( 9.049177462117294013, 12.64479190819049670, -1.199719254218446718 ) ) ;
#151263 = CARTESIAN_POINT ( 'NONE',  ( 0.07479286986305369589, 1.387406912293275729, -2.112587013352088317 ) ) ;
#151262 = CARTESIAN_POINT ( 'NONE',  ( 0.6823417656249917140, 4.905208333674755394, 1.181850606188765695 ) ) ;
#151264 = CARTESIAN_POINT ( 'NONE',  ( 2.900754761704402274, -2.089926006748676457, -0.3584049868644647585 ) ) ;
#151265 = CARTESIAN_POINT ( 'NONE',  ( 5.526144005543697446, 7.442112546579989996, -1.248357989223557452 ) ) ;
#151266 = CARTESIAN_POINT ( 'NONE',  ( 1.652609354460622626, 1.998416004623180697, 0.2920258124684270706 ) ) ;
#151267 = CARTESIAN_POINT ( 'NONE',  ( -0.6823417656250003738, 2.467708333674753618, -1.181850606188749264 ) ) ;
#151268 = CARTESIAN_POINT ( 'NONE',  ( -4.284013352238274841, 4.100363120473813794, -0.7216878364870207285 ) ) ;
#151269 = CARTESIAN_POINT ( 'NONE',  ( 3.551346171775753735, 6.230655402791975384, 1.199719254218462483 ) ) ;
#151270 = CARTESIAN_POINT ( 'NONE',  ( 1.599129061979026822, 1.768144091905754500, -1.243190488262067683 ) ) ;
#151271 = CARTESIAN_POINT ( 'NONE',  ( 6.890000000000001457, 2.439643239904603966, 2.382311923195524095 ) ) ;
#151274 = CARTESIAN_POINT ( 'NONE',  ( -0.5773502691896261751, -2.500000000000002220, -0.9999999999999991118 ) ) ;
#151273 = CARTESIAN_POINT ( 'NONE',  ( -2.788906526875773208E-15, 13.21875000068279427, -1.499999999999998446 ) ) ;
#151272 = CARTESIAN_POINT ( 'NONE',  ( 5.194709132691408549, 6.089524072008651423, 1.199719254218452935 ) ) ;
#151275 =( BOUNDED_SURFACE ( )  B_SPLINE_SURFACE ( 3, 2, ( 
 ( #73661, #58483, #104043 ),
 ( #102970, #202569, #54220 ),
 ( #8655, #106218, #91004 ),
 ( #172244, #71507, #89937 ) ),
 .UNSPECIFIED., .F., .F., .T. ) 
 B_SPLINE_SURFACE_WITH_KNOTS ( ( 4, 4 ),
 ( 3, 3 ),
 ( 3.059570999470615060, 3.223614307708551951 ),
 ( 0.000000000000000000, 1.000000000000000000 ),
 .UNSPECIFIED. ) 
 GEOMETRIC_REPRESENTATION_ITEM ( )  RATIONAL_B_SPLINE_SURFACE ( (
 ( 1.000000000000000000, 0.6179932349765480115, 1.000000000000000000),
 ( 1.000000000000000000, 0.6282795510880925249, 1.000000000000000000),
 ( 1.000000000000000000, 0.6282795510881205026, 1.000000000000000000),
 ( 1.000000000000000000, 0.6179932349766239508, 1.000000000000000000) ) ) 
 REPRESENTATION_ITEM ( '' )  SURFACE ( )  );
#151276 = CARTESIAN_POINT ( 'NONE',  ( 11.94655611907589154, 9.947990554530955265, 1.134828163062136852 ) ) ;
#151277 = CARTESIAN_POINT ( 'NONE',  ( -7.966449380362737642, -6.654700410849496706, 7.586197045692401275 ) ) ;
#151278 = CARTESIAN_POINT ( 'NONE',  ( -6.995644074971465010, 10.14503993989993091, 1.082531754730549967 ) ) ;
#151279 = COLOUR_RGB ( '', 0.72549020, 0.75294118, 0.79215686) ;
#151280 = CARTESIAN_POINT ( 'NONE',  ( 1.013517375116283592, -2.137022957946862700, 0.4851717564131745597 ) ) ;
#151281 = DIRECTION ( 'NONE',  ( -8.638326563840814399E-31, 0.000000000000000000, -1.000000000000000000 ) ) ;
#151283 = CARTESIAN_POINT ( 'NONE',  ( -1.364683531250010740, 11.63020833367472839, 0.7879004041258445001 ) ) ;
#151282 = CARTESIAN_POINT ( 'NONE',  ( 1.095004809772756493, -0.5519004177921453813, -2.194067758203117169 ) ) ;
#151284 = CARTESIAN_POINT ( 'NONE',  ( -9.657485491635913633, 10.16148791653038330, 1.040834085586084257E-14 ) ) ;
#151285 = CARTESIAN_POINT ( 'NONE',  ( -4.161989969270909917, 5.878740935614591656, 1.443375672974064550 ) ) ;
#151286 = CARTESIAN_POINT ( 'NONE',  ( -1.402160292154681736E-14, 2.009375000341422801, -1.575800808251660134 ) ) ;
#151287 = CARTESIAN_POINT ( 'NONE',  ( 4.612778539632031105, 8.351152097327862123, 0.2683542610703564812 ) ) ;
#151288 = CARTESIAN_POINT ( 'NONE',  ( -0.7500000000000179856, 9.541666666666671404, 1.299038105676658228 ) ) ;
#151289 = CARTESIAN_POINT ( 'NONE',  ( 4.318794280271901265, 1.578467719028648686, 0.6958846415187101009 ) ) ;
#151290 = CARTESIAN_POINT ( 'NONE',  ( 4.390861645979372341, 6.216034235099629157, -1.599625672291269396 ) ) ;
#151291 = CARTESIAN_POINT ( 'NONE',  ( 2.319294515261476342, -1.717818424975267932, 0.4250260156472511208 ) ) ;
#151292 = CARTESIAN_POINT ( 'NONE',  ( 3.000642180831034622, -1.983674057915509881, -0.3420062109290455954 ) ) ;
#151293 = CARTESIAN_POINT ( 'NONE',  ( 4.893709131440695081, 1.632385321431808256, 1.485157849447714451 ) ) ;
#151294 = ORIENTED_EDGE ( 'NONE', *, *, #140838, .T. ) ;
#151295 = CARTESIAN_POINT ( 'NONE',  ( 4.728773938389556619, 1.389870793851749164, -1.465793203850384030 ) ) ;
#151296 = CARTESIAN_POINT ( 'NONE',  ( -5.285699784481336927, 7.260012063351913625, 1.599625672291263179 ) ) ;
#151297 = CARTESIAN_POINT ( 'NONE',  ( 5.360953910674266965, -0.05231296482399727665, -2.015913715532565043 ) ) ;
#151299 = ORIENTED_EDGE ( 'NONE', *, *, #96162, .F. ) ;
#151298 = CARTESIAN_POINT ( 'NONE',  ( 4.535318187750695174, -0.08185482751379420663, 1.809849901470663491 ) ) ;
#151300 = EDGE_CURVE ( 'NONE', #198793, #193425, #38744, .T. ) ;
#151301 = CARTESIAN_POINT ( 'NONE',  ( 3.080767038946086611, -0.1360980058115155988, -1.865751385159146070 ) ) ;
#151302 = DIRECTION ( 'NONE',  ( 0.7592566023653005702, 0.6507913734559639396, 0.000000000000000000 ) ) ;
#151303 = CARTESIAN_POINT ( 'NONE',  ( 2.144650067465687648, 1.855875215511919363, 0.4610605321611755958 ) ) ;
#151304 = CARTESIAN_POINT ( 'NONE',  ( 1.500000000000003997, 5.900000000000022560, 1.214306433183764966E-14 ) ) ;
#151305 = VECTOR ( 'NONE', #40743, 1000.000000000000000 ) ;
#151306 = CARTESIAN_POINT ( 'NONE',  ( -10.36744940472232379, 5.031894517187950555, -7.294791872146300982 ) ) ;
#151307 =( LENGTH_UNIT ( ) NAMED_UNIT ( * ) SI_UNIT ( .MILLI., .METRE. ) );
#151308 = B_SPLINE_CURVE_WITH_KNOTS ( 'NONE', 3,
 ( #72737, #58634, #5573, #87932, #26120, #189691, #171308, #22902, #154006, #6660, #25055 ),
 .UNSPECIFIED., .F., .F.,
 ( 4, 1, 1, 1, 1, 1, 1, 1, 4 ),
 ( 0.000000000000000000, 0.2256337125576066971, 0.3978389261578171299, 0.5257960283851228489, 0.6187025735204009225, 0.6856790771877526725, 0.7354782194756434022, 0.7762620033627533056, 0.9999999999999998890 ),
 .UNSPECIFIED. ) ;
#151309 = CARTESIAN_POINT ( 'NONE',  ( 0.6823417656249917140, 3.405208333674754506, 1.181850606188765695 ) ) ;
#151310 = CARTESIAN_POINT ( 'NONE',  ( -0.1229892814952095459, -1.709044814581164973, -0.8582256167319822771 ) ) ;
#151311 = CARTESIAN_POINT ( 'NONE',  ( 6.536439455564164724, 7.758839131980592718, 1.082531754730549967 ) ) ;
#151312 = CARTESIAN_POINT ( 'NONE',  ( 1.258172656280614365, -1.962046632281065461, -0.003472340283867945618 ) ) ;
#151313 = DIRECTION ( 'NONE',  ( -8.638326563840814399E-31, 0.000000000000000000, -1.000000000000000000 ) ) ;
#151314 = CARTESIAN_POINT ( 'NONE',  ( -5.285699784481336927, 7.260012063351913625, 1.599625672291263179 ) ) ;
#151315 = CARTESIAN_POINT ( 'NONE',  ( 5.590118541908202232, 1.264772504208915072, 1.701965355810124203 ) ) ;
#151317 = CARTESIAN_POINT ( 'NONE',  ( 10.96028113393447256, -5.411711732698798905, -0.1309013025973228828 ) ) ;
#151316 = CARTESIAN_POINT ( 'NONE',  ( 8.615316546479974136, 12.13862083994696839, 1.199719254218450271 ) ) ;
#151318 = CARTESIAN_POINT ( 'NONE',  ( 5.132083838642755858, 1.015972595308231474, -1.689280876731833470 ) ) ;
#151319 = CARTESIAN_POINT ( 'NONE',  ( 1.364683531249986537, 2.405208333674752286, -0.7879004041258239610 ) ) ;
#151320 = CARTESIAN_POINT ( 'NONE',  ( 0.7033859027741823366, 1.773467923640878796, -0.9528479892364212223 ) ) ;
#151321 = ORIENTED_EDGE ( 'NONE', *, *, #115558, .F. ) ;
#151322 = CARTESIAN_POINT ( 'NONE',  ( 1.423615893443540337, -1.536295912932123642, -1.457111741773434943 ) ) ;
#151323 = CARTESIAN_POINT ( 'NONE',  ( 11.08792111388080492, 7.949474773914394277, -4.609825048350510102 ) ) ;
#151324 = CARTESIAN_POINT ( 'NONE',  ( 2.629418614236479712, 0.1040367438073786233, -2.067886086930009970 ) ) ;
#151325 = CARTESIAN_POINT ( 'NONE',  ( 5.174371902270911150, 6.065797303184739420, 1.199719254218452047 ) ) ;
#151326 = CARTESIAN_POINT ( 'NONE',  ( 6.561219994370630637, 6.619454513046008515, 0.000000000000000000 ) ) ;
#151327 = VERTEX_POINT ( 'NONE', #59864 ) ;
#151329 = CARTESIAN_POINT ( 'NONE',  ( 3.506755287428983792, 7.242964935309132990, 1.040834085586084257E-14 ) ) ;
#151328 = CARTESIAN_POINT ( 'NONE',  ( 4.734370563723459213, 0.3569306294452011530, 2.059774728693287038 ) ) ;
#151332 = ORIENTED_EDGE ( 'NONE', *, *, #164982, .F. ) ;
#151331 = CARTESIAN_POINT ( 'NONE',  ( 2.701584635150193314, 1.282363399140455273, 1.279706459777726346 ) ) ;
#151330 = CARTESIAN_POINT ( 'NONE',  ( 3.170728842436408179, -1.686227525993441834, -0.7000332573987508855 ) ) ;
#151333 = CARTESIAN_POINT ( 'NONE',  ( -3.469446951953614189E-15, -1.000000000000000888, 2.602085213965210642E-15 ) ) ;
#151334 = CARTESIAN_POINT ( 'NONE',  ( -11.33772463945037146, 13.39999999999998259, 3.599999999999999201 ) ) ;
#151335 = CARTESIAN_POINT ( 'NONE',  ( 9.805160342514797733, 10.58486009514582449, -5.518090938306281501 ) ) ;
#151336 = CARTESIAN_POINT ( 'NONE',  ( 4.805825877545530922, -0.5924843665619135002, 2.125676689404366826 ) ) ;
#151337 = CARTESIAN_POINT ( 'NONE',  ( -1.364683531250014514, 8.901041667008069425, -0.7879004041258335089 ) ) ;
#151338 = CARTESIAN_POINT ( 'NONE',  ( 3.598220562318912741, -0.9401235635465958751, 1.665135908046413871 ) ) ;
#151340 = CARTESIAN_POINT ( 'NONE',  ( -2.435661151949389147, 5.993355110582911038, 0.7998128361456341429 ) ) ;
#151339 = AXIS2_PLACEMENT_3D ( 'NONE', #45516, #110566, #108436 ) ;
#151341 = CARTESIAN_POINT ( 'NONE',  ( 8.606728586576791074, 8.935604860628076906, 0.7998128361456462443 ) ) ;
#151342 = CARTESIAN_POINT ( 'NONE',  ( 6.496543107701719499, 2.047251205643263017, 0.3077783505985449142 ) ) ;
#151343 = CARTESIAN_POINT ( 'NONE',  ( 3.834746474454188013E-15, 10.34375000068279782, 1.500000000000001554 ) ) ;
#151344 = CARTESIAN_POINT ( 'NONE',  ( 5.951666246274807115, 6.045958163516475636, 0.7216878364870317197 ) ) ;
#151345 = EDGE_CURVE ( 'NONE', #200465, #33823, #123764, .T. ) ;
#151346 = DIRECTION ( 'NONE',  ( 1.000000000000000000, -0.000000000000000000, 1.779758311459929752E-16 ) ) ;
#151347 = CARTESIAN_POINT ( 'NONE',  ( 8.455729991919987754, 13.99694205269637948, -8.515310571025079156 ) ) ;
#151348 = CARTESIAN_POINT ( 'NONE',  ( -9.612297698795947198, -6.674536912880607353, 0.2039282260588225759 ) ) ;
#151349 = DIRECTION ( 'NONE',  ( -1.535693738322999099E-12, 1.000000000000000000, 1.561558963378103181E-12 ) ) ;
#151350 = CARTESIAN_POINT ( 'NONE',  ( 3.338976900156843453, -1.651226333174139693, 0.8788041501476551165 ) ) ;
#151351 = CARTESIAN_POINT ( 'NONE',  ( 5.806634928402749196, 9.996434193103704402, -0.7998128361456481317 ) ) ;
#151352 = DIRECTION ( 'NONE',  ( 0.000000000000000000, 0.000000000000000000, -1.000000000000000000 ) ) ;
#151353 =( BOUNDED_CURVE ( )  B_SPLINE_CURVE ( 2, ( #42152, #73557, #124537, #190494, #93036, #91973, #10675, #94105, #9619 ),
 .UNSPECIFIED., .F., .T. ) 
 B_SPLINE_CURVE_WITH_KNOTS ( ( 3, 2, 2, 2, 3 ),
 ( 0.4218749999999998335, 0.4270833333333333148, 0.4375000000000000000, 0.4479166666666666852, 0.4531250000000001665 ),
 .UNSPECIFIED. ) 
 CURVE ( )  GEOMETRIC_REPRESENTATION_ITEM ( )  RATIONAL_B_SPLINE_CURVE ( ( 0.9330127018922194093, 0.9330127018922171889, 1.000000000000000000, 0.8660254037844387076, 1.000000000000000000, 0.8660254037844387076, 1.000000000000000000, 0.9330127018922171889, 0.9330127018922194093 ) ) 
 REPRESENTATION_ITEM ( '' )  );
#151354 = CARTESIAN_POINT ( 'NONE',  ( -5.721177635286839092, 9.618531641235897212, 0.7216878364870458196 ) ) ;
#151355 = CARTESIAN_POINT ( 'NONE',  ( 3.410758162289653672, 6.136912401716668519, -1.199719254218453823 ) ) ;
#151356 = CARTESIAN_POINT ( 'NONE',  ( 4.955668840994886359, 5.740367388370866131, 1.199719254218462483 ) ) ;
#151357 = CARTESIAN_POINT ( 'NONE',  ( 6.965700764728601335, -0.4599482372066622249, 2.025938098699997525 ) ) ;
#151358 = ADVANCED_FACE ( 'NONE', ( #23070 ), #43643, .T. ) ;
#151359 = CARTESIAN_POINT ( 'NONE',  ( 1.335564786618839817, 0.5826355126458090394, -1.930425043884366865 ) ) ;
#151360 = CARTESIAN_POINT ( 'NONE',  ( -9.484092147959342967, 11.02352791316275216, 1.199719254218462483 ) ) ;
#151361 = CARTESIAN_POINT ( 'NONE',  ( 5.155843554946782703, 9.237177590738404831, -0.7998128361456481317 ) ) ;
#151362 = CARTESIAN_POINT ( 'NONE',  ( 1.799034956846547795, 1.823213324544867397, 1.215573211712846158 ) ) ;
#151363 = CARTESIAN_POINT ( 'NONE',  ( 6.533835636172961259, -1.196796279342365210, -1.378804128639096849 ) ) ;
#151364 = CARTESIAN_POINT ( 'NONE',  ( -8.597841969360544567, 13.18256606422934674, 0.7998128361456341429 ) ) ;
#151365 = EDGE_CURVE ( 'NONE', #103797, #6371, #50069, .T. ) ;
#151366 = CARTESIAN_POINT ( 'NONE',  ( 5.072158865288233009, 7.010880990960010273, 1.443375672974065660 ) ) ;
#151367 = CARTESIAN_POINT ( 'NONE',  ( 8.723781775389312543, 12.26516360700784958, -1.199719254218446718 ) ) ;
#151368 = CARTESIAN_POINT ( 'NONE',  ( 4.192495815123822744, 5.914331089109666983, -1.599625672291255185 ) ) ;
#151369 = CARTESIAN_POINT ( 'NONE',  ( 6.482206841109512396, 9.616306177052839743, -1.082531754730548412 ) ) ;
#151370 = ORIENTED_EDGE ( 'NONE', *, *, #104548, .F. ) ;
#151372 = CARTESIAN_POINT ( 'NONE',  ( 0.1705643940957324023, 0.7724326726834315204, 1.859191304955130297 ) ) ;
#151371 = CARTESIAN_POINT ( 'NONE',  ( 3.386116603743833497, -0.3623624896987759914, -1.805063595765175499 ) ) ;
#151373 = CARTESIAN_POINT ( 'NONE',  ( 2.495865491978021211, 2.229134443137513966, 0.5594839687708874632 ) ) ;
#151375 = CARTESIAN_POINT ( 'NONE',  ( 0.4966286816309881114, 0.3102001241638470685, 1.834739031104109408 ) ) ;
#151374 = CARTESIAN_POINT ( 'NONE',  ( 3.009546912553647147, 5.494593250412460606, -1.082531754730543083 ) ) ;
#151376 = CARTESIAN_POINT ( 'NONE',  ( 0.000000000000000000, -3.346874999522042149, -3.793834371823813001 ) ) ;
#151377 = CARTESIAN_POINT ( 'NONE',  ( -5.525111292768871252, 6.404716915440499037, -1.199719254218446718 ) ) ;
#151378 = DIRECTION ( 'NONE',  ( 5.578564026256490882E-16, 1.000000000000000000, 9.066213480720158442E-32 ) ) ;
#151379 = CARTESIAN_POINT ( 'NONE',  ( 5.027564050633359649, -0.2746679736120913318, 1.892429487827557599 ) ) ;
#151380 = CARTESIAN_POINT ( 'NONE',  ( -8.286004436246233951, 12.81875560892930466, 1.040834085586084257E-14 ) ) ;
#151381 = CARTESIAN_POINT ( 'NONE',  ( 5.954584599377941601, 7.113081392617206511, -1.094866876611422235 ) ) ;
#151382 = CARTESIAN_POINT ( 'NONE',  ( -6.373741612200205076, 8.529394195690610303, 1.443375672974064550 ) ) ;
#151384 = CARTESIAN_POINT ( 'NONE',  ( 2.483090063216564669, 1.711211315118581711, -0.7561169667836544761 ) ) ;
#151383 = CARTESIAN_POINT ( 'NONE',  ( 4.142189164857057015, 0.5595570048471016911, 2.014385595549014418 ) ) ;
#151385 = CARTESIAN_POINT ( 'NONE',  ( 9.110716038703335684, 9.731516254683127087, -0.7216878364870197293 ) ) ;
#151386 = CARTESIAN_POINT ( 'NONE',  ( -1.364683531250010740, 5.592708333674751842, 0.7879004041258379498 ) ) ;
#151387 = CARTESIAN_POINT ( 'NONE',  ( 3.227794649281841011, 1.698692639566254936, 0.3781252810216747529 ) ) ;
#151388 = CARTESIAN_POINT ( 'NONE',  ( 4.090809663021327758, 5.795697244990093644, 1.599625672291267398 ) ) ;
#151390 = CARTESIAN_POINT ( 'NONE',  ( 5.301401758143367893, 6.143722458377430584, 1.199719254218462483 ) ) ;
#151389 = CARTESIAN_POINT ( 'NONE',  ( -0.4019237886466802689, 11.47991455036742714, -1.500000000000002887 ) ) ;
#151391 = CARTESIAN_POINT ( 'NONE',  ( 3.949580097687496405, 0.5788178622721011912, -1.624998464860913705 ) ) ;
#151392 = CARTESIAN_POINT ( 'NONE',  ( -6.042130013184518589, 10.20090211535728031, -0.7998128361456291469 ) ) ;
#151393 = CARTESIAN_POINT ( 'NONE',  ( 3.737968522918270864, 2.181131050170285857, 0.2133239450496857148 ) ) ;
#151394 = CARTESIAN_POINT ( 'NONE',  ( 6.147136880733683917, -1.866598994669689926, 1.177069016086537356 ) ) ;
#151395 = DIRECTION ( 'NONE',  ( 0.000000000000000000, -1.000000000000000000, 0.000000000000000000 ) ) ;
#151396 = CARTESIAN_POINT ( 'NONE',  ( 3.450208493196211812, -0.8844140035146315082, 1.982955601465713258 ) ) ;
#151397 = CARTESIAN_POINT ( 'NONE',  ( 1.963248404482214049, 0.3131683437365209710, -1.798463397695612809 ) ) ;
#151398 = DIRECTION ( 'NONE',  ( 0.000000000000000000, 8.546850786086437571E-32, 1.000000000000000000 ) ) ;
#151399 = CARTESIAN_POINT ( 'NONE',  ( 6.139883455347572294, 2.111525295599859575, -0.1581134299761654260 ) ) ;
#151400 = ORIENTED_EDGE ( 'NONE', *, *, #42056, .T. ) ;
#151402 = CARTESIAN_POINT ( 'NONE',  ( 0.6823417656249899377, 2.905208333674754062, 1.181850606188765695 ) ) ;
#151401 = CARTESIAN_POINT ( 'NONE',  ( 5.460555387939631800, -2.071112900911156185, -0.9828140750258400615 ) ) ;
#151403 = CARTESIAN_POINT ( 'NONE',  ( 10.24048609702354717, 10.84165528948263457, -0.7998128361456281477 ) ) ;
#151404 = CARTESIAN_POINT ( 'NONE',  ( 0.9969211937387794098, -2.069638562867767373, -0.4609060192823294932 ) ) ;
#151405 = CARTESIAN_POINT ( 'NONE',  ( -3.606105671554953318, 7.150947683548662503, 0.7216878364870317197 ) ) ;
#151406 = CARTESIAN_POINT ( 'NONE',  ( 3.307826292054301121, 4.882216645528547616, -1.443375672974057666 ) ) ;
#151407 = CARTESIAN_POINT ( 'NONE',  ( -5.138177029454855216, 7.017625839162543677, 1.443375672974064550 ) ) ;
#151409 = CARTESIAN_POINT ( 'NONE',  ( -0.7500000000000179856, 12.07291666734946389, 1.299038105676658228 ) ) ;
#151408 = CARTESIAN_POINT ( 'NONE',  ( -10.99861980075107937, -9.900000000000074962, 0.1919816227428194633 ) ) ;
#151411 = ORIENTED_EDGE ( 'NONE', *, *, #200741, .F. ) ;
#151410 = CARTESIAN_POINT ( 'NONE',  ( 1.120143885658178906, -0.5347273011463581360, 2.155877112962206965 ) ) ;
#151412 = CARTESIAN_POINT ( 'NONE',  ( 6.557263107265463020, -1.238491779027944162, 1.591905563659588907 ) ) ;
#151414 = CARTESIAN_POINT ( 'NONE',  ( 4.979373296276208727, -0.1066085398311214100, 2.059958923327874114 ) ) ;
#151413 = CARTESIAN_POINT ( 'NONE',  ( 4.660252114795294887, 6.460046772059735432, -1.599625672291256295 ) ) ;
#151416 = CARTESIAN_POINT ( 'NONE',  ( 1.001543065824772753E-15, -3.762499999999999289, 4.012584370867899430 ) ) ;
#151415 = CARTESIAN_POINT ( 'NONE',  ( 6.017840079619279692, 8.114175741012878973, -1.599625672291281386 ) ) ;
#151417 = CARTESIAN_POINT ( 'NONE',  ( 5.189738938980948291, 9.276722205444929870, 0.000000000000000000 ) ) ;
#151418 = CARTESIAN_POINT ( 'NONE',  ( -1.642778471874998480, -1.101041666188708801, 2.845375778867863303 ) ) ;
#151419 = DIRECTION ( 'NONE',  ( 1.276756478318932585E-15, -1.000000000000000000, 1.665334536937738262E-16 ) ) ;
#151420 = CARTESIAN_POINT ( 'NONE',  ( 0.3399330434069799400, 2.085199349320911555, 0.1515528320938461238 ) ) ;
#151421 = CARTESIAN_POINT ( 'NONE',  ( 4.676407821165474488, 1.496050514612049742, 1.352155788975975437 ) ) ;
#151422 = CARTESIAN_POINT ( 'NONE',  ( 4.018977146631536712, -1.760761141180338774, 0.5383908109771737838 ) ) ;
#151423 = CARTESIAN_POINT ( 'NONE',  ( 5.361359679200154105, 8.342337828120466980, 1.199719254218462483 ) ) ;
#151424 = CARTESIAN_POINT ( 'NONE',  ( 0.6567381767516925484, -1.453278249834984326, -0.9285724537800400524 ) ) ;
#151425 = CARTESIAN_POINT ( 'NONE',  ( 0.4445464637146990250, -1.457232572767804379, 1.394089106691732693 ) ) ;
#151426 = CARTESIAN_POINT ( 'NONE',  ( 1.214008909562364069, 2.217199183031343779, 0.6065299581617057401 ) ) ;
#151427 = CARTESIAN_POINT ( 'NONE',  ( -6.898401231254901234, 6.942556279419168419, -0.7998128361456291469 ) ) ;
#151428 = CARTESIAN_POINT ( 'NONE',  ( 1.071959817704574602, 2.180298862187507680, -0.6038346756046736319 ) ) ;
#151429 = CARTESIAN_POINT ( 'NONE',  ( 3.317110013156245873, 1.904127318671836600, 0.9001942471269042123 ) ) ;
#151430 = CARTESIAN_POINT ( 'NONE',  ( -6.147696309153835692, 6.137010213626392208, 0.7998128361456281477 ) ) ;
#151431 = CARTESIAN_POINT ( 'NONE',  ( 7.450369105909416589, 8.650851030771185890, -1.199719254218441611 ) ) ;
#151432 = CARTESIAN_POINT ( 'NONE',  ( 6.821160681006788629, 8.091013894996997635, 1.082531754730549967 ) ) ;
#151433 = CARTESIAN_POINT ( 'NONE',  ( 0.000000000000000000, 4.569466175184296652, -2.600000000000000533 ) ) ;
#151435 = EDGE_CURVE ( 'NONE', #150164, #96695, #87447, .T. ) ;
#151434 = CARTESIAN_POINT ( 'NONE',  ( -4.062639585589296942, 7.891496616496157301, 0.7998128361456341429 ) ) ;
#151436 = CARTESIAN_POINT ( 'NONE',  ( 6.656690234185433042, 7.828855363713562276, -1.082531754730543971 ) ) ;
#151437 = CARTESIAN_POINT ( 'NONE',  ( 5.327099315257549428, 6.547468694062620997, 1.346473575380419563 ) ) ;
#151438 = CARTESIAN_POINT ( 'NONE',  ( -3.924195396151603177, 6.665646164563756138, 1.199719254218464037 ) ) ;
#151439 = CARTESIAN_POINT ( 'NONE',  ( 4.992532747203591192, -1.233408671777506349, 1.847344450390429937 ) ) ;
#151440 = CARTESIAN_POINT ( 'NONE',  ( 3.556733441538503016, -1.932615445784117369, -1.033156731641969195 ) ) ;
#151441 = CARTESIAN_POINT ( 'NONE',  ( -3.899941742225307539, 7.701682465904834629, 0.7998128361456341429 ) ) ;
#151442 = CARTESIAN_POINT ( 'NONE',  ( -3.363304624641834106, 6.081549941127532222, -1.199719254218452047 ) ) ;
#151443 = CARTESIAN_POINT ( 'NONE',  ( 5.389097038490845648, 0.1425914310585977562, 1.956722230749983193 ) ) ;
#151444 = CARTESIAN_POINT ( 'NONE',  ( -1.364683531250012516, 2.530208333674753174, 0.7879004041258379498 ) ) ;
#151445 = CARTESIAN_POINT ( 'NONE',  ( 6.889999999999973035, 7.629137130509064946, 2.879999999999991456 ) ) ;
#151446 = CARTESIAN_POINT ( 'NONE',  ( -4.717874267875590277, 7.487641831621378863, 1.082531754730560403 ) ) ;
#151448 = CARTESIAN_POINT ( 'NONE',  ( 4.922192346260840345, -2.110166376318895587, 0.2103620946037400852 ) ) ;
#151447 = AXIS2_PLACEMENT_3D ( 'NONE', #37061, #141021, #93320 ) ;
#151449 = CARTESIAN_POINT ( 'NONE',  ( -6.373741612200205076, 8.529394195690610303, 1.443375672974064550 ) ) ;
#151450 = ORIENTED_EDGE ( 'NONE', *, *, #89445, .F. ) ;
#151452 = CARTESIAN_POINT ( 'NONE',  ( 6.684453901184132185, -2.118919246787358102, -0.4271090584619871566 ) ) ;
#151451 = CARTESIAN_POINT ( 'NONE',  ( -4.651856103264620401, 8.441266197201775512, 0.000000000000000000 ) ) ;
#151453 = CARTESIAN_POINT ( 'NONE',  ( 3.832150974156964818, 7.622593236491780999, 1.040834085586084257E-14 ) ) ;
#151454 = CARTESIAN_POINT ( 'NONE',  ( 5.636236351835953506, 0.3653394402399374741, 1.804471444190151930 ) ) ;
#151455 = FILL_AREA_STYLE_COLOUR ( '', #99848 ) ;
#151456 = CARTESIAN_POINT ( 'NONE',  ( -1.364683531249997417, 2.571875000341422357, 1.214306433183764966E-14 ) ) ;
#151457 = CARTESIAN_POINT ( 'NONE',  ( 1.083124124047912362, -0.7835505874942759741, 1.554128773191378432 ) ) ;
#151458 = CARTESIAN_POINT ( 'NONE',  ( -1.500000000000008216, 11.28125000068279427, 3.469446951953614189E-15 ) ) ;
#151459 = CARTESIAN_POINT ( 'NONE',  ( -1.402160292154681736E-14, -0.8656249996585829720, 1.575800808251672791 ) ) ;
#151460 = DIRECTION ( 'NONE',  ( 0.000000000000000000, 0.000000000000000000, 1.000000000000000000 ) ) ;
#151461 = CARTESIAN_POINT ( 'NONE',  ( 5.823154874416164084, -0.05760400987671504547, 2.161107263091876618 ) ) ;
#151462 = CARTESIAN_POINT ( 'NONE',  ( -4.485049888022365927, 4.126979712314507331, 0.7998128361456341429 ) ) ;
#151463 = CARTESIAN_POINT ( 'NONE',  ( -7.171900071504748730, 8.429933507252760805, -1.082531754730549078 ) ) ;
#151465 = AXIS2_PLACEMENT_3D ( 'NONE', #127828, #30232, #78964 ) ;
#151464 = COLOUR_RGB ( '', 0.66274510, 0.83137255, 0.94901961) ;
#151466 = CARTESIAN_POINT ( 'NONE',  ( 4.487301133948972343, 1.932317252032596633, -0.9692046190768679459 ) ) ;
#151467 = CARTESIAN_POINT ( 'NONE',  ( -0.6823417656250212460, 2.801041667008084879, 1.181850606188767472 ) ) ;
#151468 = CARTESIAN_POINT ( 'NONE',  ( 4.587161778375014265, 1.762195453814468182, -0.8837856115832108950 ) ) ;
#151469 = CARTESIAN_POINT ( 'NONE',  ( 4.376141123711778214, -0.2964218048276610618, 1.708115672221988346 ) ) ;
#151470 = CARTESIAN_POINT ( 'NONE',  ( 1.118978350340808614, -0.04878210919301298465, 2.191179638975069732 ) ) ;
#151471 = CARTESIAN_POINT ( 'NONE',  ( 2.186954941700581134, -2.263197366206463279, -0.4496495349725088686 ) ) ;
#151472 = CARTESIAN_POINT ( 'NONE',  ( 4.798151449762615428, -2.060242214822493256, -0.05457638173838111340 ) ) ;
#151473 = CARTESIAN_POINT ( 'NONE',  ( 0.3220787244772654323, 1.858110058275804111, 0.5644625801373166496 ) ) ;
#151474 = CARTESIAN_POINT ( 'NONE',  ( -8.012505595552038784, 8.450270737673262644, 0.7216878364870578100 ) ) ;
#151476 = EDGE_CURVE ( 'NONE', #99491, #54687, #85623, .T. ) ;
#151475 = CARTESIAN_POINT ( 'NONE',  ( -6.154475385960665790, 6.144919136567696505, 0.000000000000000000 ) ) ;
#151477 = CARTESIAN_POINT ( 'NONE',  ( -9.404907903324922103, 15.51845925627663192, 7.453273793731242769 ) ) ;
#151478 = PRESENTATION_STYLE_ASSIGNMENT (( #167713 ) ) ;
#151479 = CARTESIAN_POINT ( 'NONE',  ( 1.283827520628720187, 1.646837967535810021, -1.163270716046126196 ) ) ;
#151480 = CARTESIAN_POINT ( 'NONE',  ( -7.510853911846401942, 7.865010440016681592, 1.040834085586084257E-14 ) ) ;
#151481 = CARTESIAN_POINT ( 'NONE',  ( 3.399657359236216703, 1.738403758043248759, 1.359216269546263511 ) ) ;
#151482 = CARTESIAN_POINT ( 'NONE',  ( 3.285556943749998737, -2.092708332855377051, -1.896917185911906500 ) ) ;
#151483 = CARTESIAN_POINT ( 'NONE',  ( 1.182201811662712210, 1.114302846955270709, -1.490276101724023583 ) ) ;
#151484 = CARTESIAN_POINT ( 'NONE',  ( 1.355131232792150309, 3.931394762486951411, -0.6431325189496895911 ) ) ;
#151485 = CARTESIAN_POINT ( 'NONE',  ( -0.2024025116386971856, -4.140708350189164832, 1.000000000000004441 ) ) ;
#151486 = CARTESIAN_POINT ( 'NONE',  ( 0.000000000000000000, 13.49999999999999822, 0.000000000000000000 ) ) ;
#151488 = CARTESIAN_POINT ( 'NONE',  ( -1.734723475976807094E-15, 2.999999999999988898, -6.938893903907228378E-15 ) ) ;
#151487 = CARTESIAN_POINT ( 'NONE',  ( -4.941402330188276792, 8.092876352253616901, -1.081280284042404727 ) ) ;
#151489 = CARTESIAN_POINT ( 'NONE',  ( 6.667912628260062036, -1.128459271250933149, 1.455361883854713767 ) ) ;
#151490 = ORIENTED_EDGE ( 'NONE', *, *, #425, .T. ) ;
#151491 = CARTESIAN_POINT ( 'NONE',  ( 2.852473085487742477, 0.6931051061056427987, 1.940986274177344706 ) ) ;
#151492 = CARTESIAN_POINT ( 'NONE',  ( 1.360316468750001784, 2.286458333674732835, -0.7853790794158941324 ) ) ;
#151493 = CARTESIAN_POINT ( 'NONE',  ( -6.663996196316808174, 7.733415969579778171, -1.199719254218446718 ) ) ;
#151494 = CARTESIAN_POINT ( 'NONE',  ( 2.367837350726550660, 0.5366352218779540939, -1.947015567076612941 ) ) ;
#151495 = DIRECTION ( 'NONE',  ( 0.6507913734559641616, -0.7592566023653004592, 0.000000000000000000 ) ) ;
#151496 = CARTESIAN_POINT ( 'NONE',  ( 3.684065054611349144, 5.321161868511784299, -1.599625672291262513 ) ) ;
#151497 = CARTESIAN_POINT ( 'NONE',  ( 1.745067373267340960, -1.741593738584124695, 1.101550882630119244 ) ) ;
#151498 = CARTESIAN_POINT ( 'NONE',  ( -8.012344526598182026E-15, 12.79687500034139802, -1.575800808251669460 ) ) ;
#151499 = CARTESIAN_POINT ( 'NONE',  ( 5.738125327081736060, 7.717565519727259904, 1.599625672291267398 ) ) ;
#151500 = AXIS2_PLACEMENT_3D ( 'NONE', #108242, #174265, #158008 ) ;
#151501 = CARTESIAN_POINT ( 'NONE',  ( -0.1408020194050328411, 7.629137130509059617, -2.700278568655100742 ) ) ;
#151502 = CARTESIAN_POINT ( 'NONE',  ( 5.110101661328442901, -2.196521081226535443, 0.2136625748923453583 ) ) ;
#151503 = CARTESIAN_POINT ( 'NONE',  ( 6.062430963966053632, 7.101866208495718702, -1.199719254218452047 ) ) ;
#151504 = CARTESIAN_POINT ( 'NONE',  ( 1.862795570070171713, -1.530026953448139659, 1.527182012981804560 ) ) ;
#151505 = CARTESIAN_POINT ( 'NONE',  ( -3.307826292054304673, 6.802955074131234348, -0.7216878364870267237 ) ) ;
#151506 = CARTESIAN_POINT ( 'NONE',  ( 2.184780103950241248, 1.616692242240840960, -1.205043568535242304 ) ) ;
#151507 = VECTOR ( 'NONE', #188340, 1000.000000000000000 ) ;
#151508 = EDGE_CURVE ( 'NONE', #152360, #104308, #152295, .T. ) ;
#151509 = CARTESIAN_POINT ( 'NONE',  ( 2.232162068744643069, -2.100961912546659871, -0.9323289839222002051 ) ) ;
#151510 = CARTESIAN_POINT ( 'NONE',  ( 1.499999999999989120, 6.200000000000045475, 2.580000000000000515 ) ) ;
#151511 = DIRECTION ( 'NONE',  ( 0.7592566023653004592, -0.6507913734559639396, -0.000000000000000000 ) ) ;
#151512 = CARTESIAN_POINT ( 'NONE',  ( 1.853667714121303600, 8.957164077253494838, -0.7749999999999996891 ) ) ;
#151513 = CARTESIAN_POINT ( 'NONE',  ( 1.850267049257280139, 0.5840378008528935849, 1.777222254475477659 ) ) ;
#151514 = CARTESIAN_POINT ( 'NONE',  ( 3.714077560468319827, 1.074663192196689376, -1.706111893292367343 ) ) ;
#151516 = DIRECTION ( 'NONE',  ( -5.578564026256490882E-16, -1.000000000000000000, -9.066213480720158442E-32 ) ) ;
#151515 = CARTESIAN_POINT ( 'NONE',  ( 1.364683531249986537, 2.405208333674752286, -0.7879004041258239610 ) ) ;
#151518 = CARTESIAN_POINT ( 'NONE',  ( 5.444006973519509351, 0.8546016068469390881, -1.925070404590538242 ) ) ;
#151517 = CARTESIAN_POINT ( 'NONE',  ( -6.340409392685171674, 10.54889472477470846, 0.7998128361456481317 ) ) ;
#151519 = CARTESIAN_POINT ( 'NONE',  ( 6.958359152311676787, 9.141171649162195934, -1.599625672291262513 ) ) ;
#151520 = CARTESIAN_POINT ( 'NONE',  ( -7.660520486921249983, 8.896027641951645748, -1.199719254218446718 ) ) ;
#151521 = CARTESIAN_POINT ( 'NONE',  ( 1.346800533732417149, 3.461515298693836229, 0.3345042947240741693 ) ) ;
#151522 = CARTESIAN_POINT ( 'NONE',  ( 5.326427914677607234, -0.9117507067677769195, -1.802394291917883473 ) ) ;
#151523 = CARTESIAN_POINT ( 'NONE',  ( -1.364683531249997417, 5.759375000341418804, 1.214306433183764966E-14 ) ) ;
#151524 = CARTESIAN_POINT ( 'NONE',  ( 1.305618366820593179, -1.623578218988607658, -1.271935013979957452 ) ) ;
#151525 = CARTESIAN_POINT ( 'NONE',  ( 7.293923454472077239, 10.49303254931736262, 1.082531754730558626 ) ) ;
#151526 = CARTESIAN_POINT ( 'NONE',  ( 5.169401708560450004, 9.252995436621013425, 0.000000000000000000 ) ) ;
#151527 = CARTESIAN_POINT ( 'NONE',  ( 4.538947565524982686, 8.517465603079630299, 0.000000000000000000 ) ) ;
#151528 = CARTESIAN_POINT ( 'NONE',  ( -0.6823417656250003738, 1.030208333674752286, -1.181850606188749264 ) ) ;
#151530 = CARTESIAN_POINT ( 'NONE',  ( 8.748013565000626102, 3.829536045110815135, 7.724821879577326911 ) ) ;
#151529 = CARTESIAN_POINT ( 'NONE',  ( 4.797606254389322089, 6.690569611577942943, 1.599625672291268286 ) ) ;
#151531 = CARTESIAN_POINT ( 'NONE',  ( 8.066738210006686671, 9.473911335505048825, 1.082531754730558626 ) ) ;
#151533 = CARTESIAN_POINT ( 'NONE',  ( -7.005397802120338469, 5.950282834973755541, -2.500000000000000000 ) ) ;
#151532 = CARTESIAN_POINT ( 'NONE',  ( 3.402935010178400166, 0.5245792999575286109, 2.106750930608875194 ) ) ;
#151535 = CARTESIAN_POINT ( 'NONE',  ( 1.680954830071922812, 1.270413995023990106, 1.332975479855981416 ) ) ;
#151534 = CARTESIAN_POINT ( 'NONE',  ( -3.931501358282937009, 7.530575984731317618, 0.7216878364870317197 ) ) ;
#151536 = CARTESIAN_POINT ( 'NONE',  ( -1.201851678989727383E-14, 2.696875000341417916, -1.575800808251660134 ) ) ;
#151537 = CARTESIAN_POINT ( 'NONE',  ( 4.599289333468261631, -0.5842463895667610041, 2.112197083089427885 ) ) ;
#151538 = CARTESIAN_POINT ( 'NONE',  ( 6.883263157960403333, 6.034387817901857964, 2.748704107105720773 ) ) ;
#151539 = CARTESIAN_POINT ( 'NONE',  ( 4.821284755203490313, -0.1158696699916968720, 2.259674544810440278 ) ) ;
#151540 = CARTESIAN_POINT ( 'NONE',  ( -6.338600509588822263, 7.353787668397130162, -1.199719254218446718 ) ) ;
#151542 = AXIS2_PLACEMENT_3D ( 'NONE', #6402, #187303, #8550 ) ;
#151541 = CYLINDRICAL_SURFACE ( 'NONE', #121761, 0.04999999999999991257 ) ;
#151543 = CARTESIAN_POINT ( 'NONE',  ( 5.273189713885392926, 7.658326211947664497, -1.220946906274408494 ) ) ;
#151544 = CARTESIAN_POINT ( 'NONE',  ( 1.499999999999993117, 13.60416666666666607, 0.8660254037844409281 ) ) ;
#151545 = CARTESIAN_POINT ( 'NONE',  ( -5.085717018457573957, 8.947437264926888290, 0.7216878364870267237 ) ) ;
#151546 = CARTESIAN_POINT ( 'NONE',  ( 4.258669648468281110, 6.061810238003387141, 1.443375672974058777 ) ) ;
#151547 = CARTESIAN_POINT ( 'NONE',  ( 5.659369745216535463, 0.3440881560464129629, -1.735765479537496603 ) ) ;
#151548 = CARTESIAN_POINT ( 'NONE',  ( 7.958799866421889746, 9.244020251369077457, -1.199719254218441611 ) ) ;
#151549 = CARTESIAN_POINT ( 'NONE',  ( 1.413257319143443658, 1.857191001717144685, 0.9929431703323916558 ) ) ;
#151551 = CARTESIAN_POINT ( 'NONE',  ( 0.7499999999999885647, 2.066666666666688634, -1.299038105676652899 ) ) ;
#151550 = CARTESIAN_POINT ( 'NONE',  ( 1.364683531249997417, 11.98437500034139980, 2.602085213965210642E-15 ) ) ;
#151553 = EDGE_CURVE ( 'NONE', #197417, #40273, #184295, .T. ) ;
#151552 = CARTESIAN_POINT ( 'NONE',  ( 1.504289420374326447, 1.967163215448018088, 0.09980459116839916767 ) ) ;
#151554 = AXIS2_PLACEMENT_3D ( 'NONE', #23409, #89520, #73227 ) ;
#151555 = DIRECTION ( 'NONE',  ( -0.000000000000000000, -1.000000000000000000, -0.000000000000000000 ) ) ;
#151556 = CARTESIAN_POINT ( 'NONE',  ( 0.4495626703563436743, 1.451167377975391304, 1.320406988977901985 ) ) ;
#151558 = ORIENTED_EDGE ( 'NONE', *, *, #169477, .T. ) ;
#151557 = CARTESIAN_POINT ( 'NONE',  ( 6.521734044569575062, -0.3839667898355834663, 1.776778520094610903 ) ) ;
#151559 = CARTESIAN_POINT ( 'NONE',  ( 6.670248388243460447, 6.884303995813253252, -0.7216878364870257245 ) ) ;
#151560 = CARTESIAN_POINT ( 'NONE',  ( -1.364683531250000748, 1.321875000341421469, 0.000000000000000000 ) ) ;
#151561 = EDGE_CURVE ( 'NONE', #71636, #6682, #21771, .T. ) ;
#151562 = CARTESIAN_POINT ( 'NONE',  ( 6.244977087980838171, -1.579202250953464670, 1.002420361074819688 ) ) ;
#151563 = CARTESIAN_POINT ( 'NONE',  ( 3.297657676621871925, 4.870353260857385180, 1.599625672291267398 ) ) ;
#151564 = CARTESIAN_POINT ( 'NONE',  ( 8.758160245764852192, 1.972237431423702114, 7.885882905890388095 ) ) ;
#151565 = CARTESIAN_POINT ( 'NONE',  ( 5.366107254901441692, -2.060797467674013284, 0.1973761227843511823 ) ) ;
#151566 = CARTESIAN_POINT ( 'NONE',  ( 1.224999999999957012, 2.854166666666677621, 0.7072540797572558491 ) ) ;
#151567 = CARTESIAN_POINT ( 'NONE',  ( -5.112833325684928987, 5.137596099486740897, -0.7216878364870338292 ) ) ;
#151568 = CARTESIAN_POINT ( 'NONE',  ( -5.204170427930421283E-14, 3.949999999999960654, -4.683753385137379155E-14 ) ) ;
#151569 = CARTESIAN_POINT ( 'NONE',  ( -1.402160292154681736E-14, 0.4625000000000214495, 1.732050807568877637 ) ) ;
#151570 = CARTESIAN_POINT ( 'NONE',  ( 8.101160479365381306, 9.410107633136481908, -1.199719254218446718 ) ) ;
#151571 = CARTESIAN_POINT ( 'NONE',  ( -8.910733272679575379, 11.41894145625809820, -1.599625672291263179 ) ) ;
#151572 = CARTESIAN_POINT ( 'NONE',  ( 5.885121196783658526, 9.023669275293071834, 1.199719254218452047 ) ) ;
#151573 = CARTESIAN_POINT ( 'NONE',  ( 0.6823417656249882723, 0.9260416670080831025, -1.181850606188749264 ) ) ;
#151575 = EDGE_CURVE ( 'NONE', #140594, #124513, #120456, .T. ) ;
#151574 = CARTESIAN_POINT ( 'NONE',  ( 0.7499999999999885647, 1.066666666666687968, -1.299038105676652899 ) ) ;
#151577 = CARTESIAN_POINT ( 'NONE',  ( 4.660252114795294887, 6.460046772059735432, -1.599625672291256295 ) ) ;
#151576 = CARTESIAN_POINT ( 'NONE',  ( 5.301206097546149465, -1.683542251207278628, 1.007010407901312465 ) ) ;
#151578 = CARTESIAN_POINT ( 'NONE',  ( 3.532577226125938274, 1.967586357134976094, -0.4389627639644277934 ) ) ;
#151579 = CARTESIAN_POINT ( 'NONE',  ( 2.712013535993620383, 1.060242027361221862, -1.595356271853585195 ) ) ;
#151580 = CARTESIAN_POINT ( 'NONE',  ( 1.499999999999990896, 4.556250000682819490, 1.214306433183764966E-14 ) ) ;
#151581 = CARTESIAN_POINT ( 'NONE',  ( 0.7674258922165803076, 2.110627382301712540, -0.5898035449652740958 ) ) ;
#151582 = CARTESIAN_POINT ( 'NONE',  ( 0.2335667940002502385, 6.947499997881678269, -2.748442024765639147 ) ) ;
#151583 = CARTESIAN_POINT ( 'NONE',  ( 2.741296213614560440, -1.383352855433259698, -1.259238407996167153 ) ) ;
#151584 = CARTESIAN_POINT ( 'NONE',  ( 0.7499999999999867883, -0.6520833326505159899, -1.299038105676652899 ) ) ;
#151585 = CARTESIAN_POINT ( 'NONE',  ( -7.157815033010924921, 10.43820240756634199, 1.199719254218453823 ) ) ;
#151587 = CARTESIAN_POINT ( 'NONE',  ( 4.253586407750776566, 2.053249321966661434, -0.5160394917872836995 ) ) ;
#151586 = CARTESIAN_POINT ( 'NONE',  ( -5.748293942514189681, 5.808690475795744490, -0.7216878364870207285 ) ) ;
#151588 = CARTESIAN_POINT ( 'NONE',  ( 4.255647627037052709E-16, 0.5000000000000004441, 3.475000000000000089 ) ) ;
#151589 = CARTESIAN_POINT ( 'NONE',  ( 6.285608408418759119, -1.950803066209889636, 0.6937918898708083093 ) ) ;
#151591 = CARTESIAN_POINT ( 'NONE',  ( 6.720655732516676473, 3.678797444539682271, 2.787578482799071278 ) ) ;
#151590 = CARTESIAN_POINT ( 'NONE',  ( 1.364907732811880159, 0.1502005422731657047, -2.085395908040136526 ) ) ;
#151593 = EDGE_LOOP ( 'NONE', ( #213358, #94490, #177696, #40095 ) ) ;
#151592 = CARTESIAN_POINT ( 'NONE',  ( 0.2172357734837098431, -1.693002290532450882, 0.3285655886510214230 ) ) ;
#151594 = CARTESIAN_POINT ( 'NONE',  ( 6.479907352327590964, 9.647310113435821677, 1.199719254218462483 ) ) ;
#151595 = CARTESIAN_POINT ( 'NONE',  ( 8.277047300324623436, 15.22811773329036278, 8.690146159871410703 ) ) ;
#151596 = CARTESIAN_POINT ( 'NONE',  ( 0.07933194154487524519, 7.849261790823902629, -9.499668754385622194 ) ) ;
#151597 = CARTESIAN_POINT ( 'NONE',  ( 5.788968402910802169, 8.737251655829183505, 1.082531754730558626 ) ) ;
#151598 = CARTESIAN_POINT ( 'NONE',  ( -0.6823417656250003738, 12.96354166700806942, 1.181850606188754593 ) ) ;
#151600 = CARTESIAN_POINT ( 'NONE',  ( 0.02954414540562703972, -1.776926038569931254, 0.3510683431443075153 ) ) ;
#151599 = CARTESIAN_POINT ( 'NONE',  ( 7.289443866002793371, 8.533381260871966134, 1.199719254218452047 ) ) ;
#151601 = CARTESIAN_POINT ( 'NONE',  ( -9.155833807930273238, 9.576227618873799585, -0.7998128361456291469 ) ) ;
#151602 = CARTESIAN_POINT ( 'NONE',  ( 4.333802657862601215, 8.207853534148366492, 0.7998128361456462443 ) ) ;
#151603 = CARTESIAN_POINT ( 'NONE',  ( 6.526270840131753737, 8.707344961610770540, -1.599625672291283607 ) ) ;
#151604 = CARTESIAN_POINT ( 'NONE',  ( 0.1969747848976802496, -6.717152734873738318, 10.87166355890666480 ) ) ;
#151605 = CARTESIAN_POINT ( 'NONE',  ( 3.997610708356745146, 7.599328567695712522, -0.1184163795967980992 ) ) ;
#151606 = CARTESIAN_POINT ( 'NONE',  ( 2.659370686574860976, 6.254349567645977714, -0.7998128361456291469 ) ) ;
#151607 = ORIENTED_EDGE ( 'NONE', *, *, #29138, .F. ) ;
#151608 = CARTESIAN_POINT ( 'NONE',  ( 5.677361293727043901, 1.528752376640944100, 1.314985542479940817 ) ) ;
#151609 = CARTESIAN_POINT ( 'NONE',  ( 0.3289748556246674394, 1.459166701075472750, -1.538843095060193233 ) ) ;
#151610 = CARTESIAN_POINT ( 'NONE',  ( 3.092648394857516525, 6.449253795920727228, -0.4031905389056261724 ) ) ;
#151612 = AXIS2_PLACEMENT_3D ( 'NONE', #33502, #113765, #99574 ) ;
#151611 = CIRCLE ( 'NONE', #75388, 0.8299999999999999600 ) ;
#151613 = CARTESIAN_POINT ( 'NONE',  ( 0.1405533004714617507, 0.6596865332844923380, -2.358301179948574244 ) ) ;
#151614 = CARTESIAN_POINT ( 'NONE',  ( 1.817552723627605671, 2.511586290612293659, 2.499391979724956414 ) ) ;
#151615 = CARTESIAN_POINT ( 'NONE',  ( -3.145128448690310830, 6.613140923539910787, -0.7216878364870267237 ) ) ;
#151616 = CARTESIAN_POINT ( 'NONE',  ( 8.107412671292022921, 12.40247251657532956, 0.7216878364870438212 ) ) ;
#151617 = CARTESIAN_POINT ( 'NONE',  ( 3.801571140118775727, -1.488283618643148287, -1.289908803443328145 ) ) ;
#151618 = ADVANCED_FACE ( 'NONE', ( #204798 ), #89054, .T. ) ;
#151619 = CARTESIAN_POINT ( 'NONE',  ( 1.594549238318817785, -1.131586138893545979, 1.793127659086241499 ) ) ;
#151620 = CARTESIAN_POINT ( 'NONE',  ( -7.067878151425722955, 7.140279352951794500, 0.7998128361456341429 ) ) ;
#151621 = CARTESIAN_POINT ( 'NONE',  ( 0.4423565646247452077, 3.073250980203122040, -0.4181372721656086977 ) ) ;
#151622 = CARTESIAN_POINT ( 'NONE',  ( -9.495541471879707984, -9.135662283479117463, 0.2985557471763422566 ) ) ;
#151623 = CARTESIAN_POINT ( 'NONE',  ( 5.701184558104195332, -0.5354452791076976803, 2.124913622581547479 ) ) ;
#151624 = CARTESIAN_POINT ( 'NONE',  ( 1.123270288250309612, 2.971052654332832610, -0.7749999999993620881 ) ) ;
#151625 = CARTESIAN_POINT ( 'NONE',  ( 4.489231697071988769, 1.720940496173857470, -0.8657641181536148700 ) ) ;
#151626 = CARTESIAN_POINT ( 'NONE',  ( -7.344766530301162000, 9.591980256816594164, 1.599625672291295375 ) ) ;
#151627 = ADVANCED_FACE ( 'NONE', ( #200537 ), #48800, .T. ) ;
#151628 = CARTESIAN_POINT ( 'NONE',  ( -0.1294898018152357000, 1.363479816416721446, -2.179679775322340696 ) ) ;
#151629 = CARTESIAN_POINT ( 'NONE',  ( 0.8739773845415177433, 2.125910683164092152, -0.5920798734769525673 ) ) ;
#151630 = DIRECTION ( 'NONE',  ( -3.451266460341926649E-31, -5.200010849845536803E-32, 1.000000000000000000 ) ) ;
#151631 = ORIENTED_EDGE ( 'NONE', *, *, #159020, .F. ) ;
#151632 = CARTESIAN_POINT ( 'NONE',  ( 5.411112705629925301, 5.485588709422586362, 0.000000000000000000 ) ) ;
#151633 = ORIENTED_EDGE ( 'NONE', *, *, #80469, .F. ) ;
#151634 = CARTESIAN_POINT ( 'NONE',  ( 5.787944378201490103, -1.246615054290018065, -1.524717904608218877 ) ) ;
#151635 = CARTESIAN_POINT ( 'NONE',  ( 0.7670095293261131042, 1.871311197688549699, -0.5191222856946677844 ) ) ;
#151636 = CARTESIAN_POINT ( 'NONE',  ( 6.028750418185333082, 2.265939813929934488, -0.3841603865788502103 ) ) ;
#151638 = CARTESIAN_POINT ( 'NONE',  ( 4.065176880270331417, 1.594224420893322725, 0.9597675150698461444 ) ) ;
#151637 = CARTESIAN_POINT ( 'NONE',  ( -5.271087860662956537, 9.371629280740593870, 0.000000000000000000 ) ) ;
#151639 = CARTESIAN_POINT ( 'NONE',  ( 6.607619761813720238, 8.802252036906432764, 1.599625672291268286 ) ) ;
#151640 = B_SPLINE_CURVE_WITH_KNOTS ( 'NONE', 3,
 ( #106768, #187947, #42811, #75283, #76344, #172797 ),
 .UNSPECIFIED., .F., .F.,
 ( 4, 2, 4 ),
 ( 0.0006305064395556263506, 0.0009448735008584378857, 0.001259240562161249421 ),
 .UNSPECIFIED. ) ;
#151641 = CARTESIAN_POINT ( 'NONE',  ( -6.507023659554960204, 9.678945805201045971, 1.199719254218452047 ) ) ;
#151642 = CARTESIAN_POINT ( 'NONE',  ( -3.933273961740340496, 5.682181936820735579, 1.443375672974065660 ) ) ;
#151643 = CARTESIAN_POINT ( 'NONE',  ( 0.7147126110796617748, 2.027027023440019171, 0.8336157706642086662 ) ) ;
#151644 = CARTESIAN_POINT ( 'NONE',  ( 4.772106882330221289, 6.590544000850479200, -1.443375672974051449 ) ) ;
#151645 = ORIENTED_EDGE ( 'NONE', *, *, #103939, .F. ) ;
#151646 = CARTESIAN_POINT ( 'NONE',  ( 9.567965691386879357, -9.756398209953340839, -0.1670094623740806250 ) ) ;
#151647 = CARTESIAN_POINT ( 'NONE',  ( 1.393942678861017859, 1.000000000000001332, -1.636894562288534472 ) ) ;
#151648 = CARTESIAN_POINT ( 'NONE',  ( 0.8733498553583609603, 1.760202786292342170, -0.4843115980177821744 ) ) ;
#151649 = CARTESIAN_POINT ( 'NONE',  ( -3.425406365747000859, 7.148057860013469877, 1.040834085586084257E-14 ) ) ;
#151650 = CARTESIAN_POINT ( 'NONE',  ( 2.953449220662739183, -1.603453536992532902, -0.6609773998737851208 ) ) ;
#151651 = DIRECTION ( 'NONE',  ( 0.9120491373041519356, 0.000000000000000000, -0.4100809324301145642 ) ) ;
#151652 = CARTESIAN_POINT ( 'NONE',  ( -11.07790593930098311, 9.799999999999998934, -0.7000000000000009548 ) ) ;
#151653 = CYLINDRICAL_SURFACE ( 'NONE', #133001, 1.500000000000000222 ) ;
#151654 = CARTESIAN_POINT ( 'NONE',  ( 5.531824841778981927, -1.161409778037244100, -1.408645805323349487 ) ) ;
#151655 = CARTESIAN_POINT ( 'NONE',  ( 3.309375504473045293, -1.601080850277468937, -1.133301831143386007 ) ) ;
#151656 = AXIS2_PLACEMENT_3D ( 'NONE', #191019, #59969, #123997 ) ;
#151657 = LINE ( 'NONE', #28040, #206615 ) ;
#151658 = CARTESIAN_POINT ( 'NONE',  ( -7.506410603460441422, 11.90922947067921278, -0.7998128361456291469 ) ) ;
#151659 = CARTESIAN_POINT ( 'NONE',  ( 8.125414133291656071, 8.374071331795406081, -0.7998128361456291469 ) ) ;
#151660 = CARTESIAN_POINT ( 'NONE',  ( 4.723349490952149843, 1.845327050471495367, 1.044454997443218236 ) ) ;
#151661 = CARTESIAN_POINT ( 'NONE',  ( 7.506374323821472849, 8.786466794993730289, -1.199719254218452047 ) ) ;
#151662 = FACE_OUTER_BOUND ( 'NONE', #24206, .T. ) ;
#151663 = CARTESIAN_POINT ( 'NONE',  ( 3.362232293424003426, -2.068089847843882279, 0.09686330349460009481 ) ) ;
#151665 = CARTESIAN_POINT ( 'NONE',  ( 1.364683531249986537, -0.07395833299191513499, 0.7879004041258500513 ) ) ;
#151664 = FILL_AREA_STYLE_COLOUR ( '', #137861 ) ;
#151666 = ORIENTED_EDGE ( 'NONE', *, *, #31466, .T. ) ;
#151668 = ORIENTED_EDGE ( 'NONE', *, *, #2591, .T. ) ;
#151667 = CARTESIAN_POINT ( 'NONE',  ( 4.319114520555938697, 1.717138752081597719, -1.409087234901666763 ) ) ;
#151669 = CARTESIAN_POINT ( 'NONE',  ( 3.428665021107531352, -1.741954984014550512, -1.499980572608774043 ) ) ;
#151670 = CARTESIAN_POINT ( 'NONE',  ( 8.351459436338029008, 10.76645531385962862, -1.443375672974063439 ) ) ;
#151672 = CARTESIAN_POINT ( 'NONE',  ( 3.285556943750000070, -2.034374999522043481, 0.000000000000000000 ) ) ;
#151671 = CARTESIAN_POINT ( 'NONE',  ( 7.349928672384120176, 7.747540670635879145, 0.7216878364870267237 ) ) ;
#151673 =( NAMED_UNIT ( * ) PLANE_ANGLE_UNIT ( ) SI_UNIT ( $, .RADIAN. ) );
#151674 = DIRECTION ( 'NONE',  ( -0.7592566023653016805, -0.6507913734559627184, 0.000000000000000000 ) ) ;
#151675 = DIRECTION ( 'NONE',  ( 0.000000000000000000, 0.000000000000000000, -1.000000000000000000 ) ) ;
#151676 = CARTESIAN_POINT ( 'NONE',  ( 3.638835171272115421, 1.817485770107383436, 0.5952672491930725007 ) ) ;
#151677 = DIRECTION ( 'NONE',  ( 0.000000000000000000, 1.000000000000000000, 0.000000000000000000 ) ) ;
#151678 = CARTESIAN_POINT ( 'NONE',  ( 4.541862270049739969, 0.7358753100316551832, -1.560062421326340987 ) ) ;
#151679 = CARTESIAN_POINT ( 'NONE',  ( 3.837125247982266174, -1.679222704393277921, -1.116210984008485507 ) ) ;
#151680 = CARTESIAN_POINT ( 'NONE',  ( 3.762538640753902097, 2.164199696370266324, -0.7750164773838670307 ) ) ;
#151681 = CARTESIAN_POINT ( 'NONE',  ( 11.41381675112453387, 10.89999999999998259, 3.704697986577180746 ) ) ;
#151682 = CARTESIAN_POINT ( 'NONE',  ( 6.164693330894345458, -1.490570670011469812, 1.488127047250583201 ) ) ;
#151683 = CARTESIAN_POINT ( 'NONE',  ( -6.183927461608886844, 7.347575139032721303, 1.082531754730548412 ) ) ;
#151684 = ORIENTED_EDGE ( 'NONE', *, *, #84119, .T. ) ;
#151685 = CARTESIAN_POINT ( 'NONE',  ( 4.446413189832159496, 0.4709973186826624802, 1.705850592114676489 ) ) ;
#151687 = CARTESIAN_POINT ( 'NONE',  ( 0.9027369068667027152, 1.732534852245724233, -1.501034128341944607 ) ) ;
#151686 = CARTESIAN_POINT ( 'NONE',  ( 6.068156270568149324, 9.237210194708310951, 1.199719254218452047 ) ) ;
#151688 = CARTESIAN_POINT ( 'NONE',  ( 0.1634481287224815171, -1.141006008805772298, 1.314205411033820381 ) ) ;
#151689 = CARTESIAN_POINT ( 'NONE',  ( 0.6386677588215936563, 4.335493988512285846, 0.1366812159789597692 ) ) ;
#151690 = MECHANICAL_DESIGN_GEOMETRIC_PRESENTATION_REPRESENTATION (  '', ( #2902 ), #137936 ) ;
#151691 = CARTESIAN_POINT ( 'NONE',  ( 6.597619724345276104, -2.191060131252516641, 0.04951108399064289151 ) ) ;
#151692 = CARTESIAN_POINT ( 'NONE',  ( -6.050681693448748177, 10.28115541899069463, 0.7998128361456291469 ) ) ;
#151693 = CARTESIAN_POINT ( 'NONE',  ( -11.84668730067608600, 13.40000000000000036, -1.400000000000001910 ) ) ;
#151694 = DIRECTION ( 'NONE',  ( -0.000000000000000000, -1.000000000000000000, 0.000000000000000000 ) ) ;
#151695 =( BOUNDED_CURVE ( )  B_SPLINE_CURVE ( 2, ( #62163, #93613, #63220, #129382, #45929, #145587, #109911 ),
 .UNSPECIFIED., .F., .T. ) 
 B_SPLINE_CURVE_WITH_KNOTS ( ( 3, 2, 2, 3 ),
 ( 0.2500000000000002220, 0.2559523809523810978, 0.2619047619047619735, 0.2678571428571428492 ),
 .UNSPECIFIED. ) 
 CURVE ( )  GEOMETRIC_REPRESENTATION_ITEM ( )  RATIONAL_B_SPLINE_CURVE ( ( 0.9999999999999950040, 0.8660254037844437036, 1.000000000000000000, 0.8660254037844387076, 1.000000000000000000, 0.8660254037844387076, 1.000000000000000000 ) ) 
 REPRESENTATION_ITEM ( '' )  );
#151696 = CARTESIAN_POINT ( 'NONE',  ( 6.830528382861658088, -1.277203763263988101, 1.630111558092485868 ) ) ;
#151697 = CARTESIAN_POINT ( 'NONE',  ( 1.235564962061060257, 0.5807501988173838781, -1.931125984888550473 ) ) ;
#151698 = CARTESIAN_POINT ( 'NONE',  ( -1.402160292154681736E-14, 0.4937500006828175469, 1.732050807568877637 ) ) ;
#151699 = CARTESIAN_POINT ( 'NONE',  ( 5.936148346467474468, 0.9475192508551170123, -1.677314091114836980 ) ) ;
#151700 = CARTESIAN_POINT ( 'NONE',  ( 0.6823417656249934904, 11.69270833367473017, 1.181850606188764807 ) ) ;
#151701 = CARTESIAN_POINT ( 'NONE',  ( 1.178328164221422503, 2.187401300010451077, -0.3865082640040794493 ) ) ;
#151703 = ORIENTED_EDGE ( 'NONE', *, *, #49463, .T. ) ;
#151702 = CARTESIAN_POINT ( 'NONE',  ( 8.367353357928214663, 12.91366268422496688, 1.040834085586084257E-14 ) ) ;
#151705 = DIRECTION ( 'NONE',  ( -0.000000000000000000, 1.000000000000000000, -0.000000000000000000 ) ) ;
#151704 = SURFACE_STYLE_USAGE ( .BOTH. , #71478 ) ;
#151706 = CARTESIAN_POINT ( 'NONE',  ( -5.655159470231558849, 6.730679149092498648, 1.082531754730549078 ) ) ;
#151707 = CARTESIAN_POINT ( 'NONE',  ( 9.752392566931574081, 10.27221283770866300, -0.7998128361456281477 ) ) ;
#151708 = CARTESIAN_POINT ( 'NONE',  ( 0.02680830797223074380, 7.629137130509076492, -2.410890733638766825 ) ) ;
#151709 = CARTESIAN_POINT ( 'NONE',  ( 3.832672171918658943, 7.347512574185182110, -0.5939728463272093695 ) ) ;
#151710 = CARTESIAN_POINT ( 'NONE',  ( 4.845099162036492046, 0.5397016130457911176, -1.654733517006673482 ) ) ;
#151711 = CARTESIAN_POINT ( 'NONE',  ( 1.978885927095444863, 1.829411362569667743, 0.7090815385668995940 ) ) ;
#151713 = CARTESIAN_POINT ( 'NONE',  ( -1.364683531250012516, 3.092708333674755838, 0.7879004041258379498 ) ) ;
#151712 = CARTESIAN_POINT ( 'NONE',  ( 3.161022370280501814, 6.839609865302569425, 0.000000000000000000 ) ) ;
#151714 = CARTESIAN_POINT ( 'NONE',  ( -5.912409256564314930, 5.999956524776160371, -0.009440138123966573813 ) ) ;
#151715 = DIRECTION ( 'NONE',  ( 0.000000000000000000, -1.301042606982654625E-17, -1.000000000000000000 ) ) ;
#151716 = CARTESIAN_POINT ( 'NONE',  ( 6.848121815800094936, -0.8396676627679277027, 1.771385694100804375 ) ) ;
#151717 = CARTESIAN_POINT ( 'NONE',  ( -7.914208982075130905, 10.25632978388623684, -1.599625672291263179 ) ) ;
#151718 = CARTESIAN_POINT ( 'NONE',  ( -4.324687812634898876, 6.068555086205916105, 1.443375672974064550 ) ) ;
#151719 = CARTESIAN_POINT ( 'NONE',  ( 1.147787885906520033, -1.784999543274916611, -1.390116309797536864 ) ) ;
#151720 = ORIENTED_EDGE ( 'NONE', *, *, #95454, .F. ) ;
#151721 = CARTESIAN_POINT ( 'NONE',  ( 0.7499999999999867883, -0.6520833326505159899, -1.299038105676652899 ) ) ;
#151722 = CARTESIAN_POINT ( 'NONE',  ( 1.545950201917587696, 1.868165254341861647, 0.09716206808172561660 ) ) ;
#151723 = CARTESIAN_POINT ( 'NONE',  ( 0.8087042982808723135, 1.034539495461658465, -1.391586887084266921 ) ) ;
#151724 = CARTESIAN_POINT ( 'NONE',  ( 5.372676843235411503, -0.05303982195071360595, -2.191091664329389399 ) ) ;
#151725 = CARTESIAN_POINT ( 'NONE',  ( 6.071339422564090427, 0.1780416842499404351, -2.300786051158403733 ) ) ;
#151726 = CARTESIAN_POINT ( 'NONE',  ( 1.270465292308793126, -1.308197635955485216, 1.592426268366262665 ) ) ;
#151727 = CARTESIAN_POINT ( 'NONE',  ( 3.415898659897542267, 1.231191954956109447, -1.501781470047100386 ) ) ;
#151728 = CARTESIAN_POINT ( 'NONE',  ( -3.429849674132936066, 6.945315686556313040, -0.7216878364870257245 ) ) ;
#151729 = CARTESIAN_POINT ( 'NONE',  ( 5.975831987570860981, 1.113884111790110820, 1.502598383168303409 ) ) ;
#151730 = EDGE_CURVE ( 'NONE', #135098, #79131, #172072, .T. ) ;
#151731 = CARTESIAN_POINT ( 'NONE',  ( 4.002655450416458649, 7.592114961386800864, 0.1875155472659401079 ) ) ;
#151732 = CARTESIAN_POINT ( 'NONE',  ( 6.591172692507557329, 1.163088239368128773, -1.646588791553056152 ) ) ;
#151733 = CARTESIAN_POINT ( 'NONE',  ( 4.502716413514295191, 6.346531463890372926, -1.443375672974068769 ) ) ;
#151734 = CARTESIAN_POINT ( 'NONE',  ( -3.755786496842899057E-14, 1.078125000341431106, -1.570758158831814466 ) ) ;
#151735 = CARTESIAN_POINT ( 'NONE',  ( 5.133435478496918947, 0.5880181904946503169, 1.928752423557971829 ) ) ;
#151736 = CARTESIAN_POINT ( 'NONE',  ( -3.090895833791289071, 6.549869539491048442, 1.040834085586084257E-14 ) ) ;
#151737 = CARTESIAN_POINT ( 'NONE',  ( 8.585337585951586803, 11.03931315507545108, -1.599625672291255185 ) ) ;
#151739 = CARTESIAN_POINT ( 'NONE',  ( 7.860745937262095140, -5.389939693150812339, -7.694877102302460692 ) ) ;
#151738 = CARTESIAN_POINT ( 'NONE',  ( 1.717148762710469789, -0.2249250470785572054, 1.811706739299999924 ) ) ;
#151740 = CARTESIAN_POINT ( 'NONE',  ( -6.134138155540168391, 6.121192367743780949, 0.000000000000000000 ) ) ;
#151741 = CARTESIAN_POINT ( 'NONE',  ( -4.359828915246279024, 7.244161613499399799, -1.199719254218455378 ) ) ;
#151742 = CARTESIAN_POINT ( 'NONE',  ( -9.911963570431085557, 5.384551446482307213, 6.114068938207696036 ) ) ;
#151743 = VERTEX_POINT ( 'NONE', #124734 ) ;
#151744 = CARTESIAN_POINT ( 'NONE',  ( -4.760321331729590710, 8.567808963744235839, 0.7216878364870267237 ) ) ;
#151745 = CARTESIAN_POINT ( 'NONE',  ( -1.292128843000315275, 8.373613470998943598, 10.90074592850030832 ) ) ;
#151746 = CARTESIAN_POINT ( 'NONE',  ( -4.112233706258869859, 7.668264228514641623, 0.7994708601795056380 ) ) ;
#151747 = CARTESIAN_POINT ( 'NONE',  ( 5.953772690328709594, -1.464304757327790973, -1.391265315224277099 ) ) ;
#151749 = ORIENTED_EDGE ( 'NONE', *, *, #3077, .T. ) ;
#151748 = CARTESIAN_POINT ( 'NONE',  ( 0.3289748556246673838, 1.459166701075472750, -1.538843095060193233 ) ) ;
#151750 = CARTESIAN_POINT ( 'NONE',  ( -7.422162748838431412, 7.623887726591770608, -0.7998128361456362523 ) ) ;
#151751 = CARTESIAN_POINT ( 'NONE',  ( 6.491656622844908853, 6.468020902940851968, 0.7998128361456341429 ) ) ;
#151752 = CARTESIAN_POINT ( 'NONE',  ( 5.032131441678504125, 1.061211460345131252, -1.766520746938464947 ) ) ;
#151753 = CARTESIAN_POINT ( 'NONE',  ( 4.693982515131527755, 1.755768268644173791, 0.9914009648221073778 ) ) ;
#151754 = VERTEX_POINT ( 'NONE', #192823 ) ;
#151755 = ORIENTED_EDGE ( 'NONE', *, *, #183608, .F. ) ;
#151756 = CARTESIAN_POINT ( 'NONE',  ( 9.797921721691059460, 3.956598013261175772, 6.103348209225848642 ) ) ;
#151757 = CARTESIAN_POINT ( 'NONE',  ( 3.379006598303866848, 4.965260336153046516, -1.599625672291262513 ) ) ;
#151758 =( BOUNDED_CURVE ( )  B_SPLINE_CURVE ( 2, ( #113880, #15213, #33609, #179875, #197174 ),
 .UNSPECIFIED., .F., .T. ) 
 B_SPLINE_CURVE_WITH_KNOTS ( ( 3, 2, 3 ),
 ( 0.2725899390149210122, 0.2750000000000000222, 0.2781713664827957233 ),
 .UNSPECIFIED. ) 
 CURVE ( )  GEOMETRIC_REPRESENTATION_ITEM ( )  RATIONAL_B_SPLINE_CURVE ( ( 0.9449186369899742477, 0.9612535663202994574, 1.000000000000000000, 0.9490140947219055656, 0.9368349873063581690 ) ) 
 REPRESENTATION_ITEM ( '' )  );
#151759 = MECHANICAL_DESIGN_GEOMETRIC_PRESENTATION_REPRESENTATION (  '', ( #20298 ), #203664 ) ;
#151761 = EDGE_LOOP ( 'NONE', ( #55369, #134010, #35320 ) ) ;
#151760 = CARTESIAN_POINT ( 'NONE',  ( -6.805266759416629618, 6.904175738932996964, 0.000000000000000000 ) ) ;
#151762 = CARTESIAN_POINT ( 'NONE',  ( 4.634937608369048334, 8.440560775401745985, -0.4060563726728562139 ) ) ;
#151763 = CARTESIAN_POINT ( 'NONE',  ( 4.868517441940229951, -0.5404072756688071966, 1.942244311778835719 ) ) ;
#151764 = CARTESIAN_POINT ( 'NONE',  ( 3.978315823851843014, -0.1823813840945518738, -1.832081410093854501 ) ) ;
#151765 = CARTESIAN_POINT ( 'NONE',  ( -2.492951620383208944, 8.266420250602596553, 2.456391984604374024 ) ) ;
#151766 = CARTESIAN_POINT ( 'NONE',  ( 1.858496626375233163, 2.301273984257983241, -0.1728945724901974068 ) ) ;
#151767 = CARTESIAN_POINT ( 'NONE',  ( 7.856023664475727308, 8.130058794835305136, -0.7998128361456341429 ) ) ;
#151768 = CARTESIAN_POINT ( 'NONE',  ( 4.675171183009182663, 0.005162144975975196948, -2.161773191939574179 ) ) ;
#151769 = CARTESIAN_POINT ( 'NONE',  ( 7.313733799568044702, 10.62010763521636214, 1.199719254218460707 ) ) ;
#151770 = CARTESIAN_POINT ( 'NONE',  ( 0.06387186515662347797, -1.267698835582967476, 1.471343342715900615 ) ) ;
#151771 = CARTESIAN_POINT ( 'NONE',  ( -4.954615070790188369, 7.867802451642154082, -1.199719254218452047 ) ) ;
#151772 = EDGE_CURVE ( 'NONE', #157888, #130259, #11448, .T. ) ;
#151773 = CARTESIAN_POINT ( 'NONE',  ( -9.472628840046096954, 15.37212083323948519, -7.367007921997711151 ) ) ;
#151774 = CARTESIAN_POINT ( 'NONE',  ( 3.133525119713890472, -1.255248497922526463, -1.387151338369890574 ) ) ;
#151775 = CARTESIAN_POINT ( 'NONE',  ( 6.666873957964818409, -1.802346848367493592, -0.7993007979140465125 ) ) ;
#151777 = SURFACE_STYLE_FILL_AREA ( #85689 ) ;
#151776 = CARTESIAN_POINT ( 'NONE',  ( -1.500000000000001332, -0.5687499993171779566, 0.000000000000000000 ) ) ;
#151778 = CARTESIAN_POINT ( 'NONE',  ( 1.577102763248950046, -2.096353118739826993, -0.6898709473643764856 ) ) ;
#151779 = CARTESIAN_POINT ( 'NONE',  ( 5.899206235277530297, 7.015400374979486209, -1.082531754730548412 ) ) ;
#151780 = CARTESIAN_POINT ( 'NONE',  ( 5.054492339796319733, 4.791329239384148231, -0.7998128361456211532 ) ) ;
#151781 = CARTESIAN_POINT ( 'NONE',  ( -3.100010679019018500, 6.768429558830820980, 1.040834085586084257E-14 ) ) ;
#151782 = CARTESIAN_POINT ( 'NONE',  ( -6.238160075619175515, 10.29195416494877513, 0.000000000000000000 ) ) ;
#151783 = CARTESIAN_POINT ( 'NONE',  ( 6.719606758044225359, -1.912400718708512581, 0.4786219606899063117 ) ) ;
#151784 = CARTESIAN_POINT ( 'NONE',  ( 6.235062949421072531, 0.2195253172713066969, 2.297251706954360095 ) ) ;
#151785 = CARTESIAN_POINT ( 'NONE',  ( 6.795359140062033454, -1.661660808857531313, 0.8381669064597346841 ) ) ;
#151786 = CARTESIAN_POINT ( 'NONE',  ( 3.889554661416291026, -1.907601829641421887, 0.7848441205193229520 ) ) ;
#151787 = CARTESIAN_POINT ( 'NONE',  ( 6.670248388243460447, 6.884303995813253252, -0.7216878364870257245 ) ) ;
#151788 = CARTESIAN_POINT ( 'NONE',  ( 5.020262018810099924, 9.078999131912302900, 0.7998128361456331437 ) ) ;
#151789 = ORIENTED_EDGE ( 'NONE', *, *, #6451, .T. ) ;
#151790 = CARTESIAN_POINT ( 'NONE',  ( 7.822691444960700125, 10.14955932391940330, -1.443375672974058777 ) ) ;
#151791 = CARTESIAN_POINT ( 'NONE',  ( 1.364683531249990311, 4.676041667008083103, 0.7879004041258500513 ) ) ;
#151792 = CARTESIAN_POINT ( 'NONE',  ( -10.61355984101064642, 4.139919643648435787, -5.602303138431320662 ) ) ;
#151793 = CARTESIAN_POINT ( 'NONE',  ( 5.816084710138150093, 5.887779704690372817, -0.7216878364870257245 ) ) ;
#151794 = CARTESIAN_POINT ( 'NONE',  ( 6.812935010865087015, -1.682745870255862641, 1.371614790115786908 ) ) ;
#151796 = CARTESIAN_POINT ( 'NONE',  ( 5.847170753249844033, 0.5281823367668266878, -1.763884204139199330 ) ) ;
#151795 = DIRECTION ( 'NONE',  ( 1.000000000000000000, -0.000000000000000000, -0.000000000000000000 ) ) ;
#151797 = CARTESIAN_POINT ( 'NONE',  ( 5.315329802055971165, 6.350237698360829519, -1.113282574169037531 ) ) ;
#151798 = DIRECTION ( 'NONE',  ( 0.000000000000000000, 0.000000000000000000, -1.000000000000000000 ) ) ;
#151799 = CARTESIAN_POINT ( 'NONE',  ( 1.334983872447586650, -1.693447605269988276, 0.7947349781701129601 ) ) ;
#151800 = CARTESIAN_POINT ( 'NONE',  ( -4.920796802804098924, 6.860114910817498135, 1.449587651302047364 ) ) ;
#151801 = CARTESIAN_POINT ( 'NONE',  ( 2.680963302752298993, 0.4788041664877049075, -8.638326563840814180E-32 ) ) ;
#151802 = EDGE_CURVE ( 'NONE', #91840, #21255, #2571, .T. ) ;
#151803 = CARTESIAN_POINT ( 'NONE',  ( 5.461903044330952639, 7.609029316319980474, -1.335476589331906494 ) ) ;
#151804 = CARTESIAN_POINT ( 'NONE',  ( -1.201851678989727383E-14, 4.759375000341419693, -1.575800808251660134 ) ) ;
#151805 = COLOUR_RGB ( '', 0.72549020, 0.75294118, 0.79215686) ;
#151806 = CARTESIAN_POINT ( 'NONE',  ( 1.611815888142430264, -0.6431676737995162263, 1.801018335096972400 ) ) ;
#151807 = CARTESIAN_POINT ( 'NONE',  ( 2.658786778619155022, -1.538754371767250495, -0.8742638447295988380 ) ) ;
#151808 = CARTESIAN_POINT ( 'NONE',  ( 6.463545146426397991, -1.618288576614915764, -1.197193900782191234 ) ) ;
#151810 = CARTESIAN_POINT ( 'NONE',  ( 4.060093344861609665, -1.099912525845229583, 1.568156085375242093 ) ) ;
#151809 = CARTESIAN_POINT ( 'NONE',  ( -2.290964770585000920, 5.616616632417037458, -0.7216878364870257245 ) ) ;
#151811 = DIRECTION ( 'NONE',  ( 1.000000000000000000, 0.000000000000000000, 0.000000000000000000 ) ) ;
#151812 = CARTESIAN_POINT ( 'NONE',  ( 5.740667673349629574, -1.921128208576441843, -0.4332487841941043971 ) ) ;
#151813 = CARTESIAN_POINT ( 'NONE',  ( 0.5805319366703353134, 1.050441701016215923, 1.842106252469346117 ) ) ;
#151814 = CARTESIAN_POINT ( 'NONE',  ( 7.671537448944488015E-16, 0.6185895741317448682, -6.264285714285709794 ) ) ;
#151815 = CARTESIAN_POINT ( 'NONE',  ( 4.346470048663173102, 0.4987854378066917116, 1.802870001028591407 ) ) ;
#151817 = ORIENTED_EDGE ( 'NONE', *, *, #125500, .T. ) ;
#151816 = CARTESIAN_POINT ( 'NONE',  ( 5.777914075412113881, 1.032862044635925569, 1.381300780159310460 ) ) ;
#151819 = CARTESIAN_POINT ( 'NONE',  ( 2.399429999938675007, 5.743159399996332404, 0.000000000000000000 ) ) ;
#151818 = CARTESIAN_POINT ( 'NONE',  ( 3.932405576212230525, 1.181341412803040614, -1.863887651898883613 ) ) ;
#151820 = CARTESIAN_POINT ( 'NONE',  ( -1.201851678989727383E-14, 4.509375000341417916, -1.575800808251660134 ) ) ;
#151821 = CARTESIAN_POINT ( 'NONE',  ( 1.240767406152184282, -2.011986688465472906, -0.4537849334574247107 ) ) ;
#151823 = AXIS2_PLACEMENT_3D ( 'NONE', #199204, #50851, #182974 ) ;
#151822 = CARTESIAN_POINT ( 'NONE',  ( 8.274553823041976841, 8.548067636504127265, 1.040834085586084257E-14 ) ) ;
#151824 = CARTESIAN_POINT ( 'NONE',  ( -7.479294296233107708, 11.87759377891399204, 0.7998128361456481317 ) ) ;
#151825 = CARTESIAN_POINT ( 'NONE',  ( 5.397554552016226914, 6.430140077841320689, 1.082531754730549078 ) ) ;
#151826 = CARTESIAN_POINT ( 'NONE',  ( -3.432209171205097498, -0.01729076450818782182, -0.4009769568943012397 ) ) ;
#151827 = CARTESIAN_POINT ( 'NONE',  ( -7.401194801147281233, -6.836289462023139585, -7.952857047017147352 ) ) ;
#151828 = ORIENTED_EDGE ( 'NONE', *, *, #19138, .F. ) ;
#151829 = CARTESIAN_POINT ( 'NONE',  ( 3.297389726143421740, -1.827171938055579536, 0.9735347560282039403 ) ) ;
#151830 = CARTESIAN_POINT ( 'NONE',  ( -1.001543065824772872E-14, 4.962500000000019007, 1.732050807568877637 ) ) ;
#151831 = CARTESIAN_POINT ( 'NONE',  ( 6.308621549060418054, 6.254479983525607523, 0.7998128361456341429 ) ) ;
#151832 = CARTESIAN_POINT ( 'NONE',  ( -6.472689817967896886, 6.776322833669464529, -0.2902398332882798471 ) ) ;
#151833 = CARTESIAN_POINT ( 'NONE',  ( 1.401042149647635071, -0.2984598639739938220, -1.997379878556293731 ) ) ;
#151834 = ADVANCED_FACE ( 'NONE', ( #9817 ), #110597, .T. ) ;
#151836 = CARTESIAN_POINT ( 'NONE',  ( 8.487040972474689582, 9.964264558384387627, -1.082531754730543083 ) ) ;
#151835 = CARTESIAN_POINT ( 'NONE',  ( 0.07479286986305369589, 4.095183424177953668, -2.410510762676120411 ) ) ;
#151837 = CARTESIAN_POINT ( 'NONE',  ( 6.274767501101933043, -2.001204493855372579, 0.2439949869823473949 ) ) ;
#151838 = CARTESIAN_POINT ( 'NONE',  ( 5.964071289222036221, -1.018598136897935547, 1.622275196354412419 ) ) ;
#151839 = CARTESIAN_POINT ( 'NONE',  ( 4.300438532332786501, 1.693616701070689956, -1.390861761948622544 ) ) ;
#151840 = CARTESIAN_POINT ( 'NONE',  ( -1.500000000000011324, 3.952083334016153415, 0.8660254037844403729 ) ) ;
#151841 = CARTESIAN_POINT ( 'NONE',  ( 3.709155072767254424, 1.612916391665040194, -1.027221078234448859 ) ) ;
#151842 = CARTESIAN_POINT ( 'NONE',  ( -6.078132937628113908, 5.985576603521232109, 1.040834085586084257E-14 ) ) ;
#151843 = CARTESIAN_POINT ( 'NONE',  ( 4.826339496340538382, 4.733076955259818419, 1.040834085586084257E-14 ) ) ;
#151845 = CARTESIAN_POINT ( 'NONE',  ( 0.4918148228068714989, -2.006445053647107013, 0.2004575690456936732 ) ) ;
#151844 = CARTESIAN_POINT ( 'NONE',  ( 1.734723475976806897E-15, 14.57308041853048408, 11.91973154060107376 ) ) ;
#151846 = CARTESIAN_POINT ( 'NONE',  ( -0.6823417656250039265, 11.13020833367473017, -1.181850606188755259 ) ) ;
#151847 = AXIS2_PLACEMENT_3D ( 'NONE', #211414, #46821, #45752 ) ;
#151849 = CARTESIAN_POINT ( 'NONE',  ( -4.444040490229335560, 8.406740681901359480, 0.7998128361456352531 ) ) ;
#151848 = CARTESIAN_POINT ( 'NONE',  ( 6.058177568126345669, -1.550975213528119623, 1.548612826651605712 ) ) ;
#151851 = ORIENTED_EDGE ( 'NONE', *, *, #87756, .T. ) ;
#151850 = CARTESIAN_POINT ( 'NONE',  ( 4.172648073627690302, -1.609630772656017950, -0.6200716988599298540 ) ) ;
#151852 = FILL_AREA_STYLE_COLOUR ( '', #71068 ) ;
#151853 = CARTESIAN_POINT ( 'NONE',  ( 6.825640269476072497, 10.05066518344239412, 1.199719254218460707 ) ) ;
#151854 = CARTESIAN_POINT ( 'NONE',  ( 3.472859903394816872, 7.203420320602605287, -0.7998128361456291469 ) ) ;
#151855 = CARTESIAN_POINT ( 'NONE',  ( -11.44789321844504215, 12.30000000000000249, -3.303298730975397834 ) ) ;
#151856 = CARTESIAN_POINT ( 'NONE',  ( 1.469116868872882620, 1.728625619535430369, 0.9278086228877155950 ) ) ;
#151857 = EDGE_CURVE ( 'NONE', #35104, #214101, #199717, .T. ) ;
#151858 = CARTESIAN_POINT ( 'NONE',  ( 1.123270288250308280, 2.860197346350005887, 0.7749999999993786304 ) ) ;
#151859 = CARTESIAN_POINT ( 'NONE',  ( 0.1751657365761339624, 7.629137130509054288, -2.644001943226172102 ) ) ;
#151860 = ORIENTED_EDGE ( 'NONE', *, *, #147272, .T. ) ;
#151861 = CARTESIAN_POINT ( 'NONE',  ( -0.3000000000000172529, 3.975028841772365595, -0.9637995837462973725 ) ) ;
#151862 = ORIENTED_EDGE ( 'NONE', *, *, #28043, .T. ) ;
#151863 = CARTESIAN_POINT ( 'NONE',  ( 3.896947601784990223, -0.1811674076915045506, -1.802394175579679958 ) ) ;
#151864 = EDGE_LOOP ( 'NONE', ( #136683, #194384, #184902 ) ) ;
#151865 = CARTESIAN_POINT ( 'NONE',  ( 6.852720297064418986, 6.959538199522133262, 0.7998128361456331437 ) ) ;
#151866 = CARTESIAN_POINT ( 'NONE',  ( 7.834948825496932834, -9.999999999999994671, 7.720982897393586342 ) ) ;
#151867 = CARTESIAN_POINT ( 'NONE',  ( 5.408800935855493819, -0.4461688933581753336, -1.755527745762341718 ) ) ;
#151868 = CARTESIAN_POINT ( 'NONE',  ( 8.136301581532414673, 8.664975731308866003, 0.000000000000000000 ) ) ;
#151869 = PRESENTATION_LAYER_ASSIGNMENT (  '', '', ( #30811 ) ) ;
#151870 = CARTESIAN_POINT ( 'NONE',  ( -6.761669295867164031, -7.008190897455700785, -6.673079560224742579 ) ) ;
#151871 = CARTESIAN_POINT ( 'NONE',  ( 5.786614514570532997, 6.041473168147688533, -0.5398422057949890940 ) ) ;
#151873 = CARTESIAN_POINT ( 'NONE',  ( 1.364683531250000303, 15.25520833367473017, -0.7879004041258355073 ) ) ;
#151872 = CARTESIAN_POINT ( 'NONE',  ( 4.633164157742322153, 0.0009153448507570947738, -1.861241882716960561 ) ) ;
#151874 = CARTESIAN_POINT ( 'NONE',  ( 2.548326723280808892, -1.319200400300493570, 1.389225609306585119 ) ) ;
#151875 = CARTESIAN_POINT ( 'NONE',  ( -6.773376336900938099, -7.645781813054123965, -6.661184053808324457 ) ) ;
#151876 = CARTESIAN_POINT ( 'NONE',  ( -10.50659947519749693, 5.359800460605414152, -5.105385958519358169 ) ) ;
#151877 = CARTESIAN_POINT ( 'NONE',  ( 4.380693030546900957, 8.124909279031152565, 0.7216878364870219498 ) ) ;
#151878 = CARTESIAN_POINT ( 'NONE',  ( 5.938108093105483931, 8.911247961056314892, -1.082531754730537088 ) ) ;
#151879 = EDGE_CURVE ( 'NONE', #210693, #129573, #168646, .T. ) ;
#151880 = CARTESIAN_POINT ( 'NONE',  ( -9.815740026613960723, 11.51441345488021106, -1.082531754730539753 ) ) ;
#151881 = CARTESIAN_POINT ( 'NONE',  ( 0.5675189469334165349, 0.2105291993744831114, -2.151437729447757796 ) ) ;
#151882 = CARTESIAN_POINT ( 'NONE',  ( -5.237192476628793614, 9.332084666034067055, 0.7998128361456291469 ) ) ;
#151883 = CARTESIAN_POINT ( 'NONE',  ( 6.527324610336440180, 6.579909898339485252, 0.7998128361456331437 ) ) ;
#151884 = CARTESIAN_POINT ( 'NONE',  ( 0.7447965706881398695, -1.568309060004613231, 0.9341869532639992535 ) ) ;
#151885 = CARTESIAN_POINT ( 'NONE',  ( -3.744022975668147790, 7.519777238254810925, -0.7998128361456281477 ) ) ;
#151886 = EDGE_CURVE ( 'NONE', #55386, #173258, #213624, .T. ) ;
#151887 = CARTESIAN_POINT ( 'NONE',  ( 2.362075219488588562, 0.7782009281872975803, 1.651537983114875763 ) ) ;
#151888 = CARTESIAN_POINT ( 'NONE',  ( 10.32570460010716396, 11.37497670666806826, 7.285500311179339938 ) ) ;
#151889 = CARTESIAN_POINT ( 'NONE',  ( 3.139063269091638908, -0.1420806666206550495, -1.964468959564101613 ) ) ;
#151890 = CARTESIAN_POINT ( 'NONE',  ( 3.755361975916061024, 1.927010760186953497, -0.2409419434407939486 ) ) ;
#151891 = CARTESIAN_POINT ( 'NONE',  ( -3.142457743317409680, 6.888227477170756785, 0.7998128361456352531 ) ) ;
#151893 = CARTESIAN_POINT ( 'NONE',  ( 4.517907016363444939, -0.5628432189327194912, 2.044499502628312371 ) ) ;
#151892 = CARTESIAN_POINT ( 'NONE',  ( 7.452141709366786770, 8.723195411463290583, 1.199719254218452047 ) ) ;
#151894 = CARTESIAN_POINT ( 'NONE',  ( 6.776370306708059843, -7.161464053357565973, 6.781144757626057284 ) ) ;
#151895 = CARTESIAN_POINT ( 'NONE',  ( 8.341290820905593151, 10.75459192918846618, 1.599625672291281386 ) ) ;
#151896 = B_SPLINE_CURVE_WITH_KNOTS ( 'NONE', 3,
 ( #64497, #196631, #145791, #99139, #180380, #181431 ),
 .UNSPECIFIED., .F., .F.,
 ( 4, 2, 4 ),
 ( 0.000000000000000000, 0.0003147459536107448494, 0.0006294919072214896988 ),
 .UNSPECIFIED. ) ;
#151897 = CARTESIAN_POINT ( 'NONE',  ( 6.055847235078346991, 6.052673195394750572, 0.4411178842869938888 ) ) ;
#151898 = DIRECTION ( 'NONE',  ( 0.03984146075563036599, -3.484297484818016589E-16, 0.9992060137953822085 ) ) ;
#151899 = CARTESIAN_POINT ( 'NONE',  ( 7.049313524462606395, 7.188896964819984525, 0.000000000000000000 ) ) ;
#151900 = CARTESIAN_POINT ( 'NONE',  ( 11.96209379583854115, 12.27207059405763445, -0.9572398070798752157 ) ) ;
#151901 = CARTESIAN_POINT ( 'NONE',  ( 4.230939532379584200, 0.09184734775685021724, 1.823503176236190626 ) ) ;
#151902 = CARTESIAN_POINT ( 'NONE',  ( 10.99952653502853117, -9.917017194762472343, -0.1020740558599437658 ) ) ;
#151903 = CARTESIAN_POINT ( 'NONE',  ( -8.012505595996376684, 12.29174759539704986, 0.000000000000000000 ) ) ;
#151904 =( GEOMETRIC_REPRESENTATION_CONTEXT ( 3 ) GLOBAL_UNCERTAINTY_ASSIGNED_CONTEXT ( ( #122240 ) ) GLOBAL_UNIT_ASSIGNED_CONTEXT ( ( #116833, #166598, #18187 ) ) REPRESENTATION_CONTEXT ( 'NONE', 'WORKASPACE' ) );
#151905 = CARTESIAN_POINT ( 'NONE',  ( -4.948302019123040019, 8.085739352127342627, 1.088677458455259650 ) ) ;
#151906 = CARTESIAN_POINT ( 'NONE',  ( 6.903494779225153977, -6.732807188596972026, -6.688963559358321653 ) ) ;
#151907 = CARTESIAN_POINT ( 'NONE',  ( 4.768341783539651324, -1.221614081569386334, 1.416756073533788518 ) ) ;
#151908 = CARTESIAN_POINT ( 'NONE',  ( 7.938462636001388795, 9.220293482545153907, -1.199719254218441611 ) ) ;
#151909 = CARTESIAN_POINT ( 'NONE',  ( 3.088414555603569145, -1.898068263532082245, -0.3288968790781700013 ) ) ;
#151910 = CARTESIAN_POINT ( 'NONE',  ( 6.684431423333510480, 1.132142624513672091, -1.601896353945003071 ) ) ;
#151911 = CARTESIAN_POINT ( 'NONE',  ( 3.005103603723342953, 6.657704637652544832, -0.7998128361456291469 ) ) ;
#151912 = CARTESIAN_POINT ( 'NONE',  ( -0.6823417656250039265, 9.380208333674728394, -1.181850606188755259 ) ) ;
#151913 = CARTESIAN_POINT ( 'NONE',  ( -5.540478329478883524, 9.615641817700700145, 0.000000000000000000 ) ) ;
#151914 = CARTESIAN_POINT ( 'NONE',  ( 3.225950485047770933, 5.851027101609320269, 1.199719254218450271 ) ) ;
#151915 = CARTESIAN_POINT ( 'NONE',  ( -3.485854892044998543, 6.120562236477518070, -1.082531754730546636 ) ) ;
#151916 = CARTESIAN_POINT ( 'NONE',  ( 1.722414120629287337, 2.094725599053618659, 0.3070382465363735158 ) ) ;
#151917 = CARTESIAN_POINT ( 'NONE',  ( 9.215791728987056786, 11.77484298861683598, -1.599625672291262513 ) ) ;
#151918 = CARTESIAN_POINT ( 'NONE',  ( 0.3542539638296999804, 6.983552608457117117, 3.850577409504350346 ) ) ;
#151919 = CARTESIAN_POINT ( 'NONE',  ( 6.157099584139436033, 1.695871835526874483, -1.187180358042688511 ) ) ;
#151921 = CARTESIAN_POINT ( 'NONE',  ( 4.015052158831055706, 7.807088067957844046, 0.2846288760043579336 ) ) ;
#151920 = CARTESIAN_POINT ( 'NONE',  ( 0.3449248370967008537, 0.5783895242766275979, -1.748133987124582012 ) ) ;
#151922 = CARTESIAN_POINT ( 'NONE',  ( 5.942043047034061942, -1.969448396301001436, -1.185220976332189924 ) ) ;
#151923 = CARTESIAN_POINT ( 'NONE',  ( 6.317736394288140822, 7.433409217166723870, 1.082531754730558626 ) ) ;
#151924 = CARTESIAN_POINT ( 'NONE',  ( 4.095971805104285934, 6.832365301713403838, 1.082531754730549078 ) ) ;
#151925 = CARTESIAN_POINT ( 'NONE',  ( 1.781587602986109742, 1.582980622272272653, 1.658122128702421261 ) ) ;
#151926 = CARTESIAN_POINT ( 'NONE',  ( -1.164422670175135899, 3.300000000000025135, -0.7116747751938151678 ) ) ;
#151927 = CARTESIAN_POINT ( 'NONE',  ( -5.367048706163331850, 7.354919138647580290, -1.599625672291271394 ) ) ;
#151928 = CARTESIAN_POINT ( 'NONE',  ( 5.648367429523982963, -1.529681991043756017, 1.196244224141077561 ) ) ;
#151929 = CARTESIAN_POINT ( 'NONE',  ( 8.907343734053986495, 9.494248565925552441, -0.7216878364870197293 ) ) ;
#151930 = CARTESIAN_POINT ( 'NONE',  ( 0.7912717950901988484, -0.05365516122857225123, -2.012662812414119706 ) ) ;
#151931 = CARTESIAN_POINT ( 'NONE',  ( 6.350795928397162449, -1.845624747684541989, -0.8128223418941012968 ) ) ;
#151933 = CARTESIAN_POINT ( 'NONE',  ( -10.48884024596653397, 1.000000000000000888, 5.608780650328914597 ) ) ;
#151932 = CARTESIAN_POINT ( 'NONE',  ( -7.178152263431422320, 10.46192917639026554, 1.199719254218453823 ) ) ;
#151934 = FACE_OUTER_BOUND ( 'NONE', #28913, .T. ) ;
#151935 = EDGE_CURVE ( 'NONE', #139509, #119003, #75281, .T. ) ;
#151937 = CARTESIAN_POINT ( 'NONE',  ( 1.393014870165907526, 1.336991634843522236, 1.159753417114619545 ) ) ;
#151936 = CARTESIAN_POINT ( 'NONE',  ( 2.765665077289869433, 1.118955468730401526, 1.765788254259098800 ) ) ;
#151938 = CARTESIAN_POINT ( 'NONE',  ( 4.194756697597139983, 7.186718463257284917, 1.144634955760708950 ) ) ;
#151940 = CARTESIAN_POINT ( 'NONE',  ( 4.593851424282248352, -2.291655481657675519, -0.05911330884650690953 ) ) ;
#151939 = CARTESIAN_POINT ( 'NONE',  ( -11.68361888283353522, 7.298829597232358246, -2.746533259346354505 ) ) ;
#151941 = B_SPLINE_CURVE_WITH_KNOTS ( 'NONE', 3,
 ( #45230, #109220, #191440, #42034, #92919, #60382, #208757, #128682 ),
 .UNSPECIFIED., .F., .F.,
 ( 4, 2, 2, 4 ),
 ( 0.000000000000000000, 0.0001985720215089326513, 0.0003971440430178653025, 0.0007942880860357295209 ),
 .UNSPECIFIED. ) ;
#151942 = CARTESIAN_POINT ( 'NONE',  ( 3.169568575122613918, -1.035934168062458971, 1.398253053441183891 ) ) ;
#151943 = CARTESIAN_POINT ( 'NONE',  ( 10.70146331988817323, 11.37946204949139251, 0.7998128361456341429 ) ) ;
#151944 = VECTOR ( 'NONE', #63579, 1000.000000000000000 ) ;
#151945 = CARTESIAN_POINT ( 'NONE',  ( 4.227110032410640095, 8.153655147779589996, 0.7998128361456271485 ) ) ;
#151946 = CARTESIAN_POINT ( 'NONE',  ( 3.725721709451996322, -1.528540617003815383, -0.8183948105100163906 ) ) ;
#151947 = CARTESIAN_POINT ( 'NONE',  ( 3.121698260611803999, 0.3212384671735257213, -2.147181447086630612 ) ) ;
#151948 = CARTESIAN_POINT ( 'NONE',  ( 6.010342169559767633, 5.906487374108181143, -0.7998128361456281477 ) ) ;
#151949 = ADVANCED_FACE ( 'NONE', ( #42353 ), #57517, .T. ) ;
#151950 = CARTESIAN_POINT ( 'NONE',  ( 4.030482632556767975, 0.5424685788828055300, 1.942097399793737633 ) ) ;
#151951 = CARTESIAN_POINT ( 'NONE',  ( 1.718750000000001554, -0.7852924748298989455, 1.895863743164124093 ) ) ;
#151952 = CARTESIAN_POINT ( 'NONE',  ( -1.500000000000011324, 4.452083334016148086, 0.8660254037844403729 ) ) ;
#151953 = CARTESIAN_POINT ( 'NONE',  ( 2.133698649363345190, -1.256510270340875035, -1.460289853754138445 ) ) ;
#151954 = CARTESIAN_POINT ( 'NONE',  ( -1.500000000000015099, 8.760416667349462116, -0.8660254037844309360 ) ) ;
#151955 = CARTESIAN_POINT ( 'NONE',  ( 4.307018013452124983, -0.4884699388765164074, -2.166881332863872522 ) ) ;
#151956 = ORIENTED_EDGE ( 'NONE', *, *, #192264, .T. ) ;
#151957 = CARTESIAN_POINT ( 'NONE',  ( -0.1108833634137010582, 5.723767666350643601, -2.491012016648496363 ) ) ;
#151958 = CARTESIAN_POINT ( 'NONE',  ( -1.402160292154681736E-14, 2.337500000000022560, -1.732050807568863648 ) ) ;
#151959 = CARTESIAN_POINT ( 'NONE',  ( 5.126954644262057492, 9.133197518281081173, 0.7998128361456462443 ) ) ;
#151960 = CARTESIAN_POINT ( 'NONE',  ( 5.477130869796502211, 5.492333557625114437, 1.040834085586084257E-14 ) ) ;
#151961 = CARTESIAN_POINT ( 'NONE',  ( 1.642778471875001811, -2.442708332855377140, 2.845375778867859751 ) ) ;
#151962 = CARTESIAN_POINT ( 'NONE',  ( 0.8389114244844765311, 1.318684809372525857, -1.787403929136616165 ) ) ;
#151963 = CARTESIAN_POINT ( 'NONE',  ( 6.109812101310618360, 0.5708666350849946891, -1.876949146916474298 ) ) ;
#151964 = CARTESIAN_POINT ( 'NONE',  ( 7.402388683381404988, 10.61957531637824204, -1.082531754730537976 ) ) ;
#151965 = TOROIDAL_SURFACE ( 'NONE', #103565, 2.149999999999999911, 0.1000000000000000056 ) ;
#151966 = PRESENTATION_STYLE_ASSIGNMENT (( #38210 ) ) ;
#151967 = CARTESIAN_POINT ( 'NONE',  ( 6.731690493876715919, -1.469984723218084488, -1.719904613669322790 ) ) ;
#151968 = CARTESIAN_POINT ( 'NONE',  ( 6.201928923608456046, 6.200281597156833691, 0.7998128361456352531 ) ) ;
#151969 = CARTESIAN_POINT ( 'NONE',  ( -5.045042558060949034, 6.018876084893449274, 1.082531754730549078 ) ) ;
#151970 = CARTESIAN_POINT ( 'NONE',  ( 4.527816470857299436, 2.001556401900002058, -0.4979991880497411372 ) ) ;
#151971 = CARTESIAN_POINT ( 'NONE',  ( -6.091691091241777656, 6.001394449403842479, 0.7998128361456341429 ) ) ;
#151972 = CARTESIAN_POINT ( 'NONE',  ( -1.201851678989727383E-14, 3.868750000682817713, -1.732050807568863648 ) ) ;
#151973 = CARTESIAN_POINT ( 'NONE',  ( -1.364683531250010295, 5.801041667008088432, -0.7879004041258300672 ) ) ;
#151974 = CARTESIAN_POINT ( 'NONE',  ( 6.046149701670225696, 1.868418987705861234, 0.09211505606019491921 ) ) ;
#151975 = CARTESIAN_POINT ( 'NONE',  ( 4.201623210320468260, 1.587898197979008774, 0.6974748919710629380 ) ) ;
#151976 = CARTESIAN_POINT ( 'NONE',  ( 3.720004753662985664, 1.653986544816415494, 0.5419736716202552262 ) ) ;
#151977 = CARTESIAN_POINT ( 'NONE',  ( 1.716775041481681585, 2.140780187006920077, 0.8202503203454788450 ) ) ;
#151978 = CARTESIAN_POINT ( 'NONE',  ( -0.6823417656249969321, 4.280208333674755394, -1.181850606188749264 ) ) ;
#151979 = CARTESIAN_POINT ( 'NONE',  ( 5.917543283689063571, -1.162172991910553010, -1.737764066907695915 ) ) ;
#151980 = CARTESIAN_POINT ( 'NONE',  ( 6.404245030721173570, 1.437354257190478490, -1.306004427266238777 ) ) ;
#151981 = CARTESIAN_POINT ( 'NONE',  ( 3.469446951953614189E-15, 5.167241622962441383, 1.214306433183764966E-14 ) ) ;
#151982 = PRESENTATION_STYLE_ASSIGNMENT (( #168224 ) ) ;
#151983 = CARTESIAN_POINT ( 'NONE',  ( 1.424454163599726320, -1.462446849824734274, -1.388484543128357229 ) ) ;
#151984 = CARTESIAN_POINT ( 'NONE',  ( 7.596942422597253497, 13.84883568004298127, -8.824041907131851659 ) ) ;
#151985 = CARTESIAN_POINT ( 'NONE',  ( -6.692921386640485082, 10.96015871772258521, -0.7998128361456291469 ) ) ;
#151986 = CARTESIAN_POINT ( 'NONE',  ( 6.657217119509961201, 7.725507046638470321, -1.199719254218446718 ) ) ;
#151987 = CARTESIAN_POINT ( 'NONE',  ( 2.948016456289838771, -1.425740979638410399, -1.569777838261996017 ) ) ;
#151988 = CARTESIAN_POINT ( 'NONE',  ( -1.402160292154681736E-14, -0.6781249996585819728, 1.575800808251672791 ) ) ;
#151989 = CARTESIAN_POINT ( 'NONE',  ( 5.074738461036464088, -1.720261882950037124, -0.6118011564382742629 ) ) ;
#151990 = ORIENTED_EDGE ( 'NONE', *, *, #70772, .F. ) ;
#151991 = CARTESIAN_POINT ( 'NONE',  ( -5.610041701004606196, 9.767075427805856691, -0.7998128361456362523 ) ) ;
#151992 = FILL_AREA_STYLE ('',( #21943 ) ) ;
#151993 = CARTESIAN_POINT ( 'NONE',  ( 0.000000000000000000, -4.243749999044082344, -4.012584370867899430 ) ) ;
#151994 = VECTOR ( 'NONE', #116655, 1000.000000000000000 ) ;
#151995 = CARTESIAN_POINT ( 'NONE',  ( -6.742482464697739708, 6.760651051769146491, 0.7998128361456341429 ) ) ;
#151996 = CARTESIAN_POINT ( 'NONE',  ( 1.635027243301078848, 1.886126948880119780, 0.7230602950082564151 ) ) ;
#151997 = CARTESIAN_POINT ( 'NONE',  ( 6.827182134110222123, -0.006956174471953178659, 2.188967759425272330 ) ) ;
#151998 = ADVANCED_FACE ( 'NONE', ( #139853 ), #33597, .F. ) ;
#151999 = CARTESIAN_POINT ( 'NONE',  ( 8.191097360950562845, 12.70803068775103739, -0.7998128361456352531 ) ) ;
#152000 = CARTESIAN_POINT ( 'NONE',  ( 4.557361202124784683, 1.492679318236398878, 1.111055945242465093 ) ) ;
#152001 = CARTESIAN_POINT ( 'NONE',  ( 8.971744963941056028, 11.49012176272984931, 1.599625672291281386 ) ) ;
#152002 = ORIENTED_EDGE ( 'NONE', *, *, #159680, .T. ) ;
#152003 = CARTESIAN_POINT ( 'NONE',  ( -4.223528545856940042, 4.886203710709899006, -1.199719254218446718 ) ) ;
#152004 = CARTESIAN_POINT ( 'NONE',  ( -8.667740277838301921, 9.006785167099828016, -0.7998128361456291469 ) ) ;
#152005 = CARTESIAN_POINT ( 'NONE',  ( 5.408770660633122063, 1.379882519126625295, -1.195542987486551301 ) ) ;
#152007 = CARTESIAN_POINT ( 'NONE',  ( -4.023696502211203452, 7.783621949832661535, -0.4819376843918365960 ) ) ;
#152006 = CARTESIAN_POINT ( 'NONE',  ( -5.399890319992785237, 9.521898816625391504, 0.7998128361456291469 ) ) ;
#152008 = CARTESIAN_POINT ( 'NONE',  ( -1.602468905319636405E-14, -1.053124999658583638, -1.575800808251665908 ) ) ;
#152009 = CARTESIAN_POINT ( 'NONE',  ( 2.178627760304178818, -0.8125915806111455586, -1.531602080710131153 ) ) ;
#152010 = CARTESIAN_POINT ( 'NONE',  ( 0.6205767395346533100, -1.653899685646512019, 0.5418069113267124370 ) ) ;
#152011 = MECHANICAL_DESIGN_GEOMETRIC_PRESENTATION_REPRESENTATION (  '', ( #162368 ), #13610 ) ;
#152013 = CARTESIAN_POINT ( 'NONE',  ( 7.293923454472077239, 10.49303254931736262, 1.082531754730558626 ) ) ;
#152012 = CARTESIAN_POINT ( 'NONE',  ( 5.321043329010971767, 2.130378997510178785, 0.8875623774946446165 ) ) ;
#152014 = CARTESIAN_POINT ( 'NONE',  ( 5.401997860402196316, 5.267028690082820930, 0.000000000000000000 ) ) ;
#152015 = CARTESIAN_POINT ( 'NONE',  ( 1.528665837207894285, 1.985218273788964316, 0.5525772030575173410 ) ) ;
#152016 = ADVANCED_FACE ( 'NONE', ( #28210 ), #141032, .T. ) ;
#152017 = AXIS2_PLACEMENT_3D ( 'NONE', #48216, #164084, #211736 ) ;
#152018 = ADVANCED_FACE ( 'NONE', ( #43414 ), #94304, .T. ) ;
#152019 = CARTESIAN_POINT ( 'NONE',  ( 6.854781963242574605, -0.9897500569795645298, 2.071502949204959254 ) ) ;
#152020 = CARTESIAN_POINT ( 'NONE',  ( 7.465383582577691968, 15.41927370284943244, -9.344668898791677947 ) ) ;
#152021 = CARTESIAN_POINT ( 'NONE',  ( -6.934069218746458318, 7.054445274817795486, -0.7998128361456362523 ) ) ;
#152022 = CARTESIAN_POINT ( 'NONE',  ( 6.819227946136852125, -0.1326586024288610444, 1.840611662119538749 ) ) ;
#152024 = CARTESIAN_POINT ( 'NONE',  ( -6.699137298928187434, 8.909022496873262753, 1.443375672974064550 ) ) ;
#152023 = CARTESIAN_POINT ( 'NONE',  ( 3.304848191199673213, -0.3775801424153284458, -1.874573493127674961 ) ) ;
#152025 = CARTESIAN_POINT ( 'NONE',  ( 4.670673364294657404, -1.443042178620690841, 1.669811033208345341 ) ) ;
#152026 = CARTESIAN_POINT ( 'NONE',  ( -1.953008978358306879E-14, 2.125000000682797818, 1.414508159514571428 ) ) ;
#152027 = CARTESIAN_POINT ( 'NONE',  ( -6.685579144870156476, 9.853573864773576219, 1.082531754730549967 ) ) ;
#152028 = CARTESIAN_POINT ( 'NONE',  ( 4.380693030546913391, 7.164540064729805202, 1.082531754730549078 ) ) ;
#152029 = CARTESIAN_POINT ( 'NONE',  ( -3.648552735408985725, 7.270745601370182776, -0.7216878364870458196 ) ) ;
#152030 = CARTESIAN_POINT ( 'NONE',  ( 0.1881566102324930545, 1.164766123054150837, 1.649759867427439186 ) ) ;
#152031 = CARTESIAN_POINT ( 'NONE',  ( 3.944573596103123414, 2.296136059628416604, 0.2296890760785547936 ) ) ;
#152032 = CARTESIAN_POINT ( 'NONE',  ( 4.316819842036943911, -1.455217238560998272, 1.315978175897666080 ) ) ;
#152033 = CARTESIAN_POINT ( 'NONE',  ( 0.4089400952669055567, -1.579117232646386704, 1.163831224039679979 ) ) ;
#152034 = CARTESIAN_POINT ( 'NONE',  ( 7.777967379493318845, -5.907420853759296264, 7.664830294503448549 ) ) ;
#152035 = CARTESIAN_POINT ( 'NONE',  ( -9.434499673548478071, 15.42021604052381711, 7.415633384624290336 ) ) ;
#152036 = ORIENTED_EDGE ( 'NONE', *, *, #165074, .T. ) ;
#152037 = CARTESIAN_POINT ( 'NONE',  ( 6.298064597363540074, -0.9548514761729166578, -1.776169100128288658 ) ) ;
#152038 = CARTESIAN_POINT ( 'NONE',  ( -7.862839020921525091, 11.26073039346208660, -1.199719254218446718 ) ) ;
#152039 = CARTESIAN_POINT ( 'NONE',  ( -1.471045507628332367E-16, 1.899999999999999023, 2.650000000000008349 ) ) ;
#152040 = CARTESIAN_POINT ( 'NONE',  ( 3.063509990063197019, 1.831722579244631666, 1.165231348177008242 ) ) ;
#152041 = CARTESIAN_POINT ( 'NONE',  ( 0.3866926556112013635, 2.897682894409562060, 2.027578619373314073 ) ) ;
#152042 = CARTESIAN_POINT ( 'NONE',  ( 0.5453776912951785460, 0.1620316879334358084, 2.114494688702214020 ) ) ;
#152043 = CARTESIAN_POINT ( 'NONE',  ( -1.500000000000013101, 1.660416667349487119, -0.8660254037844313801 ) ) ;
#152044 = CARTESIAN_POINT ( 'NONE',  ( 10.05067194643221207, 10.62020544712608938, 0.7998128361456462443 ) ) ;
#152045 = CARTESIAN_POINT ( 'NONE',  ( 1.878856644857516578, 2.480000000000016858, 2.465765312203895387 ) ) ;
#152046 = CARTESIAN_POINT ( 'NONE',  ( 6.367678427751853221, 6.924687757192571347, 0.8275186136274095272 ) ) ;
#152047 = ORIENTED_EDGE ( 'NONE', *, *, #128773, .F. ) ;
#152048 = CARTESIAN_POINT ( 'NONE',  ( 1.686866501761717263, -0.2992900534812113489, -2.038785687196064789 ) ) ;
#152050 = CARTESIAN_POINT ( 'NONE',  ( 7.691668836200880044, 14.45522512263782389, -9.156333440833073212 ) ) ;
#152049 = CARTESIAN_POINT ( 'NONE',  ( -10.32861409551237486, 10.94447128771960287, 1.040834085586084257E-14 ) ) ;
#152051 = CARTESIAN_POINT ( 'NONE',  ( 1.364683531249990311, 2.634375000341422801, 1.214306433183764966E-14 ) ) ;
#152052 = CARTESIAN_POINT ( 'NONE',  ( -0.07933194154489606187, -9.746166700180788567, -9.499668754385620417 ) ) ;
#152053 = EDGE_LOOP ( 'NONE', ( #29083, #184173, #203606 ) ) ;
#152054 = CARTESIAN_POINT ( 'NONE',  ( 4.336511155197938727, 1.173803677898217712, -1.509565991254034678 ) ) ;
#152055 = COLOUR_RGB ( '', 0.72549020, 0.75294118, 0.79215686) ;
#152056 = FACE_OUTER_BOUND ( 'NONE', #80808, .T. ) ;
#152057 = CARTESIAN_POINT ( 'NONE',  ( -4.274898507010545856, 3.881803101134051470, -0.7998128361456221525 ) ) ;
#152058 = CARTESIAN_POINT ( 'NONE',  ( 1.177659378823514791, 1.784474613499857032, -0.3112490768260189333 ) ) ;
#152060 = CARTESIAN_POINT ( 'NONE',  ( 0.6728745832610707467, 1.688094080341449033, -0.9057684134900626516 ) ) ;
#152059 = CARTESIAN_POINT ( 'NONE',  ( -0.08896015503664694846, 7.049507384514476449, -3.948637857580539201 ) ) ;
#152061 = CARTESIAN_POINT ( 'NONE',  ( 2.471216696211364638, 1.848302923701108158, 0.9330170062570308787 ) ) ;
#152062 = CARTESIAN_POINT ( 'NONE',  ( -1.364683531250014514, -0.1989583329919157317, -0.7879004041258359514 ) ) ;
#152063 = CARTESIAN_POINT ( 'NONE',  ( 0.7957029915596275371, -0.7116629262611442464, 1.838703523458279143 ) ) ;
#152064 = CARTESIAN_POINT ( 'NONE',  ( 2.367563199519676420, 1.790531440309536926, -0.3556685536310541518 ) ) ;
#152066 = CARTESIAN_POINT ( 'NONE',  ( 5.931307043615195340, 7.129970210930432373, 1.110187140972586306 ) ) ;
#152065 = CARTESIAN_POINT ( 'NONE',  ( 0.2589922964784003301, 0.8893095213439340396, 2.129655304206728328 ) ) ;
#152067 = CARTESIAN_POINT ( 'NONE',  ( -0.6823417656250212460, 1.551041667008083769, 1.181850606188755259 ) ) ;
#152068 = CARTESIAN_POINT ( 'NONE',  ( 4.176276986610152342, -1.057847390704643509, -1.770619276543743625 ) ) ;
#152069 = CARTESIAN_POINT ( 'NONE',  ( -5.364222332501225488, 9.410009821226765325, 0.7998128361456481317 ) ) ;
#152070 = CARTESIAN_POINT ( 'NONE',  ( 8.762647353133951711, 9.117510088278095282, 1.040834085586084257E-14 ) ) ;
#152071 = CARTESIAN_POINT ( 'NONE',  ( 5.352771719296971042, 5.139321848801576387, 0.7998128361456341429 ) ) ;
#152072 = CARTESIAN_POINT ( 'NONE',  ( 6.114890974963323345, 7.092793211334054604, 1.199719254218462483 ) ) ;
#152074 = CARTESIAN_POINT ( 'NONE',  ( 1.499999999999987121, 3.795833333333356929, -0.8660254037844262731 ) ) ;
#152073 = CARTESIAN_POINT ( 'NONE',  ( 4.963951390035996170, 2.083465175373377498, -0.3060735771123861970 ) ) ;
#152075 = CARTESIAN_POINT ( 'NONE',  ( 6.303194806757332458, -1.751150776259063457, 1.104182018118210262 ) ) ;
#152076 = CARTESIAN_POINT ( 'NONE',  ( -1.402160292154681736E-14, 1.509375000341420359, -1.575800808251659024 ) ) ;
#152077 = CARTESIAN_POINT ( 'NONE',  ( 4.358765367649009903, -1.604958417591015207, 1.448176592534822005 ) ) ;
#152078 = CARTESIAN_POINT ( 'NONE',  ( 4.811197383834631580, 1.677940508811623710, -1.123774901704529317 ) ) ;
#152079 = CARTESIAN_POINT ( 'NONE',  ( 4.889022008684530185, 4.879516615612172536, -0.08706862575298174312 ) ) ;
#152080 = EDGE_CURVE ( 'NONE', #144861, #135108, #110919, .T. ) ;
#152083 = CARTESIAN_POINT ( 'NONE',  ( 4.514501963670558560, 8.210743357683563559, 1.040834085586084257E-14 ) ) ;
#152082 = CARTESIAN_POINT ( 'NONE',  ( -3.285556943749998737, -3.930208332855377407, 1.896917185911908499 ) ) ;
#152081 = DIRECTION ( 'NONE',  ( -0.7806247498001170904, 9.887923813067782263E-13, -0.6249999999996038724 ) ) ;
#152084 = CARTESIAN_POINT ( 'NONE',  ( -6.791708605802965870, 6.888357893050385705, -0.7998128361456362523 ) ) ;
#152085 = CARTESIAN_POINT ( 'NONE',  ( 2.395720570290179374, -1.993893129684479293, 0.3006499569925198956 ) ) ;
#152086 = CARTESIAN_POINT ( 'NONE',  ( -7.669108446824431269, 12.09904362127053545, -0.7998128361456291469 ) ) ;
#152088 = CARTESIAN_POINT ( 'NONE',  ( 6.620655732516651071, -0.002413161512292844035, 2.173887093218453082 ) ) ;
#152087 = CARTESIAN_POINT ( 'NONE',  ( -3.405069135326500351, 7.124331091189553433, 1.040834085586084257E-14 ) ) ;
#152089 = CARTESIAN_POINT ( 'NONE',  ( 1.364683531249997417, 8.484375000341396245, 2.602085213965210642E-15 ) ) ;
#152090 = CARTESIAN_POINT ( 'NONE',  ( 6.794158526849249924, -7.616254850791396969, 7.451274665340253733 ) ) ;
#152092 = CARTESIAN_POINT ( 'NONE',  ( 4.517203946846011675, -1.842441744247227842, 0.8197884948388589610 ) ) ;
#152091 = CARTESIAN_POINT ( 'NONE',  ( -8.039621902779392926, 9.442275643739831636, 1.082531754730558626 ) ) ;
#152093 = CARTESIAN_POINT ( 'NONE',  ( -1.500000000000011324, 5.670833333333358262, 0.8660254037844403729 ) ) ;
#152094 = CARTESIAN_POINT ( 'NONE',  ( 1.013767525470328001, -0.7718518339048777710, -1.542633921862639701 ) ) ;
#152095 = CARTESIAN_POINT ( 'NONE',  ( 4.688087255275310561, 8.691461907788344377, -0.7998128361456381397 ) ) ;
#152097 = LINE ( 'NONE', #3668, #122036 ) ;
#152096 = CARTESIAN_POINT ( 'NONE',  ( 6.778713617152772208, 10.85232362007950258, -0.7216878364870267237 ) ) ;
#152098 = PRESENTATION_LAYER_ASSIGNMENT (  '', '', ( #214343 ) ) ;
#152099 = CARTESIAN_POINT ( 'NONE',  ( -11.76226697576122504, 8.565577005366957763, 2.393665422351130001 ) ) ;
#152100 = CARTESIAN_POINT ( 'NONE',  ( 5.641831084104285132, 0.7588036158820666843, -1.709917670604633066 ) ) ;
#152101 = CARTESIAN_POINT ( 'NONE',  ( 6.398696026112846269, -1.975200287401058130, -0.3884956089365321774 ) ) ;
#152102 = FACE_OUTER_BOUND ( 'NONE', #82760, .T. ) ;
#152103 = CARTESIAN_POINT ( 'NONE',  ( -7.119440060507479018, 8.439006504414422238, 1.082531754730549078 ) ) ;
#152104 = ORIENTED_EDGE ( 'NONE', *, *, #183643, .T. ) ;
#152105 = CARTESIAN_POINT ( 'NONE',  ( 8.378575743120986630, 12.71882943370911789, 1.040834085586084257E-14 ) ) ;
#152106 = CARTESIAN_POINT ( 'NONE',  ( 0.7730648107450198703, 1.777001872080404166, -0.9530316558409924754 ) ) ;
#152107 = CARTESIAN_POINT ( 'NONE',  ( 1.160107992948592237, 1.809582681877516697, 0.08717244660690416647 ) ) ;
#152108 = CARTESIAN_POINT ( 'NONE',  ( 5.851225812749518695, 8.984124660586543243, -1.199719254218452047 ) ) ;
#152109 = CARTESIAN_POINT ( 'NONE',  ( 6.807524309086420367, -0.4794501827766698421, 2.115671360755105646 ) ) ;
#152110 = CARTESIAN_POINT ( 'NONE',  ( 7.036318535368067728, 10.19249347702934294, -1.082531754730537976 ) ) ;
#152111 = AXIS2_PLACEMENT_3D ( 'NONE', #8096, #171666, #174904 ) ;
#152112 = CARTESIAN_POINT ( 'NONE',  ( 5.777746017718023097, 9.892454120646377191, 0.7998128361456462443 ) ) ;
#152114 = CARTESIAN_POINT ( 'NONE',  ( 0.2158530320381162604, 0.9822752966809102926, -1.644539037099991718 ) ) ;
#152113 = CARTESIAN_POINT ( 'NONE',  ( -5.148345644887285744, 7.029489223833707001, -1.599625672291256295 ) ) ;
#152115 = FILL_AREA_STYLE_COLOUR ( '', #35131 ) ;
#152116 = LINE ( 'NONE', #201889, #49024 ) ;
#152117 = CARTESIAN_POINT ( 'NONE',  ( 1.364683531249986537, -1.073958332991911790, 0.7879004041258500513 ) ) ;
#152119 = VERTEX_POINT ( 'NONE', #196052 ) ;
#152118 = CARTESIAN_POINT ( 'NONE',  ( 4.717874267875568961, 4.606534188717351874, -0.7216878364870188411 ) ) ;
#152120 = CARTESIAN_POINT ( 'NONE',  ( -3.810004860640155311, 4.403759411290286252, 1.199719254218462483 ) ) ;
#152121 = EDGE_CURVE ( 'NONE', #46131, #152273, #185952, .T. ) ;
#152122 = CARTESIAN_POINT ( 'NONE',  ( 4.469695567000064429, 2.097540297429688838, -0.5223010940857697459 ) ) ;
#152123 = CARTESIAN_POINT ( 'NONE',  ( -6.292392690518209264, 8.434487120394948079, -1.443375672974066548 ) ) ;
#152124 = CARTESIAN_POINT ( 'NONE',  ( 6.427974226654860956, 7.632296364919712417, -1.082531754730548412 ) ) ;
#152125 = CARTESIAN_POINT ( 'NONE',  ( 0.5102161431939798986, -0.7575819503438313562, 1.980855387931411915 ) ) ;
#152126 = EDGE_CURVE ( 'NONE', #121694, #78339, #98540, .T. ) ;
#152127 = CARTESIAN_POINT ( 'NONE',  ( 6.721730220878607831, -1.769880579078547012, 0.4471725050417332814 ) ) ;
#152128 = CARTESIAN_POINT ( 'NONE',  ( 2.425019040235734558, -0.003784258722050458899, 1.971530340264670889 ) ) ;
#152129 = CARTESIAN_POINT ( 'NONE',  ( 4.693567934957057375, 1.782326746607498791, -0.6936623114904352239 ) ) ;
#152130 = ORIENTED_EDGE ( 'NONE', *, *, #115682, .T. ) ;
#152132 = ADVANCED_FACE ( 'NONE', ( #113795 ), #162491, .T. ) ;
#152131 = CARTESIAN_POINT ( 'NONE',  ( 9.612297698795886802, -6.674536912880676631, -0.2039282260587966522 ) ) ;
#152133 = CARTESIAN_POINT ( 'NONE',  ( 6.162556002056702731, -0.7074686763054702787, -1.838295890583282022 ) ) ;
#152134 = CARTESIAN_POINT ( 'NONE',  ( 0.1287130127310652239, -1.775900012335431155, 0.7861216482863192523 ) ) ;
#152135 = ORIENTED_EDGE ( 'NONE', *, *, #210187, .T. ) ;
#152136 = CARTESIAN_POINT ( 'NONE',  ( -4.146814880933400005, 5.931313009212638931, 1.599625672291270506 ) ) ;
#152137 = CARTESIAN_POINT ( 'NONE',  ( -3.122120512896910505, 6.864500708346841229, 0.7998128361456352531 ) ) ;
#152139 = CARTESIAN_POINT ( 'NONE',  ( 6.997416677984476863, 7.336276677169590421, 0.000000000000000000 ) ) ;
#152138 = CARTESIAN_POINT ( 'NONE',  ( 8.132193210098487057, 8.381980254736715708, 1.040834085586084257E-14 ) ) ;
#152141 = ORIENTED_EDGE ( 'NONE', *, *, #155670, .T. ) ;
#152140 = CARTESIAN_POINT ( 'NONE',  ( 5.127564033545165323, -0.2766344828325461580, 1.892035409188079997 ) ) ;
#152142 = CARTESIAN_POINT ( 'NONE',  ( 3.545738602337618506, -1.670889076328873291, -1.441789439710974285 ) ) ;
#152143 = CARTESIAN_POINT ( 'NONE',  ( 2.503190323335769740, 1.772782541628318720, -1.313999973512294694 ) ) ;
#152144 = CARTESIAN_POINT ( 'NONE',  ( 0.000000000000000000, -4.500000000000003553, 2.000000000000000000 ) ) ;
#152145 = CARTESIAN_POINT ( 'NONE',  ( 0.7328884408557728714, 1.767063509844998492, 0.7314339715377634610 ) ) ;
#152146 = CARTESIAN_POINT ( 'NONE',  ( -0.02338929933905826986, 0.006294950389555685130, -1.710968156697996401 ) ) ;
#152147 = CARTESIAN_POINT ( 'NONE',  ( -6.004825442174102967, 7.178221627660431814, 1.212153120240029969 ) ) ;
#152148 = CARTESIAN_POINT ( 'NONE',  ( 2.875506610227479332, -0.2054619808779626633, 2.060159609288146232 ) ) ;
#152149 = CARTESIAN_POINT ( 'NONE',  ( -4.412288926243578935, 7.235088616337731260, 1.199719254218464037 ) ) ;
#152150 = CARTESIAN_POINT ( 'NONE',  ( -4.712247760717829692, 8.249883430950177399, 0.6303846594760522670 ) ) ;
#152152 = CARTESIAN_POINT ( 'NONE',  ( 0.8312129145573650124, 0.1600495679085281175, 2.155820468135719814 ) ) ;
#152151 = CARTESIAN_POINT ( 'NONE',  ( -3.795392936821753604, 6.515376628678959392, -1.199719254218452047 ) ) ;
#152153 = CARTESIAN_POINT ( 'NONE',  ( 2.982162443640325566, -2.159563097825706990, -0.3721831821169723775 ) ) ;
#152154 = CARTESIAN_POINT ( 'NONE',  ( -0.6125000000000331291, 0.7916666666666558605, 1.060881119635891157 ) ) ;
#152155 = CARTESIAN_POINT ( 'NONE',  ( 3.119784744920330422, 6.653849612466795627, 0.7216878364870257245 ) ) ;
#152156 = CARTESIAN_POINT ( 'NONE',  ( 1.499999999999822586, 7.240846818246208905, 4.154462424328221104 ) ) ;
#152157 = AXIS2_PLACEMENT_3D ( 'NONE', #113589, #131940, #21049 ) ;
#152158 = CARTESIAN_POINT ( 'NONE',  ( -8.012344526598182026E-15, 13.35937500034140157, -1.575800808251669460 ) ) ;
#152159 = CARTESIAN_POINT ( 'NONE',  ( -4.633854640820660009, 8.628190524257904670, -0.7998128361456362523 ) ) ;
#152160 = CARTESIAN_POINT ( 'NONE',  ( 5.906827578720975858, -0.9711093913858243054, -1.436504219383877290 ) ) ;
#152161 = EDGE_CURVE ( 'NONE', #12895, #106915, #82453, .T. ) ;
#152162 = CARTESIAN_POINT ( 'NONE',  ( -4.939248034080176097, 4.656877549381960080, 1.214306433183764966E-14 ) ) ;
#152163 = CARTESIAN_POINT ( 'NONE',  ( 3.274343992483694787, -1.016290647400164282, -1.803532422793553636 ) ) ;
#152164 = CARTESIAN_POINT ( 'NONE',  ( 4.798512230019831293, 1.459014486584905956, -1.534486623482501644 ) ) ;
#152165 = CARTESIAN_POINT ( 'NONE',  ( 6.287230548435207567, 8.358188277972981695, -1.599625672291262513 ) ) ;
#152166 = CARTESIAN_POINT ( 'NONE',  ( -1.201851678989727383E-14, 4.946875000341420581, -1.575800808251660134 ) ) ;
#152167 = CARTESIAN_POINT ( 'NONE',  ( 3.274220328336883146, -0.9665011448860871823, -1.715865690870149285 ) ) ;
#152168 = CARTESIAN_POINT ( 'NONE',  ( 0.8438408207818194340, -1.215224102361469161, -1.476598726422105656 ) ) ;
#152169 = CARTESIAN_POINT ( 'NONE',  ( 4.910265066218413743, 1.583196867009181608, -1.657922308084827545 ) ) ;
#152170 = CARTESIAN_POINT ( 'NONE',  ( 3.492628380820804956, -0.3572889717703279788, -1.790209119249221770 ) ) ;
#152171 = CARTESIAN_POINT ( 'NONE',  ( 4.041212305325117882, 6.872442235258051646, -1.199719254218448494 ) ) ;
#152172 = CARTESIAN_POINT ( 'NONE',  ( 4.799223189113185128, 8.542918120699967588, 1.040834085586084257E-14 ) ) ;
#152173 = CARTESIAN_POINT ( 'NONE',  ( -7.043624497499477499, 8.176315654292865887, 1.199719254218450271 ) ) ;
#152174 = CARTESIAN_POINT ( 'NONE',  ( 4.517842040498582179, -0.5326873650394120530, 1.941415848259191446 ) ) ;
#152175 = CARTESIAN_POINT ( 'NONE',  ( 2.852341167582587378, -1.956174252073937359, -0.1491622203949396763 ) ) ;
#152176 = CARTESIAN_POINT ( 'NONE',  ( -7.857113714319432063, 9.125386407249497012, 1.199719254218462483 ) ) ;
#152177 = CARTESIAN_POINT ( 'NONE',  ( -4.225337428953291230, 8.081310767087481750, 0.7998128361456341429 ) ) ;
#152178 = CARTESIAN_POINT ( 'NONE',  ( 0.1751657365761521701, 1.361037063587458906, -2.300812366989886559 ) ) ;
#152180 = CARTESIAN_POINT ( 'NONE',  ( 5.489024251479373895, 1.559478583775832261, -0.8368352093669585434 ) ) ;
#152179 = CARTESIAN_POINT ( 'NONE',  ( 6.351524237630270520, 2.085149843271947301, -0.1523318108044656727 ) ) ;
#152181 = CARTESIAN_POINT ( 'NONE',  ( 11.00029519899100627, -5.907420853759282942, 5.448115916739660570E-15 ) ) ;
#152182 = CARTESIAN_POINT ( 'NONE',  ( 1.957222284144799929, 0.3726435881295561692, -2.159377063894574622 ) ) ;
#152183 = CARTESIAN_POINT ( 'NONE',  ( 6.175711810462381379, -0.9247362235058408375, 1.474125693279482174 ) ) ;
#152184 = CARTESIAN_POINT ( 'NONE',  ( 7.558834334818744338, 8.777393797832065303, 1.199719254218462483 ) ) ;
#152185 = CARTESIAN_POINT ( 'NONE',  ( 0.2335667940002502385, 6.947499997881678269, -2.748442024765639147 ) ) ;
#152186 = CARTESIAN_POINT ( 'NONE',  ( 0.3106396986791125081, 1.498014557929911117, 0.8549171915634717900 ) ) ;
#152187 = CARTESIAN_POINT ( 'NONE',  ( 1.177631936369994303, -1.035077938576201451, -2.052156377449709357 ) ) ;
#152188 = CARTESIAN_POINT ( 'NONE',  ( 0.6971427418834205136, 1.794861059153027627, 1.257291590721874686 ) ) ;
#152189 = CARTESIAN_POINT ( 'NONE',  ( 2.912931060594741162, 1.598032330669514778, -1.522282275181946032 ) ) ;
#152190 = CARTESIAN_POINT ( 'NONE',  ( 6.491432910188612126, -0.4373703761123280964, 1.975813455233149218 ) ) ;
#152191 =( GEOMETRIC_REPRESENTATION_CONTEXT ( 3 ) GLOBAL_UNCERTAINTY_ASSIGNED_CONTEXT ( ( #65544 ) ) GLOBAL_UNIT_ASSIGNED_CONTEXT ( ( #116330, #345, #50211 ) ) REPRESENTATION_CONTEXT ( 'NONE', 'WORKASPACE' ) );
#152192 = CARTESIAN_POINT ( 'NONE',  ( 0.4621001773846104554, -0.5802113591629636247, 2.092003544004197302 ) ) ;
#152193 = FACE_OUTER_BOUND ( 'NONE', #122113, .T. ) ;
#152194 = ADVANCED_FACE ( 'NONE', ( #68440 ), #114097, .T. ) ;
#152195 = CARTESIAN_POINT ( 'NONE',  ( 0.6556431738361043760, 2.038855430691276727, -0.5708433468438726122 ) ) ;
#152196 = FACE_OUTER_BOUND ( 'NONE', #141514, .T. ) ;
#152197 = CARTESIAN_POINT ( 'NONE',  ( 5.666998703487860389, -1.741597003894586937, -0.8236021136211798543 ) ) ;
#152198 = ORIENTED_EDGE ( 'NONE', *, *, #172187, .T. ) ;
#152200 = CARTESIAN_POINT ( 'NONE',  ( -0.7500000000000215383, 5.691666666666685082, 1.299038105676671107 ) ) ;
#152199 = CARTESIAN_POINT ( 'NONE',  ( 1.136728594277321980, 0.4534141614637792195, 2.246936901365268913 ) ) ;
#152201 = CARTESIAN_POINT ( 'NONE',  ( 4.196412238629597447, 4.854568018944682706, -1.199719254218452047 ) ) ;
#152202 = CARTESIAN_POINT ( 'NONE',  ( 7.006866460164219212, 7.069099046480051385, -0.7998128361456281477 ) ) ;
#152203 = CARTESIAN_POINT ( 'NONE',  ( 4.108218931252209494, -0.8498058027226679245, 2.052504409502105442 ) ) ;
#152204 = CARTESIAN_POINT ( 'NONE',  ( -8.242994207428740339, 9.679543332497402730, 1.082531754730558626 ) ) ;
#152205 = CARTESIAN_POINT ( 'NONE',  ( 5.341549334104184865, 8.215262742221458581, 1.082531754730558626 ) ) ;
#152206 = CARTESIAN_POINT ( 'NONE',  ( -7.822691444960709006, 10.14955932391940330, -1.443375672974058777 ) ) ;
#152207 = CARTESIAN_POINT ( 'NONE',  ( 4.231553341240963384, 7.950912974840849579, -0.7216878364870357165 ) ) ;
#152208 = CARTESIAN_POINT ( 'NONE',  ( 1.600232647554021392, -0.2440283035436350279, 2.001511509883910911 ) ) ;
#152210 = CARTESIAN_POINT ( 'NONE',  ( 1.182570505923411952, 1.231668817017372408, -1.654277799056037335 ) ) ;
#152209 = CARTESIAN_POINT ( 'NONE',  ( 8.372323551638698902, 9.726464550788689323, 1.199719254218462483 ) ) ;
#152211 = CARTESIAN_POINT ( 'NONE',  ( 4.831500990369687720, 4.877271539032528302, 0.3436843597541731632 ) ) ;
#152212 = CARTESIAN_POINT ( 'NONE',  ( 6.333067150914820864, 6.561202228921677815, 0.7216878364870328300 ) ) ;
#152213 = CARTESIAN_POINT ( 'NONE',  ( -0.1237769027084348328, -0.1346504581853508187, -1.811164470923332104 ) ) ;
#152214 = CARTESIAN_POINT ( 'NONE',  ( 10.91970695577495043, -5.907420853759282053, 8.673617379884035472E-15 ) ) ;
#152215 = CARTESIAN_POINT ( 'NONE',  ( -1.364683531250012516, 2.780208333674754506, 0.7879004041258379498 ) ) ;
#152216 = CARTESIAN_POINT ( 'NONE',  ( 2.459888865612788855, 0.7521488021439284299, 1.602074255657309099 ) ) ;
#152217 = CARTESIAN_POINT ( 'NONE',  ( 1.635388916632842360, 0.6352005984417673501, 1.913803229121699534 ) ) ;
#152218 = CARTESIAN_POINT ( 'NONE',  ( -0.1121326479804653220, -0.4008509640632436088, -1.803546454093779561 ) ) ;
#152219 = CARTESIAN_POINT ( 'NONE',  ( 5.144168085839278426, 0.6632553684719083575, 2.194301386939989218 ) ) ;
#152220 = CARTESIAN_POINT ( 'NONE',  ( 3.240019139272034110, 0.4481936114588759845, 1.785621944311803100 ) ) ;
#152221 = CARTESIAN_POINT ( 'NONE',  ( 7.086107841436786181, 11.41887624831828418, 1.040834085586084257E-14 ) ) ;
#152222 = CARTESIAN_POINT ( 'NONE',  ( 4.383705365265609721, 1.192707349210776036, 1.382196219385352309 ) ) ;
#152223 = CARTESIAN_POINT ( 'NONE',  ( 4.693982515131527755, 1.755768268644173791, 0.9914009648221073778 ) ) ;
#152224 = CARTESIAN_POINT ( 'NONE',  ( -9.338868881714763148, 9.789768538289042255, -0.7998128361456291469 ) ) ;
#152226 = CARTESIAN_POINT ( 'NONE',  ( -6.257970421159510188, 9.458660037064859694, 1.199719254218452047 ) ) ;
#152225 = CARTESIAN_POINT ( 'NONE',  ( 3.608526635699527141, -0.9147260449715814978, -2.069530211360113725 ) ) ;
#152227 = CARTESIAN_POINT ( 'NONE',  ( 6.335009839202000670, 0.2025031609870796001, 2.096191850513532184 ) ) ;
#152228 = CARTESIAN_POINT ( 'NONE',  ( -7.075376061485238566, 9.347967719856493218, 1.599625672291269396 ) ) ;
#152229 = CARTESIAN_POINT ( 'NONE',  ( 4.088381982606685838, 1.110138344689771239, -1.747393465062855533 ) ) ;
#152230 = CARTESIAN_POINT ( 'NONE',  ( 4.715538499454675403, 4.395883092318884522, 1.214306433183764966E-14 ) ) ;
#152231 = CARTESIAN_POINT ( 'NONE',  ( 0.6801582343749952297, 2.255208333674735499, 1.178068619123839866 ) ) ;
#152232 = APPLICATION_PROTOCOL_DEFINITION ( 'draft international standard', 'automotive_design', 1998, #11751 ) ;
#152234 = CARTESIAN_POINT ( 'NONE',  ( 2.473164231231731680, 0.09456843629558449316, -1.924295592635028029 ) ) ;
#152233 = CARTESIAN_POINT ( 'NONE',  ( -8.805130697071332335, 12.36007068230351358, 1.199719254218462483 ) ) ;
#152235 = FACE_OUTER_BOUND ( 'NONE', #4739, .T. ) ;
#152236 = CARTESIAN_POINT ( 'NONE',  ( 6.983263157960363010, -0.003310164959547181717, 1.953544951557646403 ) ) ;
#152237 = CARTESIAN_POINT ( 'NONE',  ( 4.706088717274895750, 6.583799151611112954, 1.443375672974065660 ) ) ;
#152238 = CARTESIAN_POINT ( 'NONE',  ( 5.846986258851572416, 6.004518191619921730, 0.3586427151269864222 ) ) ;
#152239 = CARTESIAN_POINT ( 'NONE',  ( -11.84668730067608600, 12.69999999999998153, 1.319999999999998286 ) ) ;
#152240 = CARTESIAN_POINT ( 'NONE',  ( -2.656508033273816238, 5.186677574539687363, -1.199719254218446718 ) ) ;
#152241 = CARTESIAN_POINT ( 'NONE',  ( 0.5104038411899833871, -0.7921320118633947693, 2.075572886547627505 ) ) ;
#152242 = CARTESIAN_POINT ( 'NONE',  ( 3.504997884693922483, 1.661208405451128245, -1.294291292614203170 ) ) ;
#152243 = CARTESIAN_POINT ( 'NONE',  ( -7.584860592202423035, 7.813701877183096833, -0.7998128361456362523 ) ) ;
#152244 = CARTESIAN_POINT ( 'NONE',  ( 7.962716289927667113, 8.184257181204083409, -0.7998128361456291469 ) ) ;
#152245 = CARTESIAN_POINT ( 'NONE',  ( 0.2911520677349140884, -1.704046917483082346, 0.7485983125269514149 ) ) ;
#152246 = CARTESIAN_POINT ( 'NONE',  ( 5.276094334012385367, 9.307193822989793475, 1.040834085586084257E-14 ) ) ;
#152247 = CARTESIAN_POINT ( 'NONE',  ( 3.649115900372475796, 7.409052317076538330, 1.040834085586084257E-14 ) ) ;
#152248 = CARTESIAN_POINT ( 'NONE',  ( -6.834718835064852449, 8.106831741398025315, 1.082531754730549078 ) ) ;
#152249 = CARTESIAN_POINT ( 'NONE',  ( -8.026063749610056419, 10.38682701267698150, -1.443375672974059665 ) ) ;
#152250 = CARTESIAN_POINT ( 'NONE',  ( 1.424255164902767934, -2.103954720533041556, 0.2648648325892372646 ) ) ;
#152251 = CARTESIAN_POINT ( 'NONE',  ( -6.129167961829681488, 9.308390501180058507, -1.199719254218452047 ) ) ;
#152253 = CARTESIAN_POINT ( 'NONE',  ( 4.246505328441081417, -1.940195102956907336, -0.2900488188990399396 ) ) ;
#152252 = CARTESIAN_POINT ( 'NONE',  ( -1.225000000000042277, 0.2291666666666811181, -0.7072540797573237947 ) ) ;
#152254 = CARTESIAN_POINT ( 'NONE',  ( 2.852577672069932735, 0.7271573612388192442, 2.035869728763760378 ) ) ;
#152255 = CARTESIAN_POINT ( 'NONE',  ( 1.417261839328866513, -1.023339270300478221, -1.530466495063505628 ) ) ;
#152256 = CARTESIAN_POINT ( 'NONE',  ( -4.059747316280317264, 7.561585642977368238, -0.4325785229164439416 ) ) ;
#152257 = CARTESIAN_POINT ( 'NONE',  ( 4.171615353782907931, -0.9995084519054014960, 1.424469360818179986 ) ) ;
#152258 = CARTESIAN_POINT ( 'NONE',  ( -1.724555757181114535, 13.99999999999846167, -11.68000002332616205 ) ) ;
#152259 = CARTESIAN_POINT ( 'NONE',  ( 5.178851490740196795, 7.065079377328788546, 1.443375672974062551 ) ) ;
#152260 = CARTESIAN_POINT ( 'NONE',  ( -9.979823206198361163, 5.589814398814587193, -5.978750339097102184 ) ) ;
#152261 = ADVANCED_FACE ( 'NONE', ( #148657 ), #99696, .T. ) ;
#152262 = CARTESIAN_POINT ( 'NONE',  ( 1.481558191429487970, 1.997200094811113491, -0.8276061316847342919 ) ) ;
#152263 = CIRCLE ( 'NONE', #96941, 0.08000000000000020983 ) ;
#152264 = CARTESIAN_POINT ( 'NONE',  ( 2.847029653296664353, -1.038834691150035461, 1.727737368502464621 ) ) ;
#152265 = CARTESIAN_POINT ( 'NONE',  ( -8.446366511189330240, 12.79791866312216442, 0.7216878364870317197 ) ) ;
#152266 = CARTESIAN_POINT ( 'NONE',  ( 1.182749364907993206, -2.109161078630458430, -0.4729781282231394490 ) ) ;
#152267 =( BOUNDED_SURFACE ( )  B_SPLINE_SURFACE ( 3, 2, ( 
 ( #143979, #107234, #73592 ),
 ( #175381, #176437, #174324 ),
 ( #205716, #192659, #76784 ),
 ( #209970, #11782, #24836 ) ),
 .UNSPECIFIED., .F., .F., .T. ) 
 B_SPLINE_SURFACE_WITH_KNOTS ( ( 4, 4 ),
 ( 3, 3 ),
 ( 0.005241070803109276581, 0.008267458746840841005 ),
 ( 0.000000000000000000, 1.000000000000000000 ),
 .UNSPECIFIED. ) 
 GEOMETRIC_REPRESENTATION_ITEM ( )  RATIONAL_B_SPLINE_SURFACE ( (
 ( 1.000000000000000000, 0.7184380228464076756, 1.000000000000000000),
 ( 1.000000000000000000, 0.7185467277397525887, 1.000000000000000000),
 ( 1.000000000000000000, 0.7186585579881041852, 1.000000000000000000),
 ( 1.000000000000000000, 0.7187737999613678097, 1.000000000000000000) ) ) 
 REPRESENTATION_ITEM ( '' )  SURFACE ( )  );
#152268 = CARTESIAN_POINT ( 'NONE',  ( 3.766447953776773883, -1.324889289065459774, 1.460063511008972137 ) ) ;
#152269 = CARTESIAN_POINT ( 'NONE',  ( 6.609000000000038177, 2.443064466336189788, 2.382833824652215160 ) ) ;
#152270 = CARTESIAN_POINT ( 'NONE',  ( 2.911592935152186090, -0.9596169164145462727, -1.688359700174842271 ) ) ;
#152273 = VERTEX_POINT ( 'NONE', #117275 ) ;
#152272 = CARTESIAN_POINT ( 'NONE',  ( -5.017926250833627755, 5.026871178826882947, 0.7216878364870257245 ) ) ;
#152271 =( NAMED_UNIT ( * ) PLANE_ANGLE_UNIT ( ) SI_UNIT ( $, .RADIAN. ) );
#152274 = CARTESIAN_POINT ( 'NONE',  ( -3.458738584817664385, 7.049295759013638474, 0.7216878364870338292 ) ) ;
#152275 = CARTESIAN_POINT ( 'NONE',  ( 4.655245641445829641, 6.524482229810530498, 1.599625672291269396 ) ) ;
#152276 = CARTESIAN_POINT ( 'NONE',  ( -4.132202957115018727, 8.042930226601317401, 0.000000000000000000 ) ) ;
#152277 = CARTESIAN_POINT ( 'NONE',  ( -5.271087860662956537, 9.371629280740593870, 0.000000000000000000 ) ) ;
#152278 = CARTESIAN_POINT ( 'NONE',  ( -9.829298179783291900, 11.53023130024440768, 1.082531754730558626 ) ) ;
#152279 = CARTESIAN_POINT ( 'NONE',  ( 6.651428954171766605, -1.847749378774863560, -1.382155756676258784 ) ) ;
#152280 = CARTESIAN_POINT ( 'NONE',  ( 3.285556943750000070, -3.434374999522042060, 0.000000000000000000 ) ) ;
#152281 = EDGE_CURVE ( 'NONE', #61789, #90767, #146550, .T. ) ;
#152282 = CARTESIAN_POINT ( 'NONE',  ( 3.766413727395605093, -0.7909564911158167844, -1.795405819223389488 ) ) ;
#152283 = CARTESIAN_POINT ( 'NONE',  ( 6.771407655021410399, 9.987393799911945536, -1.199719254218441611 ) ) ;
#152284 = CARTESIAN_POINT ( 'NONE',  ( 1.213517774399593740, 1.944071949784083264, 0.5350861613380719639 ) ) ;
#152285 = CARTESIAN_POINT ( 'NONE',  ( 3.837202554855035697, -1.762604653963547818, -1.172905022591600233 ) ) ;
#152286 = CARTESIAN_POINT ( 'NONE',  ( -0.7500000000000215383, 2.222916667349486453, 1.299038105676671107 ) ) ;
#152288 = CARTESIAN_POINT ( 'NONE',  ( -5.880485940025243607, 7.883652901494672349, 1.599625672291269396 ) ) ;
#152287 = SURFACE_STYLE_FILL_AREA ( #21181 ) ;
#152289 = CARTESIAN_POINT ( 'NONE',  ( 2.589598559577494186, -1.836209955096680613, -0.1354230481333124070 ) ) ;
#152290 = ORIENTED_EDGE ( 'NONE', *, *, #82484, .F. ) ;
#152291 = CARTESIAN_POINT ( 'NONE',  ( -9.345647958521597687, 9.797677461230342999, 0.7998128361456462443 ) ) ;
#152292 = CARTESIAN_POINT ( 'NONE',  ( 3.633072077242065861E-15, -6.802539632833518519E-15, -0.2598076211376265099 ) ) ;
#152293 = CARTESIAN_POINT ( 'NONE',  ( 3.832379111121624327, -1.093062754469842579, -1.817066923117337751 ) ) ;
#152294 = CARTESIAN_POINT ( 'NONE',  ( 1.499999999999991118, 5.535416667349481123, 0.8660254037844524744 ) ) ;
#152295 = B_SPLINE_CURVE_WITH_KNOTS ( 'NONE', 3,
 ( #36986, #172337, #101996, #68403, #35920, #169124, #201598 ),
 .UNSPECIFIED., .F., .F.,
 ( 4, 3, 4 ),
 ( 0.001837494195021916864, 0.002395020826491697005, 0.002588355962777582134 ),
 .UNSPECIFIED. ) ;
#152296 = CARTESIAN_POINT ( 'NONE',  ( 6.775324078527185989, 8.927630729746953264, -1.599625672291262513 ) ) ;
#152297 = CARTESIAN_POINT ( 'NONE',  ( 5.887979924156289790, -0.9304241717780140641, 1.838884224927712419 ) ) ;
#152299 = CARTESIAN_POINT ( 'NONE',  ( 2.401689157922583640, -0.7064633820979376866, -1.700523668893457296 ) ) ;
#152298 = CARTESIAN_POINT ( 'NONE',  ( -8.064402442030170093, 8.302891025323665630, 0.7998128361456602331 ) ) ;
#152300 = CARTESIAN_POINT ( 'NONE',  ( 9.759171643738394408, 10.28012176064996197, 0.000000000000000000 ) ) ;
#152301 = CARTESIAN_POINT ( 'NONE',  ( -1.201851678989727383E-14, 5.696875000341416140, -1.575800808251660134 ) ) ;
#152302 = SURFACE_STYLE_FILL_AREA ( #20144 ) ;
#152303 = CARTESIAN_POINT ( 'NONE',  ( 7.204675194429079505E-15, -1.443749999044083854, -3.475000000000000089 ) ) ;
#152304 = CARTESIAN_POINT ( 'NONE',  ( 2.086817400036289794, -2.164668306305051804, -0.4287355390964405211 ) ) ;
#152305 = CARTESIAN_POINT ( 'NONE',  ( 3.690934243623856581, -0.4369955660583099699, -2.219648300357620396 ) ) ;
#152306 = CARTESIAN_POINT ( 'NONE',  ( -8.351459436338048548, 8.845716885256940998, -0.7216878364870278340 ) ) ;
#152307 = CARTESIAN_POINT ( 'NONE',  ( 4.306777863985831623, -0.4033372078124509708, -1.765930869088320865 ) ) ;
#152308 = CARTESIAN_POINT ( 'NONE',  ( 4.223789564141206654, 0.8136391335250325874, -1.734469729061314913 ) ) ;
#152309 = CARTESIAN_POINT ( 'NONE',  ( -0.6823417656249969321, 4.530208333674755394, -1.181850606188749264 ) ) ;
#152310 = AXIS2_PLACEMENT_3D ( 'NONE', #161769, #10154, #160688 ) ;
#152311 = CARTESIAN_POINT ( 'NONE',  ( 3.397303563958519401, 1.553371746707431500, 1.213851982216722636 ) ) ;
#152312 = CARTESIAN_POINT ( 'NONE',  ( 5.260568668178753349, -1.354309965608934352, 1.290672426560689035 ) ) ;
#152313 = CARTESIAN_POINT ( 'NONE',  ( 4.879284944527097601, -0.09183316818502919310, 1.858928597182760711 ) ) ;
#152314 = CARTESIAN_POINT ( 'NONE',  ( -1.201851678989727383E-14, 5.696875000341416140, -1.575800808251660134 ) ) ;
#152315 = CARTESIAN_POINT ( 'NONE',  ( 0.4445464637146989695, -1.457232572767804379, 1.394089106691732693 ) ) ;
#152317 = CARTESIAN_POINT ( 'NONE',  ( 2.069099208297279002, -1.926018337604347597, -0.8524663740339888385 ) ) ;
#152316 = CARTESIAN_POINT ( 'NONE',  ( -4.758548728272219641, 4.653987725846768342, 0.7216878364870317197 ) ) ;
#152318 = CARTESIAN_POINT ( 'NONE',  ( 8.452618703115982512, 11.94880668935564216, 1.199719254218450271 ) ) ;
#152320 = CARTESIAN_POINT ( 'NONE',  ( -9.642873567817536795, 12.27310513391906532, 1.599625672291281386 ) ) ;
#152319 = CARTESIAN_POINT ( 'NONE',  ( -1.364683531249997417, 4.821875000341417916, 1.214306433183764966E-14 ) ) ;
#152321 = CARTESIAN_POINT ( 'NONE',  ( 2.830460552442021438, -1.048868820301660953, -1.842999677239331113 ) ) ;
#152322 = FACE_BOUND ( 'NONE', #20709, .T. ) ;
#152323 = CARTESIAN_POINT ( 'NONE',  ( 1.107682413490064022, 1.532168600112630230, 1.316196929287305473 ) ) ;
#152324 = CARTESIAN_POINT ( 'NONE',  ( -1.364683531250012516, 2.238541667008087988, -0.7879004041258289570 ) ) ;
#152325 = CARTESIAN_POINT ( 'NONE',  ( -2.982430605326328532, 5.462957558647244305, -1.082531754730543971 ) ) ;
#152326 = CARTESIAN_POINT ( 'NONE',  ( 4.847203612085560387, 5.613824621309978724, -1.199719254218452047 ) ) ;
#152327 = ORIENTED_EDGE ( 'NONE', *, *, #175342, .F. ) ;
#152328 = CARTESIAN_POINT ( 'NONE',  ( 2.302237272444170202, -2.161155982280529297, 0.05054500047013688047 ) ) ;
#152329 = CARTESIAN_POINT ( 'NONE',  ( 5.680503174445848735, 5.729601246382692636, 1.040834085586084257E-14 ) ) ;
#152330 = ADVANCED_FACE ( 'NONE', ( #50088 ), #182198, .F. ) ;
#152333 = CARTESIAN_POINT ( 'NONE',  ( -3.930720324626924000, 8.992102070998189589, -0.7749999999999979128 ) ) ;
#152332 = CARTESIAN_POINT ( 'NONE',  ( -3.642672431166898317, 3.097590952613070492, -2.447572309174330218 ) ) ;
#152331 = CARTESIAN_POINT ( 'NONE',  ( 5.747730777550676073, 5.670383760089384495, 0.000000000000000000 ) ) ;
#152334 = CARTESIAN_POINT ( 'NONE',  ( 4.000000000000012434, 6.499999999999999112, -0.7500000000000006661 ) ) ;
#152335 = CARTESIAN_POINT ( 'NONE',  ( 0.000000000000000000, 2.800000000000024691, 1.214306433183764966E-14 ) ) ;
#152336 = CARTESIAN_POINT ( 'NONE',  ( -9.178506806771670412, 9.810605484096178941, 1.040834085586084257E-14 ) ) ;
#152337 = CARTESIAN_POINT ( 'NONE',  ( 6.567919234911265391, -1.285863816539883908, 1.649083965234589000 ) ) ;
#152338 = CARTESIAN_POINT ( 'NONE',  ( -10.75419052074085080, -7.927673425445466826, 0.6248749548428326195 ) ) ;
#152340 = CARTESIAN_POINT ( 'NONE',  ( 1.364683531249996529, 11.46354166700806410, 0.7879004041258403923 ) ) ;
#152339 = CARTESIAN_POINT ( 'NONE',  ( 1.024742985469536016, 1.345695571256789513, -1.818664117639690714 ) ) ;
#152341 = CARTESIAN_POINT ( 'NONE',  ( -9.318531651294266638, 9.766041769465124034, -0.7998128361456291469 ) ) ;
#152342 = CARTESIAN_POINT ( 'NONE',  ( -5.219525951136856357, 6.152163700156858539, -1.082531754730543971 ) ) ;
#152343 = CARTESIAN_POINT ( 'NONE',  ( -1.201851678989727383E-14, 2.759375000341417916, -1.575800808251660134 ) ) ;
#152344 = CARTESIAN_POINT ( 'NONE',  ( 1.843739406749204335, 8.499999999999996447, 0.7750000000000004663 ) ) ;
#152345 = CARTESIAN_POINT ( 'NONE',  ( 0.7500000000000006661, 10.33333333333333393, 1.299038105676657340 ) ) ;
#152346 = CARTESIAN_POINT ( 'NONE',  ( 4.301177763854931335, 1.387281528384849860, 1.024788870506128990 ) ) ;
#152347 = CARTESIAN_POINT ( 'NONE',  ( 5.876533236880477240, 5.820653295974182129, 0.7998128361456352531 ) ) ;
#152348 = CARTESIAN_POINT ( 'NONE',  ( 2.055556868256277259, 1.765410544359298894, -0.1243799924028898551 ) ) ;
#152349 =( BOUNDED_SURFACE ( )  B_SPLINE_SURFACE ( 3, 3, ( 
 ( #27625, #176032, #190121, #41775, #59058, #77443, #62267, #157647, #209554, #127357 ),
 ( #25489, #91595, #143560, #61198, #9244, #125215, #29776, #193326, #177086, #28703 ),
 ( #194394, #94788, #112158, #166155, #18818, #115347, #117475, #114291, #100094, #51351 ),
 ( #84905, #148845, #147794, #131582, #35074, #418, #150992, #183467, #101144, #113221 ),
 ( #99040, #181338, #167232, #165095, #16687, #63332, #116402, #17742, #199705, #179226 ),
 ( #83830, #180289, #130544, #14558, #15623, #47106, #129492, #213812, #149922, #81713 ),
 ( #31912, #32965, #65432, #195474, #30851, #80656, #197584, #1491, #96929, #66489 ) ),
 .UNSPECIFIED., .T., .F., .T. ) 
 B_SPLINE_SURFACE_WITH_KNOTS ( ( 4, 3, 4 ),
 ( 4, 1, 1, 1, 1, 1, 1, 4 ),
 ( 0.000000000000000000, 0.5000000000000000000, 1.000000000000000000 ),
 ( 0.000000000000000000, 0.09090790722575105287, 0.1825853934691276381, 0.2551728700554835028, 0.3603391217242263855, 0.5205903519787860034, 0.7335386666926504429, 0.9999999999999998890 ),
 .UNSPECIFIED. ) 
 GEOMETRIC_REPRESENTATION_ITEM ( )  RATIONAL_B_SPLINE_SURFACE ( (
 ( 1.000000000000000222, 1.000000000000000222, 1.000000000000000222, 1.000000000000000222, 1.000000000000000222, 1.000000000000000444, 1.000000000000000222, 1.000000000000000222, 1.000000000000000222, 1.000000000000000222),
 ( 0.3333333333333334259, 0.3333333333333334259, 0.3333333333333334259, 0.3333333333333333148, 0.3333333333333334259, 0.3333333333333335369, 0.3333333333333334259, 0.3333333333333334814, 0.3333333333333334259, 0.3333333333333334259),
 ( 0.3333333333333334259, 0.3333333333333334259, 0.3333333333333334259, 0.3333333333333333148, 0.3333333333333334259, 0.3333333333333335369, 0.3333333333333334259, 0.3333333333333334814, 0.3333333333333334259, 0.3333333333333334259),
 ( 1.000000000000000222, 1.000000000000000222, 1.000000000000000222, 1.000000000000000222, 1.000000000000000222, 1.000000000000000444, 1.000000000000000222, 1.000000000000000222, 1.000000000000000222, 1.000000000000000222),
 ( 0.3333333333333334259, 0.3333333333333334259, 0.3333333333333334259, 0.3333333333333333148, 0.3333333333333334259, 0.3333333333333335369, 0.3333333333333334259, 0.3333333333333334814, 0.3333333333333334259, 0.3333333333333334259),
 ( 0.3333333333333334259, 0.3333333333333334259, 0.3333333333333334259, 0.3333333333333333148, 0.3333333333333334259, 0.3333333333333335369, 0.3333333333333334259, 0.3333333333333334814, 0.3333333333333334259, 0.3333333333333334259),
 ( 1.000000000000000222, 1.000000000000000222, 1.000000000000000222, 1.000000000000000222, 1.000000000000000222, 1.000000000000000444, 1.000000000000000222, 1.000000000000000222, 1.000000000000000222, 1.000000000000000222) ) ) 
 REPRESENTATION_ITEM ( '' )  SURFACE ( )  );
#152350 = CARTESIAN_POINT ( 'NONE',  ( 2.666654630192913267, 0.6802043231916419241, 1.894807776549158218 ) ) ;
#152351 = CARTESIAN_POINT ( 'NONE',  ( 10.39640486358069360, 11.02356051713265650, 0.7998128361456462443 ) ) ;
#152352 = CARTESIAN_POINT ( 'NONE',  ( 4.946401613871811875, 2.200551846729232430, 0.1665617540023768828 ) ) ;
#152353 = VERTEX_POINT ( 'NONE', #199508 ) ;
#152354 = CARTESIAN_POINT ( 'NONE',  ( 3.920179414529322504, -2.014104250368133453, 0.1526392722818684933 ) ) ;
#152355 = CARTESIAN_POINT ( 'NONE',  ( -6.831329296439251131, 9.063246493969506545, -1.599625672291271394 ) ) ;
#152357 = CARTESIAN_POINT ( 'NONE',  ( 4.376577478760902196, -0.4445230835841383898, -1.966641233467445016 ) ) ;
#152356 = CARTESIAN_POINT ( 'NONE',  ( 4.987034407221377030, -1.996844880220369545, -0.7138980100366009163 ) ) ;
#152359 = EDGE_LOOP ( 'NONE', ( #39723, #41200, #75005, #20615 ) ) ;
#152358 = CARTESIAN_POINT ( 'NONE',  ( 4.254050669898622239, 0.7686244906546428890, -1.640568623306848606 ) ) ;
#152360 = VERTEX_POINT ( 'NONE', #2363 ) ;
#152361 = CARTESIAN_POINT ( 'NONE',  ( 1.551402291579254022, 0.5461136009352780540, -1.789155053659279071 ) ) ;
#152362 = CARTESIAN_POINT ( 'NONE',  ( 1.579999999999991189, 8.674529973577531194, -2.499999999999989342 ) ) ;
#152363 = CARTESIAN_POINT ( 'NONE',  ( 1.634869402278725348, 1.785593253932623803, 0.6852637533772619749 ) ) ;
#152364 = CARTESIAN_POINT ( 'NONE',  ( -10.89408488338165348, 4.581043481790748828, -4.512313115195546231 ) ) ;
#152365 = DIRECTION ( 'NONE',  ( -0.8271092603120230313, 0.5620411653127359575, 0.000000000000000000 ) ) ;
#152366 = CARTESIAN_POINT ( 'NONE',  ( -0.6823417656250212460, 2.863541667008084879, 1.181850606188767472 ) ) ;
#152367 = CARTESIAN_POINT ( 'NONE',  ( -0.1405747822309927342, -1.479430311965252542, -1.211566217618691210 ) ) ;
#152368 = ADVANCED_FACE ( 'NONE', ( #183273 ), #127324, .T. ) ;
#152369 = CARTESIAN_POINT ( 'NONE',  ( 4.570507181582611267, 8.346359121906111511, 0.000000000000000000 ) ) ;
#152370 = CARTESIAN_POINT ( 'NONE',  ( 1.310910670669521272, -1.548711629584406113, 1.204245502051364936 ) ) ;
#152371 = CARTESIAN_POINT ( 'NONE',  ( 1.930226670627054109, 8.999999999999998224, -0.7749999999999996891 ) ) ;
#152372 = CARTESIAN_POINT ( 'NONE',  ( -5.906512197408906317, 6.919960980845699439, -1.199719254218453823 ) ) ;
#152373 = CARTESIAN_POINT ( 'NONE',  ( 3.832379111121624327, -1.093062754469842579, -1.817066923117337751 ) ) ;
#152374 = CARTESIAN_POINT ( 'NONE',  ( 9.856941372335116469, 11.45851867493453291, 1.199719254218450271 ) ) ;
#152375 = CARTESIAN_POINT ( 'NONE',  ( 5.483651708025924165, 1.321867191758316462, 1.462689542499737039 ) ) ;
#152376 = CARTESIAN_POINT ( 'NONE',  ( 1.364683531249986537, 1.655208333674748955, -0.7879004041258239610 ) ) ;
#152377 = CARTESIAN_POINT ( 'NONE',  ( 1.072522059793120652, 0.8197897455473095452, 1.838922316899212372 ) ) ;
#152378 = ORIENTED_EDGE ( 'NONE', *, *, #3571, .T. ) ;
#152379 = CARTESIAN_POINT ( 'NONE',  ( 1.546650761107182914, -1.494491507556227505, 1.499968751290579494 ) ) ;
#152381 = EDGE_CURVE ( 'NONE', #95167, #138779, #34877, .T. ) ;
#152380 = CARTESIAN_POINT ( 'NONE',  ( 11.53637437042702807, 7.311055218951850065, -3.335631568537873459 ) ) ;
#152382 = CARTESIAN_POINT ( 'NONE',  ( 2.910663983731573090, 0.6951178490613962868, 1.950330170896700022 ) ) ;
#152383 = CARTESIAN_POINT ( 'NONE',  ( 3.040771591214902259, 6.769593633051179005, -0.7998128361456362523 ) ) ;
#152384 = CARTESIAN_POINT ( 'NONE',  ( 5.574337433874081427, 6.532423756721743580, -1.199719254218452047 ) ) ;
#152385 = VERTEX_POINT ( 'NONE', #105252 ) ;
#152387 = CARTESIAN_POINT ( 'NONE',  ( 5.789495288235341874, 6.713164910151406595, 1.199719254218462483 ) ) ;
#152386 = CARTESIAN_POINT ( 'NONE',  ( 5.191392108680514816, -0.7531529969884572795, 1.950447244483977993 ) ) ;
#152390 = EDGE_LOOP ( 'NONE', ( #111168, #182448 ) ) ;
#152389 = CARTESIAN_POINT ( 'NONE',  ( 1.049118701917159946, -1.638035101892039602, 0.7738018112423280526 ) ) ;
#152388 = CARTESIAN_POINT ( 'NONE',  ( 3.030095697178539549, 1.015519584536026976, -1.516846343748608605 ) ) ;
#152391 = DIRECTION ( 'NONE',  ( 0.000000000000000000, 1.000000000000000000, 0.000000000000000000 ) ) ;
#152392 = CARTESIAN_POINT ( 'NONE',  ( -11.86145016429273191, 10.90000000000000036, -1.180000000000002158 ) ) ;
#152393 = CARTESIAN_POINT ( 'NONE',  ( 10.15156572269492052, 13.57203269338523022, 7.275605886047803672 ) ) ;
#152394 = CARTESIAN_POINT ( 'NONE',  ( 4.928867898441261275, 2.110505041808665716, 0.6446608841527908806 ) ) ;
#152395 = CARTESIAN_POINT ( 'NONE',  ( -1.402160292154681736E-14, 8.984375000341396245, 1.575800808251682339 ) ) ;
#152396 = ORIENTED_EDGE ( 'NONE', *, *, #106096, .T. ) ;
#152397 = CARTESIAN_POINT ( 'NONE',  ( 4.371672787583542608, 0.4156390277068115480, -1.866406306929219605 ) ) ;
#152398 = CARTESIAN_POINT ( 'NONE',  ( -2.449219305563052895, 6.009172956465517856, 1.040834085586084257E-14 ) ) ;
#152399 = CARTESIAN_POINT ( 'NONE',  ( 7.422199028477372451, 10.74665040227725044, -1.199719254218441611 ) ) ;
#152400 = CARTESIAN_POINT ( 'NONE',  ( 6.531696417657103737, 1.982406992490031383, -0.5971068152322636102 ) ) ;
#152401 = CARTESIAN_POINT ( 'NONE',  ( -1.500000000000015099, 10.26041666734946034, -0.8660254037844309360 ) ) ;
#152402 = CARTESIAN_POINT ( 'NONE',  ( 4.134873662043553111, 7.767843672452050541, -0.7216878364870197293 ) ) ;
#152403 = CARTESIAN_POINT ( 'NONE',  ( 5.829655996829377962, 1.081331853127937448, -1.906115348727636549 ) ) ;
#152404 = CARTESIAN_POINT ( 'NONE',  ( 5.796475149741596056, 7.337953333587568849, -1.293683646293428913 ) ) ;
#152405 = CARTESIAN_POINT ( 'NONE',  ( -5.969164047770019188, 15.44727374689618138, -10.36856719086336298 ) ) ;
#152406 = ORIENTED_EDGE ( 'NONE', *, *, #24898, .F. ) ;
#152407 =( NAMED_UNIT ( * ) PLANE_ANGLE_UNIT ( ) SI_UNIT ( $, .RADIAN. ) );
#152408 = CARTESIAN_POINT ( 'NONE',  ( 3.602682612693074660, 1.476495159181415939, -1.148357684351591912 ) ) ;
#152409 = CARTESIAN_POINT ( 'NONE',  ( 0.000000000000000000, -2.034374999522043481, -3.793834371823813445 ) ) ;
#152410 = DIRECTION ( 'NONE',  ( 1.000000000000000000, -5.578174157656880887E-15, 1.224646799146938316E-16 ) ) ;
#152411 = EDGE_CURVE ( 'NONE', #4753, #88429, #44359, .T. ) ;
#152412 = CARTESIAN_POINT ( 'NONE',  ( -8.527715433315703919, 9.051348881730875817, 1.040834085586084257E-14 ) ) ;
#152413 = CARTESIAN_POINT ( 'NONE',  ( 3.576318658954677598, 7.394398545414291313, 0.7998128361456281477 ) ) ;
#152414 = CARTESIAN_POINT ( 'NONE',  ( 5.178324605415663306, 8.128796908705222535, 1.199719254218462483 ) ) ;
#152415 = CARTESIAN_POINT ( 'NONE',  ( 0.4441182907778543631, -0.9332952320128800050, 1.734295555568473368 ) ) ;
#152416 = CARTESIAN_POINT ( 'NONE',  ( 1.107046246104196552, -0.04665650516593074226, 2.016035445577879504 ) ) ;
#152417 = CARTESIAN_POINT ( 'NONE',  ( -9.833741488613570780, 10.36711991300432345, 0.7998128361456462443 ) ) ;
#152418 = CARTESIAN_POINT ( 'NONE',  ( 4.681308178468477799, 8.683552984847038303, 0.000000000000000000 ) ) ;
#152419 = CARTESIAN_POINT ( 'NONE',  ( -0.5445930744354052777, 3.250057683544617326, 0.3999999999999455103 ) ) ;
#152420 = CARTESIAN_POINT ( 'NONE',  ( 1.588088344156918907, -2.181139600106785092, -0.2122876309011075546 ) ) ;
#152421 = CARTESIAN_POINT ( 'NONE',  ( 5.865807274569021068, 1.797851641234180287, -0.3166982042408575948 ) ) ;
#152422 = CARTESIAN_POINT ( 'NONE',  ( -3.704402285031864306, 5.344888637335695414, -1.599625672291256295 ) ) ;
#152423 = CARTESIAN_POINT ( 'NONE',  ( 5.722950238744209273, 6.809768379023969587, 1.082531754730549967 ) ) ;
#152424 = CARTESIAN_POINT ( 'NONE',  ( 8.075853055234393452, 12.57357899774884658, 0.7998128361456462443 ) ) ;
#152425 = CARTESIAN_POINT ( 'NONE',  ( 4.054051625686104998, 4.688480637177271149, -1.199719254218446718 ) ) ;
#152426 = CARTESIAN_POINT ( 'NONE',  ( 6.943184063974162434, 9.193743722760251202, -1.443375672974064550 ) ) ;
#152427 = ORIENTED_EDGE ( 'NONE', *, *, #211780, .F. ) ;
#152429 = CARTESIAN_POINT ( 'NONE',  ( 1.102198380138383449, -0.9033151347564006839, 1.799099544393264472 ) ) ;
#152428 = CARTESIAN_POINT ( 'NONE',  ( 3.808014051635350672, 1.299385917162833692, -1.304790556973287163 ) ) ;
#152430 = CARTESIAN_POINT ( 'NONE',  ( 1.652187889876779892, -0.3379717360396676806, -2.273286007567467237 ) ) ;
#152432 = CARTESIAN_POINT ( 'NONE',  ( 1.164654898877310885, 1.413799132238046985, -1.210232755764220069 ) ) ;
#152431 = CARTESIAN_POINT ( 'NONE',  ( 3.660338286009610975, 6.253849852777763729, -1.082531754730543083 ) ) ;
#152433 = CARTESIAN_POINT ( 'NONE',  ( -1.642778471875000035, -3.667708332855373676, -2.845375778867859751 ) ) ;
#152434 = CARTESIAN_POINT ( 'NONE',  ( -5.091250377131585125, 5.898545847196970726, 1.199719254218450271 ) ) ;
#152435 = CARTESIAN_POINT ( 'NONE',  ( 2.969872605471084448, 6.605953636083950364, 2.420000000000000373 ) ) ;
#152436 = CARTESIAN_POINT ( 'NONE',  ( 4.254103502353132171, 0.8128351696983120434, -1.731171583500931366 ) ) ;
#152437 = CARTESIAN_POINT ( 'NONE',  ( -8.597841969360544567, 13.18256606422934674, 0.7998128361456341429 ) ) ;
#152438 = CARTESIAN_POINT ( 'NONE',  ( 6.463930056324285189, 6.765849701160138174, -0.2895399612845122039 ) ) ;
#152439 = CARTESIAN_POINT ( 'NONE',  ( -3.902768115887413014, 5.646591783325653147, -1.599625672291283607 ) ) ;
#152441 = CARTESIAN_POINT ( 'NONE',  ( 2.764352523130030548, -1.291370965961564421, 1.353630663414123969 ) ) ;
#152440 = CARTESIAN_POINT ( 'NONE',  ( 3.966417678127855950, -1.951510144350139919, -0.7507201541567410930 ) ) ;
#152442 = CARTESIAN_POINT ( 'NONE',  ( 8.609064354997688184, 9.146255957026539818, 1.040834085586084257E-14 ) ) ;
#152443 = CARTESIAN_POINT ( 'NONE',  ( -1.364683531250012516, 5.051041667008084879, -0.7879004041258300672 ) ) ;
#152444 = CARTESIAN_POINT ( 'NONE',  ( 3.421201824283449877, -1.039729455425863147, -1.395559870880677789 ) ) ;
#152445 = CARTESIAN_POINT ( 'NONE',  ( 4.334856428067313416, 6.080418470877079429, -1.599625672291256295 ) ) ;
#152447 = CARTESIAN_POINT ( 'NONE',  ( 4.107757354816228279, 6.775838766385488654, -1.082531754730548412 ) ) ;
#152446 = CARTESIAN_POINT ( 'NONE',  ( -0.7500000000000006661, 11.48958333401613174, -1.299038105676657340 ) ) ;
#152448 = CARTESIAN_POINT ( 'NONE',  ( 3.598037535421601429, -1.723020282968828809, -0.08274337828741322454 ) ) ;
#152449 = CARTESIAN_POINT ( 'NONE',  ( 3.614928802375876771, -0.1595779646587774658, 2.185787688459623901 ) ) ;
#152450 = CARTESIAN_POINT ( 'NONE',  ( 6.024089167411393220, -1.222679950896175205, -1.837027303407394507 ) ) ;
#152451 = DIRECTION ( 'NONE',  ( 0.000000000000000000, -7.254698431490450587E-17, 1.000000000000000000 ) ) ;
#152452 = CARTESIAN_POINT ( 'NONE',  ( 3.977515510703835133, -0.1653560672004051324, 2.164858251032927061 ) ) ;
#152453 = CARTESIAN_POINT ( 'NONE',  ( 1.787459277025660542, 1.258035843444211155, 1.323286951131589895 ) ) ;
#152454 = CARTESIAN_POINT ( 'NONE',  ( 0.4019237886466816012, 12.42633545031537068, -1.499999999999998668 ) ) ;
#152455 = CARTESIAN_POINT ( 'NONE',  ( 4.628176351164477786, 2.111873176223429738, 0.1524955421974716341 ) ) ;
#152456 = ORIENTED_EDGE ( 'NONE', *, *, #75356, .F. ) ;
#152458 = CARTESIAN_POINT ( 'NONE',  ( 1.364683531249988535, 2.426041667008088432, 0.7879004041258500513 ) ) ;
#152457 = CARTESIAN_POINT ( 'NONE',  ( 4.739906352223059116, 2.286097037578460611, 0.1700548269078107355 ) ) ;
#152459 = CARTESIAN_POINT ( 'NONE',  ( 6.620655732516666170, 7.629137130509104026, 2.326260288887294969 ) ) ;
#152460 = CARTESIAN_POINT ( 'NONE',  ( 9.728138913005292210, 11.30824913904973705, -1.199719254218440723 ) ) ;
#152461 = AXIS2_PLACEMENT_3D ( 'NONE', #172427, #202754, #169213 ) ;
#152462 = CARTESIAN_POINT ( 'NONE',  ( 0.5574859923395922845, -1.816599148028580579, 1.093606109393664427 ) ) ;
#152463 = CARTESIAN_POINT ( 'NONE',  ( -3.443407828190963915, 6.961133532957338943, 0.7216878364870317197 ) ) ;
#152464 = CARTESIAN_POINT ( 'NONE',  ( 3.892599500454932304, 7.555466827257172113, 0.7216878364870257245 ) ) ;
#152465 = CARTESIAN_POINT ( 'NONE',  ( -5.599154252319524794, 6.595063384869953360, 1.082531754730546636 ) ) ;
#152467 = CARTESIAN_POINT ( 'NONE',  ( -0.7500000000000179856, 10.82291666734946212, 1.299038105676658228 ) ) ;
#152466 = DIRECTION ( 'NONE',  ( 1.000000000000000000, -0.000000000000000000, -0.000000000000000000 ) ) ;
#152468 = VERTEX_POINT ( 'NONE', #168103 ) ;
#152469 = CARTESIAN_POINT ( 'NONE',  ( 5.695935454815424848, 1.779625283580280382, 0.9480427965274510482 ) ) ;
#152471 = CARTESIAN_POINT ( 'NONE',  ( 4.311423628786446471, -1.712024382654028454, -1.150014069924868654 ) ) ;
#152470 = CARTESIAN_POINT ( 'NONE',  ( 5.769158057814842699, 6.689438141327490150, 1.199719254218462483 ) ) ;
#152473 = CARTESIAN_POINT ( 'NONE',  ( 1.737499999999999378, -2.916666666666668295, -3.009438278150925683 ) ) ;
#152472 = CARTESIAN_POINT ( 'NONE',  ( 5.332099551924443404, 9.442809587212341427, 0.000000000000000000 ) ) ;
#152474 = CARTESIAN_POINT ( 'NONE',  ( 7.523848900940885542, 7.742521570711348389, 0.7998128361456291469 ) ) ;
#152475 = CARTESIAN_POINT ( 'NONE',  ( 1.001543065824772753E-15, -1.421874999522042327, 3.793834371823811669 ) ) ;
#152476 = CARTESIAN_POINT ( 'NONE',  ( 0.1331565106231363538, 2.033293680964400885, -2.362282156872722805 ) ) ;
#152477 = CARTESIAN_POINT ( 'NONE',  ( 0.4805627621443783193, -0.2577823606141148027, -2.074612465628209890 ) ) ;
#152478 = CARTESIAN_POINT ( 'NONE',  ( 4.869767617671093340, -0.2496050341583149201, -2.000857388266870984 ) ) ;
#152479 = CARTESIAN_POINT ( 'NONE',  ( 4.405690278861111864, -0.7914791229979671883, -1.662609734262666894 ) ) ;
#152480 = CARTESIAN_POINT ( 'NONE',  ( 4.957477724091233995, 8.935474444748447098, -0.7998128361456281477 ) ) ;
#152481 = CARTESIAN_POINT ( 'NONE',  ( 0.7446035987349702845, -1.482829294443729351, 0.8806902949074472131 ) ) ;
#152482 = PLANE ( 'NONE',  #13156 ) ;
#152483 = CARTESIAN_POINT ( 'NONE',  ( 0.7218034001665899480, 2.265987065647384835, 0.3856900369042133292 ) ) ;
#152484 = CARTESIAN_POINT ( 'NONE',  ( -5.925076824372040640, 6.871343368977510302, 1.199719254218450271 ) ) ;
#152485 = CARTESIAN_POINT ( 'NONE',  ( 0.7380304622728722785, -1.600708836854593198, -1.599060815671312641 ) ) ;
#152486 = CARTESIAN_POINT ( 'NONE',  ( 3.404997959543601294, 1.660052132133410296, -1.295932331351705935 ) ) ;
#152487 = CARTESIAN_POINT ( 'NONE',  ( -4.176793841461789114, 7.030620694084159794, -1.199719254218455378 ) ) ;
#152488 = CARTESIAN_POINT ( 'NONE',  ( 7.949158136313996259, 8.168439335321471262, 1.040834085586084257E-14 ) ) ;
#152489 = CARTESIAN_POINT ( 'NONE',  ( 5.302647476276220573, 8.240153584747313076, -1.082531754730548412 ) ) ;
#152490 = CARTESIAN_POINT ( 'NONE',  ( -6.063521013809733518, 8.097193820909906137, 1.599625672291283607 ) ) ;
#152491 = CARTESIAN_POINT ( 'NONE',  ( 6.060131475184119765, 9.053608573481392696, -1.082531754730537976 ) ) ;
#152492 = CARTESIAN_POINT ( 'NONE',  ( 4.699069518069377338, 7.059409271092678573, 1.379435410134820295 ) ) ;
#152493 = CARTESIAN_POINT ( 'NONE',  ( -3.273404022695637572, 5.906389562198459231, 1.199719254218462483 ) ) ;
#152494 = CARTESIAN_POINT ( 'NONE',  ( 5.519863322019965324, -0.5397129975505778887, 2.154757917147765323 ) ) ;
#152495 = CARTESIAN_POINT ( 'NONE',  ( 2.871223686158608679, 2.080653275041044026, -0.6881803712485771163 ) ) ;
#152496 = CARTESIAN_POINT ( 'NONE',  ( -4.629219384062206011, 7.488174150459498968, -1.199719254218452047 ) ) ;
#152497 = CARTESIAN_POINT ( 'NONE',  ( -11.94105721237523099, 10.19999999999999929, 1.187919463087245386 ) ) ;
#152498 = CARTESIAN_POINT ( 'NONE',  ( 5.476992472119650124, 1.812042599547862176, 0.7524171098330989516 ) ) ;
#152499 = CARTESIAN_POINT ( 'NONE',  ( -0.6823417656250212460, 2.551041667008084435, 1.181850606188767472 ) ) ;
#152500 = FACE_OUTER_BOUND ( 'NONE', #99343, .T. ) ;
#152501 = CARTESIAN_POINT ( 'NONE',  ( -4.094199201646926412, 7.720390135322642067, 0.7216878364870317197 ) ) ;
#152502 = CARTESIAN_POINT ( 'NONE',  ( 4.834296457332984076, -1.136628438424293508, -1.790084250976264002 ) ) ;
#152503 = CARTESIAN_POINT ( 'NONE',  ( -6.455090533882193782, 9.584670485287619002, -1.082531754730549967 ) ) ;
#152504 = ORIENTED_EDGE ( 'NONE', *, *, #129415, .T. ) ;
#152506 = CARTESIAN_POINT ( 'NONE',  ( 6.385629968321593353, 1.486944277142748572, 1.569300510047972219 ) ) ;
#152505 = CARTESIAN_POINT ( 'NONE',  ( -5.804299160426237059, 7.865044668620976509, -1.443375672974066548 ) ) ;
#152507 = CARTESIAN_POINT ( 'NONE',  ( 6.844168616800228477, 6.879284895888727824, -0.7998128361456281477 ) ) ;
#152508 = CARTESIAN_POINT ( 'NONE',  ( 5.267088776126935379, 1.772936381825638952, -0.4966186330585887210 ) ) ;
#152509 = AXIS2_PLACEMENT_3D ( 'NONE', #23641, #25775, #137420 ) ;
#152510 = CARTESIAN_POINT ( 'NONE',  ( -1.364683531249997417, 2.821875000341422801, 1.214306433183764966E-14 ) ) ;
#152511 = CARTESIAN_POINT ( 'NONE',  ( 1.065484398342542383, -1.105240684350906610, 1.344476687319878794 ) ) ;
#152512 = LINE ( 'NONE', #165557, #101460 ) ;
#152513 = DIRECTION ( 'NONE',  ( -0.6123724356957848114, 0.7071067811865540120, 0.3535533905932775611 ) ) ;
#152514 = CARTESIAN_POINT ( 'NONE',  ( -15.75000000000000000, 10.89999999999998259, 1.399999999999998579 ) ) ;
#152515 = ADVANCED_FACE ( 'NONE', ( #170225, #201632 ), #54356, .T. ) ;
#152516 = CARTESIAN_POINT ( 'NONE',  ( 5.084929678302336775, -0.2608814864752464491, -2.145832476913120068 ) ) ;
#152517 = CARTESIAN_POINT ( 'NONE',  ( -3.948449050077848632, 5.629609863222681199, 1.599625672291267398 ) ) ;
#152518 = CARTESIAN_POINT ( 'NONE',  ( -6.331294547457448019, 10.33033470543493770, 0.7216878364870458196 ) ) ;
#152519 = CARTESIAN_POINT ( 'NONE',  ( 4.135729569369491543, -1.488772398488470872, -1.567562023322838671 ) ) ;
#152520 = CARTESIAN_POINT ( 'NONE',  ( 1.364683531249990311, 3.384375000341416140, 1.214306433183764966E-14 ) ) ;
#152521 = CARTESIAN_POINT ( 'NONE',  ( 5.202397865228217455, -0.6614073030348812665, -1.857238293531390916 ) ) ;
#152522 = CARTESIAN_POINT ( 'NONE',  ( 4.393670956608656475, 0.08463240572039069931, 1.731882585348672343 ) ) ;
#152523 = CARTESIAN_POINT ( 'NONE',  ( 0.4159077360078728969, -1.177411712353953588, -1.848246096435968600 ) ) ;
#152524 = CARTESIAN_POINT ( 'NONE',  ( 1.782679935646735769, -1.233298141988391272, 1.950204222970158385 ) ) ;
#152525 = CARTESIAN_POINT ( 'NONE',  ( 3.567699708620798216, 2.011335548252995764, -0.4479969848151729162 ) ) ;
#152526 = CARTESIAN_POINT ( 'NONE',  ( 6.497608386930124880, -1.941524946301041554, 0.05238333795444527485 ) ) ;
#152527 = CARTESIAN_POINT ( 'NONE',  ( -7.510853911846401942, 7.865010440016681592, 1.040834085586084257E-14 ) ) ;
#152528 = CARTESIAN_POINT ( 'NONE',  ( -4.468294144155606773, 7.370704380560280100, 1.199719254218452935 ) ) ;
#152529 = CARTESIAN_POINT ( 'NONE',  ( 0.7499999999999902300, 3.014583334016149418, 1.299038105676669330 ) ) ;
#152530 = CARTESIAN_POINT ( 'NONE',  ( -3.817502770699643388, 6.611447778194983194, 1.199719254218452935 ) ) ;
#152531 = CARTESIAN_POINT ( 'NONE',  ( -6.602457619730773608, 8.725953194484466380, 1.443375672974078761 ) ) ;
#152532 = CARTESIAN_POINT ( 'NONE',  ( 3.698430944683338328, -2.204125419102770600, -0.1106900096672913392 ) ) ;
#152533 = CARTESIAN_POINT ( 'NONE',  ( -3.285556943750000514, -2.326041666188709112, -1.896917185911906500 ) ) ;
#152534 = CARTESIAN_POINT ( 'NONE',  ( 1.006444858994318681, 0.5332790290331288485, 1.782932314864177137 ) ) ;
#152535 =( BOUNDED_SURFACE ( )  B_SPLINE_SURFACE ( 1, 2, ( 
 ( #22660, #191565, #56260, #171063, #155895, #90907, #88771, #76754, #58389, #107201, #124545, #173225, #24805, #156971, #172148, #43229, #7483, #73565, #108275, #38942, #122418, #189451, #8560, #188376, #93044, #158039, #105025, #26936, #40014, #106125, #23740, #74640, #140746, #159086, #142875, #190502, #42160, #174296, #91981, #160154, #62633, #61581, #44284, #28015, #192632, #128793, #94113, #111469, #11752, #30150, #196906, #79955, #48546, #15998, #13877, #98348, #179604, #78882, #213142, #145005, #114664, #113601, #180658, #146058, #45350, #162289, #212071, #211011, #63710, #161222, #110405, #77826, #46411, #129867, #126668, #130914, #194774, #163358, #177475, #112527, #176409, #95173, #81029, #143947, #178540, #82083, #60507, #29089, #97299, #164414, #96239, #12809, #209943, #148176, #127749, #193706, #32283, #195851, #64772, #47491, #31225, #14933, #147116, #33336, #136196, #201151, #200090, #182781, #202214, #53868, #131952, #151376, #101544, #49592, #99418, #120001, #185978, #83147, #118928, #65805, #165473, #21330, #152433, #90376, #183854, #2945, #37611, #1877, #4012, #100471, #214178, #197963, #167613, #17068, #103692, #52789, #51739, #34399, #169741 ),
 ( #115716, #149225, #181706, #800, #66868, #184908, #133013, #199013, #50658, #70082, #116784, #35466, #69017, #135134, #166546, #18134, #86362, #84223, #150311, #67937, #19211, #134082, #117862, #36532, #85290, #102619, #168674, #20278, #192113, #207308, #12298, #125089, #191047, #143427, #29647, #57861, #158574, #43777, #206234, #128301, #193196, #140215, #110950, #8029, #124023, #74119, #107754, #76247, #176957, #78378, #41640, #175903, #160704, #144499, #173780, #10173, #157516, #189989, #25355, #91455, #142356, #9111, #58931, #75187, #126150, #210506, #27494, #62141, #112027, #109890, #194263, #61068, #174845, #94661, #26422, #45909, #209423, #178029, #93594, #141299, #159638, #11235, #92534, #77314, #42712, #108820, #208366, #59997, #127227, #44844, #156445, #28573, #198507, #212632, #31782, #161784, #130418, #116275, #211565, #114163, #51220, #95732, #64273, #132508, #199576, #180156, #196405, #195341, #183341, #117344, #63199, #13375, #79449, #49095, #129363, #17617, #82637, #81581, #48050, #83703, #149791, #145566, #32833, #197454, #46973, #113089, #1365, #67427, #179095, #291, #30717, #96800, #162849, #33889, #14427, #65304, #98910, #164962, #80517 ) ),
 .UNSPECIFIED., .F., .F., .T. ) 
 B_SPLINE_SURFACE_WITH_KNOTS ( ( 2, 2 ),
 ( 3, 2, 2, 2, 2, 2, 2, 2, 2, 2, 2, 2, 2, 2, 2, 2, 2, 2, 2, 2, 2, 2, 2, 2, 2, 2, 2, 2, 2, 2, 2, 2, 2, 2, 2, 2, 2, 2, 2, 2, 2, 2, 2, 2, 2, 2, 2, 2, 2, 2, 2, 2, 2, 2, 2, 2, 2, 2, 2, 2, 2, 2, 2, 2, 2, 2, 2, 2, 2, 3 ),
 ( 0.000000000000000000, 1.000000000000000000 ),
 ( 0.000000000000000000, 0.01388888888888888812, 0.02777777777777777624, 0.04166666666666666435, 0.05555555555555555247, 0.06944444444444444753, 0.08333333333333332871, 0.09722222222222222376, 0.1111111111111111049, 0.1250000000000000000, 0.1388888888888888951, 0.1527777777777777901, 0.1666666666666666574, 0.1805555555555555525, 0.1944444444444444475, 0.2083333333333333426, 0.2222222222222222099, 0.2361111111111111049, 0.2500000000000000000, 0.2638888888888888951, 0.2777777777777777901, 0.2916666666666666852, 0.3055555555555555802, 0.3194444444444444198, 0.3333333333333333148, 0.3472222222222222099, 0.3611111111111111049, 0.3750000000000000000, 0.3888888888888888951, 0.4027777777777777901, 0.4166666666666666852, 0.4305555555555555802, 0.4444444444444444198, 0.4583333333333333148, 0.4722222222222222099, 0.4861111111111111049, 0.5000000000000000000, 0.5138888888888888395, 0.5277777777777777901, 0.5416666666666666297, 0.5555555555555555802, 0.5694444444444444198, 0.5833333333333333703, 0.5972222222222222099, 0.6111111111111111605, 0.6250000000000000000, 0.6388888888888888395, 0.6527777777777777901, 0.6666666666666666297, 0.6805555555555555802, 0.6944444444444444198, 0.7083333333333333703, 0.7222222222222222099, 0.7361111111111111605, 0.7500000000000000000, 0.7638888888888888395, 0.7777777777777777901, 0.7916666666666666297, 0.8055555555555555802, 0.8194444444444444198, 0.8333333333333333703, 0.8472222222222222099, 0.8611111111111111605, 0.8750000000000000000, 0.8888888888888888395, 0.9027777777777777901, 0.9166666666666666297, 0.9305555555555555802, 0.9444444444444444198, 0.9523586252412667985 ),
 .UNSPECIFIED. ) 
 GEOMETRIC_REPRESENTATION_ITEM ( )  RATIONAL_B_SPLINE_SURFACE ( (
 ( 1.000000000000000000, 0.8660254037844387076, 1.000000000000000000, 0.8660254037844387076, 1.000000000000000000, 0.8660254037844387076, 1.000000000000000000, 0.8660254037844387076, 1.000000000000000000, 0.8660254037844387076, 1.000000000000000000, 0.8660254037844387076, 1.000000000000000000, 0.8660254037844387076, 1.000000000000000000, 0.8660254037844387076, 1.000000000000000000, 0.8660254037844387076, 1.000000000000000000, 0.8660254037844387076, 1.000000000000000000, 0.8660254037844387076, 1.000000000000000000, 0.8660254037844387076, 1.000000000000000000, 0.8660254037844387076, 1.000000000000000000, 0.8660254037844387076, 1.000000000000000000, 0.8660254037844387076, 1.000000000000000000, 0.8660254037844387076, 1.000000000000000000, 0.8660254037844387076, 1.000000000000000000, 0.8660254037844387076, 1.000000000000000000, 0.8660254037844387076, 1.000000000000000000, 0.8660254037844387076, 1.000000000000000000, 0.8660254037844387076, 1.000000000000000000, 0.8660254037844387076, 1.000000000000000000, 0.8660254037844387076, 1.000000000000000000, 0.8660254037844387076, 1.000000000000000000, 0.8660254037844387076, 1.000000000000000000, 0.8660254037844387076, 1.000000000000000000, 0.8660254037844387076, 1.000000000000000000, 0.8660254037844387076, 1.000000000000000000, 0.8660254037844387076, 1.000000000000000000, 0.8660254037844387076, 1.000000000000000000, 0.8660254037844387076, 1.000000000000000000, 0.8660254037844387076, 1.000000000000000000, 0.8660254037844387076, 1.000000000000000000, 0.8660254037844387076, 1.000000000000000000, 0.8660254037844387076, 1.000000000000000000, 0.8660254037844387076, 1.000000000000000000, 0.8660254037844387076, 1.000000000000000000, 0.8660254037844387076, 1.000000000000000000, 0.8660254037844387076, 1.000000000000000000, 0.8660254037844387076, 1.000000000000000000, 0.8660254037844387076, 1.000000000000000000, 0.8660254037844387076, 1.000000000000000000, 0.8660254037844387076, 1.000000000000000000, 0.8660254037844387076, 1.000000000000000000, 0.8660254037844387076, 1.000000000000000000, 0.8660254037844387076, 1.000000000000000000, 0.8660254037844387076, 1.000000000000000000, 0.8660254037844387076, 1.000000000000000000, 0.8660254037844387076, 1.000000000000000000, 0.8660254037844387076, 1.000000000000000000, 0.8660254037844387076, 1.000000000000000000, 0.8660254037844387076, 1.000000000000000000, 0.8660254037844387076, 1.000000000000000000, 0.8660254037844387076, 1.000000000000000000, 0.8660254037844387076, 1.000000000000000000, 0.8660254037844387076, 1.000000000000000000, 0.8660254037844387076, 1.000000000000000000, 0.8660254037844387076, 1.000000000000000000, 0.8660254037844387076, 1.000000000000000000, 0.8660254037844387076, 1.000000000000000000, 0.8660254037844387076, 1.000000000000000000, 0.8660254037844387076, 1.000000000000000000, 0.8660254037844387076, 1.000000000000000000, 0.8660254037844387076, 1.000000000000000000, 0.8660254037844387076, 1.000000000000000000, 0.8660254037844387076, 1.000000000000000000, 0.8660254037844387076, 1.000000000000000000, 0.8660254037844387076, 1.000000000000000000, 0.9236584592825519691, 0.9343189473637074638),
 ( 1.000000000000000000, 0.8660254037844387076, 1.000000000000000000, 0.8660254037844387076, 1.000000000000000000, 0.8660254037844387076, 1.000000000000000000, 0.8660254037844387076, 1.000000000000000000, 0.8660254037844387076, 1.000000000000000000, 0.8660254037844387076, 1.000000000000000000, 0.8660254037844387076, 1.000000000000000000, 0.8660254037844387076, 1.000000000000000000, 0.8660254037844387076, 1.000000000000000000, 0.8660254037844387076, 1.000000000000000000, 0.8660254037844387076, 1.000000000000000000, 0.8660254037844387076, 1.000000000000000000, 0.8660254037844387076, 1.000000000000000000, 0.8660254037844387076, 1.000000000000000000, 0.8660254037844387076, 1.000000000000000000, 0.8660254037844387076, 1.000000000000000000, 0.8660254037844387076, 1.000000000000000000, 0.8660254037844387076, 1.000000000000000000, 0.8660254037844387076, 1.000000000000000000, 0.8660254037844387076, 1.000000000000000000, 0.8660254037844387076, 1.000000000000000000, 0.8660254037844387076, 1.000000000000000000, 0.8660254037844387076, 1.000000000000000000, 0.8660254037844387076, 1.000000000000000000, 0.8660254037844387076, 1.000000000000000000, 0.8660254037844387076, 1.000000000000000000, 0.8660254037844387076, 1.000000000000000000, 0.8660254037844387076, 1.000000000000000000, 0.8660254037844387076, 1.000000000000000000, 0.8660254037844387076, 1.000000000000000000, 0.8660254037844387076, 1.000000000000000000, 0.8660254037844387076, 1.000000000000000000, 0.8660254037844387076, 1.000000000000000000, 0.8660254037844387076, 1.000000000000000000, 0.8660254037844387076, 1.000000000000000000, 0.8660254037844387076, 1.000000000000000000, 0.8660254037844387076, 1.000000000000000000, 0.8660254037844387076, 1.000000000000000000, 0.8660254037844387076, 1.000000000000000000, 0.8660254037844387076, 1.000000000000000000, 0.8660254037844387076, 1.000000000000000000, 0.8660254037844387076, 1.000000000000000000, 0.8660254037844387076, 1.000000000000000000, 0.8660254037844387076, 1.000000000000000000, 0.8660254037844387076, 1.000000000000000000, 0.8660254037844387076, 1.000000000000000000, 0.8660254037844387076, 1.000000000000000000, 0.8660254037844387076, 1.000000000000000000, 0.8660254037844387076, 1.000000000000000000, 0.8660254037844387076, 1.000000000000000000, 0.8660254037844387076, 1.000000000000000000, 0.8660254037844387076, 1.000000000000000000, 0.8660254037844387076, 1.000000000000000000, 0.8660254037844387076, 1.000000000000000000, 0.8660254037844387076, 1.000000000000000000, 0.8660254037844387076, 1.000000000000000000, 0.8660254037844387076, 1.000000000000000000, 0.8660254037844387076, 1.000000000000000000, 0.8660254037844387076, 1.000000000000000000, 0.8660254037844387076, 1.000000000000000000, 0.8660254037844387076, 1.000000000000000000, 0.8660254037844387076, 1.000000000000000000, 0.8660254037844387076, 1.000000000000000000, 0.8660254037844387076, 1.000000000000000000, 0.8660254037844387076, 1.000000000000000000, 0.8660254037844387076, 1.000000000000000000, 0.8660254037844387076, 1.000000000000000000, 0.8660254037844387076, 1.000000000000000000, 0.9236584592825519691, 0.9343189473637074638) ) ) 
 REPRESENTATION_ITEM ( '' )  SURFACE ( )  );
#152536 = CARTESIAN_POINT ( 'NONE',  ( -0.1290005225502641184, 1.996213967822700663, -2.587563282167547385 ) ) ;
#152537 = CARTESIAN_POINT ( 'NONE',  ( -9.499633399276474321, -8.038540703696495981, 0.09463244300327114389 ) ) ;
#152539 = CARTESIAN_POINT ( 'NONE',  ( 6.925078400183557470, 1.239878965558613322, 2.257517960274835200 ) ) ;
#152538 = CARTESIAN_POINT ( 'NONE',  ( -5.249610431062532889, 7.793670086080374482, -1.296690129572550365 ) ) ;
#152540 = CARTESIAN_POINT ( 'NONE',  ( 6.703072984701052839, -0.3981723446819797063, 1.804146177254343009 ) ) ;
#152541 = ORIENTED_EDGE ( 'NONE', *, *, #181995, .T. ) ;
#152542 = CARTESIAN_POINT ( 'NONE',  ( 2.993097573648812126, 1.768379194316849423, -1.058085006197813538 ) ) ;
#152543 = CARTESIAN_POINT ( 'NONE',  ( -3.755786496842897795E-14, 1.453125000341440876, 1.570758158831776052 ) ) ;
#152544 = CARTESIAN_POINT ( 'NONE',  ( -6.579784621333750749, 6.570836901177822931, 0.7998128361456341429 ) ) ;
#152545 = CARTESIAN_POINT ( 'NONE',  ( 2.385421078170113507, 0.09676420124534937384, -2.017471438767451275 ) ) ;
#152546 = DIRECTION ( 'NONE',  ( 1.000000000000000000, -0.000000000000000000, -0.000000000000000000 ) ) ;
#152547 = CARTESIAN_POINT ( 'NONE',  ( 3.161022370280501814, 6.839609865302569425, 0.000000000000000000 ) ) ;
#152548 = CARTESIAN_POINT ( 'NONE',  ( 1.832957655136749908, 0.2007874442899897915, 2.051070037287055392 ) ) ;
#152550 = CARTESIAN_POINT ( 'NONE',  ( 0.6823417656249934904, 13.94270833367473195, 1.181850606188764807 ) ) ;
#152549 = CARTESIAN_POINT ( 'NONE',  ( 4.861705877774147311, 4.996687906539577284, 0.6087874222351703501 ) ) ;
#152551 = CARTESIAN_POINT ( 'NONE',  ( 5.795220594837462436, 8.848508896363995291, -1.199719254218440723 ) ) ;
#152552 = CARTESIAN_POINT ( 'NONE',  ( 2.246985366953961449, 2.726529103553876787, 2.500000000000000444 ) ) ;
#152553 = CARTESIAN_POINT ( 'NONE',  ( 5.988949835885216011, -0.3198878037087344306, -2.183464699167809275 ) ) ;
#152554 = CARTESIAN_POINT ( 'NONE',  ( 1.493687833870473325, 1.635750924671933282, 1.413141523588061776 ) ) ;
#152555 = CARTESIAN_POINT ( 'NONE',  ( -5.748293942514189681, 5.808690475795744490, -0.7216878364870207285 ) ) ;
#152556 = CARTESIAN_POINT ( 'NONE',  ( 0.4269707148552639997, -1.727061408318403712, 1.040797348915108111 ) ) ;
#152557 = CARTESIAN_POINT ( 'NONE',  ( 1.845480572931688767, -1.229624162049542058, 1.941665159144045250 ) ) ;
#152558 = CARTESIAN_POINT ( 'NONE',  ( 4.629897721447052028, 8.429254678175810866, 0.5782609040035974202 ) ) ;
#152559 = CARTESIAN_POINT ( 'NONE',  ( -0.4368516432692234330, -5.631911363926715985, -10.55905904256945860 ) ) ;
#152560 = PLANE ( 'NONE',  #134048 ) ;
#152561 = TOROIDAL_SURFACE ( 'NONE', #180256, 7.049999999999999822, 0.9999999999999997780 ) ;
#152562 = CARTESIAN_POINT ( 'NONE',  ( 2.026040307571222332, 1.079255042350239391, -1.527726335390042767 ) ) ;
#152563 = CARTESIAN_POINT ( 'NONE',  ( 3.485564796978508184, -0.5807542032013839339, 1.931124776463407189 ) ) ;
#152565 = CARTESIAN_POINT ( 'NONE',  ( 0.000000000000000000, 2.999999999999999112, -2.420000000000000373 ) ) ;
#152564 = CARTESIAN_POINT ( 'NONE',  ( 1.364683531249988757, 1.384375000341421469, 0.000000000000000000 ) ) ;
#152567 = CARTESIAN_POINT ( 'NONE',  ( 5.602208710206744158, -2.106257355024013567, -0.001338375500582050358 ) ) ;
#152566 = CARTESIAN_POINT ( 'NONE',  ( -8.362681821530818738, 8.650883634741092010, -0.7998128361456291469 ) ) ;
#152568 = CARTESIAN_POINT ( 'NONE',  ( 6.123478934866503742, 10.29580919065294431, 0.7998128361456462443 ) ) ;
#152570 = CARTESIAN_POINT ( 'NONE',  ( -8.362681821530818738, 8.650883634741092010, -0.7998128361456291469 ) ) ;
#152569 = CARTESIAN_POINT ( 'NONE',  ( 4.899292406491845497, 6.809203455697518947, -1.599625672291273171 ) ) ;
#152571 = CARTESIAN_POINT ( 'NONE',  ( 3.840479349152599919, 7.346192795665340114, 0.4818892653144311033 ) ) ;
#152572 = CARTESIAN_POINT ( 'NONE',  ( 5.185809364388858533, 1.945378451193703118, -0.5428193807620449451 ) ) ;
#152573 = CARTESIAN_POINT ( 'NONE',  ( -1.364683531250010295, 5.488541667008087543, -0.7879004041258300672 ) ) ;
#152574 = CARTESIAN_POINT ( 'NONE',  ( 0.3388347341246043531, -1.999784422754165458, -0.5045462532434812353 ) ) ;
#152575 = CARTESIAN_POINT ( 'NONE',  ( 8.270110514656034084, 9.711179024262627024, 1.082531754730558626 ) ) ;
#152576 = CARTESIAN_POINT ( 'NONE',  ( 5.132170659515546518, 1.116069247042193124, -1.851066442873222639 ) ) ;
#152577 = CARTESIAN_POINT ( 'NONE',  ( 6.526270840131753737, 8.707344961610770540, -1.599625672291283607 ) ) ;
#152578 = CARTESIAN_POINT ( 'NONE',  ( -1.364683531250014514, -0.9072916663252470482, 0.7879004041258379498 ) ) ;
#152580 = CARTESIAN_POINT ( 'NONE',  ( 9.648753856163393650, 3.729559674063779084, -7.135166539715068978 ) ) ;
#152579 = CARTESIAN_POINT ( 'NONE',  ( 4.854701522145073334, 7.821512988214679218, -1.199719254218450271 ) ) ;
#152581 = CARTESIAN_POINT ( 'NONE',  ( 6.263503779389103521, 10.25124547602188763, 1.040834085586084257E-14 ) ) ;
#152583 = CARTESIAN_POINT ( 'NONE',  ( -2.744871144686030107, 2.962149295542713112, -2.500000000000111022 ) ) ;
#152582 = CARTESIAN_POINT ( 'NONE',  ( 2.770184829093131462, -2.147865496273542174, 0.3164581508635355145 ) ) ;
#152585 = CARTESIAN_POINT ( 'NONE',  ( 2.085277916773973228, -0.7859315772556186852, 1.665205719185464561 ) ) ;
#152584 = CARTESIAN_POINT ( 'NONE',  ( -5.666945020832185875, 7.634521829102760115, 1.443375672974064550 ) ) ;
#152586 = CARTESIAN_POINT ( 'NONE',  ( 0.6823417656249917140, 3.342708333674754506, 1.181850606188765695 ) ) ;
#152587 = CARTESIAN_POINT ( 'NONE',  ( 4.581673536070863584, -1.032772929490553215, 1.932928240684625099 ) ) ;
#152588 = CARTESIAN_POINT ( 'NONE',  ( 6.883263157960362477, -0.004191378316371896506, 2.053658919477070910 ) ) ;
#152589 = CARTESIAN_POINT ( 'NONE',  ( 5.067353023127458833, 0.2270735253321141400, -2.251102950005756220 ) ) ;
#152590 = CARTESIAN_POINT ( 'NONE',  ( -5.422371370461663176, 8.413518134592214537, -1.199719254218446718 ) ) ;
#152591 = CARTESIAN_POINT ( 'NONE',  ( 1.364683531249988535, 5.717708333674752730, -0.7879004041258300672 ) ) ;
#152592 = CARTESIAN_POINT ( 'NONE',  ( 4.626831674679969808, 8.450518883791096059, -0.3637425496919588497 ) ) ;
#152593 = COLOUR_RGB ( '', 0.31764706, 0.68627451, 0.89019608) ;
#152594 = CARTESIAN_POINT ( 'NONE',  ( 1.500000000000001332, 13.37499999999999822, 0.000000000000000000 ) ) ;
#152595 = CARTESIAN_POINT ( 'NONE',  ( -6.414416072596857532, 6.656109304217339151, -0.7216878364870338292 ) ) ;
#152596 = CARTESIAN_POINT ( 'NONE',  ( 4.719646871332936477, 8.520355426614829142, -0.7216878364870357165 ) ) ;
#152597 = CARTESIAN_POINT ( 'NONE',  ( 4.938602502702000407, 0.3022688342860947452, 1.743538433004296673 ) ) ;
#152598 = B_SPLINE_CURVE_WITH_KNOTS ( 'NONE', 3,
 ( #60585, #61658, #11825, #146135, #77900, #142950 ),
 .UNSPECIFIED., .F., .F.,
 ( 4, 2, 4 ),
 ( 3.471140604459606978E-18, 0.0006533246752568837691, 0.001306649350513764069 ),
 .UNSPECIFIED. ) ;
#152599 = CARTESIAN_POINT ( 'NONE',  ( 8.015895134177609904, 10.37496362800581018, 1.599625672291281386 ) ) ;
#152600 = CARTESIAN_POINT ( 'NONE',  ( 1.993330679213504153, 1.832751758872013914, -1.037179240317965823 ) ) ;
#152602 = CARTESIAN_POINT ( 'NONE',  ( -1.201851678989727383E-14, 1.962500000000020783, 1.732050807568877637 ) ) ;
#152601 = CARTESIAN_POINT ( 'NONE',  ( -0.6823417656250039265, 11.31770833367473728, -1.181850606188755259 ) ) ;
#152603 = CARTESIAN_POINT ( 'NONE',  ( 2.312896453495900673, -1.524290774635113088, 1.247285826271822939 ) ) ;
#152604 = CARTESIAN_POINT ( 'NONE',  ( -5.144392941742557568, 4.966489618313220333, -0.7998128361456362523 ) ) ;
#152605 = CARTESIAN_POINT ( 'NONE',  ( 0.2210476084268316321, -1.750679471464357650, -0.8856473702157914296 ) ) ;
#152607 = ORIENTED_EDGE ( 'NONE', *, *, #175600, .T. ) ;
#152606 = CARTESIAN_POINT ( 'NONE',  ( 5.871335974614770414, -1.558408318232169298, -0.9234296637983196998 ) ) ;
#152608 = CARTESIAN_POINT ( 'NONE',  ( 4.839897650398541806, 8.590371658866210680, 1.040834085586084257E-14 ) ) ;
#152609 = AXIS2_PLACEMENT_3D ( 'NONE', #122653, #57560, #202713 ) ;
#152610 = CARTESIAN_POINT ( 'NONE',  ( -0.6823417656250003738, -0.7197916663252492686, -1.181850606188749264 ) ) ;
#152611 = CARTESIAN_POINT ( 'NONE',  ( 6.209813078548920728, -1.856259414618817383, 0.2309603555875269776 ) ) ;
#152612 = CARTESIAN_POINT ( 'NONE',  ( 3.216308754939877446, 4.775446185561722956, -1.599625672291262513 ) ) ;
#152613 = VERTEX_POINT ( 'NONE', #119412 ) ;
#152614 = CARTESIAN_POINT ( 'NONE',  ( 5.647352632913819726, 1.828451368696734747, -0.9708816006866529680 ) ) ;
#152615 = CARTESIAN_POINT ( 'NONE',  ( 1.224999999999949241, 2.895833333333309501, -0.7072540797573237947 ) ) ;
#152616 = CARTESIAN_POINT ( 'NONE',  ( -5.329763783503577379, 6.351050847909847086, 1.082531754730549078 ) ) ;
#152617 = CARTESIAN_POINT ( 'NONE',  ( 1.499999999999989120, 0.2750000000000182854, 0.000000000000000000 ) ) ;
#152618 = CARTESIAN_POINT ( 'NONE',  ( 7.426115451983150706, 9.686887332112256388, -1.599625672291262513 ) ) ;
#152619 = CARTESIAN_POINT ( 'NONE',  ( -8.317037166979361018, 11.79062823052953668, 1.199719254218453823 ) ) ;
#152620 = CARTESIAN_POINT ( 'NONE',  ( 5.692444392891300886, 7.734547439830227411, -1.599625672291281386 ) ) ;
#152621 = CARTESIAN_POINT ( 'NONE',  ( -1.364683531250000748, 0.009375000341420303140, 0.000000000000000000 ) ) ;
#152622 = CARTESIAN_POINT ( 'NONE',  ( 0.7499999999999902300, 1.483333333333357373, 1.299038105676657340 ) ) ;
#152624 = CARTESIAN_POINT ( 'NONE',  ( 5.335297142177534369, 6.183267073083954735, -1.199719254218452047 ) ) ;
#152623 = CARTESIAN_POINT ( 'NONE',  ( 5.547302793442128177, 1.730978599593002043, -0.9233319674036490898 ) ) ;
#152625 = CARTESIAN_POINT ( 'NONE',  ( 3.690779688840303496, -1.198677090843719872, -1.620934038430859703 ) ) ;
#152626 = CARTESIAN_POINT ( 'NONE',  ( 2.167068266397979670, 1.749796802513942318, -0.7803250849751103280 ) ) ;
#152627 = CARTESIAN_POINT ( 'NONE',  ( -0.1108833634137010304, 0.2458664895051872190, -1.931623620491630611 ) ) ;
#152628 = CARTESIAN_POINT ( 'NONE',  ( 0.01162390915069450026, -2.148011843722149372, 0.4338911918742721641 ) ) ;
#152629 = CARTESIAN_POINT ( 'NONE',  ( 0.000000000000000000, 0.000000000000000000, -0.5000000000000004441 ) ) ;
#152630 = CARTESIAN_POINT ( 'NONE',  ( 2.038157526861613889, 1.849479306444936411, 0.2792354855166642724 ) ) ;
#152631 = CARTESIAN_POINT ( 'NONE',  ( 1.364683531249990311, 5.134375000341417916, 1.214306433183764966E-14 ) ) ;
#152632 = CARTESIAN_POINT ( 'NONE',  ( 4.482685760555058074, -1.311686992106766203, 1.527362355471563182 ) ) ;
#152633 = CARTESIAN_POINT ( 'NONE',  ( -7.100719765255177229, 9.307259030929609267, -1.599625672291263179 ) ) ;
#152635 = CARTESIAN_POINT ( 'NONE',  ( 4.745783977240443541, 2.094000167431044446, -0.3121058131653231538 ) ) ;
#152634 = CARTESIAN_POINT ( 'NONE',  ( -5.924549939491850381, 6.014322472269677533, 0.000000000000000000 ) ) ;
#152637 = EDGE_CURVE ( 'NONE', #99612, #140322, #100029, .T. ) ;
#152636 = CARTESIAN_POINT ( 'NONE',  ( -1.110223024625156540E-16, 1.551257596039481879, 2.000000000000006217 ) ) ;
#152638 = CARTESIAN_POINT ( 'NONE',  ( 6.514133371570012265, 2.065101995627930620, -0.1482383472809906122 ) ) ;
#152640 = CARTESIAN_POINT ( 'NONE',  ( 1.214306433183764966E-14, 2.428612866367529932E-14, 1.500000000000001332 ) ) ;
#152639 = CARTESIAN_POINT ( 'NONE',  ( 1.523107970189445215, -1.967458627398379623, 0.7076814851830464104 ) ) ;
#152642 = EDGE_LOOP ( 'NONE', ( #173409, #20939, #37292, #151048 ) ) ;
#152641 = CARTESIAN_POINT ( 'NONE',  ( 6.141596500199405284, -1.324292569296809052, -1.256812384211228428 ) ) ;
#152643 = CARTESIAN_POINT ( 'NONE',  ( 6.726816770674637347, 10.99970333242910669, -0.7998128361456291469 ) ) ;
#152644 = CARTESIAN_POINT ( 'NONE',  ( -3.895996091634230218, 7.334980739573080832, 0.5863762202383783206 ) ) ;
#152645 = FACE_OUTER_BOUND ( 'NONE', #117004, .T. ) ;
#152646 = CARTESIAN_POINT ( 'NONE',  ( -10.20579153398542616, 5.000000000000003553, 7.525503907114123869 ) ) ;
#152647 = CARTESIAN_POINT ( 'NONE',  ( 6.439759776366769550, 8.536139043893143707, 1.443375672974076540 ) ) ;
#152648 = CARTESIAN_POINT ( 'NONE',  ( -8.012344526598182026E-15, 12.85937500034139802, -1.575800808251669460 ) ) ;
#152649 = LINE ( 'NONE', #80202, #91869 ) ;
#152651 = CARTESIAN_POINT ( 'NONE',  ( 0.9963917123081984517, -1.767100618702711179, -0.3976972079893052459 ) ) ;
#152650 = CARTESIAN_POINT ( 'NONE',  ( 7.530627977747744062, 7.750430493652658015, -0.7998128361456341429 ) ) ;
#152652 = CARTESIAN_POINT ( 'NONE',  ( -7.212047647465563038, 10.50147379109678880, -1.199719254218446718 ) ) ;
#152653 = CIRCLE ( 'NONE', #190825, 10.24999999999998934 ) ;
#152654 = CARTESIAN_POINT ( 'NONE',  ( 4.320244504248938355, 8.192035688265757898, 1.040834085586084257E-14 ) ) ;
#152655 = VECTOR ( 'NONE', #135870, 1000.000000000000114 ) ;
#152656 = CARTESIAN_POINT ( 'NONE',  ( -7.142181811248260459E-15, -6.134628647623513231, 11.00029519899099917 ) ) ;
#152657 = CARTESIAN_POINT ( 'NONE',  ( 4.000938479675252069, 7.594566414207783112, 0.1672846332331431873 ) ) ;
#152658 = CARTESIAN_POINT ( 'NONE',  ( 4.033714395265605823, 4.664753868353354704, -1.199719254218446718 ) ) ;
#152659 = ORIENTED_EDGE ( 'NONE', *, *, #35597, .T. ) ;
#152660 = CARTESIAN_POINT ( 'NONE',  ( 6.222279831957801655, 1.994873610751910942, 0.2930524845206964879 ) ) ;
#152661 = CARTESIAN_POINT ( 'NONE',  ( 0.2234921222181683598, 1.847112181986635626, 1.041312259928407702 ) ) ;
#152662 = CARTESIAN_POINT ( 'NONE',  ( 1.350906756270435993, 4.584752781686859626E-14, 0.1093157834398475192 ) ) ;
#152663 = CARTESIAN_POINT ( 'NONE',  ( 0.1399997263886003374, 0.002789056014650820314, -1.999853399661279063 ) ) ;
#152664 = FACE_BOUND ( 'NONE', #135888, .T. ) ;
#152665 = CARTESIAN_POINT ( 'NONE',  ( -3.795919822146289313, 5.451659097302528068, -1.443375672974053447 ) ) ;
#152666 = CARTESIAN_POINT ( 'NONE',  ( 9.571693261567954636, 12.19006144329456731, 1.443375672974076540 ) ) ;
#152667 = CARTESIAN_POINT ( 'NONE',  ( 3.098452163322249042, 1.954020348291004794, 0.2456459092235723785 ) ) ;
#152668 = CARTESIAN_POINT ( 'NONE',  ( 4.095327490859664188, -0.3419149367107060522, 1.987051255384481463 ) ) ;
#152669 = CARTESIAN_POINT ( 'NONE',  ( -5.682838942422375084, 9.781729199468104596, 0.000000000000000000 ) ) ;
#152670 = CARTESIAN_POINT ( 'NONE',  ( 0.9311234436981489226, -1.996869630441517662, 3.475000000000000533 ) ) ;
#152671 = CARTESIAN_POINT ( 'NONE',  ( -1.500000000000015099, 10.22916666666667318, -0.8660254037844309360 ) ) ;
#152672 = CARTESIAN_POINT ( 'NONE',  ( 4.224703044441734612, 0.1064595904514322594, 2.188988589495489911 ) ) ;
#152673 = DIRECTION ( 'NONE',  ( 1.000000000000000000, 0.000000000000000000, 0.000000000000000000 ) ) ;
#152674 = CARTESIAN_POINT ( 'NONE',  ( 3.399358865922623263, 1.517880436307640579, 1.186064745714454638 ) ) ;
#152675 = CARTESIAN_POINT ( 'NONE',  ( -6.347188469492005325, 10.55680364771601809, -0.7998128361456291469 ) ) ;
#152676 = CARTESIAN_POINT ( 'NONE',  ( -0.02948999725178609935, 2.037268340021273882, -2.343334633859140315 ) ) ;
#152677 = CARTESIAN_POINT ( 'NONE',  ( 0.1333542156527478262, 0.001576319744088505292, -2.046049510433409768 ) ) ;
#152678 = CARTESIAN_POINT ( 'NONE',  ( -0.4206437366318691584, 7.996079560418738907, 1.998769755887072286 ) ) ;
#152679 = ORIENTED_EDGE ( 'NONE', *, *, #127070, .T. ) ;
#152680 = CARTESIAN_POINT ( 'NONE',  ( 5.248414862265931902, 5.295774558831261913, 0.000000000000000000 ) ) ;
#152681 = VERTEX_POINT ( 'NONE', #55413 ) ;
#152682 = CARTESIAN_POINT ( 'NONE',  ( 4.610180678033913182, 1.969109005737102347, -0.04407691609572064739 ) ) ;
#152684 = CARTESIAN_POINT ( 'NONE',  ( 3.580729931658500398, -1.350255368601901651, 1.493277094049742182 ) ) ;
#152683 = CARTESIAN_POINT ( 'NONE',  ( 0.1693407553623625106, 1.118952433510589817, 1.587118285914286941 ) ) ;
#152685 = CARTESIAN_POINT ( 'NONE',  ( 4.938965133657190698, 1.317805461337580697, 1.882938791714399374 ) ) ;
#152687 = CARTESIAN_POINT ( 'NONE',  ( 3.924516644892431572, -1.252765583397809079, 1.376256255023865283 ) ) ;
#152686 = CARTESIAN_POINT ( 'NONE',  ( -4.517335436343488553, 8.499999999999996447, -0.7750000000000013545 ) ) ;
#152688 = CARTESIAN_POINT ( 'NONE',  ( 7.700104897918568447, 7.948153567185284096, 0.000000000000000000 ) ) ;
#152689 = CARTESIAN_POINT ( 'NONE',  ( 0.001745240643721140961, -9.900000000000005684, 0.09998476951564826132 ) ) ;
#152690 = DIRECTION ( 'NONE',  ( 0.000000000000000000, 0.000000000000000000, -1.000000000000000000 ) ) ;
#152691 = CARTESIAN_POINT ( 'NONE',  ( -7.019370843573183194, 9.212351955633947043, 1.599625672291283607 ) ) ;
#152692 = CARTESIAN_POINT ( 'NONE',  ( -4.502716413514313842, 5.386162249589033557, -1.082531754730549967 ) ) ;
#152693 = CARTESIAN_POINT ( 'NONE',  ( 0.1874131419884322858, 1.628132678060219884, 1.467219630700428157 ) ) ;
#152694 = CARTESIAN_POINT ( 'NONE',  ( 4.853455804012203778, 8.606189504748821051, 0.7216878364870438212 ) ) ;
#152695 = ORIENTED_EDGE ( 'NONE', *, *, #208007, .F. ) ;
#152696 = CARTESIAN_POINT ( 'NONE',  ( 10.62873463776380056, 12.29999999999998295, 3.199999999999997957 ) ) ;
#152697 = CARTESIAN_POINT ( 'NONE',  ( -1.138412281109779656E-15, -6.681160345272285639, -10.14529669463342820 ) ) ;
#152698 = CARTESIAN_POINT ( 'NONE',  ( 0.1350027811974127134, -1.670744041527939094, 0.7364786222084362954 ) ) ;
#152699 = CARTESIAN_POINT ( 'NONE',  ( -4.786191920824102830, 5.542644314838231168, 1.199719254218462483 ) ) ;
#152700 = CARTESIAN_POINT ( 'NONE',  ( 3.006226939181593227, -1.670314528538990873, 0.4657782236400943021 ) ) ;
#152701 = CARTESIAN_POINT ( 'NONE',  ( -4.448483798615272100, 8.203998508444197313, 0.000000000000000000 ) ) ;
#152702 = LINE ( 'NONE', #200363, #209115 ) ;
#152703 = CARTESIAN_POINT ( 'NONE',  ( -1.499999999999972689, 3.379166666666690411, -0.8660254037844548058 ) ) ;
#152704 = CARTESIAN_POINT ( 'NONE',  ( 5.268108045213575785, 0.9031548532531764595, 1.586571422427636824 ) ) ;
#152705 = CARTESIAN_POINT ( 'NONE',  ( 2.799599750139214471, -1.450362073461785473, -1.321114446766240347 ) ) ;
#152706 = CARTESIAN_POINT ( 'NONE',  ( -1.225000000000029843, -0.4374999993171646562, -4.163336342344337027E-14 ) ) ;
#152707 = CARTESIAN_POINT ( 'NONE',  ( -7.994504133552415404, 12.47867192245318435, -0.7998128361456281477 ) ) ;
#152708 = CARTESIAN_POINT ( 'NONE',  ( 7.610204295972345712, 7.772993188256215547, 0.7998128361456341429 ) ) ;
#152709 = CARTESIAN_POINT ( 'NONE',  ( 4.283913115580790354, 2.056533504189705930, -0.5163123687341104606 ) ) ;
#152710 = CARTESIAN_POINT ( 'NONE',  ( 8.154303043976348420, 8.478051404252736845, 0.7998128361456281477 ) ) ;
#152711 = CARTESIAN_POINT ( 'NONE',  ( -8.286004436246233951, 12.81875560892930466, 1.040834085586084257E-14 ) ) ;
#152712 = VECTOR ( 'NONE', #170153, 1000.000000000000000 ) ;
#152713 = CARTESIAN_POINT ( 'NONE',  ( 1.991162705694597301, 0.1987741427678466066, 2.060657922996151914 ) ) ;
#152715 = CARTESIAN_POINT ( 'NONE',  ( -0.6823417656250003738, -0.4697916663252491021, -1.181850606188749264 ) ) ;
#152714 = DIRECTION ( 'NONE',  ( 0.000000000000000000, 0.000000000000000000, -1.000000000000000000 ) ) ;
#152717 = ORIENTED_EDGE ( 'NONE', *, *, #203130, .F. ) ;
#152716 = CARTESIAN_POINT ( 'NONE',  ( 4.969482899335432968, -1.875980303166164376, -1.189202907730102732 ) ) ;
#152718 = CARTESIAN_POINT ( 'NONE',  ( 1.793957786719975633, 1.699999873817940044, -1.547402956443538313 ) ) ;
#152719 = CARTESIAN_POINT ( 'NONE',  ( 10.24960094225127172, 11.06021530882240356, -0.7216878364870257245 ) ) ;
#152721 = CARTESIAN_POINT ( 'NONE',  ( -3.285556943749998737, -1.830208332855373987, 1.896917185911908499 ) ) ;
#152720 = CARTESIAN_POINT ( 'NONE',  ( 5.063044020060520900, 4.871582543017558109, 0.7998128361456352531 ) ) ;
#152722 = CARTESIAN_POINT ( 'NONE',  ( 1.124100812432970948E-16, -0.5000000000000004441, -2.025000000000006573 ) ) ;
#152723 = ORIENTED_EDGE ( 'NONE', *, *, #17759, .T. ) ;
#152724 = CARTESIAN_POINT ( 'NONE',  ( 1.224646799147353059E-15, 8.500000000000000000, 9.999999999999996447 ) ) ;
#152725 = CARTESIAN_POINT ( 'NONE',  ( 3.041163856788456687, 0.05134138945498378792, 1.911883771832747048 ) ) ;
#152726 = CARTESIAN_POINT ( 'NONE',  ( 0.1021010164683408133, 6.360493866598983637, -3.113991822131907838 ) ) ;
#152727 = CARTESIAN_POINT ( 'NONE',  ( 4.119902764342167956, -0.8871895459346083035, -1.478924549062347049 ) ) ;
#152728 = CARTESIAN_POINT ( 'NONE',  ( 3.309780021317248355, -1.205041885261768808, -1.616693488061982098 ) ) ;
#152729 = CARTESIAN_POINT ( 'NONE',  ( 3.850415763719742479, 0.2810032917593773272, -2.281380581095279858 ) ) ;
#152730 = CARTESIAN_POINT ( 'NONE',  ( -11.44779964734733113, 12.60189529870398850, -3.599999963171534478 ) ) ;
#152731 = CARTESIAN_POINT ( 'NONE',  ( 6.604139054488365801, -2.105657007711879469, 0.04960021190137350877 ) ) ;
#152732 = CARTESIAN_POINT ( 'NONE',  ( -4.977251789992602760, 8.820894498384422633, 0.000000000000000000 ) ) ;
#152733 = ORIENTED_EDGE ( 'NONE', *, *, #28043, .F. ) ;
#152734 = CARTESIAN_POINT ( 'NONE',  ( 4.305725593384774896, -1.765090080884828661, 0.1286423764911871492 ) ) ;
#152736 = CARTESIAN_POINT ( 'NONE',  ( 0.3579208530809056543, 2.266420720034970415, -0.3425275222256763397 ) ) ;
#152735 = CARTESIAN_POINT ( 'NONE',  ( 5.840530312436913007, 10.03597880781023299, 0.000000000000000000 ) ) ;
#152737 = CARTESIAN_POINT ( 'NONE',  ( 6.333933918656591722, 1.821832875601756774, 0.2651207078676054429 ) ) ;
#152738 = CARTESIAN_POINT ( 'NONE',  ( -7.957709816578236506, 8.248692638954882028, 0.7998128361456341429 ) ) ;
#152739 = CIRCLE ( 'NONE', #170046, 0.08000000000000020983 ) ;
#152740 = CARTESIAN_POINT ( 'NONE',  ( 6.087848540548081999, -2.180536604488235941, -0.2183335821156970336 ) ) ;
#152741 = CARTESIAN_POINT ( 'NONE',  ( -4.950662367645459305, 5.804802846121667415, -1.199719254218453823 ) ) ;
#152742 = CARTESIAN_POINT ( 'NONE',  ( -1.360316468750012886, -0.05729166632526227348, 0.7853790794158901356 ) ) ;
#152743 = CARTESIAN_POINT ( 'NONE',  ( -0.1298852118744100725, 0.003815113116375076861, -1.726395881205538663 ) ) ;
#152744 = CARTESIAN_POINT ( 'NONE',  ( 0.3796378701454300453, -0.1059898317679157376, 2.168723291021804833 ) ) ;
#152745 = CARTESIAN_POINT ( 'NONE',  ( 1.692592581891849912, 1.490968054865527304, -1.357870634957742961 ) ) ;
#152746 = CARTESIAN_POINT ( 'NONE',  ( -1.364683531250010295, 5.280208333674758059, 0.7879004041258379498 ) ) ;
#152747 = CARTESIAN_POINT ( 'NONE',  ( 4.371652425709642742, 1.868346805267994570, -0.4693074334855638630 ) ) ;
#152748 = CARTESIAN_POINT ( 'NONE',  ( -1.364683531250014514, 12.08854166700806765, -0.7879004041258335089 ) ) ;
#152749 = CARTESIAN_POINT ( 'NONE',  ( 1.529832089473160517, -0.2657924667638748017, 2.205375646708715998 ) ) ;
#152751 = ORIENTED_EDGE ( 'NONE', *, *, #89522, .T. ) ;
#152750 = CARTESIAN_POINT ( 'NONE',  ( 9.728138913005292210, 11.30824913904973705, -1.199719254218440723 ) ) ;
#152753 = CARTESIAN_POINT ( 'NONE',  ( 0.4956004317509306034, 7.799479031273147456, -1.990828115380115282 ) ) ;
#152752 = CARTESIAN_POINT ( 'NONE',  ( 1.257539916218596732, 3.033837156058346807, -0.7749999999999874767 ) ) ;
#152754 = CARTESIAN_POINT ( 'NONE',  ( 3.215772567386471437, 6.427315425527130088, -0.8732430475888955934 ) ) ;
#152755 = CARTESIAN_POINT ( 'NONE',  ( 10.71502147350184231, 11.39527989537399755, 0.000000000000000000 ) ) ;
#152756 = CARTESIAN_POINT ( 'NONE',  ( 1.394453263437886604E-15, -2.362500000000000266, 3.474999999999999645 ) ) ;
#152757 = DIRECTION ( 'NONE',  ( 0.8164965809277295872, 1.445884258466820787E-16, -0.5773502691896208461 ) ) ;
#152758 = CARTESIAN_POINT ( 'NONE',  ( 4.370479661831958573, -0.005723030808118654937, -1.740626722379432501 ) ) ;
#152760 = CARTESIAN_POINT ( 'NONE',  ( 2.084357000244409175, 1.132115006494602394, -1.602057852124554316 ) ) ;
#152759 = AXIS2_PLACEMENT_3D ( 'NONE', #37038, #55434, #103122 ) ;
#152762 = CARTESIAN_POINT ( 'NONE',  ( -1.364683531250012516, 2.551041667008089320, -0.7879004041258289570 ) ) ;
#152761 = CARTESIAN_POINT ( 'NONE',  ( 5.996784015946103885, 5.890669528225568996, 1.040834085586084257E-14 ) ) ;
#152763 = ADVANCED_FACE ( 'NONE', ( #106351 ), #122267, .F. ) ;
#152764 = DIRECTION ( 'NONE',  ( 0.000000000000000000, 0.000000000000000000, 1.000000000000000000 ) ) ;
#152765 = CARTESIAN_POINT ( 'NONE',  ( 10.71502147350184231, 11.39527989537399755, 0.000000000000000000 ) ) ;
#152766 = CARTESIAN_POINT ( 'NONE',  ( 0.2915633711191143451, -1.886499572934543956, 0.8344948317597818965 ) ) ;
#152767 = CARTESIAN_POINT ( 'NONE',  ( -8.128276786592724790, 9.441743324901704426, -1.199719254218446718 ) ) ;
#152768 = CARTESIAN_POINT ( 'NONE',  ( -4.080641047588907888, 6.744203074620265248, -1.082531754730548412 ) ) ;
#152769 = CARTESIAN_POINT ( 'NONE',  ( 5.366422816783521732, -1.968444216653497003, -0.4370823996120917765 ) ) ;
#152770 = CARTESIAN_POINT ( 'NONE',  ( 1.007111469781604596, 1.711705730394815106, -1.479659443445595413 ) ) ;
#152772 = ORIENTED_EDGE ( 'NONE', *, *, #109845, .T. ) ;
#152771 = CARTESIAN_POINT ( 'NONE',  ( -4.706651882238427120, 8.642844295920152575, 1.040834085586084257E-14 ) ) ;
#152773 = CARTESIAN_POINT ( 'NONE',  ( -1.402160292154681736E-14, -0.006249999317184824418, 1.732050807568877637 ) ) ;
#152774 = CARTESIAN_POINT ( 'NONE',  ( 1.247088714334358972, -1.471066981041386335, -1.155250539242147045 ) ) ;
#152775 = CARTESIAN_POINT ( 'NONE',  ( 0.01762850287782054270, -1.587011929513387098, 0.6995264333442567928 ) ) ;
#152776 = CARTESIAN_POINT ( 'NONE',  ( 3.861010967126535576, 0.2669419790740577558, -2.175157288012785184 ) ) ;
#152777 = CARTESIAN_POINT ( 'NONE',  ( 5.825286519090714599, -0.06434016213947668650, 2.306860349555530654 ) ) ;
#152778 = CARTESIAN_POINT ( 'NONE',  ( 0.7607050128039081205, -1.493160483426679841, 1.420726879377065988 ) ) ;
#152779 = CARTESIAN_POINT ( 'NONE',  ( 3.908095550721983447, 1.372505747409875632, -1.374073360379985065 ) ) ;
#152780 = CARTESIAN_POINT ( 'NONE',  ( -3.104453987404957260, 6.565687385373657925, -0.7216878364870257245 ) ) ;
#152781 = EDGE_CURVE ( 'NONE', #133641, #209973, #206831, .T. ) ;
#152782 = CARTESIAN_POINT ( 'NONE',  ( 6.046149701670225696, 1.868418987705861234, 0.09211505606019490533 ) ) ;
#152783 =( NAMED_UNIT ( * ) PLANE_ANGLE_UNIT ( ) SI_UNIT ( $, .RADIAN. ) );
#152784 = CARTESIAN_POINT ( 'NONE',  ( 5.007715329123863766E-16, 0.8281250003414059035, -1.570758158831786266 ) ) ;
#152785 = CARTESIAN_POINT ( 'NONE',  ( 4.395157833011634096, -0.8647231026696032830, -1.821742675176166060 ) ) ;
#152786 = CARTESIAN_POINT ( 'NONE',  ( -3.755245360860931303, 5.404205559136275205, -1.443375672974051449 ) ) ;
#152787 = CARTESIAN_POINT ( 'NONE',  ( -5.119085517611572378, 8.129960982925583224, 1.199719254218452935 ) ) ;
#152788 = CARTESIAN_POINT ( 'NONE',  ( 8.178592977541601527, 10.56477777859713463, 1.599625672291281386 ) ) ;
#152790 = FACE_OUTER_BOUND ( 'NONE', #191535, .T. ) ;
#152789 = CARTESIAN_POINT ( 'NONE',  ( 1.928079105319381314, 1.052063804484974385, -1.491885150056403431 ) ) ;
#152791 = CARTESIAN_POINT ( 'NONE',  ( -4.960304097753355457, 6.880383762169266504, 1.599625672291263179 ) ) ;
#152792 = CARTESIAN_POINT ( 'NONE',  ( 0.08000000000000194456, 19.00000000000000000, 11.91973154060107376 ) ) ;
#152793 = CARTESIAN_POINT ( 'NONE',  ( -10.40865662669954084, 4.028931174475638421, 7.242212795919873436 ) ) ;
#152794 = ORIENTED_EDGE ( 'NONE', *, *, #87773, .T. ) ;
#152795 = CARTESIAN_POINT ( 'NONE',  ( -6.143253000323532831, 7.300121600866474658, 1.082531754730548412 ) ) ;
#152796 = UNCERTAINTY_MEASURE_WITH_UNIT (LENGTH_MEASURE( 1.000000000000000082E-05 ), #142440, 'distance_accuracy_value', 'NONE');
#152797 = DIRECTION ( 'NONE',  ( -0.000000000000000000, -1.000000000000000000, -0.000000000000000000 ) ) ;
#152798 = CARTESIAN_POINT ( 'NONE',  ( -10.13488352141530768, 11.78278451552804817, 1.199719254218462483 ) ) ;
#152799 = CARTESIAN_POINT ( 'NONE',  ( 5.777991907792089599, 1.989422559269612201, -0.3473161181037613954 ) ) ;
#152801 = ORIENTED_EDGE ( 'NONE', *, *, #151575, .T. ) ;
#152800 = CARTESIAN_POINT ( 'NONE',  ( -0.1104750535120025967, -0.004616138082884357029, -2.103378236956429337 ) ) ;
#152802 = CARTESIAN_POINT ( 'NONE',  ( -7.584860592202423035, 7.813701877183096833, -0.7998128361456362523 ) ) ;
#152803 = CARTESIAN_POINT ( 'NONE',  ( 5.192936529234042808, 6.017179691316550283, -1.199719254218452047 ) ) ;
#152804 = CARTESIAN_POINT ( 'NONE',  ( 5.225487584538335284, -1.957599804553040945, 0.6444962787128440951 ) ) ;
#152805 = CARTESIAN_POINT ( 'NONE',  ( 3.586564705785996843, -0.5826563296015655480, 1.930417576838711957 ) ) ;
#152806 = ORIENTED_EDGE ( 'NONE', *, *, #103174, .T. ) ;
#152807 = ORIENTED_EDGE ( 'NONE', *, *, #125818, .T. ) ;
#152808 = DIRECTION ( 'NONE',  ( 0.000000000000000000, 1.000000000000000000, 0.000000000000000000 ) ) ;
#152809 = CARTESIAN_POINT ( 'NONE',  ( 3.192055101013606233, 5.811482486902795230, -1.199719254218446718 ) ) ;
#152810 = VECTOR ( 'NONE', #5855, 1000.000000000000000 ) ;
#152812 = EDGE_LOOP ( 'NONE', ( #126531, #107702, #32949, #80468, #147597, #63031, #43294, #113788 ) ) ;
#152811 = CARTESIAN_POINT ( 'NONE',  ( -6.444921918449773024, 8.612437886315108315, 1.599625672291269396 ) ) ;
#152813 = CARTESIAN_POINT ( 'NONE',  ( 5.214490215732396017, 7.828485850976955263, 1.269369371331245500 ) ) ;
#152814 = CARTESIAN_POINT ( 'NONE',  ( 4.182970119252515495, -1.034007530860373336, -1.730600854597413640 ) ) ;
#152815 = CARTESIAN_POINT ( 'NONE',  ( 3.380630241506640932, 1.664009615612583204, -0.7882418170854917916 ) ) ;
#152816 = PRESENTATION_LAYER_ASSIGNMENT (  '', '', ( #132131 ) ) ;
#152817 = EDGE_CURVE ( 'NONE', #210028, #96576, #154904, .T. ) ;
#152818 = CARTESIAN_POINT ( 'NONE',  ( 3.855102659574559443, 8.506872032338398171, 2.500000000000000444 ) ) ;
#152819 = CARTESIAN_POINT ( 'NONE',  ( 1.612422076237954860, -2.289831013633353063, 0.2861181584819341706 ) ) ;
#152820 = CARTESIAN_POINT ( 'NONE',  ( 6.343235766347262938, 8.493804042195527870, -1.599625672291281386 ) ) ;
#152821 = CARTESIAN_POINT ( 'NONE',  ( 4.815789973571149574, -2.120931333841672650, 0.4164600335647972162 ) ) ;
#152822 = CARTESIAN_POINT ( 'NONE',  ( 6.747154001095143627, 11.02343010125301959, -0.7998128361456291469 ) ) ;
#152823 = CARTESIAN_POINT ( 'NONE',  ( 6.614805131849967879, -0.1256686391097518729, 1.812046779126045726 ) ) ;
#152824 = CARTESIAN_POINT ( 'NONE',  ( -6.423865854776591000, 6.388931673527803667, 1.040834085586084257E-14 ) ) ;
#152825 = CARTESIAN_POINT ( 'NONE',  ( -9.497949338967845989, 14.58023493191535813, -7.334250927369855511 ) ) ;
#152826 = CARTESIAN_POINT ( 'NONE',  ( 11.33772463945037146, 10.19999999999998153, 3.679999999999999272 ) ) ;
#152827 = CARTESIAN_POINT ( 'NONE',  ( 1.815107966846595255, -0.2319292346777863389, 1.856160199827073587 ) ) ;
#152828 = CARTESIAN_POINT ( 'NONE',  ( 6.719606758044225359, -1.912400718708512581, 0.4786219606899063117 ) ) ;
#152831 = EDGE_CURVE ( 'NONE', #172003, #72609, #149600, .T. ) ;
#152830 = PRESENTATION_STYLE_ASSIGNMENT (( #20671 ) ) ;
#152829 = CARTESIAN_POINT ( 'NONE',  ( 1.364683531249990311, 5.613541667008087543, 0.7879004041258500513 ) ) ;
#152832 = CARTESIAN_POINT ( 'NONE',  ( 1.137671262558290763, -1.993743905544292927, 0.9465009238469668240 ) ) ;
#152833 = ORIENTED_EDGE ( 'NONE', *, *, #7723, .T. ) ;
#152834 = B_SPLINE_CURVE_WITH_KNOTS ( 'NONE', 3,
 ( #100347, #102482, #87299, #115591, #132884, #116656 ),
 .UNSPECIFIED., .F., .F.,
 ( 4, 2, 4 ),
 ( 5.346776843295201289E-18, 0.001422024648551337882, 0.002844049297102670126 ),
 .UNSPECIFIED. ) ;
#152835 = CARTESIAN_POINT ( 'NONE',  ( 11.97929049433705373, 9.719999999999998863, 0.7046979865771783036 ) ) ;
#152836 = CARTESIAN_POINT ( 'NONE',  ( 3.571683402196252910, 6.254382171615883834, 1.199719254218462483 ) ) ;
#152837 = CARTESIAN_POINT ( 'NONE',  ( -4.948889764188092677, 5.732458465429559169, 1.199719254218462483 ) ) ;
#152838 = CARTESIAN_POINT ( 'NONE',  ( -1.040834085586084257E-14, -9.746166700180788567, -9.579665964948867796 ) ) ;
#152839 = CARTESIAN_POINT ( 'NONE',  ( 6.385619905723967094, 1.359199996644964381, 1.428251207276862500 ) ) ;
#152840 = ADVANCED_FACE ( 'NONE', ( #72717 ), #25362, .T. ) ;
#152841 = CARTESIAN_POINT ( 'NONE',  ( 0.6402171227658737251, -1.634652429315278654, -1.629011242183490804 ) ) ;
#152842 = CARTESIAN_POINT ( 'NONE',  ( 0.6253529088778920775, 0.1960189665039281104, -1.952063659030291998 ) ) ;
#152843 = CARTESIAN_POINT ( 'NONE',  ( 4.645415531332927728, 1.844630620182326153, -0.9228673458712335353 ) ) ;
#152844 = CARTESIAN_POINT ( 'NONE',  ( 4.514501963670558560, 8.210743357683563559, 1.040834085586084257E-14 ) ) ;
#152845 = CARTESIAN_POINT ( 'NONE',  ( 5.342795052237045539, 8.390955439988655229, -1.199719254218450271 ) ) ;
#152846 = EDGE_LOOP ( 'NONE', ( #95408, #43000, #114382, #212105 ) ) ;
#152847 = CARTESIAN_POINT ( 'NONE',  ( 8.392133896734668141, 9.853539636687704828, 1.082531754730558626 ) ) ;
#152848 = CARTESIAN_POINT ( 'NONE',  ( 1.364683531249988535, 2.926041667008082658, 0.7879004041258500513 ) ) ;
#152849 = CARTESIAN_POINT ( 'NONE',  ( -10.72915461426146244, 4.504162602840288798, -5.276318705760902894 ) ) ;
#152850 = CARTESIAN_POINT ( 'NONE',  ( 4.487385655998878953, 6.258369236797239665, 1.443375672974062551 ) ) ;
#152851 = CARTESIAN_POINT ( 'NONE',  ( 6.408646267151912213, 0.6747503738608184864, 2.063755040143978370 ) ) ;
#152852 = CARTESIAN_POINT ( 'NONE',  ( 4.845164456061270997, 0.5726227986864868003, -1.750029900461601340 ) ) ;
#152853 = CARTESIAN_POINT ( 'NONE',  ( 5.630352418794719149, 6.139657267270441920, -0.8181431533968346326 ) ) ;
#152854 = CARTESIAN_POINT ( 'NONE',  ( 0.3857445262360515437, -0.8876765639535091346, 1.646530163845527195 ) ) ;
#152855 = CARTESIAN_POINT ( 'NONE',  ( -5.066364649336571269, 6.741537443998309342, 1.444296757982476587 ) ) ;
#152856 = CARTESIAN_POINT ( 'NONE',  ( 0.3866926556111174862, 2.897682894409570054, 2.027578619373079594 ) ) ;
#152857 = CARTESIAN_POINT ( 'NONE',  ( 5.845834525830363226, 7.300097092180095615, -1.274846751706928849 ) ) ;
#152858 = CARTESIAN_POINT ( 'NONE',  ( 1.277824965264368728, 1.883817941867833134, -0.3277997056638781714 ) ) ;
#152859 = CARTESIAN_POINT ( 'NONE',  ( 2.148939158097754376, -1.419410118233652485, -1.056944606630695560 ) ) ;
#152860 = CARTESIAN_POINT ( 'NONE',  ( 6.375645430456404306, 0.3419251235410331602, -1.983688181122665650 ) ) ;
#152862 = CARTESIAN_POINT ( 'NONE',  ( 4.657778235022878022, 1.106396155499450140, 1.563574394034000115 ) ) ;
#152861 = CARTESIAN_POINT ( 'NONE',  ( -10.17947440576205054, 10.77047498301088346, 0.7998128361456462443 ) ) ;
#152863 = DIRECTION ( 'NONE',  ( -0.6507913734559650498, 0.7592566023652995710, 0.000000000000000000 ) ) ;
#152864 = CARTESIAN_POINT ( 'NONE',  ( 5.951603224533720038, 1.490215702738381331, 1.287855809377226102 ) ) ;
#152865 = CARTESIAN_POINT ( 'NONE',  ( -0.06985027309261250539, -2.078401542846250116, 0.4200961532789050379 ) ) ;
#152866 = CARTESIAN_POINT ( 'NONE',  ( -1.500000000000008216, 10.99999999999999645, 3.469446951953614189E-15 ) ) ;
#152867 = CARTESIAN_POINT ( 'NONE',  ( 3.871829239884491791, 1.038646522470688671, 1.555605274479121114 ) ) ;
#152869 = ORIENTED_EDGE ( 'NONE', *, *, #146351, .T. ) ;
#152868 = CARTESIAN_POINT ( 'NONE',  ( 6.041572768212772893, -1.254329016146822351, -1.184272192918204514 ) ) ;
#152871 = CARTESIAN_POINT ( 'NONE',  ( 4.392478581147586603, 4.226905887534702977, -0.7216878364870188411 ) ) ;
#152870 = CARTESIAN_POINT ( 'NONE',  ( 3.528125218122651230, -1.314342534882004809, -1.772652456903674567 ) ) ;
#152872 = CARTESIAN_POINT ( 'NONE',  ( -1.201851678989727383E-14, 3.009375000341419248, -1.575800808251660134 ) ) ;
#152873 = CARTESIAN_POINT ( 'NONE',  ( 0.7310139678005268538, -1.941628062548940381, -0.6965263486069167564 ) ) ;
#152874 = CARTESIAN_POINT ( 'NONE',  ( 6.154511665599609493, 9.267681812253174556, 1.199719254218462483 ) ) ;
#152875 = CARTESIAN_POINT ( 'NONE',  ( -10.16591625214838679, 10.75465713712827487, 1.040834085586084257E-14 ) ) ;
#152876 = CARTESIAN_POINT ( 'NONE',  ( -5.580151458600902004, 15.44693024363194134, -10.58312568620482708 ) ) ;
#152877 = CARTESIAN_POINT ( 'NONE',  ( -5.037017762676898158, 5.835274463666530131, -1.199719254218446718 ) ) ;
#152878 = CARTESIAN_POINT ( 'NONE',  ( -7.586197045692500751, -6.654700410849692993, -7.966449380362629284 ) ) ;
#152879 = EDGE_LOOP ( 'NONE', ( #190360, #104438, #58057, #129861 ) ) ;
#152880 = CARTESIAN_POINT ( 'NONE',  ( 2.840353284027045344, -1.066491845456703835, 1.774417039089710935 ) ) ;
#152881 = CARTESIAN_POINT ( 'NONE',  ( -1.500000000000011324, 4.920833333333354709, 0.8660254037844403729 ) ) ;
#152882 = CARTESIAN_POINT ( 'NONE',  ( 5.606460214450851964, 6.499623990736163037, 1.199719254218462483 ) ) ;
#152883 = CARTESIAN_POINT ( 'NONE',  ( -6.564228937702958788, 6.791309396811020527, 0.4070866938790471679 ) ) ;
#152884 = CARTESIAN_POINT ( 'NONE',  ( 1.084635305120797089, -1.279634344436600513, 1.562581769784775920 ) ) ;
#152885 = DIRECTION ( 'NONE',  ( 1.000000000000000000, 0.000000000000000000, 0.000000000000000000 ) ) ;
#152887 = CARTESIAN_POINT ( 'NONE',  ( 7.605760987586388744, 11.81721221891873697, 1.040834085586084257E-14 ) ) ;
#152886 = CARTESIAN_POINT ( 'NONE',  ( 0.1749903794560749015, 6.948553613792602057, -2.550375946188668586 ) ) ;
#152888 = CARTESIAN_POINT ( 'NONE',  ( 6.134138708105167481, 0.1511139231759016377, -2.010518800921741622 ) ) ;
#152889 = CARTESIAN_POINT ( 'NONE',  ( 6.368375084315238688, -1.880202862833039834, -0.3662410793365057926 ) ) ;
#152890 = CARTESIAN_POINT ( 'NONE',  ( -3.231779075379147770, 6.036511184309971689, 7.500000000000000000 ) ) ;
#152891 = CARTESIAN_POINT ( 'NONE',  ( 3.913774547416096095, -1.127657808996849198, -1.879056921112079115 ) ) ;
#152892 = CARTESIAN_POINT ( 'NONE',  ( -1.201851678989727383E-14, 3.493750000682815493, 1.732050807568877637 ) ) ;
#152893 = CARTESIAN_POINT ( 'NONE',  ( 2.900541297466651347, -1.884798985816903860, -0.3226963764228693576 ) ) ;
#152894 = CARTESIAN_POINT ( 'NONE',  ( -5.766295404513795297, 5.621766148221195358, 0.7998128361456341429 ) ) ;
#152895 = CARTESIAN_POINT ( 'NONE',  ( 3.456965981360264895, 6.016582164020185530, -1.082531754730543971 ) ) ;
#152897 = CARTESIAN_POINT ( 'NONE',  ( 1.089470510105726708, -0.4871801946146369078, 1.956568126268923846 ) ) ;
#152896 = SURFACE_SIDE_STYLE ('',( #86832 ) ) ;
#152899 = EDGE_CURVE ( 'NONE', #14256, #107724, #96171, .T. ) ;
#152898 = CARTESIAN_POINT ( 'NONE',  ( 1.364683531249996529, 11.02604166700807120, 0.7879004041258405033 ) ) ;
#152901 = CARTESIAN_POINT ( 'NONE',  ( -5.492988512192097161, 6.437516681426083132, 1.199719254218452935 ) ) ;
#152900 = CARTESIAN_POINT ( 'NONE',  ( 6.374583145400191775, -0.1054333438532777389, -2.189162923280890904 ) ) ;
#152903 = ORIENTED_EDGE ( 'NONE', *, *, #21155, .F. ) ;
#152902 = CARTESIAN_POINT ( 'NONE',  ( 3.451896303776471608, 1.724958192144626867, 0.0007732285732166971348 ) ) ;
#152904 = SURFACE_SIDE_STYLE ('',( #105243 ) ) ;
#152905 = CARTESIAN_POINT ( 'NONE',  ( 7.446452682403650769, 9.710614100936176385, -1.599625672291262513 ) ) ;
#152906 = CARTESIAN_POINT ( 'NONE',  ( 4.822949958159288286, 6.649860922651058992, -1.599625672291256295 ) ) ;
#152907 = AXIS2_PLACEMENT_3D ( 'NONE', #68110, #36698, #104932 ) ;
#152908 = DIRECTION ( 'NONE',  ( -0.6507913734559640506, -0.7592566023653004592, 0.000000000000000000 ) ) ;
#152909 = CARTESIAN_POINT ( 'NONE',  ( 1.082386330805637398, 1.171445227557347923, -1.573568114121715933 ) ) ;
#152910 = DIRECTION ( 'NONE',  ( 1.000000000000000000, -8.673617379884035472E-16, 0.000000000000000000 ) ) ;
#152911 = CARTESIAN_POINT ( 'NONE',  ( 3.897079088924235712, 6.634010472798538949, 1.199719254218462483 ) ) ;
#152912 = CARTESIAN_POINT ( 'NONE',  ( 0.07536363704233051131, 7.629137130509080045, -2.744199452819145790 ) ) ;
#152913 = VERTEX_POINT ( 'NONE', #211240 ) ;
#152914 =( NAMED_UNIT ( * ) SI_UNIT ( $, .STERADIAN. ) SOLID_ANGLE_UNIT ( ) );
#152915 = ORIENTED_EDGE ( 'NONE', *, *, #190788, .F. ) ;
#152916 = CARTESIAN_POINT ( 'NONE',  ( 3.545387212860445114, -1.672524232984048620, 0.6962571228125400413 ) ) ;
#152917 = VERTEX_POINT ( 'NONE', #160380 ) ;
#152918 = CARTESIAN_POINT ( 'NONE',  ( 10.38962578677386084, 11.01565159419135043, 0.000000000000000000 ) ) ;
#152919 = CARTESIAN_POINT ( 'NONE',  ( 3.074666975249065626, 6.809138247757705820, 0.000000000000000000 ) ) ;
#152920 = CARTESIAN_POINT ( 'NONE',  ( 5.443967095383744237, -1.154075521934978532, -1.396247737120015930 ) ) ;
#152921 = CARTESIAN_POINT ( 'NONE',  ( 6.902509602688803980, 9.146290184594002781, -1.443375672974064550 ) ) ;
#152922 = CARTESIAN_POINT ( 'NONE',  ( -6.447267651612378359, -6.532648833121157850, -6.949925879317520483 ) ) ;
#152923 = CARTESIAN_POINT ( 'NONE',  ( 5.844719547729445353, 6.005894922780862899, -0.3676955087418033452 ) ) ;
#152925 = CARTESIAN_POINT ( 'NONE',  ( -1.364683531250000748, 15.10937500034140157, 0.000000000000000000 ) ) ;
#152924 = CARTESIAN_POINT ( 'NONE',  ( 5.389040371011321717, 0.1367655989435011543, 1.856064314752596145 ) ) ;
#152926 = CARTESIAN_POINT ( 'NONE',  ( 2.513182649960711945, -1.786459940013595205, 0.6919045257178286779 ) ) ;
#152927 = FACE_OUTER_BOUND ( 'NONE', #91557, .T. ) ;
#152928 = CARTESIAN_POINT ( 'NONE',  ( -10.94023239993386554, 4.766145680744502400, 4.420001064107922595 ) ) ;
#152929 = CARTESIAN_POINT ( 'NONE',  ( 9.499734081922104778, -9.919612995835008107, -0.07111086427374714580 ) ) ;
#152930 = CYLINDRICAL_SURFACE ( 'NONE', #84291, 1.224999999999996980 ) ;
#152931 = CARTESIAN_POINT ( 'NONE',  ( 6.968527767744104651, 8.192665819532020777, 1.082531754730558626 ) ) ;
#152932 = B_SPLINE_CURVE_WITH_KNOTS ( 'NONE', 3,
 ( #209811, #93978, #113471, #91847, #43097, #160019, #128673, #125468, #177340, #95037, #141679, #179476, #207692, #11618, #127613, #59311, #191430, #211945, #92909, #193578, #109211, #145934, #143814, #175222, #13750, #47356, #158955, #26807, #63581, #61446, #10550, #157904, #111336, #46284, #9498, #195721, #76624, #129738, #96107, #75570 ),
 .UNSPECIFIED., .F., .F.,
 ( 4, 2, 2, 2, 2, 2, 2, 2, 2, 2, 2, 2, 2, 2, 2, 2, 2, 2, 2, 4 ),
 ( -6.000000000487433838E-08, 0.0003665413137380137175, 0.0007331426274760322829, 0.001466345254952070715, 0.002932750509904150180, 0.005865561019808307811, 0.007331966274760386842, 0.008798371529712465874, 0.01026477678466454491, 0.01173118203961662567, 0.01319758729456870470, 0.01393078992204474335, 0.01466399254952078374, 0.01613039780447286450, 0.01759680305942494180, 0.02052961356932909293, 0.02199601882428117369, 0.02272922145175720887, 0.02309582276549522820, 0.02346242407923325446 ),
 .UNSPECIFIED. ) ;
#152933 = CARTESIAN_POINT ( 'NONE',  ( -2.767835915484202047, 6.380892334706859792, -0.7998128361456281477 ) ) ;
#152934 = CARTESIAN_POINT ( 'NONE',  ( 0.1456854043008250221, -1.672057201651616642, -1.369741535119282982 ) ) ;
#152935 = CARTESIAN_POINT ( 'NONE',  ( -5.586841817283045408, 8.675676665875643678, 1.199719254218454489 ) ) ;
#152936 = CARTESIAN_POINT ( 'NONE',  ( 1.693425821628431471, -0.7032018978916483309, 1.968960419152628871 ) ) ;
#152937 = CARTESIAN_POINT ( 'NONE',  ( 5.180097208873055692, 8.201141289397330780, -1.199719254218450271 ) ) ;
#152938 = CARTESIAN_POINT ( 'NONE',  ( 6.334985678650366658, 0.1896739171414266178, 1.917017188598265420 ) ) ;
#152939 = CARTESIAN_POINT ( 'NONE',  ( -4.660252114795309097, 6.460046772059735432, -1.599625672291256295 ) ) ;
#152940 = EDGE_CURVE ( 'NONE', #200355, #50012, #199862, .T. ) ;
#152941 = CARTESIAN_POINT ( 'NONE',  ( 2.397230751819504402, 1.409552409829779140, 1.160114028286141075 ) ) ;
#152942 = CARTESIAN_POINT ( 'NONE',  ( 12.13020669054560408, 8.043700598764450760, -3.170917236059372257 ) ) ;
#152943 = CARTESIAN_POINT ( 'NONE',  ( 1.828231037913151447, -0.9045423626323212396, -1.684975973026317408 ) ) ;
#152944 = CARTESIAN_POINT ( 'NONE',  ( 1.223035424556912387, -1.779184897175438707, -0.8450996447877844320 ) ) ;
#152945 = CARTESIAN_POINT ( 'NONE',  ( 4.089352007823720214, -0.7402336266850146895, 1.795645171352943770 ) ) ;
#152946 = ORIENTED_EDGE ( 'NONE', *, *, #79298, .F. ) ;
#152947 = DIRECTION ( 'NONE',  ( -0.7592566023652995710, 0.6507913734559650498, -0.000000000000000000 ) ) ;
#152948 = CARTESIAN_POINT ( 'NONE',  ( -5.652823702255029836, 5.559658838911111900, -0.7998128361456362523 ) ) ;
#152950 = CARTESIAN_POINT ( 'NONE',  ( 3.955424862866574021, -1.843446357660895041, 1.048082435718917571 ) ) ;
#152949 = CARTESIAN_POINT ( 'NONE',  ( 4.706615602599436343, 5.520081620234675412, 1.199719254218452935 ) ) ;
#152951 = CARTESIAN_POINT ( 'NONE',  ( -10.50000000000000000, 13.39999999999998259, 3.599999999999999201 ) ) ;
#152952 = CARTESIAN_POINT ( 'NONE',  ( 8.666686507633574621, 11.13422023037111330, 1.599625672291281386 ) ) ;
#152953 = CARTESIAN_POINT ( 'NONE',  ( 5.684994455280509840, 6.294486374732538359, 1.096603583888225764 ) ) ;
#152954 = CARTESIAN_POINT ( 'NONE',  ( -5.249999999999987566, -1.374772708486751593, 1.000000000000000888 ) ) ;
#152955 = CARTESIAN_POINT ( 'NONE',  ( 5.501576472095266901, 9.640532660744973725, -0.7998128361456481317 ) ) ;
#152957 =( BOUNDED_CURVE ( )  B_SPLINE_CURVE ( 2, ( #36617, #104849, #84308 ),
 .UNSPECIFIED., .F., .T. ) 
 B_SPLINE_CURVE_WITH_KNOTS ( ( 3, 3 ),
 ( 0.2750000000000000777, 0.2778239691812269263 ),
 .UNSPECIFIED. ) 
 CURVE ( )  GEOMETRIC_REPRESENTATION_ITEM ( )  RATIONAL_B_SPLINE_CURVE ( ( 0.9999999999999982236, 0.9091983686127850239, 0.9414788213740286071 ) ) 
 REPRESENTATION_ITEM ( '' )  );
#152956 = DIRECTION ( 'NONE',  ( 0.01745240643728004568, 0.000000000000000000, 0.9998476951563912696 ) ) ;
#152958 = CARTESIAN_POINT ( 'NONE',  ( 4.248545464119923842, 0.4890907236730773766, 1.758887239191930796 ) ) ;
#152959 = CARTESIAN_POINT ( 'NONE',  ( -8.283668668269720925, 8.766627655843896250, 1.056142170575426150E-14 ) ) ;
#152960 = CARTESIAN_POINT ( 'NONE',  ( -8.324343129110692630, 12.65555805069709550, 0.7216878364870338292 ) ) ;
#152961 =( GEOMETRIC_REPRESENTATION_CONTEXT ( 3 ) GLOBAL_UNCERTAINTY_ASSIGNED_CONTEXT ( ( #203084 ) ) GLOBAL_UNIT_ASSIGNED_CONTEXT ( ( #160485, #80298, #30497 ) ) REPRESENTATION_CONTEXT ( 'NONE', 'WORKASPACE' ) );
#152962 = CARTESIAN_POINT ( 'NONE',  ( -5.196461137543813891, 7.842688287721260032, 1.273345793684066862 ) ) ;
#152963 = CARTESIAN_POINT ( 'NONE',  ( 6.796206128891365772, -7.030236945367178691, -6.776587425048098190 ) ) ;
#152964 = CARTESIAN_POINT ( 'NONE',  ( 4.680451076648031616, -1.814532364864028136, -0.4542276060127621862 ) ) ;
#152965 = CARTESIAN_POINT ( 'NONE',  ( 8.209625708274705502, 9.536650400197368427, 1.199719254218462483 ) ) ;
#152966 = CIRCLE ( 'NONE', #208297, 0.08000000000000020983 ) ;
#152967 = CARTESIAN_POINT ( 'NONE',  ( 2.227063406323766870, -8.064668077616128736E-05, 1.926676517253867793 ) ) ;
#152968 = CARTESIAN_POINT ( 'NONE',  ( 3.094265954482837255, 2.800000000000017586, 2.490342512183689294 ) ) ;
#152969 = CARTESIAN_POINT ( 'NONE',  ( 3.680148631105580215, 6.380924938676771241, -1.199719254218446718 ) ) ;
#152970 = CARTESIAN_POINT ( 'NONE',  ( -1.364683531250010295, 9.692708333674737275, 0.7879004041258445001 ) ) ;
#152971 = CARTESIAN_POINT ( 'NONE',  ( -6.898401231254901234, 6.942556279419168419, -0.7998128361456291469 ) ) ;
#152972 = CARTESIAN_POINT ( 'NONE',  ( 4.741601036477289810, 6.554953847355395880, 1.599625672291267398 ) ) ;
#152973 = EDGE_CURVE ( 'NONE', #176198, #42265, #2712, .T. ) ;
#152974 = CARTESIAN_POINT ( 'NONE',  ( -4.787437638956935082, 6.678706226906775179, -1.443375672974066548 ) ) ;
#152975 = CARTESIAN_POINT ( 'NONE',  ( 0.8435474745839615096, 0.4086855458026328880, -2.077256349191716200 ) ) ;
#152976 = CARTESIAN_POINT ( 'NONE',  ( 6.972266317189433020E-16, 0.5000000006828014820, -1.225000000000012745 ) ) ;
#152977 = CARTESIAN_POINT ( 'NONE',  ( -1.364067407192364412, 3.688075514171739400, -0.6250643920678800036 ) ) ;
#152978 = CARTESIAN_POINT ( 'NONE',  ( 5.858279169847476098, -2.070434559870216074, -0.005763162253501209233 ) ) ;
#152980 = CARTESIAN_POINT ( 'NONE',  ( 4.005937425286727027, 7.819599604358462130, 0.1919598339409686050 ) ) ;
#152979 = CARTESIAN_POINT ( 'NONE',  ( 0.4504185290156897947, -1.555054577268409899, -0.9855837367087336709 ) ) ;
#152981 = CARTESIAN_POINT ( 'NONE',  ( 6.082725252809636274, -0.7780705872160005310, 2.163147651226764889 ) ) ;
#152982 = CARTESIAN_POINT ( 'NONE',  ( 6.507550544879468823, 6.694489845221929691, -0.7216878364870257245 ) ) ;
#152984 = CARTESIAN_POINT ( 'NONE',  ( 0.2305739854149619072, 7.031539004852044528, 3.921949077993606370 ) ) ;
#152983 = CARTESIAN_POINT ( 'NONE',  ( 3.431622278034673901, 7.017660067766835930, -1.734723475976807094E-15 ) ) ;
#152985 = CARTESIAN_POINT ( 'NONE',  ( 1.008267258593512183, -1.035053087846869335, -2.045343892876672065 ) ) ;
#152986 = CARTESIAN_POINT ( 'NONE',  ( -0.02191154088443912629, -9.962467531990274239, -9.579628365760338937 ) ) ;
#152987 = CARTESIAN_POINT ( 'NONE',  ( -5.773793314573309132, 7.829454515125894964, 1.599625672291263179 ) ) ;
#152988 = CARTESIAN_POINT ( 'NONE',  ( 6.140568862321206467, -1.639224632874112020, 1.040935801138809236 ) ) ;
#152989 = EDGE_LOOP ( 'NONE', ( #90464, #137713, #49940, #105816 ) ) ;
#152990 = CARTESIAN_POINT ( 'NONE',  ( 8.717529583462654941, 9.272798723569005475, 0.7216878364870458196 ) ) ;
#152991 = ORIENTED_EDGE ( 'NONE', *, *, #56061, .F. ) ;
#152992 = CARTESIAN_POINT ( 'NONE',  ( -0.1228044941411730595, -1.800067586368118588, -0.9016598371343366169 ) ) ;
#152993 = CARTESIAN_POINT ( 'NONE',  ( -10.62011439820619429, 11.28455497419572318, -0.7998128361456221525 ) ) ;
#152994 = CARTESIAN_POINT ( 'NONE',  ( -8.701635661872465732, 9.046329781806354831, 1.040834085586084257E-14 ) ) ;
#152995 = DIRECTION ( 'NONE',  ( -0.000000000000000000, -1.000000000000000000, -0.000000000000000000 ) ) ;
#152997 = CARTESIAN_POINT ( 'NONE',  ( 1.287592460671227457, -0.8000790430911768336, 1.578758917787604021 ) ) ;
#152996 = CARTESIAN_POINT ( 'NONE',  ( 3.240259679068544507, 0.5084995621511109176, 2.027717503869540749 ) ) ;
#152999 = CARTESIAN_POINT ( 'NONE',  ( 4.330218815260163723, 2.247629863848239040, 0.4493651543184833397 ) ) ;
#152998 = FILL_AREA_STYLE_COLOUR ( '', #183528 ) ;
#153000 = CARTESIAN_POINT ( 'NONE',  ( 3.538731034799988073, -1.318886434843706601, -1.135564254951209273 ) ) ;
#153001 = ADVANCED_FACE ( 'NONE', ( #210173 ), #40809, .T. ) ;
#153002 = CARTESIAN_POINT ( 'NONE',  ( 8.703444544968814256, 12.24143683818393313, -1.199719254218446718 ) ) ;
#153003 = CIRCLE ( 'NONE', #56069, 1.500000000000005107 ) ;
#153004 = CARTESIAN_POINT ( 'NONE',  ( 2.987300135396570688, 1.631410314640189929, 0.5874552976607245736 ) ) ;
#153005 = CARTESIAN_POINT ( 'NONE',  ( 3.543588177981399134, 1.964110833604881812, -0.9256020844959752525 ) ) ;
#153006 = CARTESIAN_POINT ( 'NONE',  ( 3.174580523894166006, 6.855427711185178019, 0.7998128361456341429 ) ) ;
#153007 = CARTESIAN_POINT ( 'NONE',  ( 4.188685576152741064, 1.555700494002542067, -1.282988152656767911 ) ) ;
#153008 = CARTESIAN_POINT ( 'NONE',  ( 2.062500000000001776, -1.451031289061204266, -1.451031289061035956 ) ) ;
#153009 =( BOUNDED_CURVE ( )  B_SPLINE_CURVE ( 2, ( #157326, #11038, #137879, #41453, #23014 ),
 .UNSPECIFIED., .F., .T. ) 
 B_SPLINE_CURVE_WITH_KNOTS ( ( 3, 2, 3 ),
 ( 0.1229971016045082050, 0.1250000000000000000, 0.1273350245274847692 ),
 .UNSPECIFIED. ) 
 CURVE ( )  GEOMETRIC_REPRESENTATION_ITEM ( )  RATIONAL_B_SPLINE_CURVE ( ( 0.9331125556462565029, 0.9355989990887658703, 1.000000000000000000, 0.9249198476264313129, 0.9339904139662591476 ) ) 
 REPRESENTATION_ITEM ( '' )  );
#153010 = CARTESIAN_POINT ( 'NONE',  ( -1.500000000000011324, 2.952083334016149418, 0.8660254037844403729 ) ) ;
#153011 = CARTESIAN_POINT ( 'NONE',  ( 1.483290174073574441, 1.780938433730950621, -0.7347945396837353149 ) ) ;
#153012 = CARTESIAN_POINT ( 'NONE',  ( -1.500000000000008216, 8.781250000682797818, 3.469446951953614189E-15 ) ) ;
#153013 = CARTESIAN_POINT ( 'NONE',  ( 4.974942202162922378, -1.608427002576447995, 1.532403895573146491 ) ) ;
#153014 = ORIENTED_EDGE ( 'NONE', *, *, #197793, .F. ) ;
#153015 = CARTESIAN_POINT ( 'NONE',  ( 6.883263157960373135, 2.058310207169287143, 2.252834201749584153 ) ) ;
#153016 = CARTESIAN_POINT ( 'NONE',  ( 0.7499999999999902300, 1.233333333333357151, 1.299038105676657340 ) ) ;
#153017 = CARTESIAN_POINT ( 'NONE',  ( 7.070740804726770357, 8.207951346058097286, 1.199719254218462483 ) ) ;
#153018 = ADVANCED_FACE ( 'NONE', ( #191792, #95409 ), #75929, .T. ) ;
#153019 = CARTESIAN_POINT ( 'NONE',  ( 5.192409643909512873, 6.120528008391641350, -1.082531754730549078 ) ) ;
#153020 = CARTESIAN_POINT ( 'NONE',  ( 1.001543065824772753E-15, -1.071874999522044014, 3.793834371823810780 ) ) ;
#153021 = CARTESIAN_POINT ( 'NONE',  ( 0.2413015266095243083, 2.127564327900688390, 0.6385326005407893080 ) ) ;
#153022 = CARTESIAN_POINT ( 'NONE',  ( 6.268018250734934682, -1.947192974725008963, 0.2387856323943157166 ) ) ;
#153023 = CARTESIAN_POINT ( 'NONE',  ( 7.890482213473377193, 11.18901776815221716, -1.082531754730543083 ) ) ;
#153024 = CARTESIAN_POINT ( 'NONE',  ( -0.001208985763515336336, 3.412797577246581060, 2.002358321876673397 ) ) ;
#153025 = CARTESIAN_POINT ( 'NONE',  ( 0.4566077865506940059, 0.8268718848777978359, 1.997384878126715613 ) ) ;
#153026 = VECTOR ( 'NONE', #185040, 1000.000000000000000 ) ;
#153028 = AXIS2_PLACEMENT_3D ( 'NONE', #52221, #37023, #155058 ) ;
#153027 = CARTESIAN_POINT ( 'NONE',  ( -6.129694847154231852, 6.323934541200937787, -0.7216878364870338292 ) ) ;
#153029 = CARTESIAN_POINT ( 'NONE',  ( 3.807127647779250168, -1.688003362470591684, 1.185206751978077788 ) ) ;
#153030 = CARTESIAN_POINT ( 'NONE',  ( -4.232116505760120440, 8.089219690028791376, -0.7998128361456281477 ) ) ;
#153031 = CARTESIAN_POINT ( 'NONE',  ( -1.499999999999997780, 3.681250000682819046, 1.214306433183764966E-14 ) ) ;
#153032 = CARTESIAN_POINT ( 'NONE',  ( -1.201851678989727383E-14, 5.009375000341421469, -1.575800808251660134 ) ) ;
#153033 = CARTESIAN_POINT ( 'NONE',  ( 4.692568346783878575, -0.4079999995015987091, -1.825350503840660110 ) ) ;
#153034 = CARTESIAN_POINT ( 'NONE',  ( 4.131323472851686773, 0.4681366286901997853, 1.669664985128198831 ) ) ;
#153035 = CARTESIAN_POINT ( 'NONE',  ( 3.843067196288481480, 0.5821562417002418277, -1.640339850388317089 ) ) ;
#153036 = CARTESIAN_POINT ( 'NONE',  ( 0.6797070353673840826, 1.544897314466355143, 1.693757226825955753 ) ) ;
#153037 = CARTESIAN_POINT ( 'NONE',  ( 1.364683531249988535, 3.967708333674751842, -0.7879004041258239610 ) ) ;
#153038 = CARTESIAN_POINT ( 'NONE',  ( 4.511325128988150190, -2.050071535818901225, 0.4094859698564096706 ) ) ;
#153039 = CARTESIAN_POINT ( 'NONE',  ( 0.4273693582952375891, 0.9489586001507933632, -1.577591209259328275 ) ) ;
#153040 = EDGE_CURVE ( 'NONE', #191004, #213528, #79764, .T. ) ;
#153041 = DIRECTION ( 'NONE',  ( 0.000000000000000000, 0.000000000000000000, 1.000000000000000000 ) ) ;
#153042 = CARTESIAN_POINT ( 'NONE',  ( 1.266250242576156815, 1.862016182229693673, -0.7743172429433076154 ) ) ;
#153043 = CARTESIAN_POINT ( 'NONE',  ( 2.609770642201841184, 0.3830433331901660354, -0.1872689674646474400 ) ) ;
#153044 = CARTESIAN_POINT ( 'NONE',  ( 6.717278222822382183, -7.473374494058092843, -6.750415307812249743 ) ) ;
#153045 = CARTESIAN_POINT ( 'NONE',  ( -7.167456763118792651, 11.51378332361394818, 0.000000000000000000 ) ) ;
#153046 = CARTESIAN_POINT ( 'NONE',  ( 4.984594031318565932, 8.967110136513669616, 0.7998128361456462443 ) ) ;
#153047 = CARTESIAN_POINT ( 'NONE',  ( 2.315225504062240702, 1.701464259299827919, -1.265282535349021575 ) ) ;
#153048 = CYLINDRICAL_SURFACE ( 'NONE', #139463, 3.475000000000000089 ) ;
#153049 = CARTESIAN_POINT ( 'NONE',  ( 5.936143289257818978, 0.8957264799932495025, -1.590785280889392528 ) ) ;
#153050 = ORIENTED_EDGE ( 'NONE', *, *, #160143, .F. ) ;
#153051 = CARTESIAN_POINT ( 'NONE',  ( -6.200875153403786477, 8.327716660428123419, -1.599625672291271394 ) ) ;
#153052 = CARTESIAN_POINT ( 'NONE',  ( 3.285556943750000514, -0.7510416661887079348, 1.896917185911906500 ) ) ;
#153053 = CARTESIAN_POINT ( 'NONE',  ( -6.856673000209188906, 9.022537805042615489, 1.599625672291283607 ) ) ;
#153054 = CARTESIAN_POINT ( 'NONE',  ( 1.916276942859599597, -2.019257470013501088, 0.05376132052286108215 ) ) ;
#153055 = CARTESIAN_POINT ( 'NONE',  ( 0.07735805125222078305, -0.0005418671161615954465, -2.088975025666544472 ) ) ;
#153056 = CIRCLE ( 'NONE', #135752, 4.000000000000000000 ) ;
#153057 = CARTESIAN_POINT ( 'NONE',  ( -4.604929450496978660, 5.401447776115099408, -1.199719254218453823 ) ) ;
#153058 = CARTESIAN_POINT ( 'NONE',  ( 4.117883143796479573, 1.847306362133010360, -0.2240370018555241372 ) ) ;
#153059 = CARTESIAN_POINT ( 'NONE',  ( 9.240045382913317340, 10.73880668727576015, -1.199719254218446718 ) ) ;
#153060 = CARTESIAN_POINT ( 'NONE',  ( 2.972033609136344623, 6.549060441754430251, -0.4946758370507742253 ) ) ;
#153061 = ORIENTED_EDGE ( 'NONE', *, *, #131422, .F. ) ;
#153062 = ORIENTED_EDGE ( 'NONE', *, *, #82220, .F. ) ;
#153063 = CARTESIAN_POINT ( 'NONE',  ( -5.413783410558481002, 5.210502155273325720, -0.7998128361456221525 ) ) ;
#153064 = CARTESIAN_POINT ( 'NONE',  ( -6.970863535720637216, 11.28442455831609337, 0.7998128361456481317 ) ) ;
#153065 = CARTESIAN_POINT ( 'NONE',  ( 4.969292227364340953, 0.1756445257206709631, -1.817221496977147854 ) ) ;
#153067 = CARTESIAN_POINT ( 'NONE',  ( -4.182100719528288657, 7.584231438125928371, -0.9338283797597360936 ) ) ;
#153066 = CARTESIAN_POINT ( 'NONE',  ( -5.427006627220116286, 9.553534508390610469, -0.7998128361456362523 ) ) ;
#153068 = CARTESIAN_POINT ( 'NONE',  ( 5.178155719255617129, 7.862379301422712352, -1.251444257556088457 ) ) ;
#153069 = CARTESIAN_POINT ( 'NONE',  ( 1.668881318695322413, -0.6185640615885504845, -1.619952590838618312 ) ) ;
#153070 = CARTESIAN_POINT ( 'NONE',  ( 0.6732859938517594678, -0.9703907760119870884, 1.444448127723398478 ) ) ;
#153071 = CARTESIAN_POINT ( 'NONE',  ( 5.531924057230363623, -1.459877215294088204, -1.787231782134098168 ) ) ;
#153072 = CARTESIAN_POINT ( 'NONE',  ( 4.065465959251388206, 5.836405933916976707, -1.599625672291269396 ) ) ;
#153073 = CARTESIAN_POINT ( 'NONE',  ( 1.440775599906311433, 0.3991536164789717955, 2.021572055866586837 ) ) ;
#153074 = CARTESIAN_POINT ( 'NONE',  ( 6.817052309572890323, 6.847649204123507083, 0.7998128361456341429 ) ) ;
#153075 = CARTESIAN_POINT ( 'NONE',  ( 0.5442957877539145173, 1.882187304385819493, -0.7230256762977352869 ) ) ;
#153076 = DIRECTION ( 'NONE',  ( -0.000000000000000000, -1.000000000000000000, -0.000000000000000000 ) ) ;
#153077 = CARTESIAN_POINT ( 'NONE',  ( -7.286581212701773502, 7.465709267765667789, 0.7998128361456341429 ) ) ;
#153078 = CARTESIAN_POINT ( 'NONE',  ( 0.2156151883831447236, -1.933912933822299784, 0.3821239771369787097 ) ) ;
#153081 = EDGE_CURVE ( 'NONE', #162407, #104139, #185636, .T. ) ;
#153080 = CARTESIAN_POINT ( 'NONE',  ( -5.008811405605897882, 4.808311159487113073, 0.7998128361456281477 ) ) ;
#153079 = CARTESIAN_POINT ( 'NONE',  ( 3.463059065379545221, -1.560675823418774533, 1.104941681961457256 ) ) ;
#153082 = CARTESIAN_POINT ( 'NONE',  ( 4.582781371344160526, -2.140174514510746029, -0.5380331057033281850 ) ) ;
#153083 = CARTESIAN_POINT ( 'NONE',  ( 1.224999999999951017, 2.166666667349502529, 0.7072540797572777205 ) ) ;
#153084 = CARTESIAN_POINT ( 'NONE',  ( -7.553300976144787349, 8.945177572657957654, -1.082531754730549967 ) ) ;
#153085 = CARTESIAN_POINT ( 'NONE',  ( 4.543390873910913896, 5.433615786718446472, 1.082531754730549078 ) ) ;
#153086 = CARTESIAN_POINT ( 'NONE',  ( -5.275531169048911728, 6.287779464379406491, -1.082531754730549967 ) ) ;
#153087 = CARTESIAN_POINT ( 'NONE',  ( 5.901066629635802308, -0.3109326959268610691, -2.097457242586676429 ) ) ;
#153088 = VERTEX_POINT ( 'NONE', #109573 ) ;
#153089 = EDGE_CURVE ( 'NONE', #164105, #21883, #177704, .T. ) ;
#153090 = CARTESIAN_POINT ( 'NONE',  ( 3.663348518144835086, -2.033753252616496532, -1.090341736564947484 ) ) ;
#153091 = CARTESIAN_POINT ( 'NONE',  ( 4.211346380768822506, -1.629847038978438079, -1.091715234301626314 ) ) ;
#153092 = CARTESIAN_POINT ( 'NONE',  ( -5.635349125135588721, 6.603604063193491136, 1.199719254218452935 ) ) ;
#153093 = CARTESIAN_POINT ( 'NONE',  ( 0.6550357524967264089, 1.634203043994170157, -1.084997510809107446 ) ) ;
#153094 = CARTESIAN_POINT ( 'NONE',  ( 8.856876352573948452, 14.66742331072540040, 8.031069393654634681 ) ) ;
#153095 = CARTESIAN_POINT ( 'NONE',  ( -9.421119845716953378, 15.43474195405156912, 7.432612891326888516 ) ) ;
#153096 = ORIENTED_EDGE ( 'NONE', *, *, #65958, .T. ) ;
#153097 = CARTESIAN_POINT ( 'NONE',  ( 6.315638730379727228, -1.320822524126588515, -1.523799118890494020 ) ) ;
#153098 = CARTESIAN_POINT ( 'NONE',  ( -7.323375529675950624, 11.69568855126397011, -0.7998128361456291469 ) ) ;
#153099 = DIRECTION ( 'NONE',  ( 1.000000000000000000, -0.000000000000000000, -0.000000000000000000 ) ) ;
#153100 = CARTESIAN_POINT ( 'NONE',  ( 3.274467656630496659, -1.066080149914239161, -1.891199154716957098 ) ) ;
#153101 = CARTESIAN_POINT ( 'NONE',  ( 4.366607992053101128, 7.252070536440704096, -1.199719254218448494 ) ) ;
#153102 = CARTESIAN_POINT ( 'NONE',  ( 0.8266187642571948269, -0.9586779626098644869, -1.891633453305548773 ) ) ;
#153103 = CARTESIAN_POINT ( 'NONE',  ( 0.7499999999999902300, 1.514583334016148086, 1.299038105676657340 ) ) ;
#153104 = CARTESIAN_POINT ( 'NONE',  ( 9.348510611822643313, 10.86534945433664134, 1.199719254218453823 ) ) ;
#153105 = CARTESIAN_POINT ( 'NONE',  ( 1.870725386045717142, 2.481143736744112704, 2.471938233550914354 ) ) ;
#153106 = CARTESIAN_POINT ( 'NONE',  ( 6.090086331970060662, 7.118959255344424086, 1.132899493623270359 ) ) ;
#153107 = ORIENTED_EDGE ( 'NONE', *, *, #73338, .F. ) ;
#153108 = CARTESIAN_POINT ( 'NONE',  ( 0.7025034608351670151, -0.6919086601019829308, -1.941309234904058600 ) ) ;
#153110 = CARTESIAN_POINT ( 'NONE',  ( -1.579999999999998073, 8.674529973577531194, -2.499999999999990230 ) ) ;
#153109 = CARTESIAN_POINT ( 'NONE',  ( -9.775592450653132204, 11.36361159963886891, -1.199719254218441611 ) ) ;
#153111 = CARTESIAN_POINT ( 'NONE',  ( 0.6823417656249899377, 1.842708333674752952, 1.181850606188755259 ) ) ;
#153112 = FILL_AREA_STYLE ('',( #122848 ) ) ;
#153113 = ORIENTED_EDGE ( 'NONE', *, *, #73338, .T. ) ;
#153114 = CARTESIAN_POINT ( 'NONE',  ( 4.459560945705238311, -1.480416612418914646, -1.210464771850598975 ) ) ;
#153115 =( GEOMETRIC_REPRESENTATION_CONTEXT ( 3 ) GLOBAL_UNCERTAINTY_ASSIGNED_CONTEXT ( ( #192988 ) ) GLOBAL_UNIT_ASSIGNED_CONTEXT ( ( #110478, #160225, #126742 ) ) REPRESENTATION_CONTEXT ( 'NONE', 'WORKASPACE' ) );
#153116 = CARTESIAN_POINT ( 'NONE',  ( 6.875920180786008196, 8.050936961452347163, -1.199719254218452047 ) ) ;
#153117 = AXIS2_PLACEMENT_3D ( 'NONE', #206362, #71007, #119858 ) ;
#153118 = CARTESIAN_POINT ( 'NONE',  ( -4.790108344329849110, 4.482881244673243337, 0.7998128361456341429 ) ) ;
#153119 = CARTESIAN_POINT ( 'NONE',  ( 0.1932431142802397694, 1.690279412936572134, -0.6521791651670250101 ) ) ;
#153121 = CARTESIAN_POINT ( 'NONE',  ( 0.7256311455483875905, 0.7733690622436960593, -1.752846625659326696 ) ) ;
#153120 = CARTESIAN_POINT ( 'NONE',  ( -6.486624235763164492, 6.835203243035253173, 0.7121179707554707861 ) ) ;
#153122 = CARTESIAN_POINT ( 'NONE',  ( 1.592325325408463055, 1.022198633559557646, -1.800363622228560168 ) ) ;
#153123 = CARTESIAN_POINT ( 'NONE',  ( -1.364683531250014514, 0.09270833367475767028, 0.7879004041258379498 ) ) ;
#153124 = CARTESIAN_POINT ( 'NONE',  ( 0.9539096209374531288, 1.969307747869667446, -0.09461285551524113713 ) ) ;
#153125 = CARTESIAN_POINT ( 'NONE',  ( 3.281694405262673087, 1.158851912627656189, 1.410738560442346801 ) ) ;
#153127 = CARTESIAN_POINT ( 'NONE',  ( 5.590372323399994237, 7.390087136190794936, 1.241407824010079652 ) ) ;
#153126 = CARTESIAN_POINT ( 'NONE',  ( 6.305322857734435793, 1.832379230283949667, 1.229636283518860118 ) ) ;
#153128 = CARTESIAN_POINT ( 'NONE',  ( 0.6823417656249882723, 0.6760416670080898749, -1.181850606188749264 ) ) ;
#153129 = CARTESIAN_POINT ( 'NONE',  ( 4.281722439037777050, -1.974808133235542495, 0.5956899724020509046 ) ) ;
#153130 = CARTESIAN_POINT ( 'NONE',  ( -5.605406444246153974, 8.627059054007450101, -1.199719254218440723 ) ) ;
#153131 = CARTESIAN_POINT ( 'NONE',  ( 8.101160479365381306, 9.410107633136481908, -1.199719254218446718 ) ) ;
#153132 = CARTESIAN_POINT ( 'NONE',  ( -1.734723475976807094E-15, 2.999999999999988898, -6.938893903907228378E-15 ) ) ;
#153133 = CARTESIAN_POINT ( 'NONE',  ( 5.168682875307768931, 7.053215992657626110, -1.599625672291256295 ) ) ;
#153135 = CARTESIAN_POINT ( 'NONE',  ( 0.7499999999999902300, 3.483333333333352044, 1.299038105676669330 ) ) ;
#153134 = CARTESIAN_POINT ( 'NONE',  ( 5.227606396355295892, -2.000638224736817516, 0.6578950869102012655 ) ) ;
#153136 = CARTESIAN_POINT ( 'NONE',  ( 6.250451049865752395, -2.060019788584551481, -0.2068627631737207651 ) ) ;
#153137 = CARTESIAN_POINT ( 'NONE',  ( 1.364683531249988757, 1.196875000341421469, 0.000000000000000000 ) ) ;
#153138 = CARTESIAN_POINT ( 'NONE',  ( 3.585389192675687564, 1.955840111083558597, -0.9206723451176119788 ) ) ;
#153139 = CARTESIAN_POINT ( 'NONE',  ( 4.670572394037289854, 0.7749771354828223213, 1.865277368486473630 ) ) ;
#153142 = CARTESIAN_POINT ( 'NONE',  ( 4.853455804012212660, 7.645820290447483458, 1.082531754730558626 ) ) ;
#153141 = CARTESIAN_POINT ( 'NONE',  ( 3.285556943750000070, -3.434374999522042060, 0.000000000000000000 ) ) ;
#153140 = CARTESIAN_POINT ( 'NONE',  ( -0.6124999999999967137, 1.541666666666677177, 1.060881119635903147 ) ) ;
#153143 = CARTESIAN_POINT ( 'NONE',  ( -4.457598643843001973, 8.422558527783969851, 0.000000000000000000 ) ) ;
#153144 = CARTESIAN_POINT ( 'NONE',  ( 2.606657977298726614, 1.900416011228076130, 0.6748465934659984011 ) ) ;
#153145 = CARTESIAN_POINT ( 'NONE',  ( -8.178592977541617515, 10.56477777859713463, 1.599625672291295375 ) ) ;
#153147 = CARTESIAN_POINT ( 'NONE',  ( -11.92619526913699879, 12.69999999999998153, 1.328859060402684644 ) ) ;
#153146 = CARTESIAN_POINT ( 'NONE',  ( -4.440459003675619520, 5.139289244831666714, 1.199719254218462483 ) ) ;
#153148 = CARTESIAN_POINT ( 'NONE',  ( 7.032126278729658786, 15.00000000000000000, -9.944928355699694578 ) ) ;
#153149 = CARTESIAN_POINT ( 'NONE',  ( -11.88237951145550575, 11.25680652621284494, 0.9087114598430686696 ) ) ;
#153150 = PLANE ( 'NONE',  #118730 ) ;
#153152 = CARTESIAN_POINT ( 'NONE',  ( 4.359000025081374297, -0.002827702239943663542, -2.016598147179492262 ) ) ;
#153151 = CARTESIAN_POINT ( 'NONE',  ( -7.280365300414089802, 10.47721470291632784, 1.082531754730549967 ) ) ;
#153153 = CARTESIAN_POINT ( 'NONE',  ( 0.7499999999999920064, 5.733333333333353821, 1.299038105676669330 ) ) ;
#153154 = CARTESIAN_POINT ( 'NONE',  ( -1.364683531250014514, 14.90104166700806410, -0.7879004041258335089 ) ) ;
#153155 = CARTESIAN_POINT ( 'NONE',  ( 6.159189016523521687, -1.482050057771692186, -0.8820200739605223994 ) ) ;
#153156 = CARTESIAN_POINT ( 'NONE',  ( 4.701645408888975197, 8.707279753670952971, 0.000000000000000000 ) ) ;
#153158 = CARTESIAN_POINT ( 'NONE',  ( 5.969332771766739931, 10.18624834369502885, -0.7998128361456481317 ) ) ;
#153157 = CARTESIAN_POINT ( 'NONE',  ( 8.758204044747998296, 11.24099069033793974, 1.443375672974076540 ) ) ;
#153159 = CARTESIAN_POINT ( 'NONE',  ( -11.08179121629665786, 7.064944825185786037, 4.608651903429358043 ) ) ;
#153160 = CARTESIAN_POINT ( 'NONE',  ( 5.975831987570860981, 1.113884111790110820, 1.502598383168303409 ) ) ;
#153161 = CARTESIAN_POINT ( 'NONE',  ( -0.07552757677437360595, -0.8618087116909570744, -1.817275918844815541 ) ) ;
#153162 = PRESENTATION_STYLE_ASSIGNMENT (( #198688 ) ) ;
#153163 = CARTESIAN_POINT ( 'NONE',  ( -1.451998047840333594, 7.315968950356099398, -4.301760722582879559 ) ) ;
#153164 = VERTEX_POINT ( 'NONE', #79120 ) ;
#153165 = CARTESIAN_POINT ( 'NONE',  ( 9.612367721964607981, 12.23751498042398289, -1.443375672974058777 ) ) ;
#153166 = CARTESIAN_POINT ( 'NONE',  ( 0.8785300617164050196, -0.4926655378557908138, -1.955167820405806056 ) ) ;
#153167 = CARTESIAN_POINT ( 'NONE',  ( 3.079110283634975964, 6.606396074300548982, 0.7216878364870257245 ) ) ;
#153168 = CARTESIAN_POINT ( 'NONE',  ( -10.50000000000000000, 10.90000000000000036, -3.600000000000002309 ) ) ;
#153169 = CARTESIAN_POINT ( 'NONE',  ( 8.744645890689993095, 9.304434415334227992, -0.7216878364870197293 ) ) ;
#153170 = CARTESIAN_POINT ( 'NONE',  ( 5.991813822235618758, 9.077867661661846554, 1.199719254218462483 ) ) ;
#153171 = PRESENTATION_LAYER_ASSIGNMENT (  '', '', ( #21717 ) ) ;
#153173 = CARTESIAN_POINT ( 'NONE',  ( 5.976186790766067958, -1.906884764771042517, -0.1824196792480689000 ) ) ;
#153172 = CARTESIAN_POINT ( 'NONE',  ( -5.473741331615264549, 7.409117525016355010, -1.599625672291256295 ) ) ;
#153174 = CIRCLE ( 'NONE', #163550, 1.249999999999999778 ) ;
#153175 = CARTESIAN_POINT ( 'NONE',  ( 1.921775512840651956, 9.000000000008071765, 0.7750000000000004663 ) ) ;
#153176 = CARTESIAN_POINT ( 'NONE',  ( 1.154700538379228147, -4.295408888568413630, -1.734723475976807094E-15 ) ) ;
#153177 = CARTESIAN_POINT ( 'NONE',  ( 1.408750476333324952, 7.229967155398369982, 4.273289540531094666 ) ) ;
#153179 = ORIENTED_EDGE ( 'NONE', *, *, #108300, .T. ) ;
#153178 = CARTESIAN_POINT ( 'NONE',  ( 2.385871846325007706, 5.727341554113725586, -0.7216878364870267237 ) ) ;
#153180 = CARTESIAN_POINT ( 'NONE',  ( -2.598358995313378550, 6.183169261174235487, 0.7998128361456341429 ) ) ;
#153181 = CARTESIAN_POINT ( 'NONE',  ( 2.553791647773369089, 0.5774160426356907960, -2.083079400968433248 ) ) ;
#153182 = CARTESIAN_POINT ( 'NONE',  ( -6.400857919427531684, 9.521399101757175742, 1.082531754730549967 ) ) ;
#153183 = CARTESIAN_POINT ( 'NONE',  ( 5.722950238744198614, 8.730506807626655430, 1.082531754730549967 ) ) ;
#153184 = CARTESIAN_POINT ( 'NONE',  ( 0.4047333657465709278, -2.105317319661216047, -0.2534319464195868843 ) ) ;
#153185 = CARTESIAN_POINT ( 'NONE',  ( 5.596661130663158623, -0.4455768995972574364, -1.770251349769519367 ) ) ;
#153186 = AXIS2_PLACEMENT_3D ( 'NONE', #34716, #71467, #99730 ) ;
#153187 = CARTESIAN_POINT ( 'NONE',  ( 1.897670943237000918, -0.6677869454260307869, 1.854917580456706183 ) ) ;
#153188 = CARTESIAN_POINT ( 'NONE',  ( 4.799029005866479736, -0.2398712174674077491, -1.897248949554980024 ) ) ;
#153189 = ORIENTED_EDGE ( 'NONE', *, *, #30238, .F. ) ;
#153190 = CARTESIAN_POINT ( 'NONE',  ( -4.370663978927099791, 5.060324124126027279, 7.500000000000000000 ) ) ;
#153191 = CARTESIAN_POINT ( 'NONE',  ( 5.441845355777640059, 1.321472782793672085, 1.460616519443626249 ) ) ;
#153192 = CARTESIAN_POINT ( 'NONE',  ( 0.09355730106928944467, -1.941490229121365374, -0.04880333718709597285 ) ) ;
#153193 = ORIENTED_EDGE ( 'NONE', *, *, #7856, .F. ) ;
#153194 = CARTESIAN_POINT ( 'NONE',  ( -4.659162064951642535, 5.464719159645540003, 1.199719254218452935 ) ) ;
#153196 = CARTESIAN_POINT ( 'NONE',  ( -0.3776192402222742217, 3.049641483663600106, 0.4287046358292067039 ) ) ;
#153195 = CARTESIAN_POINT ( 'NONE',  ( -6.116136693540540570, 10.14959355252370266, 0.000000000000000000 ) ) ;
#153198 = CARTESIAN_POINT ( 'NONE',  ( 5.194182247366868843, 8.113610817686430110, 1.082531754730548412 ) ) ;
#153197 = CARTESIAN_POINT ( 'NONE',  ( 6.272618624616828953, 10.46980549536166016, 1.040834085586084257E-14 ) ) ;
#153200 = ORIENTED_EDGE ( 'NONE', *, *, #40921, .F. ) ;
#153199 = CARTESIAN_POINT ( 'NONE',  ( 5.443983014310386892, -1.216401775450553169, -1.475513148251464068 ) ) ;
#153202 = EDGE_CURVE ( 'NONE', #3975, #59123, #110632, .T. ) ;
#153201 = AXIS2_PLACEMENT_3D ( 'NONE', #69541, #82609, #32807 ) ;
#153203 = CARTESIAN_POINT ( 'NONE',  ( 1.061882456046374434, 0.4290601450722114074, -2.164491299336705588 ) ) ;
#153204 = CARTESIAN_POINT ( 'NONE',  ( -5.570361349191150779, 5.866663122702686195, 0.5491554309224304653 ) ) ;
#153205 = CARTESIAN_POINT ( 'NONE',  ( 6.463545146426397991, -1.618288576614915764, -1.197193900782191234 ) ) ;
#153206 = CARTESIAN_POINT ( 'NONE',  ( -0.4019237886466871523, 8.698664549684629321, -1.499999999999998668 ) ) ;
#153207 = CARTESIAN_POINT ( 'NONE',  ( 1.255262969126037241E-15, 12.31951671548121219, -10.25000000000000000 ) ) ;
#153208 = DIRECTION ( 'NONE',  ( -5.828670879282089587E-16, 0.8656921114426507913, -0.5005768354468322912 ) ) ;
#153209 = CARTESIAN_POINT ( 'NONE',  ( 2.928250347896840022, 1.105370970781336837, 1.750397071514836478 ) ) ;
#153210 = CARTESIAN_POINT ( 'NONE',  ( -4.089755892816631544, 7.923132308261379819, -0.7998128361456281477 ) ) ;
#153211 = CARTESIAN_POINT ( 'NONE',  ( -4.624779211906307808, 8.357533986720639518, 0.2900094174717957607 ) ) ;
#153213 = CARTESIAN_POINT ( 'NONE',  ( 1.077287230265553397, -0.05381693868444264311, -2.161191418701657430 ) ) ;
#153212 = CARTESIAN_POINT ( 'NONE',  ( -5.413783410558481002, 5.210502155273325720, -0.7998128361456221525 ) ) ;
#153214 = CARTESIAN_POINT ( 'NONE',  ( -1.154700538379266339, -4.295408888568413630, 2.602085213965210642E-15 ) ) ;
#153215 = EDGE_CURVE ( 'NONE', #65129, #103298, #210232, .T. ) ;
#153216 = DIRECTION ( 'NONE',  ( 1.000000000000000000, 3.451266460341926649E-31, 8.638326563840810896E-31 ) ) ;
#153217 = CARTESIAN_POINT ( 'NONE',  ( -1.364683531250010295, 12.69270833367473550, 0.7879004041258445001 ) ) ;
#153219 = CARTESIAN_POINT ( 'NONE',  ( -5.926849427829407269, 6.943687749669614995, -1.199719254218453823 ) ) ;
#153218 = CARTESIAN_POINT ( 'NONE',  ( 6.925078400183562799, 2.053856789352814793, 2.261525409452989965 ) ) ;
#153220 = CARTESIAN_POINT ( 'NONE',  ( 5.959525138608227302, -1.649545596257080637, -0.5353374286216765476 ) ) ;
#153221 = CARTESIAN_POINT ( 'NONE',  ( -2.415323921528888196, 5.969628341758991930, 0.7998128361456341429 ) ) ;
#153222 = CARTESIAN_POINT ( 'NONE',  ( 3.151297481648129395, 1.777980080355131109, -1.060267355625019503 ) ) ;
#153223 = CARTESIAN_POINT ( 'NONE',  ( 4.816069135992575134, 1.087346734782314472, -1.816536155142484121 ) ) ;
#153224 = CARTESIAN_POINT ( 'NONE',  ( 7.124973419181436007, 8.271222729588529887, -1.199719254218446718 ) ) ;
#153225 = CARTESIAN_POINT ( 'NONE',  ( -1.364683531249997417, 4.759375000341424133, 1.214306433183764966E-14 ) ) ;
#153226 = CARTESIAN_POINT ( 'NONE',  ( 2.360148646665951144, -1.969129416856093551, 0.04326586078102003657 ) ) ;
#153227 = CARTESIAN_POINT ( 'NONE',  ( 1.142663480069527671, 1.843847066288730074, 0.5072560978593986247 ) ) ;
#153228 = CARTESIAN_POINT ( 'NONE',  ( 4.453268702153020620, 0.5046191974597475927, -2.235886964606835559 ) ) ;
#153229 = CARTESIAN_POINT ( 'NONE',  ( 2.297230901563730665, 1.410920830412419003, 1.158640757216542028 ) ) ;
#153230 = CARTESIAN_POINT ( 'NONE',  ( 4.206772801990143584, 8.129928378955675328, 0.7998128361456271485 ) ) ;
#153231 = CARTESIAN_POINT ( 'NONE',  ( 4.595850884908202261, 7.345281218159464665, -1.082531754730549078 ) ) ;
#153232 = CARTESIAN_POINT ( 'NONE',  ( -6.509886312855995172, 10.74661779830734254, -0.7998128361456291469 ) ) ;
#153233 = CARTESIAN_POINT ( 'NONE',  ( 3.304942742240731590, -0.3968801077466362903, -1.973537420673168397 ) ) ;
#153234 = CARTESIAN_POINT ( 'NONE',  ( 3.274216958324972726, -0.9628348462043828659, -1.709115330885315087 ) ) ;
#153235 = CARTESIAN_POINT ( 'NONE',  ( -6.886651960737580680, 10.12184548991413457, -1.199719254218440723 ) ) ;
#153236 = CARTESIAN_POINT ( 'NONE',  ( -4.550733115681270036, 8.460939068270139529, 0.7998128361456481317 ) ) ;
#153237 = CARTESIAN_POINT ( 'NONE',  ( 0.07536363704235825300, -0.001874865094115065866, -2.144269471569634433 ) ) ;
#153239 = CARTESIAN_POINT ( 'NONE',  ( 4.926482082969720899, 1.694141084728201907, 0.5120089106541975132 ) ) ;
#153238 = CARTESIAN_POINT ( 'NONE',  ( 6.685487044060022477, -0.8959250478542144513, 1.887356362924677233 ) ) ;
#153240 = CARTESIAN_POINT ( 'NONE',  ( 0.6916816545035618935, -0.7852976098030055585, 2.046091368998310678 ) ) ;
#153241 = CARTESIAN_POINT ( 'NONE',  ( 6.527322169609689695, -1.143008000885838760, -1.312471774050189444 ) ) ;
#153242 = CARTESIAN_POINT ( 'NONE',  ( 8.125414133291656071, 8.374071331795406081, -0.7998128361456291469 ) ) ;
#153243 = CARTESIAN_POINT ( 'NONE',  ( 0.1331715793776314105, 6.947497095909970000, -2.548608419791003055 ) ) ;
#153244 = CARTESIAN_POINT ( 'NONE',  ( 1.159977488309314797, -0.5597072352675269702, -2.229110579909891143 ) ) ;
#153245 = CARTESIAN_POINT ( 'NONE',  ( 0.8553300576445364012, 0.4222666777726029608, -2.150330908352434012 ) ) ;
#153246 = CARTESIAN_POINT ( 'NONE',  ( 3.510573375967055654, -0.8941257848905452832, -2.017821460644920073 ) ) ;
#153247 = AXIS2_PLACEMENT_3D ( 'NONE', #42116, #90862, #174253 ) ;
#153248 = CARTESIAN_POINT ( 'NONE',  ( 0.2393977111345606534, -0.1477851991248577135, -2.137246755706405210 ) ) ;
#153249 = DIRECTION ( 'NONE',  ( 1.000000000000000000, -7.387867266669436732E-31, 0.000000000000000000 ) ) ;
#153250 = CARTESIAN_POINT ( 'NONE',  ( 1.218125882790439762, 1.038422275552937757, -1.845119264165562711 ) ) ;
#153251 = CARTESIAN_POINT ( 'NONE',  ( 3.562500000000002665, -1.451031289061261109, -1.451031289060973561 ) ) ;
#153252 = DIRECTION ( 'NONE',  ( 5.551115123125765446E-17, 0.000000000000000000, -1.000000000000000000 ) ) ;
#153253 = CARTESIAN_POINT ( 'NONE',  ( 5.174797004712035076, -1.813887718507047220, -0.6490126392820031453 ) ) ;
#153254 = ORIENTED_EDGE ( 'NONE', *, *, #137619, .T. ) ;
#153256 = CARTESIAN_POINT ( 'NONE',  ( 1.364683531249986537, -0.7822916663252464931, -0.7879004041258309554 ) ) ;
#153255 = CARTESIAN_POINT ( 'NONE',  ( 1.505871038028598230, -2.274393761632488964, 0.2862045095256612326 ) ) ;
#153257 = CARTESIAN_POINT ( 'NONE',  ( 3.161022370280501814, 6.839609865302569425, 0.000000000000000000 ) ) ;
#153258 = CARTESIAN_POINT ( 'NONE',  ( 5.819474248763732760, 7.812472595022922128, -1.599625672291262513 ) ) ;
#153259 = CARTESIAN_POINT ( 'NONE',  ( 3.405137934272496558, -0.4347481476216079055, -2.178183672434565565 ) ) ;
#153260 = CARTESIAN_POINT ( 'NONE',  ( -8.351459436338041442, 9.806086099558291025, -1.082531754730543971 ) ) ;
#153261 = DIRECTION ( 'NONE',  ( 0.000000000000000000, 1.000000000000000000, 0.000000000000000000 ) ) ;
#153262 = CARTESIAN_POINT ( 'NONE',  ( 5.260200412422194383, 7.159986452624450770, -1.443375672974051449 ) ) ;
#153263 = CARTESIAN_POINT ( 'NONE',  ( -8.473482818416675499, 9.948446711983361723, -1.082531754730543083 ) ) ;
#153264 = CARTESIAN_POINT ( 'NONE',  ( 6.373741612200171325, 7.569024981389272710, 1.082531754730549967 ) ) ;
#153265 = ORIENTED_EDGE ( 'NONE', *, *, #190444, .T. ) ;
#153266 = CARTESIAN_POINT ( 'NONE',  ( 1.459611520199757706, -1.915600648959712382, -0.6298732728240025169 ) ) ;
#153268 = CARTESIAN_POINT ( 'NONE',  ( 6.619587925713169341, 0.3565228922877783924, -2.031493691534612012 ) ) ;
#153267 = CARTESIAN_POINT ( 'NONE',  ( 8.158255747121103241, 10.54105100977322174, 1.599625672291281386 ) ) ;
#153269 = CARTESIAN_POINT ( 'NONE',  ( 4.855228407025239612, 8.678533884922511987, 0.000000000000000000 ) ) ;
#153270 = CARTESIAN_POINT ( 'NONE',  ( 6.093256065386793985, -0.5776499228958801302, 1.641946315008017576 ) ) ;
#153271 = FACE_OUTER_BOUND ( 'NONE', #102508, .T. ) ;
#153272 = CARTESIAN_POINT ( 'NONE',  ( 1.364683531249986537, 2.155208333674751398, -0.7879004041258239610 ) ) ;
#153273 = CARTESIAN_POINT ( 'NONE',  ( 1.194210174654856127, -0.4229520329555501723, -1.718335688698314101 ) ) ;
#153274 = CARTESIAN_POINT ( 'NONE',  ( 1.494767762416524093, -2.000856930885573259, 0.2496086726550551249 ) ) ;
#153275 = CARTESIAN_POINT ( 'NONE',  ( 0.2394788589213901198, 1.836227513651207177, 0.1364553164684492448 ) ) ;
#153276 = CARTESIAN_POINT ( 'NONE',  ( 4.177453601039508690, 1.497175104222212783, 1.735980874517801587 ) ) ;
#153277 = CARTESIAN_POINT ( 'NONE',  ( 3.433393508698717511, 0.8267853122289525736, -1.645126075773599039 ) ) ;
#153278 = EDGE_CURVE ( 'NONE', #198335, #108029, #145235, .T. ) ;
#153279 = CARTESIAN_POINT ( 'NONE',  ( 9.257519960032755790, 9.694861462993381807, 0.7998128361456462443 ) ) ;
#153280 =( NAMED_UNIT ( * ) PLANE_ANGLE_UNIT ( ) SI_UNIT ( $, .RADIAN. ) );
#153281 = CARTESIAN_POINT ( 'NONE',  ( 4.594645031659345236, -0.4005623417570289280, -1.780931357837008733 ) ) ;
#153282 = CARTESIAN_POINT ( 'NONE',  ( 4.957657809308734898, -1.899617967926207740, -0.6767155953601932117 ) ) ;
#153283 = CARTESIAN_POINT ( 'NONE',  ( -7.506410603460441422, 11.90922947067921278, -0.7998128361456291469 ) ) ;
#153285 = CARTESIAN_POINT ( 'NONE',  ( -7.469616286486262524, 7.679250187180907794, 0.7998128361456341429 ) ) ;
#153284 = CARTESIAN_POINT ( 'NONE',  ( 2.958202477073975878, 2.251720482184274008, -0.2206431264100849887 ) ) ;
#153286 = CARTESIAN_POINT ( 'NONE',  ( 6.001026715709635972, 1.723673884808615497, -1.209685691799726737 ) ) ;
#153287 = FACE_OUTER_BOUND ( 'NONE', #5704, .T. ) ;
#153288 = CARTESIAN_POINT ( 'NONE',  ( 3.068866956829822801, 1.501395149897828851, -1.425812640530661479 ) ) ;
#153289 = CARTESIAN_POINT ( 'NONE',  ( 2.205172540517054802, 5.724451730578533848, 1.040834085586084257E-14 ) ) ;
#153290 = CARTESIAN_POINT ( 'NONE',  ( 0.6801582343749883464, 1.505208333674713739, 1.178068619123805227 ) ) ;
#153291 = CARTESIAN_POINT ( 'NONE',  ( 5.901066629635801419, -0.3109326959268611246, -2.097457242586676429 ) ) ;
#153293 = CARTESIAN_POINT ( 'NONE',  ( 2.227063406323766870, -8.064668077616128736E-05, 1.926676517253867793 ) ) ;
#153292 = CARTESIAN_POINT ( 'NONE',  ( -8.748035429315585532, 11.22912730566677553, -1.599625672291263179 ) ) ;
#153294 = UNCERTAINTY_MEASURE_WITH_UNIT (LENGTH_MEASURE( 1.000000000000000082E-05 ), #105235, 'distance_accuracy_value', 'NONE');
#153295 = FACE_BOUND ( 'NONE', #212277, .T. ) ;
#153296 = CARTESIAN_POINT ( 'NONE',  ( 6.385607329849364078, -1.855618941174362879, 0.6602924305801564087 ) ) ;
#153297 = CARTESIAN_POINT ( 'NONE',  ( 5.356880090730874677, 5.422317325373725794, 0.7216878364870328300 ) ) ;
#153298 = CARTESIAN_POINT ( 'NONE',  ( 5.568360837313221623, 6.179671487343128433, 0.8958872440008452953 ) ) ;
#153299 = DIRECTION ( 'NONE',  ( 0.000000000000000000, -1.000000000000000000, 0.000000000000000000 ) ) ;
#153300 = CARTESIAN_POINT ( 'NONE',  ( -3.418627288940168096, 7.140148937072163804, -0.7998128361456281477 ) ) ;
#153301 = CARTESIAN_POINT ( 'NONE',  ( 0.8443251495477720470, -1.414827328263716266, -1.712562173056450643 ) ) ;
#153302 = AXIS2_PLACEMENT_3D ( 'NONE', #52774, #54919, #118911 ) ;
#153303 = CARTESIAN_POINT ( 'NONE',  ( 3.487430266828908998, 1.904693919176775552, -0.8987260315082377105 ) ) ;
#153304 = CARTESIAN_POINT ( 'NONE',  ( -5.517242166118370150, 5.401480380085008193, 0.7998128361456281477 ) ) ;
#153305 = CARTESIAN_POINT ( 'NONE',  ( 7.100719765255169236, 9.307259030929609267, -1.599625672291262513 ) ) ;
#153306 = CARTESIAN_POINT ( 'NONE',  ( 0.7306206827372868640, -1.750454575335522067, -0.6323700682324316924 ) ) ;
#153307 = CARTESIAN_POINT ( 'NONE',  ( 6.154511665599609493, 9.267681812253174556, 1.199719254218462483 ) ) ;
#153308 = EDGE_CURVE ( 'NONE', #121817, #47282, #186112, .T. ) ;
#153309 = CARTESIAN_POINT ( 'NONE',  ( 6.010342169559767633, 5.906487374108181143, -0.7998128361456281477 ) ) ;
#153310 = CARTESIAN_POINT ( 'NONE',  ( -5.451787166470911217, 9.374519104275787384, 0.7216878364870267237 ) ) ;
#153311 = CARTESIAN_POINT ( 'NONE',  ( -7.863365906246061243, 10.19701286208565705, -1.443375672974059665 ) ) ;
#153312 = CARTESIAN_POINT ( 'NONE',  ( 0.7387272492362946252, 1.258454933865692293, -1.706699550108881080 ) ) ;
#153313 = CARTESIAN_POINT ( 'NONE',  ( -5.589704470584107909, 9.743348658981940247, -0.7998128361456362523 ) ) ;
#153315 = CARTESIAN_POINT ( 'NONE',  ( 4.826587731031282580, -1.282962940432516907, 1.484285152025546672 ) ) ;
#153314 = CARTESIAN_POINT ( 'NONE',  ( 0.6124999999999862776, 1.083333333333352799, 1.060881119635887604 ) ) ;
#153316 = CARTESIAN_POINT ( 'NONE',  ( 2.413140945657660907, 1.930630709398067246, 0.9725960170764782475 ) ) ;
#153317 = CARTESIAN_POINT ( 'NONE',  ( 1.557894219809667247, -1.301531972126177772, 1.302644501960325885 ) ) ;
#153319 = CARTESIAN_POINT ( 'NONE',  ( -4.989408424308831691, 6.622959204541034595, -1.241733208710007696 ) ) ;
#153318 = CARTESIAN_POINT ( 'NONE',  ( -2.173285075505815599E-15, -8.011313137147263674, 11.00000000000000178 ) ) ;
#153320 = CARTESIAN_POINT ( 'NONE',  ( 3.591523995615089948, -1.738451970352115961, -0.08344189160913899339 ) ) ;
#153321 = CARTESIAN_POINT ( 'NONE',  ( -9.898321827453750998, 15.00000000001253753, -7.924999999985899990 ) ) ;
#153322 = CARTESIAN_POINT ( 'NONE',  ( 5.016153647376205171, 6.875265226737464985, 1.443375672974062551 ) ) ;
#153323 = CARTESIAN_POINT ( 'NONE',  ( -11.41048919578708443, 9.369870944694024928, -1.242167297096143264 ) ) ;
#153324 = CARTESIAN_POINT ( 'NONE',  ( 1.217891636700708435, -2.108894920778502602, 0.4742063263511315796 ) ) ;
#153325 = MECHANICAL_DESIGN_GEOMETRIC_PRESENTATION_REPRESENTATION (  '', ( #35651 ), #84054 ) ;
#153326 = CARTESIAN_POINT ( 'NONE',  ( 3.550157523342875709, 1.823840110401256931, -0.8594984857327039318 ) ) ;
#153327 = CARTESIAN_POINT ( 'NONE',  ( -10.15469386651127515, 11.90985960142705657, 1.082531754730558626 ) ) ;
#153329 = CIRCLE ( 'NONE', #115365, 0.08000000000000012657 ) ;
#153328 = CARTESIAN_POINT ( 'NONE',  ( 0.1808504484964272296, -2.097240537080494516, -0.5235256853268267507 ) ) ;
#153330 = CARTESIAN_POINT ( 'NONE',  ( 3.080892710809614243, -0.1436740641204778401, -1.966277672030048107 ) ) ;
#153331 = CARTESIAN_POINT ( 'NONE',  ( 6.609000000000036401, 7.629137130509092479, 2.600000000000000977 ) ) ;
#153332 = CARTESIAN_POINT ( 'NONE',  ( 2.226030366740273880, 1.884328139559983573, 0.4695921692644353107 ) ) ;
#153336 = ORIENTED_EDGE ( 'NONE', *, *, #202203, .T. ) ;
#153335 = EDGE_CURVE ( 'NONE', #70036, #137942, #210719, .T. ) ;
#153334 = CARTESIAN_POINT ( 'NONE',  ( -3.662110889467009578, 7.286563447771212232, 0.7216878364870338292 ) ) ;
#153333 = LINE ( 'NONE', #89419, #101375 ) ;
#153337 = CARTESIAN_POINT ( 'NONE',  ( -4.624739795592936353, 7.449261290616792763, -1.082531754730549967 ) ) ;
#153338 = CARTESIAN_POINT ( 'NONE',  ( -0.1108833634137010027, 1.377173795795206157, -2.152720132533674668 ) ) ;
#153339 = CARTESIAN_POINT ( 'NONE',  ( 4.441177836928239309, 7.339068688795062911, 1.199719254218452047 ) ) ;
#153340 = CARTESIAN_POINT ( 'NONE',  ( -5.167592825464113915, 6.057888380243431570, 1.199719254218452935 ) ) ;
#153341 = CARTESIAN_POINT ( 'NONE',  ( -5.094831863685302942, 9.165997284266655498, 0.7998128361456291469 ) ) ;
#153342 = CARTESIAN_POINT ( 'NONE',  ( -8.771762197917311710, 13.17754696430482042, 0.7216878364870317197 ) ) ;
#153343 = EDGE_CURVE ( 'NONE', #121123, #91407, #2098, .T. ) ;
#153344 = CARTESIAN_POINT ( 'NONE',  ( 6.545943480548680249, 0.8917086005404940563, -2.128542236993334669 ) ) ;
#153345 = CARTESIAN_POINT ( 'NONE',  ( 6.584431417889404337, 1.130572321132311098, -1.603143135845342515 ) ) ;
#153346 = AXIS2_PLACEMENT_3D ( 'NONE', #106781, #124138, #137106 ) ;
#153347 = CARTESIAN_POINT ( 'NONE',  ( 3.836726278109466204, -1.889416792123297162, -0.5274722977551549175 ) ) ;
#153348 = CARTESIAN_POINT ( 'NONE',  ( 8.932124273304774320, 9.315233161810734686, 0.7998128361456462443 ) ) ;
#153349 = CARTESIAN_POINT ( 'NONE',  ( 1.635388916632842360, 0.6352005984417673501, 1.913803229121699534 ) ) ;
#153350 = ORIENTED_EDGE ( 'NONE', *, *, #174069, .F. ) ;
#153351 = CARTESIAN_POINT ( 'NONE',  ( 2.448581487809509571, -1.456371601587917120, 1.537162028231451538 ) ) ;
#153352 = CARTESIAN_POINT ( 'NONE',  ( 0.7499999999999902300, 1.764583334016148086, 1.299038105676657340 ) ) ;
#153354 = CARTESIAN_POINT ( 'NONE',  ( -5.636439174979254396, 7.598931675607687453, -1.599625672291256295 ) ) ;
#153353 = CARTESIAN_POINT ( 'NONE',  ( -10.18278199833531517, 3.974415841077576950, 5.432519183637573690 ) ) ;
#153355 = CARTESIAN_POINT ( 'NONE',  ( 3.661895226921572100, -1.235415792305821103, 1.365283978338522441 ) ) ;
#153356 = ORIENTED_EDGE ( 'NONE', *, *, #214235, .F. ) ;
#153357 = CARTESIAN_POINT ( 'NONE',  ( -9.484092147959342967, 11.02352791316275216, 1.199719254218462483 ) ) ;
#153358 = CARTESIAN_POINT ( 'NONE',  ( 7.013428937081386927, 5.939655416065874327, 2.436399677959149468 ) ) ;
#153359 = CARTESIAN_POINT ( 'NONE',  ( 3.849942018323779358, -1.464806807754112539, -1.533599281611098597 ) ) ;
#153360 = CARTESIAN_POINT ( 'NONE',  ( -10.20626665084797580, 3.700502905159950728, -5.921468070729088318 ) ) ;
#153361 = CARTESIAN_POINT ( 'NONE',  ( 6.154511665599609493, 9.267681812253174556, 1.199719254218462483 ) ) ;
#153362 = CARTESIAN_POINT ( 'NONE',  ( 5.764934849280819229, -1.861221615537820728, -0.8850300128313455250 ) ) ;
#153364 = CARTESIAN_POINT ( 'NONE',  ( 2.577489280727011778, -0.9446877197298314544, 1.580272903027237774 ) ) ;
#153363 = CARTESIAN_POINT ( 'NONE',  ( -7.552055258011950656, 8.769484874890757453, 1.199719254218462483 ) ) ;
#153365 = CARTESIAN_POINT ( 'NONE',  ( 8.235688245297327015, 11.69572115523387268, -1.199719254218446718 ) ) ;
#153366 = CARTESIAN_POINT ( 'NONE',  ( -0.6823417656249969321, 5.717708333674756283, -1.181850606188749264 ) ) ;
#153367 = CARTESIAN_POINT ( 'NONE',  ( 3.094081423030320538E-15, 0.2401923788623722134, -11.09999999999959819 ) ) ;
#153368 = FACE_OUTER_BOUND ( 'NONE', #8000, .T. ) ;
#153369 = CARTESIAN_POINT ( 'NONE',  ( 10.99529341469513533, -7.794776013890245991, -0.3288329489799977634 ) ) ;
#153370 = CARTESIAN_POINT ( 'NONE',  ( 2.157103830005083100, -1.704838622333640030, 1.401371054633032909 ) ) ;
#153371 = CARTESIAN_POINT ( 'NONE',  ( 3.866728509311831985, -1.522874988181441180, 1.673262526929709670 ) ) ;
#153372 = CARTESIAN_POINT ( 'NONE',  ( -7.890482213473404727, 8.307910125248191946, 0.7216878364870578100 ) ) ;
#153373 = CARTESIAN_POINT ( 'NONE',  ( 3.586021145937230870, 1.010873021915110748, 1.503094931805592394 ) ) ;
#153374 = CARTESIAN_POINT ( 'NONE',  ( 4.645656780685024856, 1.893963204498310571, -0.2871864570129621375 ) ) ;
#153375 = CARTESIAN_POINT ( 'NONE',  ( -1.364683531250010295, 4.842708333674756283, 0.7879004041258379498 ) ) ;
#153376 = CARTESIAN_POINT ( 'NONE',  ( 4.434422825387909661, 1.933224968735423266, 0.3856102937377944295 ) ) ;
#153377 = CARTESIAN_POINT ( 'NONE',  ( 1.043825456435763410, 0.7835056195745603302, -1.760039731681047215 ) ) ;
#153378 = CARTESIAN_POINT ( 'NONE',  ( 4.926551758443064699, 1.790249073151507497, 0.5424879929923772659 ) ) ;
#153379 = CARTESIAN_POINT ( 'NONE',  ( 3.739178398684524396, 0.3374720328367666888, 2.282779155512550062 ) ) ;
#153380 = CARTESIAN_POINT ( 'NONE',  ( 4.615577964900333008, 0.4086796715298928184, -1.815441397462829398 ) ) ;
#153381 = CARTESIAN_POINT ( 'NONE',  ( -0.6823417656250212460, 5.051041667008086655, 1.181850606188767472 ) ) ;
#153382 = CARTESIAN_POINT ( 'NONE',  ( 0.5324358445358172709, 0.5899921999869184308, 1.928256190492839028 ) ) ;
#153384 = CARTESIAN_POINT ( 'NONE',  ( 1.524195097446314318, -1.171203135327163913, -1.750160316008353201 ) ) ;
#153383 = CARTESIAN_POINT ( 'NONE',  ( -3.538314903042294457, 6.111489239315849531, 1.082531754730560403 ) ) ;
#153385 = CARTESIAN_POINT ( 'NONE',  ( 3.131570294632282092, 5.636953862837537521, -1.082531754730543971 ) ) ;
#153387 = CARTESIAN_POINT ( 'NONE',  ( -10.66756793585402363, 11.33991743478486391, 0.7998128361456462443 ) ) ;
#153386 = DIRECTION ( 'NONE',  ( 0.000000000000000000, 0.000000000000000000, -1.000000000000000000 ) ) ;
#153388 = CARTESIAN_POINT ( 'NONE',  ( 6.573507624224045109, 2.070638407997299257, -0.6205318887850322929 ) ) ;
#153389 = CARTESIAN_POINT ( 'NONE',  ( 3.269896953881154644, 0.5115095171020591636, -2.057881918134551125 ) ) ;
#153390 = CARTESIAN_POINT ( 'NONE',  ( 7.960204194457795477E-17, -2.500000000000002220, 0.6500000000000000222 ) ) ;
#153391 = CARTESIAN_POINT ( 'NONE',  ( 1.019792603244329410, -0.4866989216864863188, 1.960159232486478498 ) ) ;
#153392 = CARTESIAN_POINT ( 'NONE',  ( 0.6823417656249882723, 0.4260416670080896528, -1.181850606188749264 ) ) ;
#153393 = CARTESIAN_POINT ( 'NONE',  ( 6.387299765813869712, 6.624473612970537495, 0.000000000000000000 ) ) ;
#153394 = CARTESIAN_POINT ( 'NONE',  ( 4.660252114795294887, 6.460046772059735432, -1.599625672291256295 ) ) ;
#153395 = ORIENTED_EDGE ( 'NONE', *, *, #137004, .F. ) ;
#153396 = CARTESIAN_POINT ( 'NONE',  ( 1.792469030454997059, -2.151019407201111289, -0.2137723215496489249 ) ) ;
#153397 = CARTESIAN_POINT ( 'NONE',  ( 6.610000000000026965, 7.052677709320480659, 2.598153670447616470 ) ) ;
#153400 = CARTESIAN_POINT ( 'NONE',  ( -3.947104627881522720, 8.980740528188976057, -0.7749999999999979128 ) ) ;
#153399 = CARTESIAN_POINT ( 'NONE',  ( 6.825078400183553384, 0.5907600490881077526, 1.908621492364571903 ) ) ;
#153398 = CARTESIAN_POINT ( 'NONE',  ( 4.875038752565570732, 7.845239757038595663, -1.199719254218452047 ) ) ;
#153401 = CARTESIAN_POINT ( 'NONE',  ( -3.719872605471121751, 6.605953636083950364, 2.420000000000000373 ) ) ;
#153402 = CARTESIAN_POINT ( 'NONE',  ( 5.489470343000498076, -0.4852711138302409077, 1.957169415941109047 ) ) ;
#153403 = CARTESIAN_POINT ( 'NONE',  ( -7.700668062882065179, 10.96756792579566664, -1.082531754730543971 ) ) ;
#153404 = B_SPLINE_CURVE_WITH_KNOTS ( 'NONE', 3,
 ( #61121, #178085, #92589, #14484, #93647, #95784 ),
 .UNSPECIFIED., .F., .F.,
 ( 4, 2, 4 ),
 ( 0.000000000000000000, 0.5000000000000000000, 1.000000000000000000 ),
 .UNSPECIFIED. ) ;
#153405 = EDGE_CURVE ( 'NONE', #195316, #127089, #38336, .T. ) ;
#153406 = CARTESIAN_POINT ( 'NONE',  ( 6.462449937854951365, -1.911777437574797345, -0.8467615847161328313 ) ) ;
#153407 = CARTESIAN_POINT ( 'NONE',  ( 0.000000000000000000, -6.583980363594990948, 0.000000000000000000 ) ) ;
#153409 = CARTESIAN_POINT ( 'NONE',  ( -0.6823417656250003738, 12.40104166700806232, 1.181850606188754593 ) ) ;
#153408 = CARTESIAN_POINT ( 'NONE',  ( 0.08136044664198981147, -0.1580758092474404408, -2.227059435111256924 ) ) ;
#153410 = CARTESIAN_POINT ( 'NONE',  ( -7.797910906154257304, 12.24931315715533486, 0.000000000000000000 ) ) ;
#153411 = CARTESIAN_POINT ( 'NONE',  ( -5.002595493318215070, 7.819816594637776674, 1.082531754730560403 ) ) ;
#153412 = CARTESIAN_POINT ( 'NONE',  ( 1.364683531249986537, 2.217708333674751398, -0.7879004041258239610 ) ) ;
#153413 = CARTESIAN_POINT ( 'NONE',  ( 0.6124999999999846123, 2.645833334016141514, 1.060881119635910252 ) ) ;
#153414 = CARTESIAN_POINT ( 'NONE',  ( 0.7500000000000006661, 9.583333333333332149, 1.299038105676657340 ) ) ;
#153415 = CARTESIAN_POINT ( 'NONE',  ( 3.633171361085251849, -1.593041208078986193, 0.6618793944016196917 ) ) ;
#153416 = CARTESIAN_POINT ( 'NONE',  ( 4.206772801990143584, 8.129928378955675328, 0.7998128361456271485 ) ) ;
#153417 = CARTESIAN_POINT ( 'NONE',  ( 1.510649146982666613, 1.557664219135522110, 0.8400682108315477015 ) ) ;
#153418 = VECTOR ( 'NONE', #69737, 1000.000000000000000 ) ;
#153419 = CARTESIAN_POINT ( 'NONE',  ( 2.895184040856535468, -0.1504547458161388240, -2.007539188286605825 ) ) ;
#153420 = EDGE_CURVE ( 'NONE', #172181, #173465, #99636, .T. ) ;
#153421 = CARTESIAN_POINT ( 'NONE',  ( 5.333140672905051893, 0.1575165696711364749, 2.201206011701982934 ) ) ;
#153422 = VERTEX_POINT ( 'NONE', #66030 ) ;
#153423 = CARTESIAN_POINT ( 'NONE',  ( 4.306902303582704761, -0.4466378413249347257, -1.969604032634456825 ) ) ;
#153424 = CARTESIAN_POINT ( 'NONE',  ( -6.882699257592852504, 8.058845884393651460, -1.199719254218452047 ) ) ;
#153426 = CARTESIAN_POINT ( 'NONE',  ( 3.761342352588430860, 1.897692735847063661, -0.6820134568972098243 ) ) ;
#153425 = CARTESIAN_POINT ( 'NONE',  ( 4.266349992362879817, 2.119992548681798095, -0.05317809935000831351 ) ) ;
#153428 = EDGE_LOOP ( 'NONE', ( #137849, #2786, #23010, #203139, #33197 ) ) ;
#153427 = CARTESIAN_POINT ( 'NONE',  ( 4.482537919100934687, -1.178242479775050811, 1.376196796631526720 ) ) ;
#153429 = CARTESIAN_POINT ( 'NONE',  ( 6.249382461256315580, 6.255644057745969988, -0.7998128361456481317 ) ) ;
#153430 = ORIENTED_EDGE ( 'NONE', *, *, #165205, .F. ) ;
#153431 = CARTESIAN_POINT ( 'NONE',  ( 1.815107966846595255, -0.2319292346777863389, 1.856160199827073587 ) ) ;
#153433 = VECTOR ( 'NONE', #208725, 1000.000000000000000 ) ;
#153432 = CARTESIAN_POINT ( 'NONE',  ( -10.91864124492992616, -9.978085788838701120, 0.1530507449821368049 ) ) ;
#153434 = CARTESIAN_POINT ( 'NONE',  ( 5.690068458729246714, 1.084374654971603569, 1.450890516563392518 ) ) ;
#153435 = CARTESIAN_POINT ( 'NONE',  ( 0.7500000000000006661, 9.666666666666671404, -1.299038105676657340 ) ) ;
#153436 = CARTESIAN_POINT ( 'NONE',  ( -10.43233925736708301, 5.066585305077033752, -5.254699789447807134 ) ) ;
#153437 = CYLINDRICAL_SURFACE ( 'NONE', #131773, 0.3999999999999997446 ) ;
#153438 = B_SPLINE_CURVE_WITH_KNOTS ( 'NONE', 3,
 ( #203687, #59589, #190642, #8702 ),
 .UNSPECIFIED., .F., .F.,
 ( 4, 4 ),
 ( 0.000000000000000000, 6.033646489354572420E-05 ),
 .UNSPECIFIED. ) ;
#153439 = CARTESIAN_POINT ( 'NONE',  ( -1.201851678989727383E-14, 3.134375000341420137, 1.575800808251672791 ) ) ;
#153440 = CARTESIAN_POINT ( 'NONE',  ( 0.5977379272000953314, 1.286164058678052946, 1.415416067018962387 ) ) ;
#153441 = CARTESIAN_POINT ( 'NONE',  ( 5.072158865288222351, 8.931619419562697004, 0.7216878364870317197 ) ) ;
#153442 = CARTESIAN_POINT ( 'NONE',  ( 1.820681965693775162, -1.389665069980907441, 1.385087887197037571 ) ) ;
#153443 = CARTESIAN_POINT ( 'NONE',  ( -3.675669043080673770, 7.302381293653823491, 0.000000000000000000 ) ) ;
#153444 = CARTESIAN_POINT ( 'NONE',  ( -5.692444392891315097, 7.734547439830227411, -1.599625672291271394 ) ) ;
#153445 = CARTESIAN_POINT ( 'NONE',  ( 3.656581996618038843, 2.110704406498860486, 0.2042969539849878724 ) ) ;
#153446 = CARTESIAN_POINT ( 'NONE',  ( -0.02948999725182511675, 6.948707995275583471, -2.521364601437687369 ) ) ;
#153447 = CARTESIAN_POINT ( 'NONE',  ( 5.958271952116948711, 0.7966545185628256531, 1.803378638538119860 ) ) ;
#153448 = CARTESIAN_POINT ( 'NONE',  ( 0.6823417656249882723, 1.176041667008083325, -1.181850606188749264 ) ) ;
#153449 = CARTESIAN_POINT ( 'NONE',  ( 0.7561087546162044148, 0.8121304633340595824, -1.842289638184602341 ) ) ;
#153450 = ORIENTED_EDGE ( 'NONE', *, *, #113143, .F. ) ;
#153451 = CARTESIAN_POINT ( 'NONE',  ( 0.8259615556985228091, 0.8540520341687988237, -1.937501654548081875 ) ) ;
#153452 = CARTESIAN_POINT ( 'NONE',  ( 11.91937595155575735, 6.691077280819706097, 0.9935125740681040041 ) ) ;
#153453 = CARTESIAN_POINT ( 'NONE',  ( 2.559107912120599071, 1.664280205102614429, -1.231313097332722872 ) ) ;
#153454 = CARTESIAN_POINT ( 'NONE',  ( 4.878955176071345434, 6.785476686873604280, -1.599625672291269396 ) ) ;
#153455 = CARTESIAN_POINT ( 'NONE',  ( 5.899733120602060232, 6.912052057904395141, -1.199719254218452047 ) ) ;
#153456 = ORIENTED_EDGE ( 'NONE', *, *, #26315, .F. ) ;
#153458 = CARTESIAN_POINT ( 'NONE',  ( 5.626797444871351139, 6.523350759560078593, 1.199719254218462483 ) ) ;
#153457 = CARTESIAN_POINT ( 'NONE',  ( 4.751946794759532189, 0.7997392584290877737, 1.931828438813171456 ) ) ;
#153461 = ORIENTED_EDGE ( 'NONE', *, *, #147708, .F. ) ;
#153460 = CARTESIAN_POINT ( 'NONE',  ( 1.594102673003819248, -0.9688845198280521265, 1.530366366333405281 ) ) ;
#153459 = CARTESIAN_POINT ( 'NONE',  ( 2.643341535394112984, -1.351257319430071657, -1.227710988083303478 ) ) ;
#153462 = CARTESIAN_POINT ( 'NONE',  ( 6.199877634063251541, -0.7475181258948644381, 2.076568058718592624 ) ) ;
#153463 = FACE_OUTER_BOUND ( 'NONE', #72987, .T. ) ;
#153464 = CARTESIAN_POINT ( 'NONE',  ( 4.559734661428293201, 0.4870809927834463537, -2.152189095746533720 ) ) ;
#153465 = CARTESIAN_POINT ( 'NONE',  ( 1.364683531249997417, 8.796875000341403350, 2.602085213965210642E-15 ) ) ;
#153466 = VERTEX_POINT ( 'NONE', #80187 ) ;
#153467 = CARTESIAN_POINT ( 'NONE',  ( 3.229067839489424330, 1.729836904712976686, 0.8154208365811002057 ) ) ;
#153468 = CARTESIAN_POINT ( 'NONE',  ( -2.761056838677368397, 6.372983411765559048, 0.7998128361456341429 ) ) ;
#153469 = CARTESIAN_POINT ( 'NONE',  ( 7.584896871841365851, 10.93646455286856956, -1.199719254218446718 ) ) ;
#153470 = CARTESIAN_POINT ( 'NONE',  ( 6.057099581687969803, 1.694805161836069107, -1.188877858866774107 ) ) ;
#153471 = CARTESIAN_POINT ( 'NONE',  ( -1.360316468750019991, 0.4218750003414165062, -4.336808689942017736E-14 ) ) ;
#153472 = CARTESIAN_POINT ( 'NONE',  ( 5.899973326018037589, -0.7874313895239596350, -2.045375389432432467 ) ) ;
#153473 = CARTESIAN_POINT ( 'NONE',  ( 5.991454128980707949, 7.190850779781567503, -1.201235417510186254 ) ) ;
#153474 = CARTESIAN_POINT ( 'NONE',  ( -4.778160426688590867, 15.44696632703637995, -10.96857316220853029 ) ) ;
#153475 = VERTEX_POINT ( 'NONE', #166774 ) ;
#153476 = ADVANCED_FACE ( 'NONE', ( #148402 ), #75426, .T. ) ;
#153477 = DIRECTION ( 'NONE',  ( 0.000000000000000000, 1.000000000000000000, 0.000000000000000000 ) ) ;
#153478 = CARTESIAN_POINT ( 'NONE',  ( 4.024554299415397551, 1.775361691451295520, 0.5892213400080712482 ) ) ;
#153479 = CARTESIAN_POINT ( 'NONE',  ( -0.02319159430949970652, 0.003959926571647092407, -1.810968101872318714 ) ) ;
#153480 = CARTESIAN_POINT ( 'NONE',  ( 10.51582573219069694, 9.987091415217268064, 3.554376768052132540 ) ) ;
#153481 = AXIS2_PLACEMENT_3D ( 'NONE', #136616, #199447, #201572 ) ;
#153482 = MECHANICAL_DESIGN_GEOMETRIC_PRESENTATION_REPRESENTATION (  '', ( #80818 ), #136330 ) ;
#153483 = CARTESIAN_POINT ( 'NONE',  ( -6.385527162356466668, 10.39360608948380182, 0.000000000000000000 ) ) ;
#153484 = CARTESIAN_POINT ( 'NONE',  ( 5.747730777550676073, 5.670383760089384495, 0.000000000000000000 ) ) ;
#153485 = CARTESIAN_POINT ( 'NONE',  ( 0.4265231311835169792, -1.290831556599820074, 1.487489745873808555 ) ) ;
#153486 = CARTESIAN_POINT ( 'NONE',  ( 1.300407892936685572, 1.352140309104767013, -1.496066053310755262 ) ) ;
#153487 = AXIS2_PLACEMENT_3D ( 'NONE', #17232, #83307, #67042 ) ;
#153488 = CARTESIAN_POINT ( 'NONE',  ( -7.947050595904583403, 12.42330946186405249, 0.7998128361456481317 ) ) ;
#153489 = CARTESIAN_POINT ( 'NONE',  ( 7.842465510862060896, 8.114240948952696542, 0.000000000000000000 ) ) ;
#153490 = CARTESIAN_POINT ( 'NONE',  ( -3.599999999999999201, -0.5000000000000004441, 0.000000000000000000 ) ) ;
#153491 = CARTESIAN_POINT ( 'NONE',  ( 1.746283639092637729, 0.6896231194409886411, 2.080178558289603963 ) ) ;
#153492 = CARTESIAN_POINT ( 'NONE',  ( 5.777927443424748510, 1.091106472389313131, 1.463626628978510702 ) ) ;
#153493 = CARTESIAN_POINT ( 'NONE',  ( -8.611400122974211868, 13.19838391011195888, 1.040834085586084257E-14 ) ) ;
#153494 = CARTESIAN_POINT ( 'NONE',  ( 5.506019780925567986, 8.477421273504887722, -1.082531754730548412 ) ) ;
#153495 = CARTESIAN_POINT ( 'NONE',  ( 9.480175724453529185, 12.08329098332774265, 1.599625672291279388 ) ) ;
#153496 = EDGE_CURVE ( 'NONE', #118849, #61426, #9702, .T. ) ;
#153497 = CARTESIAN_POINT ( 'NONE',  ( 3.867100128395839942, 5.534702787927018974, -1.599625672291255185 ) ) ;
#153498 = CARTESIAN_POINT ( 'NONE',  ( 4.927462483923885195, 4.713404084191450849, -0.7998128361456481317 ) ) ;
#153499 = ORIENTED_EDGE ( 'NONE', *, *, #74564, .T. ) ;
#153501 = CARTESIAN_POINT ( 'NONE',  ( 1.014315213425314166, -2.013265974724808061, 0.002173784167216683862 ) ) ;
#153500 = CARTESIAN_POINT ( 'NONE',  ( 3.561895345837225779, -1.234009368583251387, 1.366721199326895952 ) ) ;
#153502 = CARTESIAN_POINT ( 'NONE',  ( 1.880608668887576052, -0.2816854878555269392, 2.281025131504022863 ) ) ;
#153504 = CARTESIAN_POINT ( 'NONE',  ( 6.455910365318025868, -0.6640748382394038307, 1.846044136633723243 ) ) ;
#153503 = CARTESIAN_POINT ( 'NONE',  ( 2.548569689688999329, 5.917155704705049146, -0.7216878364870267237 ) ) ;
#153505 = CARTESIAN_POINT ( 'NONE',  ( -4.334856428067329404, 6.080418470877079429, -1.599625672291256295 ) ) ;
#153506 = FACE_OUTER_BOUND ( 'NONE', #193418, .T. ) ;
#153507 = CARTESIAN_POINT ( 'NONE',  ( 4.095896644567202038, 1.253117935160457552, 1.444681106026260320 ) ) ;
#153508 = B_SPLINE_CURVE_WITH_KNOTS ( 'NONE', 3,
 ( #193640, #76692, #142808, #107136, #173160, #94045, #24741, #208812, #60444, #44219, #110341, #45282, #176344, #160085, #143883, #11687, #29023, #73496, #96176, #95107, #78816, #66799, #15935, #12742, #129804 ),
 .UNSPECIFIED., .F., .F.,
 ( 4, 3, 3, 3, 3, 3, 3, 3, 4 ),
 ( 0.000000000000000000, 2.847723191052633419E-05, 6.630505566359037818E-05, 8.958118362427361825E-05, 9.621695898307921417E-05, 0.0001106671188294728486, 0.0001194291616091207911, 0.0001339184197518205287, 0.0001602236158699500094 ),
 .UNSPECIFIED. ) ;
#153509 = CARTESIAN_POINT ( 'NONE',  ( -8.809047120577080392, 11.30030761213851953, 1.599625672291269396 ) ) ;
#153510 = CARTESIAN_POINT ( 'NONE',  ( 6.465908158583062892, 6.764574590967027845, 0.2795716154820517829 ) ) ;
#153511 = CARTESIAN_POINT ( 'NONE',  ( -7.756673280794142755, 8.222076047114187602, -0.7216878364870338292 ) ) ;
#153513 = CARTESIAN_POINT ( 'NONE',  ( 1.498681428038322050, 1.531199225506232553, -1.074333469806128427 ) ) ;
#153512 = CARTESIAN_POINT ( 'NONE',  ( 2.366838851271795718, 0.09958507307840713807, -2.088488507012337347 ) ) ;
#153514 = CARTESIAN_POINT ( 'NONE',  ( 2.407577179044288584, 0.4389615990625857500, 1.967586618684707522 ) ) ;
#153515 = CARTESIAN_POINT ( 'NONE',  ( 7.619319141200057821, 10.87266085050000974, 1.082531754730557072 ) ) ;
#153516 = CARTESIAN_POINT ( 'NONE',  ( 0.6823417656249899377, 3.988541667008085767, -1.181850606188754593 ) ) ;
#153517 = CARTESIAN_POINT ( 'NONE',  ( 2.788295088316892656, 1.491546084125561888, -0.8966509355741271170 ) ) ;
#153518 = CARTESIAN_POINT ( 'NONE',  ( 3.011882680530176604, 6.665613560593854459, 0.7998128361456341429 ) ) ;
#153520 = CARTESIAN_POINT ( 'NONE',  ( 0.4132722983370792913, 3.247815196129578919, -1.957108758695520923 ) ) ;
#153519 = DIRECTION ( 'NONE',  ( 0.000000000000000000, 0.000000000000000000, -1.000000000000000000 ) ) ;
#153521 = CARTESIAN_POINT ( 'NONE',  ( 3.457353000975535551, 0.4177302890290990889, -1.673392258113172382 ) ) ;
#153522 = CARTESIAN_POINT ( 'NONE',  ( 3.474349307649237328, -2.112600797985896950, -0.5827812199917583591 ) ) ;
#153523 = DIRECTION ( 'NONE',  ( -0.000000000000000000, 1.000000000000000000, 9.023263958591317418E-17 ) ) ;
#153524 = CARTESIAN_POINT ( 'NONE',  ( -2.788906526875773208E-15, 8.687500000000000000, -1.499999999999998446 ) ) ;
#153525 = CARTESIAN_POINT ( 'NONE',  ( 3.836941170392699885, -2.090934008593826832, -0.5840943183372940828 ) ) ;
#153526 = CARTESIAN_POINT ( 'NONE',  ( 1.945663734523142230, 0.6997465788082489757, -1.686465609443507763 ) ) ;
#153527 = LINE ( 'NONE', #88534, #76385 ) ;
#153528 = CARTESIAN_POINT ( 'NONE',  ( 5.032460059670339270, 0.6174496738353585368, 2.025276144886530627 ) ) ;
#153529 = EDGE_LOOP ( 'NONE', ( #115564, #70053, #176403, #72215 ) ) ;
#153531 = CARTESIAN_POINT ( 'NONE',  ( -1.201851678989727383E-14, 2.384375000341416584, 1.575800808251672791 ) ) ;
#153530 = CARTESIAN_POINT ( 'NONE',  ( 5.021132725759672510, -2.177342503763429082, 0.7171727232720275236 ) ) ;
#153532 = CARTESIAN_POINT ( 'NONE',  ( 6.720655732516684466, 7.052972427687314472, 2.524416814197846914 ) ) ;
#153533 = CARTESIAN_POINT ( 'NONE',  ( 8.204655514564224816, 12.72384853363364066, 1.040834085586084257E-14 ) ) ;
#153534 = CARTESIAN_POINT ( 'NONE',  ( 0.7508259783030580836, 2.089789393294994468, 0.3585813216958123606 ) ) ;
#153535 = CARTESIAN_POINT ( 'NONE',  ( -4.717874267875590277, 7.487641831621378863, 1.082531754730560403 ) ) ;
#153536 = DIRECTION ( 'NONE',  ( 0.000000000000000000, 0.000000000000000000, -1.000000000000000000 ) ) ;
#153537 = CARTESIAN_POINT ( 'NONE',  ( -5.870317324592821073, 6.911420302522161663, -1.082531754730543083 ) ) ;
#153538 =( BOUNDED_SURFACE ( )  B_SPLINE_SURFACE ( 3, 3, ( 
 ( #175650, #10979, #27237, #158332, #59746, #78124, #146361, #93344, #80262, #61883, #128048 ),
 ( #62941, #112834, #9926, #45652, #208118, #129109, #178850, #162593, #76000, #142105, #191863 ),
 ( #53893, #153532, #212374, #69043, #170839, #168702, #135160, #20306, #36558, #148474, #197201 ),
 ( #65057, #131213, #163660, #118955, #98653, #121115, #82383, #81329, #103717, #88540, #48840 ),
 ( #114954, #187080, #213434, #201179, #52817, #147408, #102646, #86391, #2975, #22430, #184934 ),
 ( #152459, #15242, #5101, #196155, #54963, #120028, #4039, #113909, #70108, #136221, #202241 ),
 ( #180954, #186004, #71177, #37639, #32577, #64015, #38713, #169768, #21358, #87464, #16298 ) ),
 .UNSPECIFIED., .T., .F., .T. ) 
 B_SPLINE_SURFACE_WITH_KNOTS ( ( 4, 3, 4 ),
 ( 4, 1, 1, 1, 1, 1, 1, 1, 4 ),
 ( 0.000000000000000000, 0.5000000000000000000, 1.000000000000000000 ),
 ( 0.000000000000000000, 0.2254494161556361009, 0.3971188491599597081, 0.5240836380151728813, 0.6154273167216615104, 0.6803253696226415626, 0.7282602231486813293, 0.7688932809586735972, 1.000000000000000000 ),
 .UNSPECIFIED. ) 
 GEOMETRIC_REPRESENTATION_ITEM ( )  RATIONAL_B_SPLINE_SURFACE ( (
 ( 1.000000000000000222, 1.000000000000000222, 0.9999999999999995559, 1.000000000000000666, 0.9999999999999997780, 0.9999999999999997780, 1.000000000000000000, 1.000000000000000000, 1.000000000000000000, 1.000000000000000000, 1.000000000000000000),
 ( 0.3333333333333334259, 0.3333333333333334259, 0.3333333333333332593, 0.3333333333333335369, 0.3333333333333333148, 0.3333333333333333148, 0.3333333333333334259, 0.3333333333333333703, 0.3333333333333333148, 0.3333333333333333703, 0.3333333333333333703),
 ( 0.3333333333333334259, 0.3333333333333334259, 0.3333333333333332593, 0.3333333333333335369, 0.3333333333333333148, 0.3333333333333333148, 0.3333333333333334259, 0.3333333333333333703, 0.3333333333333333148, 0.3333333333333333703, 0.3333333333333333703),
 ( 1.000000000000000222, 1.000000000000000222, 0.9999999999999995559, 1.000000000000000666, 0.9999999999999997780, 0.9999999999999997780, 1.000000000000000000, 1.000000000000000000, 1.000000000000000000, 1.000000000000000000, 1.000000000000000000),
 ( 0.3333333333333334259, 0.3333333333333334259, 0.3333333333333332593, 0.3333333333333335369, 0.3333333333333333148, 0.3333333333333333148, 0.3333333333333334259, 0.3333333333333333703, 0.3333333333333333148, 0.3333333333333333703, 0.3333333333333333703),
 ( 0.3333333333333334259, 0.3333333333333334259, 0.3333333333333332593, 0.3333333333333335369, 0.3333333333333333148, 0.3333333333333333148, 0.3333333333333334259, 0.3333333333333333703, 0.3333333333333333148, 0.3333333333333333703, 0.3333333333333333703),
 ( 1.000000000000000222, 1.000000000000000222, 0.9999999999999995559, 1.000000000000000666, 0.9999999999999997780, 0.9999999999999997780, 1.000000000000000000, 1.000000000000000000, 1.000000000000000000, 1.000000000000000000, 1.000000000000000000) ) ) 
 REPRESENTATION_ITEM ( '' )  SURFACE ( )  );
#153539 = CARTESIAN_POINT ( 'NONE',  ( 6.883263157960365142, -0.001323150302089473379, 1.953658984494692330 ) ) ;
#153540 = ORIENTED_EDGE ( 'NONE', *, *, #128141, .F. ) ;
#153541 = CARTESIAN_POINT ( 'NONE',  ( 5.133435478496918947, 0.5880181904946503169, 1.928752423557971829 ) ) ;
#153543 = CARTESIAN_POINT ( 'NONE',  ( 3.151292761600641867, 1.771340389172958441, -1.056411398746412544 ) ) ;
#153542 = CARTESIAN_POINT ( 'NONE',  ( 5.660692828905515839, 6.562895374266609849, -1.199719254218445830 ) ) ;
#153545 = CARTESIAN_POINT ( 'NONE',  ( -0.2411972340276023752, 5.722880186377757639, -2.494559970919587588 ) ) ;
#153544 = CARTESIAN_POINT ( 'NONE',  ( 7.354371980770088690, 7.544798497178720531, 0.000000000000000000 ) ) ;
#153546 = CARTESIAN_POINT ( 'NONE',  ( 7.537407054554579489, 7.758339416593960536, 0.000000000000000000 ) ) ;
#153547 = CARTESIAN_POINT ( 'NONE',  ( -1.642778471874998480, -1.451041666188708446, 2.845375778867863303 ) ) ;
#153548 = FILL_AREA_STYLE_COLOUR ( '', #40671 ) ;
#153549 = CARTESIAN_POINT ( 'NONE',  ( 0.09384556119819162379, -2.090229486699231032, -0.04899896570133810414 ) ) ;
#153550 = CARTESIAN_POINT ( 'NONE',  ( 4.307267641921147749, 1.238321930042911578, -1.591317616567271775 ) ) ;
#153551 = CARTESIAN_POINT ( 'NONE',  ( 2.946635061770470632, -1.506786691049965432, -1.057933238436038925 ) ) ;
#153552 = EDGE_CURVE ( 'NONE', #56590, #60185, #58106, .T. ) ;
#153553 = CARTESIAN_POINT ( 'NONE',  ( 6.006425746053997372, 6.966250444273174303, -1.199719254218445830 ) ) ;
#153554 = CARTESIAN_POINT ( 'NONE',  ( 1.254464346661397833, -1.363098773983735024, 1.056675342818178542 ) ) ;
#153555 = CARTESIAN_POINT ( 'NONE',  ( -3.621833129746822255, 4.096114899008192367, -2.500000000000000444 ) ) ;
#153556 = CARTESIAN_POINT ( 'NONE',  ( 1.073308018423566823, -1.027821916426611581, 2.056166664744577321 ) ) ;
#153557 = CARTESIAN_POINT ( 'NONE',  ( -6.437424008390261854, 6.404749519410410485, 0.7998128361456341429 ) ) ;
#153558 = CARTESIAN_POINT ( 'NONE',  ( 0.4743659920835150978, 1.303974419552447639, 1.848657746038349092 ) ) ;
#153559 = CARTESIAN_POINT ( 'NONE',  ( 2.965558217497352267, 0.3084109246280877237, -2.083234000326895430 ) ) ;
#153560 = CARTESIAN_POINT ( 'NONE',  ( -4.960304097753355457, 6.880383762169266504, 1.599625672291263179 ) ) ;
#153561 = CARTESIAN_POINT ( 'NONE',  ( 6.751070424600909448, 9.963667031088037973, -1.199719254218441611 ) ) ;
#153562 = CARTESIAN_POINT ( 'NONE',  ( 6.522881301506172846, 6.782652071278222117, -0.7216878364870458196 ) ) ;
#153563 = SURFACE_STYLE_FILL_AREA ( #135195 ) ;
#153564 = CARTESIAN_POINT ( 'NONE',  ( -6.795661308947694934, 8.951357498570873261, -1.599625672291263179 ) ) ;
#153565 = B_SPLINE_CURVE_WITH_KNOTS ( 'NONE', 3,
 ( #208554, #164892, #110082, #132438, #175035, #27693, #143625 ),
 .UNSPECIFIED., .F., .F.,
 ( 4, 3, 4 ),
 ( 0.0001126021369352535047, 0.001495765174703663240, 0.002006790696433110015 ),
 .UNSPECIFIED. ) ;
#153566 = CARTESIAN_POINT ( 'NONE',  ( 5.788968402910802169, 8.737251655829183505, 1.082531754730558626 ) ) ;
#153567 = CARTESIAN_POINT ( 'NONE',  ( 4.954777096267108050, 6.838018505022927407, 1.425084580847448379 ) ) ;
#153568 = CARTESIAN_POINT ( 'NONE',  ( -4.731959306369413198, 5.479372931307791461, -1.199719254218446718 ) ) ;
#153569 = CARTESIAN_POINT ( 'NONE',  ( 3.445754134864047025, -2.051236611594880799, 0.8531546545873994747 ) ) ;
#153570 = CARTESIAN_POINT ( 'NONE',  ( 2.449409141518565036, 0.5832169002529237201, -2.112351429719904861 ) ) ;
#153571 = CARTESIAN_POINT ( 'NONE',  ( -6.250472511100020334, 7.250971670160158311, 1.199719254218450271 ) ) ;
#153572 = CARTESIAN_POINT ( 'NONE',  ( -4.014095998097799267, 6.840806543492835345, -1.199719254218450271 ) ) ;
#153573 = CARTESIAN_POINT ( 'NONE',  ( 6.021922112293466967, 1.933069186966931863, -0.3339256516061983038 ) ) ;
#153574 = CARTESIAN_POINT ( 'NONE',  ( 1.364683531249986537, 1.655208333674748955, -0.7879004041258239610 ) ) ;
#153575 = CARTESIAN_POINT ( 'NONE',  ( -2.875737979874388284, 6.369128386579808954, -0.7216878364870458196 ) ) ;
#153577 = ORIENTED_EDGE ( 'NONE', *, *, #28211, .F. ) ;
#153576 = CARTESIAN_POINT ( 'NONE',  ( -5.910991785878183080, 5.998504626387068051, -0.7216878364870278340 ) ) ;
#153578 = CARTESIAN_POINT ( 'NONE',  ( 4.711248855110969913, 1.761570823303935551, -1.180294879073326308 ) ) ;
#153579 = CARTESIAN_POINT ( 'NONE',  ( -3.461074353238556167, 7.259946855412102273, 0.000000000000000000 ) ) ;
#153580 = ORIENTED_EDGE ( 'NONE', *, *, #7723, .F. ) ;
#153582 = CARTESIAN_POINT ( 'NONE',  ( 5.541917325712655717, 0.8799508658935292216, -1.974686638939105343 ) ) ;
#153581 = CARTESIAN_POINT ( 'NONE',  ( -5.316205630334255972, 8.255971431148344308, -1.082531754730549967 ) ) ;
#153583 = CARTESIAN_POINT ( 'NONE',  ( 4.971035877704902184, 8.951292290631053916, 1.040834085586084257E-14 ) ) ;
#153584 = CARTESIAN_POINT ( 'NONE',  ( 5.108874002337426390, -0.2646564886703614006, 1.822002613180016883 ) ) ;
#153585 = CARTESIAN_POINT ( 'NONE',  ( 9.499606442108964544, -9.900000000000005684, -0.08647222121513538362 ) ) ;
#153586 = CARTESIAN_POINT ( 'NONE',  ( -1.364683531250014514, 2.051041667008086655, -0.7879004041258289570 ) ) ;
#153587 = CARTESIAN_POINT ( 'NONE',  ( 0.4502399561126956273, -1.468881883692290113, -0.9332017962183251081 ) ) ;
#153588 = CARTESIAN_POINT ( 'NONE',  ( 1.266901613973835827, 3.782120141946687664, 0.4965463943947275305 ) ) ;
#153589 = CARTESIAN_POINT ( 'NONE',  ( 0.6823417656249882723, -1.094791666325249713, 1.181850606188755259 ) ) ;
#153590 = DIRECTION ( 'NONE',  ( 0.7384114592165670343, 0.000000000000000000, -0.6743504407188151140 ) ) ;
#153591 = CARTESIAN_POINT ( 'NONE',  ( 4.698204674003193304, -2.161138953124014161, -0.05634304724232848394 ) ) ;
#153592 = CARTESIAN_POINT ( 'NONE',  ( -3.598799709423620374, 6.286017863381107240, 1.199719254218464037 ) ) ;
#153593 = AXIS2_PLACEMENT_3D ( 'NONE', #214030, #84062, #86199 ) ;
#153594 = CARTESIAN_POINT ( 'NONE',  ( -7.334597914868735025, 9.580116872145431728, -1.443375672974058777 ) ) ;
#153595 = B_SPLINE_CURVE_WITH_KNOTS ( 'NONE', 3,
 ( #153479, #54911, #119976, #202187, #136169, #185956, #74366, #53845, #171857, #189172 ),
 .UNSPECIFIED., .F., .F.,
 ( 4, 1, 1, 1, 1, 1, 1, 4 ),
 ( 0.000000000000000000, 0.09884949474608377418, 0.1930937302289311708, 0.2616037862002966730, 0.3630310524065313849, 0.5216543902990324888, 0.7338513509102306820, 0.9999999999999998890 ),
 .UNSPECIFIED. ) ;
#153596 = CARTESIAN_POINT ( 'NONE',  ( 3.397504326804317909, 1.702965868850464082, 1.331369057855802174 ) ) ;
#153597 = CARTESIAN_POINT ( 'NONE',  ( 5.325445421541009416, -1.872857986210634484, 0.6156230612282005410 ) ) ;
#153598 = CARTESIAN_POINT ( 'NONE',  ( 3.971823236585111161, 1.486633142371917238, 0.8919779901093974894 ) ) ;
#153599 = CARTESIAN_POINT ( 'NONE',  ( 1.206853476500208133, 1.935082376036290075, 1.028754739392373496 ) ) ;
#153600 = CARTESIAN_POINT ( 'NONE',  ( 1.870602726103831381, 1.187374005633199836, 1.978520242944050711 ) ) ;
#153601 = CARTESIAN_POINT ( 'NONE',  ( 3.374343653733542059, -1.230474546199412877, 1.652924668896506688 ) ) ;
#153602 = CARTESIAN_POINT ( 'NONE',  ( 5.935097076209718381, -1.409686562828060152, -1.336055723097711256 ) ) ;
#153604 = EDGE_CURVE ( 'NONE', #115034, #79990, #197130, .T. ) ;
#153603 = CARTESIAN_POINT ( 'NONE',  ( -8.487040972030346353, 9.003895343564625620, 1.040834085586084257E-14 ) ) ;
#153605 = CARTESIAN_POINT ( 'NONE',  ( -5.601453741101424022, 6.564059448486966986, -1.199719254218453823 ) ) ;
#153606 = CARTESIAN_POINT ( 'NONE',  ( -11.89197415570408900, 13.80000000000000071, -0.8055989572471861093 ) ) ;
#153607 = CARTESIAN_POINT ( 'NONE',  ( -3.371191130072114856E-16, 3.975933801733733564, -11.54759062144378845 ) ) ;
#153608 = CARTESIAN_POINT ( 'NONE',  ( -5.355107487273497391, 9.191449801886996340, 0.7216878364870458196 ) ) ;
#153609 = CARTESIAN_POINT ( 'NONE',  ( 3.628125149645112568, -1.312672481567092708, -1.773765351669121415 ) ) ;
#153610 = CARTESIAN_POINT ( 'NONE',  ( 1.642778471875000035, -2.763541666188709556, -2.845375778867859751 ) ) ;
#153611 = ORIENTED_EDGE ( 'NONE', *, *, #122354, .T. ) ;
#153612 = CARTESIAN_POINT ( 'NONE',  ( 0.8130640335680532349, -1.568041438259277554, -1.001899246494031948 ) ) ;
#153613 = CARTESIAN_POINT ( 'NONE',  ( -0.02919842301645457147, 6.946858002156226064, -2.668856405631584217 ) ) ;
#153614 = FACE_OUTER_BOUND ( 'NONE', #107014, .T. ) ;
#153616 = CARTESIAN_POINT ( 'NONE',  ( 6.925078400183597438, 7.629137130509070275, 2.744348168701661095 ) ) ;
#153615 = CARTESIAN_POINT ( 'NONE',  ( -6.514548575684607989, 6.824011503973982151, -0.5624163230865379948 ) ) ;
#153617 = CARTESIAN_POINT ( 'NONE',  ( 6.632757984263843554, -1.642112545546599023, 0.8327811610863435909 ) ) ;
#153618 = ORIENTED_EDGE ( 'NONE', *, *, #95972, .T. ) ;
#153619 = CARTESIAN_POINT ( 'NONE',  ( 3.696211625926352440, -2.058462806815289259, -0.1027275840673105151 ) ) ;
#153620 = CARTESIAN_POINT ( 'NONE',  ( -1.360316468750054852, 0.9114583336747262843, 0.7853790794158720390 ) ) ;
#153621 = EDGE_CURVE ( 'NONE', #170502, #108282, #139256, .T. ) ;
#153622 = CARTESIAN_POINT ( 'NONE',  ( -6.230135280679522936, 7.227244901336242755, 1.199719254218450271 ) ) ;
#153623 = CARTESIAN_POINT ( 'NONE',  ( -3.810548893104181101, 8.469546410357015276, 2.500000000000000000 ) ) ;
#153624 = CARTESIAN_POINT ( 'NONE',  ( 4.521807925357579805, 5.234196320127330715, -1.199719254218452047 ) ) ;
#153625 = CARTESIAN_POINT ( 'NONE',  ( 1.516555680085801994, 1.384881227076775190, -1.526387457142893256 ) ) ;
#153627 = CARTESIAN_POINT ( 'NONE',  ( -1.364683531250014514, 13.83854166700806765, -0.7879004041258335089 ) ) ;
#153626 = CARTESIAN_POINT ( 'NONE',  ( 0.000000000000000000, 0.000000000000000000, 0.000000000000000000 ) ) ;
#153628 = CARTESIAN_POINT ( 'NONE',  ( 7.305145839664861640, 7.417091655897478653, 0.7998128361456341429 ) ) ;
#153629 =( BOUNDED_CURVE ( )  B_SPLINE_CURVE ( 2, ( #198852, #2779, #82985, #137090, #38514, #50500, #202034, #101373, #118753 ),
 .UNSPECIFIED., .F., .T. ) 
 B_SPLINE_CURVE_WITH_KNOTS ( ( 3, 2, 2, 2, 3 ),
 ( 0.3303571428571428492, 0.3333333333333333148, 0.3392857142857143016, 0.3452380952380952328, 0.3482142857142856429 ),
 .UNSPECIFIED. ) 
 CURVE ( )  GEOMETRIC_REPRESENTATION_ITEM ( )  RATIONAL_B_SPLINE_CURVE ( ( 0.9330127018922194093, 0.9330127018922194093, 1.000000000000000000, 0.8660254037844387076, 1.000000000000000000, 0.8660254037844387076, 1.000000000000000000, 0.9330127018922206306, 0.9330127018922194093 ) ) 
 REPRESENTATION_ITEM ( '' )  );
#153630 = CARTESIAN_POINT ( 'NONE',  ( 1.772846837484799210, 2.502368107626177451, 2.500000000000000444 ) ) ;
#153631 = CARTESIAN_POINT ( 'NONE',  ( 5.461621781982892720, 0.4335984126433762853, -2.163701019753036192 ) ) ;
#153632 = CARTESIAN_POINT ( 'NONE',  ( 0.3511320849261707622, -1.736299752564632204, 1.287366282644891724 ) ) ;
#153633 = CARTESIAN_POINT ( 'NONE',  ( -4.934804725694231564, 5.819988937140460727, -1.082531754730544860 ) ) ;
#153634 = CARTESIAN_POINT ( 'NONE',  ( 0.2687680251878405424, -0.2516378192510167477, -2.000730910237565663 ) ) ;
#153635 =( NAMED_UNIT ( * ) SI_UNIT ( $, .STERADIAN. ) SOLID_ANGLE_UNIT ( ) );
#153636 = CARTESIAN_POINT ( 'NONE',  ( 6.569012486276131213, -1.474873517498687336, 1.216900358440069052 ) ) ;
#153638 = ORIENTED_EDGE ( 'NONE', *, *, #104334, .T. ) ;
#153637 = CARTESIAN_POINT ( 'NONE',  ( 3.121116478100642411, 6.446053203092279027, -0.5571924983477014592 ) ) ;
#153639 = CIRCLE ( 'NONE', #208956, 1.872309607372811158 ) ;
#153640 = EDGE_CURVE ( 'NONE', #138803, #68330, #18400, .T. ) ;
#153641 = CARTESIAN_POINT ( 'NONE',  ( 1.481098450213329976, 1.729700800547562478, -0.7128637423776186255 ) ) ;
#153642 = CARTESIAN_POINT ( 'NONE',  ( 3.169157936054858293, 1.820986098869777470, -0.8666075021629695563 ) ) ;
#153644 = DIRECTION ( 'NONE',  ( 1.000000000000000000, 0.000000000000000000, -1.224646799147353207E-16 ) ) ;
#153643 = CARTESIAN_POINT ( 'NONE',  ( 1.364683531249988757, 0.8843750003414210248, 0.000000000000000000 ) ) ;
#153646 = CARTESIAN_POINT ( 'NONE',  ( 4.951841757635310870, 0.6616352077237923623, -1.999514825752574332 ) ) ;
#153645 = CARTESIAN_POINT ( 'NONE',  ( -9.365985188942097750, 9.821404230054264772, 0.7998128361456462443 ) ) ;
#153647 = VECTOR ( 'NONE', #25526, 1000.000000000000000 ) ;
#153648 = CARTESIAN_POINT ( 'NONE',  ( 6.662942426112080874, 9.860851032851066122, 1.199719254218460707 ) ) ;
#153650 = CARTESIAN_POINT ( 'NONE',  ( -8.376239975144482486, 8.666701480623698828, 1.040834085586084257E-14 ) ) ;
#153649 = CARTESIAN_POINT ( 'NONE',  ( 5.248941747146098180, 6.152795455539095570, -1.199719254218452047 ) ) ;
#153651 = CARTESIAN_POINT ( 'NONE',  ( 3.901829752285186803, 7.334923791204486676, 0.6872182573793610416 ) ) ;
#153652 = CARTESIAN_POINT ( 'NONE',  ( 4.078382194585396192, 0.9556978891391977315, 1.779404116599448082 ) ) ;
#153653 = B_SPLINE_CURVE_WITH_KNOTS ( 'NONE', 3,
 ( #55494, #105335, #70644, #156213, #200646, #171372, #22965 ),
 .UNSPECIFIED., .F., .F.,
 ( 4, 3, 4 ),
 ( 2.452946696069607193E-07, 0.0004046562657335365035, 0.0006364688305826707347 ),
 .UNSPECIFIED. ) ;
#153654 = CARTESIAN_POINT ( 'NONE',  ( 1.364683531249988535, 4.655208333674755394, -0.7879004041258300672 ) ) ;
#153655 = CARTESIAN_POINT ( 'NONE',  ( 0.5146022356567416800, 0.7859572577839054608, 1.907140732884365697 ) ) ;
#153656 = CARTESIAN_POINT ( 'NONE',  ( 7.592202833972727660, 11.80139437303613015, -0.7216878364870267237 ) ) ;
#153657 = CARTESIAN_POINT ( 'NONE',  ( 5.272814564875167420, -2.033366364591123521, -0.7337546567489708904 ) ) ;
#153658 = CARTESIAN_POINT ( 'NONE',  ( 5.338878628731272613, 9.450718510153643948, -0.7998128361456481317 ) ) ;
#153659 = CARTESIAN_POINT ( 'NONE',  ( 0.6823417656249882723, -0.5947916663252492686, 1.181850606188755259 ) ) ;
#153661 = CYLINDRICAL_SURFACE ( 'NONE', #82964, 6.249999999999995559 ) ;
#153660 = CARTESIAN_POINT ( 'NONE',  ( 5.020262018810099924, 9.078999131912302900, 0.7998128361456331437 ) ) ;
#153662 = CARTESIAN_POINT ( 'NONE',  ( 8.731087737076324018, 9.288616569451617622, 1.040834085586084257E-14 ) ) ;
#153664 = CARTESIAN_POINT ( 'NONE',  ( -6.280867513185877376E-15, -8.256136661604328353, 10.93205753685578330 ) ) ;
#153663 = CARTESIAN_POINT ( 'NONE',  ( 3.086559893568251223, 1.208301842568102247, -1.803703480758335642 ) ) ;
#153666 = CARTESIAN_POINT ( 'NONE',  ( 2.313779677144182312, 1.201330555204615180, -1.395457044143719072 ) ) ;
#153665 = CARTESIAN_POINT ( 'NONE',  ( -4.582292731738899505, 8.289832587096611860, 0.7216878364870458196 ) ) ;
#153667 = CARTESIAN_POINT ( 'NONE',  ( 1.364683531249990311, 3.634375000341416584, 1.214306433183764966E-14 ) ) ;
#153668 = CARTESIAN_POINT ( 'NONE',  ( 3.245827600587628758, 2.191739723504753101, -0.002129563554123526260 ) ) ;
#153669 = CARTESIAN_POINT ( 'NONE',  ( -15.75000000000000000, 12.30000000000000071, 0.6999999999999992895 ) ) ;
#153670 = CARTESIAN_POINT ( 'NONE',  ( 5.383742603502962965, 1.515107113446222398, 1.680479692888930288 ) ) ;
#153671 = CARTESIAN_POINT ( 'NONE',  ( -4.693093728624763372, 8.627026450037540428, 0.7998128361456481317 ) ) ;
#153672 = CARTESIAN_POINT ( 'NONE',  ( -5.000000000000009770, 3.850000000000006306, 0.5000000000000064393 ) ) ;
#153673 = CARTESIAN_POINT ( 'NONE',  ( 6.476386945563378461, 6.757828299745357370, 0.2189195654383000456 ) ) ;
#153674 = CARTESIAN_POINT ( 'NONE',  ( 1.499999999999993117, 14.35416666666666785, 0.8660254037844409281 ) ) ;
#153675 = CARTESIAN_POINT ( 'NONE',  ( 5.722950238744209273, 6.809768379023969587, 1.082531754730549967 ) ) ;
#153676 = CARTESIAN_POINT ( 'NONE',  ( 5.940640833738206616, 0.3468769465994473444, 1.735210755170372376 ) ) ;
#153677 = CARTESIAN_POINT ( 'NONE',  ( 6.909851844459134362, 11.21324425184434936, -0.7998128361456291469 ) ) ;
#153678 = CARTESIAN_POINT ( 'NONE',  ( 1.378104160372157994, 1.254256560567709622, 1.691567388252762649 ) ) ;
#153680 = CARTESIAN_POINT ( 'NONE',  ( 1.499999999999989120, 2.254166666666685970, 0.8660254037844524744 ) ) ;
#153679 = CARTESIAN_POINT ( 'NONE',  ( -1.402160292154681736E-14, 11.92187500034140157, 1.575800808251682339 ) ) ;
#153681 = CARTESIAN_POINT ( 'NONE',  ( 2.189847533163618465, -1.284324338361255258, -1.493307823759764341 ) ) ;
#153682 = CARTESIAN_POINT ( 'NONE',  ( 4.271419947503845012E-16, 3.900000000000000799, -2.400000000000007461 ) ) ;
#153683 = CARTESIAN_POINT ( 'NONE',  ( 0.2562055958934654210, -1.961350414083770977, -0.05204156388862594962 ) ) ;
#153685 = EDGE_LOOP ( 'NONE', ( #130248, #85673, #62007, #87751 ) ) ;
#153684 = CARTESIAN_POINT ( 'NONE',  ( 5.660388270892238616, 1.809938998256973575, 0.08008182766248285456 ) ) ;
#153686 = CARTESIAN_POINT ( 'NONE',  ( 6.819388077993785657, 7.058300300521964665, 1.040834085586084257E-14 ) ) ;
#153687 = CARTESIAN_POINT ( 'NONE',  ( 0.6823417656249882723, -0.8447916663252494907, 1.181850606188755259 ) ) ;
#153688 = CARTESIAN_POINT ( 'NONE',  ( 5.313307075269409374, -0.2735208697075517947, 1.850433306854900817 ) ) ;
#153689 = ORIENTED_EDGE ( 'NONE', *, *, #174645, .F. ) ;
#153690 = CARTESIAN_POINT ( 'NONE',  ( 5.190316231837919680, 1.068962568377257671, -1.772817291931286787 ) ) ;
#153691 = CARTESIAN_POINT ( 'NONE',  ( 1.224999999999989875, 2.624999999999995559, -2.255140518769849223E-14 ) ) ;
#153692 = CARTESIAN_POINT ( 'NONE',  ( -4.611181641979265500, 8.393812659035525314, 0.000000000000000000 ) ) ;
#153693 = AXIS2_PLACEMENT_3D ( 'NONE', #67809, #51613, #1753 ) ;
#153694 = CARTESIAN_POINT ( 'NONE',  ( 0.7499999999999885647, 0.5666666666666875241, -1.299038105676652899 ) ) ;
#153695 = CARTESIAN_POINT ( 'NONE',  ( 8.599949509769960088, 8.927695937686774386, 1.040834085586084257E-14 ) ) ;
#153696 = CARTESIAN_POINT ( 'NONE',  ( -7.492852449846775897, 11.89341162479659531, 0.000000000000000000 ) ) ;
#153697 = CARTESIAN_POINT ( 'NONE',  ( 5.169401708560450004, 9.252995436621013425, 0.000000000000000000 ) ) ;
#153698 = CARTESIAN_POINT ( 'NONE',  ( -0.6823417656250246877, -0.6989583329919113464, 1.181850606188755259 ) ) ;
#153700 = VECTOR ( 'NONE', #113295, 1000.000000000000000 ) ;
#153699 = CARTESIAN_POINT ( 'NONE',  ( -1.499999999999997780, 1.650000000000019451, 0.000000000000000000 ) ) ;
#153702 = CARTESIAN_POINT ( 'NONE',  ( 3.825371897350130723, 7.614684313550482031, 0.7998128361456321445 ) ) ;
#153701 = CARTESIAN_POINT ( 'NONE',  ( 4.756279191188107269, -1.961398630904508833, -0.05015466537350299348 ) ) ;
#153703 = CARTESIAN_POINT ( 'NONE',  ( 2.266953675890924558, -2.015725231744563750, 0.04666741021024793656 ) ) ;
#153704 = CARTESIAN_POINT ( 'NONE',  ( 2.536237933002471134, 0.6498936893539140058, 1.802224345963408192 ) ) ;
#153705 = CARTESIAN_POINT ( 'NONE',  ( -0.1108833634137010027, 2.037774818562386514, -2.313487243312782216 ) ) ;
#153706 = CARTESIAN_POINT ( 'NONE',  ( 0.4686481397476391364, -2.065551408369214137, -0.7328327568804984260 ) ) ;
#153707 = DIRECTION ( 'NONE',  ( 0.000000000000000000, 0.000000000000000000, 1.000000000000000000 ) ) ;
#153708 = CARTESIAN_POINT ( 'NONE',  ( 2.477632765499269141, 1.147360842229189437, 1.477270975257204411 ) ) ;
#153709 = CARTESIAN_POINT ( 'NONE',  ( -0.6823417656249969321, 5.217708333674756283, -1.181850606188749264 ) ) ;
#153710 = CARTESIAN_POINT ( 'NONE',  ( 4.166274970888473206, 2.012660793657996106, -0.05373556394885727755 ) ) ;
#153711 = CARTESIAN_POINT ( 'NONE',  ( -7.621654909176601045, 12.04368116068139472, 0.7998128361456481317 ) ) ;
#153713 = CARTESIAN_POINT ( 'NONE',  ( 4.271193901148872207, 1.890388351848461657, -0.9536453560208182356 ) ) ;
#153712 = CARTESIAN_POINT ( 'NONE',  ( -3.931501358282937009, 7.530575984731317618, 0.7216878364870317197 ) ) ;
#153714 = CARTESIAN_POINT ( 'NONE',  ( -7.013428937081434000, 5.939655416065874327, -2.436399677959149468 ) ) ;
#153715 = CARTESIAN_POINT ( 'NONE',  ( 5.951642636407409093, 1.565221049572671719, 1.355249363302114318 ) ) ;
#153717 = CARTESIAN_POINT ( 'NONE',  ( 11.87815913191693618, 13.80307820631413307, 1.708869976696506754 ) ) ;
#153716 = CARTESIAN_POINT ( 'NONE',  ( 1.294599682487684422, 1.707161730183017534, -1.206694161613943272 ) ) ;
#153719 = ORIENTED_EDGE ( 'NONE', *, *, #50950, .F. ) ;
#153718 = CARTESIAN_POINT ( 'NONE',  ( 5.930640623865813588, 1.760069778787749506, 0.4843501209313359479 ) ) ;
#153720 = CARTESIAN_POINT ( 'NONE',  ( 7.076466111328892694, 10.34329533227067799, -1.199719254218441611 ) ) ;
#153721 = CARTESIAN_POINT ( 'NONE',  ( -4.406036734316890247, 7.123831375802920363, -1.082531754730548412 ) ) ;
#153722 = CARTESIAN_POINT ( 'NONE',  ( -11.97185388258315086, 13.87999990720392596, 0.8311143155443557751 ) ) ;
#153723 = CARTESIAN_POINT ( 'NONE',  ( 6.683806541412754321, 8.820860269780128604, -1.443375672974058777 ) ) ;
#153724 = CARTESIAN_POINT ( 'NONE',  ( -0.6823417656250003738, 13.21354166700806942, 1.181850606188754593 ) ) ;
#153725 = CARTESIAN_POINT ( 'NONE',  ( 0.06471810551328219252, -1.456173922333989790, 1.077237379209189827 ) ) ;
#153726 = CARTESIAN_POINT ( 'NONE',  ( -7.914208982075130905, 10.25632978388623684, -1.599625672291263179 ) ) ;
#153727 = CARTESIAN_POINT ( 'NONE',  ( 4.469384193999260901, 8.366031992974468423, -0.7998128361456231517 ) ) ;
#153728 = CARTESIAN_POINT ( 'NONE',  ( 0.4694063952341809287, -6.700000000000007283, 10.98997987423604172 ) ) ;
#153729 = FACE_OUTER_BOUND ( 'NONE', #1396, .T. ) ;
#153730 = CARTESIAN_POINT ( 'NONE',  ( 3.195971524519376494, 4.751719416737803847, -1.599625672291262513 ) ) ;
#153731 = EDGE_LOOP ( 'NONE', ( #151755, #86206, #51044, #120568 ) ) ;
#153732 = ADVANCED_FACE ( 'NONE', ( #18370 ), #84447, .T. ) ;
#153733 = CARTESIAN_POINT ( 'NONE',  ( 5.642203898613793456, 0.8197873783117490820, 1.842442240159094080 ) ) ;
#153734 = CARTESIAN_POINT ( 'NONE',  ( -0.004992717928550480244, -2.057963470346049650, -0.5107951590591561786 ) ) ;
#153735 = CARTESIAN_POINT ( 'NONE',  ( 0.2126227708255458981, -7.873890270133753525E-15, -1.223618500935122366 ) ) ;
#153736 = CLOSED_SHELL ( 'NONE', ( #141403, #106232, #64576, #53084, #199942, #83275, #52579, #17967 ) ) ;
#153737 = CARTESIAN_POINT ( 'NONE',  ( -0.1399997263889836974, 2.022132088033218533, -2.415689637818136948 ) ) ;
#153738 = CARTESIAN_POINT ( 'NONE',  ( -3.958617665510266725, 7.562211676496538360, -0.7216878364870267237 ) ) ;
#153739 = CARTESIAN_POINT ( 'NONE',  ( 10.41229878561526512, 11.25002945941372623, -0.7216878364870257245 ) ) ;
#153740 = CARTESIAN_POINT ( 'NONE',  ( 3.959776185634265921, -0.5760637367184845425, 1.883274482577349973 ) ) ;
#153741 = CARTESIAN_POINT ( 'NONE',  ( 4.446888776373093322, -1.802426293348384334, -0.9040943451460029534 ) ) ;
#153742 = CARTESIAN_POINT ( 'NONE',  ( -6.018930129462987999, 9.109503353427070849, 1.199719254218452047 ) ) ;
#153743 = CARTESIAN_POINT ( 'NONE',  ( -5.602498012743508227, 5.726462300312828546, -0.1687859242097844992 ) ) ;
#153744 = CARTESIAN_POINT ( 'NONE',  ( 4.505938053128990539, -0.9357023767473917619, -1.981784127816770935 ) ) ;
#153745 = SPHERICAL_SURFACE ( 'NONE', #147013, 0.5000000000000001110 ) ;
#153746 = CARTESIAN_POINT ( 'NONE',  ( 3.663036927850862323, -1.698304795282145063, -0.9092769472496107230 ) ) ;
#153747 = CARTESIAN_POINT ( 'NONE',  ( -6.723954117373590833, 9.932031339322813679, -1.199719254218440723 ) ) ;
#153748 = CARTESIAN_POINT ( 'NONE',  ( -0.1296875068447916890, 6.948706544289747988, -2.421546651465163347 ) ) ;
#153749 = CARTESIAN_POINT ( 'NONE',  ( 0.2236267563471248943, -0.1037379595543522215, 2.204571545119632603 ) ) ;
#153750 = CARTESIAN_POINT ( 'NONE',  ( 0.08058608058606961388, -6.134628647623513231, -10.99970480893079738 ) ) ;
#153751 = ORIENTED_EDGE ( 'NONE', *, *, #107978, .F. ) ;
#153752 = CARTESIAN_POINT ( 'NONE',  ( 4.258669648468278446, 7.022179452304728287, 1.082531754730549078 ) ) ;
#153753 = CARTESIAN_POINT ( 'NONE',  ( 4.557443512217212778, 1.579177641033597368, 1.176567834677658908 ) ) ;
#153755 = CARTESIAN_POINT ( 'NONE',  ( 3.703774327200870076, 1.459685083667804362, 1.386552827976398339 ) ) ;
#153754 = CARTESIAN_POINT ( 'NONE',  ( 0.04629046987890492182, -1.559278246393133838, 1.157480633202745635 ) ) ;
#153756 = CARTESIAN_POINT ( 'NONE',  ( 5.290469632519504195, -2.184888740097378879, 0.7135917202819259675 ) ) ;
#153758 = CARTESIAN_POINT ( 'NONE',  ( 2.694024576921652425, 0.8818583146339260548, -1.638763372900291726 ) ) ;
#153757 = CARTESIAN_POINT ( 'NONE',  ( -7.095713291905736853, 9.371694488680407886, 1.599625672291269396 ) ) ;
#153759 = CARTESIAN_POINT ( 'NONE',  ( 5.851225812749518695, 8.984124660586543243, -1.199719254218452047 ) ) ;
#153760 = FACE_BOUND ( 'NONE', #108571, .T. ) ;
#153761 =( NAMED_UNIT ( * ) SI_UNIT ( $, .STERADIAN. ) SOLID_ANGLE_UNIT ( ) );
#153762 = CARTESIAN_POINT ( 'NONE',  ( -7.867809214632013770, 8.073532260025807261, 1.040834085586084257E-14 ) ) ;
#153763 = AXIS2_PLACEMENT_3D ( 'NONE', #128020, #161504, #145280 ) ;
#153764 = CARTESIAN_POINT ( 'NONE',  ( -5.316205630334268406, 6.335233002545657577, -1.082531754730549967 ) ) ;
#153765 = CARTESIAN_POINT ( 'NONE',  ( 5.794497793856321799, 1.708647746284063684, -1.204582154990775811 ) ) ;
#153766 = CARTESIAN_POINT ( 'NONE',  ( 6.344852701515477200, 6.504675694630598137, -0.7216878364870257245 ) ) ;
#153767 = EDGE_LOOP ( 'NONE', ( #122902, #139230, #206175, #75381, #142261, #66710, #151862, #50442, #174557, #160633, #187800, #10255, #53715, #56565, #169437, #193563 ) ) ;
#153768 = DIRECTION ( 'NONE',  ( -1.000000000000000000, 0.000000000000000000, 0.000000000000000000 ) ) ;
#153769 = CARTESIAN_POINT ( 'NONE',  ( -1.138412281109779656E-15, -5.530538574611999714, -11.29689844398641974 ) ) ;
#153770 = CARTESIAN_POINT ( 'NONE',  ( 0.6623940301842005107, -1.324425631624454036, 1.256838194884236204 ) ) ;
#153771 = CARTESIAN_POINT ( 'NONE',  ( -4.249591082879585535, 7.045274465746411252, 1.199719254218464037 ) ) ;
#153772 = CARTESIAN_POINT ( 'NONE',  ( 2.883173651945786009, -0.5064310303744267161, -1.658517218374066848 ) ) ;
#153773 = CARTESIAN_POINT ( 'NONE',  ( 6.509000000000033204, 1.287336644856639456, 2.017667062298739822 ) ) ;
#153774 = CARTESIAN_POINT ( 'NONE',  ( -5.045605722580076780, 9.038290442985410067, -0.7998128361456231517 ) ) ;
#153775 = CARTESIAN_POINT ( 'NONE',  ( -5.900304042155601003, 6.007113627712965531, 0.2101855125488115983 ) ) ;
#153776 = CARTESIAN_POINT ( 'NONE',  ( 6.912935025559954205, -1.683935878860399971, 1.369999676949062550 ) ) ;
#153777 = CARTESIAN_POINT ( 'NONE',  ( 5.338443970399977978, 1.799313579390570128, 0.3082849261525285600 ) ) ;
#153778 = CARTESIAN_POINT ( 'NONE',  ( 3.239059677355364375, -0.1396402669299641186, -1.956817938210092089 ) ) ;
#153779 = CARTESIAN_POINT ( 'NONE',  ( -1.225000000000004086, -0.7083333326505274474, -0.7072540797572998139 ) ) ;
#153780 = CARTESIAN_POINT ( 'NONE',  ( -8.479735010343349089, 11.98044238112085758, 1.199719254218453823 ) ) ;
#153781 = CARTESIAN_POINT ( 'NONE',  ( 6.425674737872927089, 9.584038729905381970, -1.199719254218440723 ) ) ;
#153782 = CARTESIAN_POINT ( 'NONE',  ( 3.809332071562030908, 1.790574611000576244, -1.135637872363919110 ) ) ;
#153783 = CARTESIAN_POINT ( 'NONE',  ( 6.827182134110219458, 3.682144966263277919, 2.702925436647873880 ) ) ;
#153784 = AXIS2_PLACEMENT_3D ( 'NONE', #87962, #138865, #120542 ) ;
#153785 = CARTESIAN_POINT ( 'NONE',  ( -7.811469059767924605, 12.26513100303794168, -0.7998128361456281477 ) ) ;
#153786 = CARTESIAN_POINT ( 'NONE',  ( 2.184514099445804547, 1.195434181571125132, -1.690031224328606196 ) ) ;
#153788 = CARTESIAN_POINT ( 'NONE',  ( 1.500000000000001332, 14.65625000068279604, 0.000000000000000000 ) ) ;
#153787 = DIRECTION ( 'NONE',  ( -5.828670879282089587E-16, 0.8656921114426509023, -0.5005768354468322912 ) ) ;
#153791 = ORIENTED_EDGE ( 'NONE', *, *, #204906, .T. ) ;
#153790 = CARTESIAN_POINT ( 'NONE',  ( 4.653117599668723514, 0.3792583102804178985, 2.188544891856615049 ) ) ;
#153789 = CIRCLE ( 'NONE', #57000, 0.08000000000000002942 ) ;
#153792 = CARTESIAN_POINT ( 'NONE',  ( 1.776460590643181625, 1.997282851074515975, -1.137850514363091481 ) ) ;
#153793 = CARTESIAN_POINT ( 'NONE',  ( 9.734391104931955141, 10.45913716528321125, 0.7216878364870438212 ) ) ;
#153795 = CARTESIAN_POINT ( 'NONE',  ( 1.737500000000001155, -0.2333333333333319215, 3.009438278150922130 ) ) ;
#153794 = CARTESIAN_POINT ( 'NONE',  ( 5.546694241766559230, 9.485244025454063532, 0.000000000000000000 ) ) ;
#153796 = CARTESIAN_POINT ( 'NONE',  ( -1.579999999999998073, 8.674529973577531194, -2.499999999999990230 ) ) ;
#153797 = CARTESIAN_POINT ( 'NONE',  ( 6.620655732516645742, 0.007553340620044741646, 1.826407896915737794 ) ) ;
#153798 = FACE_OUTER_BOUND ( 'NONE', #11421, .T. ) ;
#153799 = CARTESIAN_POINT ( 'NONE',  ( 2.619282413590624525, 1.617716081779559278, 1.019604094833974628 ) ) ;
#153800 = CARTESIAN_POINT ( 'NONE',  ( -10.39230484541327648, 3.499999999999989342, -5.999999999999976019 ) ) ;
#153801 = CARTESIAN_POINT ( 'NONE',  ( 3.733171248123872132, -1.593707704047672591, 0.6599822260907485250 ) ) ;
#153802 = CARTESIAN_POINT ( 'NONE',  ( 2.307827663788959871, -1.164988201124015577, -1.645758576239789051 ) ) ;
#153803 =( BOUNDED_SURFACE ( )  B_SPLINE_SURFACE ( 3, 2, ( 
 ( #169449, #170512, #184618 ),
 ( #21034, #116498, #134847 ),
 ( #151088, #34116, #17842 ),
 ( #86068, #182487, #54633 ) ),
 .UNSPECIFIED., .F., .F., .F. ) 
 B_SPLINE_SURFACE_WITH_KNOTS ( ( 4, 4 ),
 ( 3, 3 ),
 ( 0.5050616349177523556, 1.570796326794896558 ),
 ( 0.000000000000000000, 1.000000000000000000 ),
 .UNSPECIFIED. ) 
 GEOMETRIC_REPRESENTATION_ITEM ( )  RATIONAL_B_SPLINE_SURFACE ( (
 ( 1.000000000000000000, 0.9374448844494615019, 1.000000000000000000),
 ( 1.000000000000000000, 0.8980788380694217921, 1.000000000000000000),
 ( 1.000000000000000000, 0.8161930835858733913, 1.000000000000000000),
 ( 1.000000000000000000, 0.7071067811866033059, 1.000000000000000000) ) ) 
 REPRESENTATION_ITEM ( '' )  SURFACE ( )  );
#153804 = CARTESIAN_POINT ( 'NONE',  ( 3.428665021107531352, -1.741954984014550512, -1.499980572608774043 ) ) ;
#153805 = AXIS2_PLACEMENT_3D ( 'NONE', #17341, #65034, #68222 ) ;
#153806 = CARTESIAN_POINT ( 'NONE',  ( 3.304270634109522486, -2.259957100417890441, 0.1074057698594049759 ) ) ;
#153807 = CARTESIAN_POINT ( 'NONE',  ( 6.551405291548149101, -1.690254494844857014, -1.256206543278805876 ) ) ;
#153808 = CARTESIAN_POINT ( 'NONE',  ( -4.177320726786315497, 7.887641591310407208, -0.7216878364870458196 ) ) ;
#153809 = ORIENTED_EDGE ( 'NONE', *, *, #150631, .F. ) ;
#153810 = CARTESIAN_POINT ( 'NONE',  ( 4.270580540438973394, -1.650736559713336771, -0.6384287733962620282 ) ) ;
#153812 = CARTESIAN_POINT ( 'NONE',  ( 1.219134843238580235, -0.05193690637114551506, 2.291835786607650416 ) ) ;
#153811 = CARTESIAN_POINT ( 'NONE',  ( 7.537407054554579489, 7.758339416593960536, 0.000000000000000000 ) ) ;
#153813 = B_SPLINE_CURVE_WITH_KNOTS ( 'NONE', 3,
 ( #77295, #90358, #74102, #10151, #57842, #158554 ),
 .UNSPECIFIED., .F., .F.,
 ( 4, 2, 4 ),
 ( 0.000000000000000000, 0.002406600572792975002, 0.004813201145585950871 ),
 .UNSPECIFIED. ) ;
#153814 = CARTESIAN_POINT ( 'NONE',  ( 6.158133876658566486, -1.298579738958350660, 1.305440813956220136 ) ) ;
#153815 = CARTESIAN_POINT ( 'NONE',  ( -4.634189577772691138, 4.300976017023221409, 1.214306433183764966E-14 ) ) ;
#153816 = CARTESIAN_POINT ( 'NONE',  ( 5.876942531769461020, 2.026063101133714461, -0.8356547683932223913 ) ) ;
#153817 = CARTESIAN_POINT ( 'NONE',  ( -5.224688093219839402, 7.188831756880171397, -1.599625672291271394 ) ) ;
#153818 = CARTESIAN_POINT ( 'NONE',  ( -3.164938793786285842, 5.779846795137578930, -1.199719254218452935 ) ) ;
#153819 = CARTESIAN_POINT ( 'NONE',  ( 9.499640643549723151, -8.037485387949198312, -0.09382487309179397827 ) ) ;
#153820 = CARTESIAN_POINT ( 'NONE',  ( 6.197728532230423859, -1.496850047335227085, -1.430563974149069661 ) ) ;
#153821 = CARTESIAN_POINT ( 'NONE',  ( 0.7433754753295095385, 0.3886281223182270761, -1.978556061772406505 ) ) ;
#153822 = CARTESIAN_POINT ( 'NONE',  ( -0.7500000000000006661, -0.6104166659838470288, -1.299038105676652011 ) ) ;
#153823 = CARTESIAN_POINT ( 'NONE',  ( 4.828697303143684394, 1.844096510799615674, 0.5574245839122073942 ) ) ;
#153824 = CARTESIAN_POINT ( 'NONE',  ( 1.364683531249996529, 10.46354166700806765, 0.7879004041258405033 ) ) ;
#153825 = AXIS2_PLACEMENT_3D ( 'NONE', #73273, #8282, #25596 ) ;
#153826 = CARTESIAN_POINT ( 'NONE',  ( 1.231071286002645815, 1.486838745870424860, -1.650645422243676164 ) ) ;
#153828 = ORIENTED_EDGE ( 'NONE', *, *, #185659, .T. ) ;
#153827 = CYLINDRICAL_SURFACE ( 'NONE', #175202, 0.7499999999999997780 ) ;
#153830 = DIRECTION ( 'NONE',  ( -3.216245299353269257E-16, 6.661338147750950089E-16, -1.000000000000000000 ) ) ;
#153829 = CARTESIAN_POINT ( 'NONE',  ( 1.408440994508639577, 7.230285460703519185, -4.273713947604624863 ) ) ;
#153831 = CARTESIAN_POINT ( 'NONE',  ( -3.145128448690340139, 6.613140923539886806, -0.7216878364870489282 ) ) ;
#153832 = CARTESIAN_POINT ( 'NONE',  ( 2.920892028740289081, 5.495125569250587816, 1.199719254218452047 ) ) ;
#153833 = CARTESIAN_POINT ( 'NONE',  ( 1.464175926609780964E-14, -2.537500000000001865, -3.475000000000000533 ) ) ;
#153834 = DIRECTION ( 'NONE',  ( 0.6507913734559658270, 0.7592566023652989049, 0.000000000000000000 ) ) ;
#153835 = CARTESIAN_POINT ( 'NONE',  ( 4.546296192243603151, -1.394137154979861570, 1.041651924218311986 ) ) ;
#153836 = CARTESIAN_POINT ( 'NONE',  ( 2.488659587246493832, 1.902222718079676689, 0.4795239450603656084 ) ) ;
#153838 = CARTESIAN_POINT ( 'NONE',  ( 0.6823417656249899377, 2.905208333674754062, 1.181850606188765695 ) ) ;
#153837 = CARTESIAN_POINT ( 'NONE',  ( 5.823390672269506574, 6.752709524857930745, -1.199719254218446718 ) ) ;
#153839 = CARTESIAN_POINT ( 'NONE',  ( -4.373253022481784491, 7.180661499490419430, 1.044565980707335529 ) ) ;
#153840 = CARTESIAN_POINT ( 'NONE',  ( -11.41267819554183127, 3.447199233515635619, 3.708203932499423150 ) ) ;
#153841 = CARTESIAN_POINT ( 'NONE',  ( 0.1860857499333635756, -1.268064657576525978, -1.627672589050175089 ) ) ;
#153842 = CARTESIAN_POINT ( 'NONE',  ( -9.671043645249580933, 10.17730576241299900, 0.7998128361456462443 ) ) ;
#153843 = CARTESIAN_POINT ( 'NONE',  ( -4.568734577680894304, 5.392907097791561633, -1.082531754730543971 ) ) ;
#153844 = PRESENTATION_LAYER_ASSIGNMENT (  '', '', ( #133150 ) ) ;
#153845 = CARTESIAN_POINT ( 'NONE',  ( 0.8840797711214362087, 1.521441056815290516, 1.674750314396955542 ) ) ;
#153847 = VERTEX_POINT ( 'NONE', #130092 ) ;
#153846 = CARTESIAN_POINT ( 'NONE',  ( -6.067437437315529536, 7.037430750744921859, 1.199719254218450271 ) ) ;
#153848 = CARTESIAN_POINT ( 'NONE',  ( -1.402160292154681736E-14, -0.7562499993171803991, 1.732050807568877637 ) ) ;
#153849 = CARTESIAN_POINT ( 'NONE',  ( 1.352582913587907942, -1.478046865151939615, 1.146363905606573086 ) ) ;
#153850 = CARTESIAN_POINT ( 'NONE',  ( 0.1934855802202296304, 1.507424494634423517, 0.8570536861387479943 ) ) ;
#153852 = CARTESIAN_POINT ( 'NONE',  ( 3.808297599986898430, 1.548825491099754315, -1.550762550882843094 ) ) ;
#153851 = CARTESIAN_POINT ( 'NONE',  ( -0.6801582343750438575, 1.932291667008062541, 1.178068619123787908 ) ) ;
#153853 = CARTESIAN_POINT ( 'NONE',  ( 5.649573025266686699, -1.814708426832438048, -1.425321367006604056 ) ) ;
#153854 = CARTESIAN_POINT ( 'NONE',  ( 6.907514182033759553, -0.4531076517439984186, 2.017496682098403937 ) ) ;
#153855 = CARTESIAN_POINT ( 'NONE',  ( 2.923698373526161465, 1.078347508963822587, -1.614843327186490374 ) ) ;
#153856 = CARTESIAN_POINT ( 'NONE',  ( -4.894130264408862452, 7.693273827576896373, -1.082531754730548412 ) ) ;
#153857 = AXIS2_PLACEMENT_3D ( 'NONE', #140426, #156650, #139337 ) ;
#153858 = PLANE ( 'NONE',  #12960 ) ;
#153859 = CARTESIAN_POINT ( 'NONE',  ( 5.411112705629925301, 5.485588709422586362, 0.000000000000000000 ) ) ;
#153860 = CARTESIAN_POINT ( 'NONE',  ( 1.360316468749985797, 0.2864583336747233422, -0.7853790794158961308 ) ) ;
#153861 = CARTESIAN_POINT ( 'NONE',  ( 2.988907892087853568, -2.013985899409028946, 0.1017507309580278629 ) ) ;
#153862 = CARTESIAN_POINT ( 'NONE',  ( -2.941756144040963417, 6.375873234782333476, -0.7216878364870257245 ) ) ;
#153863 = CARTESIAN_POINT ( 'NONE',  ( -5.094831863685302942, 9.165997284266655498, 0.7998128361456291469 ) ) ;
#153864 = CARTESIAN_POINT ( 'NONE',  ( 8.072990401933337168, 11.50590700464255356, -1.199719254218446718 ) ) ;
#153866 = CARTESIAN_POINT ( 'NONE',  ( 3.660338285565247762, 7.214219066560688454, 1.040834085586084257E-14 ) ) ;
#153865 = CARTESIAN_POINT ( 'NONE',  ( 0.7502976729042536430, 0.5272139720400963459, 1.747899773703022408 ) ) ;
#153867 = CARTESIAN_POINT ( 'NONE',  ( -5.448397627845328550, 7.449826213943242514, 1.599625672291263179 ) ) ;
#153868 = CARTESIAN_POINT ( 'NONE',  ( -6.140917232347002042, 6.129101290685087911, -0.7998128361456361413 ) ) ;
#153869 = CARTESIAN_POINT ( 'NONE',  ( -10.68898853036274055, 3.992937990999307907, 4.901699750972148273 ) ) ;
#153870 = ORIENTED_EDGE ( 'NONE', *, *, #15231, .T. ) ;
#153871 = CARTESIAN_POINT ( 'NONE',  ( 0.3741789627117291239, 1.245922373857488274, 1.766349570875298758 ) ) ;
#153872 = CARTESIAN_POINT ( 'NONE',  ( -6.739811759324831897, 7.996106819701333634, -1.082531754730549967 ) ) ;
#153873 = EDGE_CURVE ( 'NONE', #177822, #33058, #31453, .T. ) ;
#153874 = CARTESIAN_POINT ( 'NONE',  ( -4.288456660624211381, 3.897620947016656956, 1.214306433183764966E-14 ) ) ;
#153875 = CARTESIAN_POINT ( 'NONE',  ( -9.972185678051314284, 11.59297036493672017, 1.199719254218462483 ) ) ;
#153876 = CARTESIAN_POINT ( 'NONE',  ( 6.147130067458792091, 0.1999419896685956377, 2.009763438563259008 ) ) ;
#153878 = ORIENTED_EDGE ( 'NONE', *, *, #195731, .F. ) ;
#153877 = CARTESIAN_POINT ( 'NONE',  ( 5.637407045567618624, -0.05664847855723317838, 2.220727194027871665 ) ) ;
#153879 = CARTESIAN_POINT ( 'NONE',  ( -6.454563648557663846, 9.688018802362710957, -1.199719254218452047 ) ) ;
#153880 = CARTESIAN_POINT ( 'NONE',  ( 5.309989718046547402, 9.346738437696316737, 0.7998128361456462443 ) ) ;
#153881 = CARTESIAN_POINT ( 'NONE',  ( 5.295800851330623615, -0.7439313745516599186, 1.922114966912706224 ) ) ;
#153882 = CARTESIAN_POINT ( 'NONE',  ( 3.533827422916273164, -1.646839391163470223, 1.163268690995450383 ) ) ;
#153883 = ORIENTED_EDGE ( 'NONE', *, *, #51382, .F. ) ;
#153884 = FILL_AREA_STYLE_COLOUR ( '', #169815 ) ;
#153885 = CARTESIAN_POINT ( 'NONE',  ( 4.878236342818665250, 4.585697242910212523, 1.040834085586084257E-14 ) ) ;
#153887 = ORIENTED_EDGE ( 'NONE', *, *, #163618, .F. ) ;
#153886 = CARTESIAN_POINT ( 'NONE',  ( -6.583366107887490770, 9.838288338247510367, 1.199719254218452935 ) ) ;
#153888 = CARTESIAN_POINT ( 'NONE',  ( 5.260375520412221562, 7.786458765878076171, 1.288147692060326532 ) ) ;
#153889 = CARTESIAN_POINT ( 'NONE',  ( 4.095077249698628741, 1.080899603560569799, -1.701687522498253946 ) ) ;
#153890 = CARTESIAN_POINT ( 'NONE',  ( 3.116968920156853340, -1.774181764490849522, 0.4917334186493869108 ) ) ;
#153891 = CARTESIAN_POINT ( 'NONE',  ( 8.134310703387671364E-16, 2.000000000682804924, -1.225000000000021849 ) ) ;
#153892 = CARTESIAN_POINT ( 'NONE',  ( 2.210004991130873453, -0.5033687547432836862, 2.251983625769232500 ) ) ;
#153893 = CARTESIAN_POINT ( 'NONE',  ( 3.237364818613055473, 6.998952398349030268, -1.734723475976807094E-15 ) ) ;
#153894 = CARTESIAN_POINT ( 'NONE',  ( 3.919328646192806520, -0.1633067429045453600, 2.155504054270485970 ) ) ;
#153895 = CARTESIAN_POINT ( 'NONE',  ( 8.945682426918439845, 9.331051007693339727, 1.040834085586084257E-14 ) ) ;
#153896 = CARTESIAN_POINT ( 'NONE',  ( -4.737684612971557740, 7.614716917520386374, 1.199719254218464037 ) ) ;
#153897 = CARTESIAN_POINT ( 'NONE',  ( 3.761312542938214598, -2.295521343867617414, -0.1171695491895396041 ) ) ;
#153898 = CARTESIAN_POINT ( 'NONE',  ( -9.508835372382730355, 15.10147904770789573, -7.212874380515887474 ) ) ;
#153899 = CARTESIAN_POINT ( 'NONE',  ( 1.230687378724321990, 2.810186076401617772, 0.7750000000000152323 ) ) ;
#153900 = CARTESIAN_POINT ( 'NONE',  ( 2.342468781959532453, 0.4075140148256419792, 1.825566309089213579 ) ) ;
#153901 = EDGE_CURVE ( 'NONE', #194227, #102576, #2245, .T. ) ;
#153902 = CARTESIAN_POINT ( 'NONE',  ( 6.578986288830292573, -0.09655258645749519031, -1.969210242046049331 ) ) ;
#153904 = CARTESIAN_POINT ( 'NONE',  ( -5.966470118465691641, 9.118576350588734059, -1.199719254218452047 ) ) ;
#153903 = CARTESIAN_POINT ( 'NONE',  ( -0.6823417656250212460, 4.551041667008086655, 1.181850606188767472 ) ) ;
#153905 = CARTESIAN_POINT ( 'NONE',  ( 1.893488989520499377, 1.919108310403025985, -1.089527612406354873 ) ) ;
#153906 = ORIENTED_EDGE ( 'NONE', *, *, #142863, .F. ) ;
#153907 = CARTESIAN_POINT ( 'NONE',  ( -4.741649638052999549, 5.202212439478444139, 1.069586989871945670 ) ) ;
#153908 = CARTESIAN_POINT ( 'NONE',  ( 4.379447312414087357, 5.068108938359919158, -1.199719254218452047 ) ) ;
#153909 = CARTESIAN_POINT ( 'NONE',  ( -4.731959306369413198, 5.479372931307791461, -1.199719254218446718 ) ) ;
#153910 = CARTESIAN_POINT ( 'NONE',  ( -8.081892667527540652, -5.166862915010159263, 7.462104991928526054 ) ) ;
#153911 = CARTESIAN_POINT ( 'NONE',  ( 6.368046306259418365, 1.013251383440600284, 1.691012432383535602 ) ) ;
#153912 = CARTESIAN_POINT ( 'NONE',  ( 5.444061505814771884, 0.9398705156117830306, -2.107803560374045038 ) ) ;
#153913 = CARTESIAN_POINT ( 'NONE',  ( 0.7835587076311965049, -1.864072139945194717, 0.6119401183290391621 ) ) ;
#153914 = CARTESIAN_POINT ( 'NONE',  ( 4.311423628786446471, -1.712024382654028454, -1.150014069924868654 ) ) ;
#153915 = CARTESIAN_POINT ( 'NONE',  ( 5.016153647376201619, 7.835634441038803466, 1.082531754730558626 ) ) ;
#153916 = CARTESIAN_POINT ( 'NONE',  ( 6.481679955784983349, 9.719654494127929922, -1.199719254218452047 ) ) ;
#153917 = CARTESIAN_POINT ( 'NONE',  ( 7.415946836550712185, 10.63539316174243865, 1.082531754730558626 ) ) ;
#153918 = CARTESIAN_POINT ( 'NONE',  ( -0.6823417656249969321, 3.530208333674754506, -1.181850606188749264 ) ) ;
#153919 = CARTESIAN_POINT ( 'NONE',  ( -5.540653355401692792, 14.53096581237021567, 10.65389762808975149 ) ) ;
#153920 = CARTESIAN_POINT ( 'NONE',  ( 4.812781342726858647, 6.637997537979888563, 1.443375672974062551 ) ) ;
#153921 = CARTESIAN_POINT ( 'NONE',  ( 6.197752310581432056, -1.568275824509495875, -1.501738253884659979 ) ) ;
#153922 = CARTESIAN_POINT ( 'NONE',  ( -0.01485505708498172442, 7.054063922337708625, -3.955400951015620947 ) ) ;
#153924 = CARTESIAN_POINT ( 'NONE',  ( 4.757273854911123756, 1.820453720981948242, -0.2752165127944474210 ) ) ;
#153923 = CARTESIAN_POINT ( 'NONE',  ( 0.000000000000000000, 0.03624871340549007392, 0.000000000000000000 ) ) ;
#153925 = B_SPLINE_CURVE_WITH_KNOTS ( 'NONE', 3,
 ( #132348, #85685, #20665, #182105, #168007, #33734, #51062, #2271, #52129, #99812, #65152, #35866, #185305, #36928, #17464, #103011 ),
 .UNSPECIFIED., .F., .F.,
 ( 4, 3, 3, 3, 3, 4 ),
 ( 1.835777882413431832E-05, 2.688023894040715345E-05, 5.355394816894561410E-05, 9.073944566320893250E-05, 0.0001419156937261367561, 0.0001738851243175512954 ),
 .UNSPECIFIED. ) ;
#153926 = CARTESIAN_POINT ( 'NONE',  ( 9.537847510268184337, -7.985988503423661733, -0.1421055763938764704 ) ) ;
#153927 = CARTESIAN_POINT ( 'NONE',  ( 1.906201616980772950, 3.231688558335350514, 0.4612787108932545066 ) ) ;
#153928 = CARTESIAN_POINT ( 'NONE',  ( 0.1923495491853322581, -0.4021996241703913455, -1.833441224692602844 ) ) ;
#153929 = CARTESIAN_POINT ( 'NONE',  ( -4.390790479118549250, 7.352160220884910835, 1.215098293768980930 ) ) ;
#153930 = CARTESIAN_POINT ( 'NONE',  ( 0.000000000000000000, 4.000000000000003553, 0.000000000000000000 ) ) ;
#153931 = CARTESIAN_POINT ( 'NONE',  ( 5.950060389077887812, 7.221515259811701171, 1.225279837341096689 ) ) ;
#153932 = CARTESIAN_POINT ( 'NONE',  ( 0.5570965697654255422, -1.639946202723217450, 0.9833419947904219471 ) ) ;
#153933 = CARTESIAN_POINT ( 'NONE',  ( 1.955557038561178240, 1.765385265556310701, -0.1263916157485909797 ) ) ;
#153934 = CARTESIAN_POINT ( 'NONE',  ( 6.604166866988625095, -0.8575501651001187220, 1.819208590218702071 ) ) ;
#153936 = CARTESIAN_POINT ( 'NONE',  ( 4.552287420941045326, -1.248256511182913364, 1.453175340101879875 ) ) ;
#153935 = CARTESIAN_POINT ( 'NONE',  ( -9.829825065107822724, 11.42688298316931572, 1.199719254218462483 ) ) ;
#153937 = CARTESIAN_POINT ( 'NONE',  ( -1.754755943840817123, 0.9608980427861949503, 1.301694008101299538 ) ) ;
#153938 = CARTESIAN_POINT ( 'NONE',  ( 5.635196759804959044, -0.04649108105550652653, -1.969165932527061402 ) ) ;
#153939 = CARTESIAN_POINT ( 'NONE',  ( -0.1225938595818750754, -1.897163925677572305, -0.9476133185889324961 ) ) ;
#153940 = CARTESIAN_POINT ( 'NONE',  ( -1.596166908135297824, -1.206333752204373555, 1.472837400516048723 ) ) ;
#153941 = CARTESIAN_POINT ( 'NONE',  ( 2.729206520949432946, -1.746158693253213379, 0.6715030345267187784 ) ) ;
#153943 = ORIENTED_EDGE ( 'NONE', *, *, #126911, .T. ) ;
#153942 = CARTESIAN_POINT ( 'NONE',  ( -0.01727558406095473439, -0.1313277740116538805, -1.795991579427682616 ) ) ;
#153945 = CARTESIAN_POINT ( 'NONE',  ( 3.714570900464285064, 4.396382807705524698, 1.082531754730560403 ) ) ;
#153944 = CARTESIAN_POINT ( 'NONE',  ( 3.457846583235091753, 0.5364296187198510646, -2.140574738106671759 ) ) ;
#153946 = CARTESIAN_POINT ( 'NONE',  ( -1.201851678989727383E-14, 3.634375000341422357, 1.575800808251672791 ) ) ;
#153947 = CARTESIAN_POINT ( 'NONE',  ( 1.135301032730736237, -0.04873925880971052838, -2.062252310772247910 ) ) ;
#153948 = CARTESIAN_POINT ( 'NONE',  ( 5.750629710490689384, 9.860818428881154674, -0.7998128361456291469 ) ) ;
#153950 = CARTESIAN_POINT ( 'NONE',  ( -8.618179199781044630, 13.20629283305325963, 0.7998128361456341429 ) ) ;
#153949 = CIRCLE ( 'NONE', #198898, 11.99999999999999112 ) ;
#153951 = FACE_OUTER_BOUND ( 'NONE', #147373, .T. ) ;
#153952 = CARTESIAN_POINT ( 'NONE',  ( -3.419980048151579854, -0.02405074183678669250, -0.4062349772740375120 ) ) ;
#153953 = CARTESIAN_POINT ( 'NONE',  ( -7.455003611050273982, -6.808400134080597965, -7.905503641038500895 ) ) ;
#153954 = VERTEX_POINT ( 'NONE', #3166 ) ;
#153955 = CARTESIAN_POINT ( 'NONE',  ( 2.928250347896840022, 1.105370970781336837, 1.750397071514836478 ) ) ;
#153957 = CARTESIAN_POINT ( 'NONE',  ( -0.7499999999999972244, 3.858333333333359594, -1.299038105676652011 ) ) ;
#153956 = AXIS2_PLACEMENT_3D ( 'NONE', #162278, #212060, #116773 ) ;
#153958 = CARTESIAN_POINT ( 'NONE',  ( 5.118366684358879759, 5.930181538962194132, 1.199719254218462483 ) ) ;
#153959 = CARTESIAN_POINT ( 'NONE',  ( -5.971735067414164710, 7.203215006737162085, 1.225879040106806706 ) ) ;
#153960 = CARTESIAN_POINT ( 'NONE',  ( 0.5397205009909338269, -1.917025550485540908, 0.6358503350361620621 ) ) ;
#153961 = CARTESIAN_POINT ( 'NONE',  ( 1.499999999990964339, 7.854386371700860181, 3.680172642296245744 ) ) ;
#153962 = CARTESIAN_POINT ( 'NONE',  ( 0.6823417656249917140, 3.342708333674754506, 1.181850606188765695 ) ) ;
#153964 = CARTESIAN_POINT ( 'NONE',  ( 8.405692050792682224, 12.75046512599275772, -0.7216878364870328300 ) ) ;
#153963 = CARTESIAN_POINT ( 'NONE',  ( 0.1747926744264712562, 2.889263262932476817, -2.344248796821886138 ) ) ;
#153965 = CARTESIAN_POINT ( 'NONE',  ( 6.063827332385394620, 1.649827434358666967, -1.158513616066357832 ) ) ;
#153966 = CARTESIAN_POINT ( 'NONE',  ( 5.753135696777640362, 0.1336808224800915823, -1.911095040969860825 ) ) ;
#153967 = CARTESIAN_POINT ( 'NONE',  ( 6.539320575229290000, 0.004092658091040673150, 2.003502637948690879 ) ) ;
#153968 = CARTESIAN_POINT ( 'NONE',  ( 3.439196427729715566, -1.660734982795486481, -1.430121640581413889 ) ) ;
#153969 = CARTESIAN_POINT ( 'NONE',  ( -1.500000000000013101, 2.452083334016154748, 0.8660254037844403729 ) ) ;
#153970 = CARTESIAN_POINT ( 'NONE',  ( 2.918110517850933672, -1.910018876965378309, 0.09814724848770939314 ) ) ;
#153971 = CARTESIAN_POINT ( 'NONE',  ( -5.850506979496850057, 6.784345216623154151, -1.199719254218446718 ) ) ;
#153972 = CARTESIAN_POINT ( 'NONE',  ( 3.497640442201256139, 7.024404915969360452, 1.040834085586084257E-14 ) ) ;
#153974 = CARTESIAN_POINT ( 'NONE',  ( 0.6500178175347063325, 0.9963223104369984817, 1.753020061881370051 ) ) ;
#153973 = CYLINDRICAL_SURFACE ( 'NONE', #66495, 0.3999999999999997446 ) ;
#153975 = CARTESIAN_POINT ( 'NONE',  ( -0.6823417656250003738, 10.46354166700806587, 1.181850606188754593 ) ) ;
#153977 = CARTESIAN_POINT ( 'NONE',  ( -6.791708605802965870, 6.888357893050385705, -0.7998128361456362523 ) ) ;
#153976 = CARTESIAN_POINT ( 'NONE',  ( 6.550331612656306035, -1.695486744446069727, 1.388264742925699569 ) ) ;
#153979 = ORIENTED_EDGE ( 'NONE', *, *, #33879, .T. ) ;
#153978 = CARTESIAN_POINT ( 'NONE',  ( 3.399128784836574990, 1.359029604673635871, 1.061868196530877384 ) ) ;
#153980 = CARTESIAN_POINT ( 'NONE',  ( 6.608709811657416999, 9.797579649320619311, -1.199719254218440723 ) ) ;
#153981 = CARTESIAN_POINT ( 'NONE',  ( 4.660252114795294887, 6.460046772059735432, -1.599625672291256295 ) ) ;
#153982 = FACE_OUTER_BOUND ( 'NONE', #12938, .T. ) ;
#153983 = CARTESIAN_POINT ( 'NONE',  ( 0.1507198084474276056, -0.4258245693303016610, -1.922078969575198526 ) ) ;
#153984 = CARTESIAN_POINT ( 'NONE',  ( 3.330499290451326200, 7.037332938835193730, -0.7998128361456291469 ) ) ;
#153985 = DIRECTION ( 'NONE',  ( -3.491481338843133750E-15, -0.000000000000000000, -1.000000000000000000 ) ) ;
#153986 = VERTEX_POINT ( 'NONE', #138548 ) ;
#153987 = CARTESIAN_POINT ( 'NONE',  ( 0.000000000000000000, -2.000000000000001776, 0.000000000000000000 ) ) ;
#153988 = ORIENTED_EDGE ( 'NONE', *, *, #174354, .T. ) ;
#153989 = CARTESIAN_POINT ( 'NONE',  ( 3.914574264990647201, -0.5719694332564858597, -1.718857104472475861 ) ) ;
#153990 = STYLED_ITEM ( 'NONE', ( #169156 ), #93359 ) ;
#153991 = ORIENTED_EDGE ( 'NONE', *, *, #43201, .F. ) ;
#153992 = CARTESIAN_POINT ( 'NONE',  ( 9.890836756369282057, 11.49806328964105617, -1.199719254218440723 ) ) ;
#153993 = CARTESIAN_POINT ( 'NONE',  ( 3.573456005653643519, 6.326726552307992080, -1.199719254218453823 ) ) ;
#153994 = CARTESIAN_POINT ( 'NONE',  ( 4.863805359840983833, 0.5633507197577434233, -1.721726771216978369 ) ) ;
#153995 = CARTESIAN_POINT ( 'NONE',  ( 6.170369307550816806, 9.252495721234380355, 1.082531754730549967 ) ) ;
#153996 = LINE ( 'NONE', #87922, #41937 ) ;
#153997 = CARTESIAN_POINT ( 'NONE',  ( 5.811422509517683466, 6.026224704000590293, 0.4751317933852049480 ) ) ;
#153998 = EDGE_CURVE ( 'NONE', #179867, #40807, #40569, .T. ) ;
#154000 = CARTESIAN_POINT ( 'NONE',  ( 1.364683531250000303, 14.50520833367473372, -0.7879004041258355073 ) ) ;
#153999 = CARTESIAN_POINT ( 'NONE',  ( 5.037489322368606359, 1.736649509538616964, -0.6695082933049227858 ) ) ;
#154001 = CARTESIAN_POINT ( 'NONE',  ( 2.565921762024740982, -0.9824477935329900546, 1.644319621262643638 ) ) ;
#154002 = CARTESIAN_POINT ( 'NONE',  ( -15.75000000000000000, 10.19999999999998153, 3.199999999999997957 ) ) ;
#154003 = CARTESIAN_POINT ( 'NONE',  ( -10.94029418865078362, 4.766281873824294024, -4.419956640179717233 ) ) ;
#154004 = MECHANICAL_DESIGN_GEOMETRIC_PRESENTATION_REPRESENTATION (  '', ( #192010 ), #88274 ) ;
#154005 =( NAMED_UNIT ( * ) SI_UNIT ( $, .STERADIAN. ) SOLID_ANGLE_UNIT ( ) );
#154006 = CARTESIAN_POINT ( 'NONE',  ( 6.925078400183556582, 1.239878965558613100, 2.257517960274834756 ) ) ;
#154007 = CARTESIAN_POINT ( 'NONE',  ( 6.155038550924133212, 10.12470270947942730, 0.7216878364870438212 ) ) ;
#154008 = CARTESIAN_POINT ( 'NONE',  ( -4.060830702492950195, 4.696389560118578999, -1.199719254218452047 ) ) ;
#154010 = EDGE_CURVE ( 'NONE', #79400, #154255, #200311, .T. ) ;
#154009 = MECHANICAL_DESIGN_GEOMETRIC_PRESENTATION_REPRESENTATION (  '', ( #140119 ), #192020 ) ;
#154011 = CARTESIAN_POINT ( 'NONE',  ( 1.025464405625675646, -1.327728713622891688, -1.614889332886438655 ) ) ;
#154012 = CARTESIAN_POINT ( 'NONE',  ( 6.039231080244466199, 6.010467446565510130, 0.7998128361456352531 ) ) ;
#154013 = CARTESIAN_POINT ( 'NONE',  ( 6.370143239528382573, 0.9910226482379416169, 1.651782778771145432 ) ) ;
#154014 = CARTESIAN_POINT ( 'NONE',  ( -4.042302355168801320, 7.867769847672247074, 0.7998128361456341429 ) ) ;
#154015 = CARTESIAN_POINT ( 'NONE',  ( 2.836711209001481659, 0.2215568149019596367, 1.812007907362273018 ) ) ;
#154016 = CARTESIAN_POINT ( 'NONE',  ( 11.57754556164262993, 8.947311289249686439, -4.715264992745044736 ) ) ;
#154017 = CARTESIAN_POINT ( 'NONE',  ( 1.775505761281343631, 0.3235837346332003372, -1.884644527778083001 ) ) ;
#154018 = CARTESIAN_POINT ( 'NONE',  ( 1.609744333363828384, 0.5749553099084430130, -1.883740962975283706 ) ) ;
#154019 = CARTESIAN_POINT ( 'NONE',  ( 3.474105628906531518, -1.872487600191057755, -0.5149888314514885490 ) ) ;
#154020 = ORIENTED_EDGE ( 'NONE', *, *, #157920, .F. ) ;
#154021 = CARTESIAN_POINT ( 'NONE',  ( 0.7499999999999902300, 3.264583334016149418, 1.299038105676669330 ) ) ;
#154022 = CARTESIAN_POINT ( 'NONE',  ( -4.359828915246279024, 7.244161613499399799, -1.199719254218455378 ) ) ;
#154024 = CARTESIAN_POINT ( 'NONE',  ( 4.394861267144759331, -2.057662932662501110, -0.5123870273424437904 ) ) ;
#154023 = CARTESIAN_POINT ( 'NONE',  ( 5.969332771766739931, 10.18624834369502885, -0.7998128361456481317 ) ) ;
#154025 = CARTESIAN_POINT ( 'NONE',  ( 6.770610912236884715, -7.154544010627095219, 6.663994888585883736 ) ) ;
#154026 = CARTESIAN_POINT ( 'NONE',  ( 10.08456733046637765, 10.65975006183261087, 0.000000000000000000 ) ) ;
#154027 = CARTESIAN_POINT ( 'NONE',  ( -6.557303570864871034, 7.679217583210999010, -1.199719254218452047 ) ) ;
#154028 = CARTESIAN_POINT ( 'NONE',  ( 3.606105671554957759, 4.269840040644637291, -1.082531754730543083 ) ) ;
#154029 = ORIENTED_EDGE ( 'NONE', *, *, #35597, .F. ) ;
#154030 = CARTESIAN_POINT ( 'NONE',  ( 6.119526231721748033, 8.232809585132461194, 1.599625672291269396 ) ) ;
#154031 = FACE_OUTER_BOUND ( 'NONE', #54119, .T. ) ;
#154032 = CARTESIAN_POINT ( 'NONE',  ( 3.545350327189537687, -1.383302465072188792, -1.191577590537174158 ) ) ;
#154033 = CYLINDRICAL_SURFACE ( 'NONE', #94076, 1.500000000000000222 ) ;
#154034 = CARTESIAN_POINT ( 'NONE',  ( -9.991996023591624976, 10.75967623705280296, 1.040834085586084257E-14 ) ) ;
#154035 = CARTESIAN_POINT ( 'NONE',  ( -4.584908210271880336, 8.498668195373706880, -0.01721603403951645073 ) ) ;
#154036 = CARTESIAN_POINT ( 'NONE',  ( 2.449293598294706414E-16, -4.500000000000003553, -2.000000000000000000 ) ) ;
#154037 = CARTESIAN_POINT ( 'NONE',  ( 4.205816867194319464, -1.865656749788859647, 0.1373567816406878750 ) ) ;
#154038 = CARTESIAN_POINT ( 'NONE',  ( 9.237182729612253951, 9.671134694169463586, 0.7998128361456462443 ) ) ;
#154040 = EDGE_CURVE ( 'NONE', #154752, #69931, #120227, .T. ) ;
#154039 = CARTESIAN_POINT ( 'NONE',  ( 2.473164231231731680, 0.09456843629558449316, -1.924295592635028029 ) ) ;
#154041 = CARTESIAN_POINT ( 'NONE',  ( 6.614115624646348834, 1.956711779489667125, -0.1410536379464824575 ) ) ;
#154042 = CARTESIAN_POINT ( 'NONE',  ( -0.6823417656250003738, 8.713541667008065872, 1.181850606188754593 ) ) ;
#154043 = CARTESIAN_POINT ( 'NONE',  ( -6.039267359883488950, 9.133230122250985517, 1.199719254218452047 ) ) ;
#154044 = CARTESIAN_POINT ( 'NONE',  ( 3.174580523894166006, 6.855427711185178019, 0.7998128361456341429 ) ) ;
#154045 = CARTESIAN_POINT ( 'NONE',  ( -5.614485009390564940, 5.722856397143323726, 0.000000000000000000 ) ) ;
#154046 = CARTESIAN_POINT ( 'NONE',  ( 1.247838713208373029, 2.085211562554165621, -0.3660346322543471809 ) ) ;
#154047 = CARTESIAN_POINT ( 'NONE',  ( 10.38962578677386084, 11.01565159419135043, 0.000000000000000000 ) ) ;
#154049 = EDGE_CURVE ( 'NONE', #99270, #195556, #62679, .T. ) ;
#154048 = DIRECTION ( 'NONE',  ( -0.000000000000000000, -8.546850786086437571E-32, -1.000000000000000000 ) ) ;
#154050 = CARTESIAN_POINT ( 'NONE',  ( 5.137584473783054051, 1.933663220787355419, -0.7400441640052906056 ) ) ;
#154052 = CARTESIAN_POINT ( 'NONE',  ( 1.364683531249986537, 2.217708333674751398, -0.7879004041258239610 ) ) ;
#154051 = CARTESIAN_POINT ( 'NONE',  ( 0.4152503475762688856, -0.9843521281015167324, -1.555853522519357934 ) ) ;
#154053 = ORIENTED_EDGE ( 'NONE', *, *, #10280, .F. ) ;
#154054 = CARTESIAN_POINT ( 'NONE',  ( 5.520273603857641653, -2.079230528169520031, 0.9805040003046764374 ) ) ;
#154055 = CARTESIAN_POINT ( 'NONE',  ( 5.829642864196157070, 8.784705193995428374, 1.082531754730558626 ) ) ;
#154057 = CARTESIAN_POINT ( 'NONE',  ( -8.915975476025518986, 3.467171072964058354, -8.027980377473689089 ) ) ;
#154056 = CARTESIAN_POINT ( 'NONE',  ( 3.607878275012313285, 6.262922849939428716, 1.082531754730549078 ) ) ;
#154058 = CARTESIAN_POINT ( 'NONE',  ( 1.728911070687192186, 0.2280534122649588435, 2.280891765651926750 ) ) ;
#154059 = CARTESIAN_POINT ( 'NONE',  ( 5.063152511717405879, 4.908155404373435005, -0.2552525419090029835 ) ) ;
#154060 = CARTESIAN_POINT ( 'NONE',  ( -7.123883369337781879, 7.275895117174344229, 0.7998128361456341429 ) ) ;
#154061 = ADVANCED_FACE ( 'NONE', ( #42941 ), #176131, .T. ) ;
#154062 = CARTESIAN_POINT ( 'NONE',  ( 5.560475942038150876, -1.756435177671934911, -0.8285927890409640062 ) ) ;
#154063 = ORIENTED_EDGE ( 'NONE', *, *, #62788, .F. ) ;
#154064 = CARTESIAN_POINT ( 'NONE',  ( 8.554831740098659765, 10.04335378727902395, 1.082531754730558626 ) ) ;
#154065 = ORIENTED_EDGE ( 'NONE', *, *, #210306, .F. ) ;
#154066 = CARTESIAN_POINT ( 'NONE',  ( -0.1931356145602729502, -0.4479747710816587292, -1.970277229543435427 ) ) ;
#154067 = CARTESIAN_POINT ( 'NONE',  ( 5.296111364736042937, -0.9110065213352031011, -1.799124599017036585 ) ) ;
#154069 = CARTESIAN_POINT ( 'NONE',  ( 11.07790593930098311, 12.30000000000000071, 0.6999999999999992895 ) ) ;
#154068 = CARTESIAN_POINT ( 'NONE',  ( -7.167456763118792651, 11.51378332361394818, 0.000000000000000000 ) ) ;
#154070 = CARTESIAN_POINT ( 'NONE',  ( 3.285556943750000070, -2.471874999522040373, 0.000000000000000000 ) ) ;
#154072 = CARTESIAN_POINT ( 'NONE',  ( 1.445802646165544880, 1.767618460842989014, 0.09138547110125286310 ) ) ;
#154071 = CARTESIAN_POINT ( 'NONE',  ( 2.238330470135694750, 0.4590858415520538416, 2.039436070248427324 ) ) ;
#154073 = CARTESIAN_POINT ( 'NONE',  ( 9.367496997597598352, 4.518459255872631530, -7.500000000000005329 ) ) ;
#154074 = CARTESIAN_POINT ( 'NONE',  ( 3.697495799125404492, -0.6661743112182354487, 2.193330854740268343 ) ) ;
#154075 = CARTESIAN_POINT ( 'NONE',  ( 3.820004643325402238, 1.653240603489447569, 0.5438404159014453843 ) ) ;
#154076 = CARTESIAN_POINT ( 'NONE',  ( 2.544126380858701797, 6.119897877643793116, 0.7998128361456462443 ) ) ;
#154077 = CARTESIAN_POINT ( 'NONE',  ( -4.869786032514803686, 4.879826965026095031, -0.6311548526560835093 ) ) ;
#154078 = CARTESIAN_POINT ( 'NONE',  ( 2.618122797784384836, 0.4666061159355525678, -1.669766330342295158 ) ) ;
#154079 = CARTESIAN_POINT ( 'NONE',  ( 3.332658328316660423, -1.295540365661397297, 1.742140367482351238 ) ) ;
#154080 = CARTESIAN_POINT ( 'NONE',  ( 5.172599298813543633, 5.993452922492633839, -1.199719254218452047 ) ) ;
#154081 = CARTESIAN_POINT ( 'NONE',  ( 4.434779938697545276, -1.616694733667634942, 1.205040202231235869 ) ) ;
#154082 = CARTESIAN_POINT ( 'NONE',  ( 2.625000000000002665, -2.052068128417949833, 1.560916121760785068E-13 ) ) ;
#154083 = CARTESIAN_POINT ( 'NONE',  ( -1.499999999999997780, 2.931250000682818158, 1.214306433183764966E-14 ) ) ;
#154084 = CARTESIAN_POINT ( 'NONE',  ( 0.7449895426413064570, -1.653788825565579046, 0.9876836116205435223 ) ) ;
#154085 = CARTESIAN_POINT ( 'NONE',  ( -0.7500000000000179856, 8.822916667349467446, 1.299038105676658228 ) ) ;
#154086 = CARTESIAN_POINT ( 'NONE',  ( 4.482826657505923684, -1.449732756002309664, 1.683255901693592849 ) ) ;
#154087 = ORIENTED_EDGE ( 'NONE', *, *, #80889, .F. ) ;
#154088 = FACE_OUTER_BOUND ( 'NONE', #210179, .T. ) ;
#154089 = CARTESIAN_POINT ( 'NONE',  ( -1.500000000000013101, 0.6708333333333583726, 0.8660254037844403729 ) ) ;
#154090 = CARTESIAN_POINT ( 'NONE',  ( 6.577677080924314801, 10.82570702772039262, 1.040834085586084257E-14 ) ) ;
#154091 = CARTESIAN_POINT ( 'NONE',  ( 6.629573926958101993, 6.836850457647000390, -0.7216878364870257245 ) ) ;
#154092 = CARTESIAN_POINT ( 'NONE',  ( -1.642778471875000035, -1.217708332855376607, -2.845375778867859751 ) ) ;
#154093 = CARTESIAN_POINT ( 'NONE',  ( 0.6982527715983916083, 1.495984496936525021, 1.642170479989105480 ) ) ;
#154094 = CARTESIAN_POINT ( 'NONE',  ( 5.740667459973674447, -1.913685094937540132, -0.4313615418530327150 ) ) ;
#154095 = CARTESIAN_POINT ( 'NONE',  ( 8.215877900201359552, 11.56864606933486606, -1.082531754730543083 ) ) ;
#154096 = CARTESIAN_POINT ( 'NONE',  ( 0.4214394802095830506, -0.1064560406111268731, 2.159113264384164399 ) ) ;
#154097 = PRESENTATION_LAYER_ASSIGNMENT (  '', '', ( #164440 ) ) ;
#154098 = CARTESIAN_POINT ( 'NONE',  ( -5.478903473698260029, 6.525047153136981137, -1.082531754730549967 ) ) ;
#154099 = CARTESIAN_POINT ( 'NONE',  ( 3.525881619439541037, 2.013048741316531220, -0.4491155694474731619 ) ) ;
#154100 = CARTESIAN_POINT ( 'NONE',  ( -5.253948220495577637, 6.088359997788290734, 1.199719254218450271 ) ) ;
#154101 = TOROIDAL_SURFACE ( 'NONE', #26067, 6.399999999999999467, 0.2000000000000000111 ) ;
#154102 = CARTESIAN_POINT ( 'NONE',  ( -1.500000000000011324, 4.410416667349484676, -0.8660254037844313801 ) ) ;
#154103 = CARTESIAN_POINT ( 'NONE',  ( -1.001543065824772872E-14, 5.384375000341415252, 1.575800808251672791 ) ) ;
#154104 = CARTESIAN_POINT ( 'NONE',  ( 5.167206475355686557, 0.1846639555213614448, -1.861428779493356167 ) ) ;
#154105 = CARTESIAN_POINT ( 'NONE',  ( 4.113671241589770489, 0.09026135180613574505, 1.731944212183807341 ) ) ;
#154106 = CARTESIAN_POINT ( 'NONE',  ( 3.139928233896288390, 0.4259470162499751633, 1.687361108405739385 ) ) ;
#154107 = CARTESIAN_POINT ( 'NONE',  ( 0.4863598079122740114, -2.275998871909711951, -0.2730087134108442615 ) ) ;
#154108 = CARTESIAN_POINT ( 'NONE',  ( 1.364683531249988535, 4.426041667008082214, 0.7879004041258500513 ) ) ;
#154109 = CARTESIAN_POINT ( 'NONE',  ( 4.968349523292523884, -1.969100025901071360, -0.7031758509000278767 ) ) ;
#154110 = CARTESIAN_POINT ( 'NONE',  ( 0.5152501731416662123, -0.9825955030486509534, -1.556829690179861281 ) ) ;
#154112 = EDGE_LOOP ( 'NONE', ( #113205, #209353 ) ) ;
#154111 = CARTESIAN_POINT ( 'NONE',  ( 0.04536292375656306164, -10.00000000000004441, 10.91964218157388267 ) ) ;
#154113 = CARTESIAN_POINT ( 'NONE',  ( 0.8619541869999207684, -0.05229984143813663777, -2.015912905633105101 ) ) ;
#154114 = CARTESIAN_POINT ( 'NONE',  ( 1.143014088299774578, 2.045220145331683614, 0.5602274146137007360 ) ) ;
#154115 = CARTESIAN_POINT ( 'NONE',  ( 6.825078400183547167, -0.008500281443135963844, 2.244262395727573356 ) ) ;
#154116 = CARTESIAN_POINT ( 'NONE',  ( 0.000000000000000000, -0.5000000000000004441, 0.000000000000000000 ) ) ;
#154117 = CARTESIAN_POINT ( 'NONE',  ( -7.503547950159405566, 10.84155747757291266, 1.199719254218453823 ) ) ;
#154118 = CARTESIAN_POINT ( 'NONE',  ( 5.900823170445728572, 7.907379670318584353, 1.599625672291267398 ) ) ;
#154119 = CARTESIAN_POINT ( 'NONE',  ( 2.508575005364023003, -2.114979441823850337, -0.1534387461676610942 ) ) ;
#154120 = DIRECTION ( 'NONE',  ( 0.000000000000000000, 0.000000000000000000, 1.000000000000000000 ) ) ;
#154121 = CARTESIAN_POINT ( 'NONE',  ( 4.424309136736732206, 1.121156565774838354, -1.440799707636587712 ) ) ;
#154122 = VERTEX_POINT ( 'NONE', #57034 ) ;
#154123 = CARTESIAN_POINT ( 'NONE',  ( -6.095272577795516789, 9.268845886473535245, 1.199719254218452047 ) ) ;
#154124 = EDGE_CURVE ( 'NONE', #164674, #161364, #30688, .T. ) ;
#154125 = CARTESIAN_POINT ( 'NONE',  ( 2.205172540517054802, 5.724451730578533848, 1.040834085586084257E-14 ) ) ;
#154126 = CARTESIAN_POINT ( 'NONE',  ( -3.285556943750000070, -0.1968749995220411830, 0.000000000000000000 ) ) ;
#154127 = CARTESIAN_POINT ( 'NONE',  ( -6.344325816190970357, 9.489131654609717970, 1.199719254218452047 ) ) ;
#154128 = CARTESIAN_POINT ( 'NONE',  ( 2.039325177177089721, 0.004250232316239943575, 2.019972748817438823 ) ) ;
#154129 = CARTESIAN_POINT ( 'NONE',  ( 6.001041448284401447, 1.807427358944500684, -1.265864663738118345 ) ) ;
#154130 = CARTESIAN_POINT ( 'NONE',  ( -3.634467696915153034, 6.397906858779740524, 1.199719254218452935 ) ) ;
#154131 = CARTESIAN_POINT ( 'NONE',  ( 4.205779932802704124, 0.6304169756579135475, -1.751020666094662337 ) ) ;
#154132 = CARTESIAN_POINT ( 'NONE',  ( 8.204655514564224816, 12.72384853363364066, 1.040834085586084257E-14 ) ) ;
#154133 = DIRECTION ( 'NONE',  ( -9.436895709313856232E-16, 0.8656921114426507913, 0.5005768354468325132 ) ) ;
#154134 = EDGE_LOOP ( 'NONE', ( #106893, #58358, #89032, #3564 ) ) ;
#154135 = ORIENTED_EDGE ( 'NONE', *, *, #17378, .T. ) ;
#154136 = CARTESIAN_POINT ( 'NONE',  ( -3.795392936821753604, 6.515376628678959392, -1.199719254218452047 ) ) ;
#154137 = CARTESIAN_POINT ( 'NONE',  ( -7.797910906154257304, 12.24931315715533486, 0.000000000000000000 ) ) ;
#154138 = CARTESIAN_POINT ( 'NONE',  ( 5.145057536039753465, -1.563975785779356587, 0.9416349707431559413 ) ) ;
#154139 = CIRCLE ( 'NONE', #8791, 11.95586206894144965 ) ;
#154141 = CARTESIAN_POINT ( 'NONE',  ( -4.398207409718558836, 7.344456035913847103, -1.221965942340837552 ) ) ;
#154140 = CARTESIAN_POINT ( 'NONE',  ( -5.015590482412729756, 4.816220082428420923, 0.000000000000000000 ) ) ;
#154142 = CARTESIAN_POINT ( 'NONE',  ( 5.269423316188119877, 7.778230059001682406, -1.291559732514224068 ) ) ;
#154143 = CARTESIAN_POINT ( 'NONE',  ( 0.4734851067992265627, 1.504414441068102404, 0.8618086654073161545 ) ) ;
#154144 = CARTESIAN_POINT ( 'NONE',  ( 0.4798830478778244868, -0.2081801751476043960, -1.727770289196085329 ) ) ;
#154145 = CARTESIAN_POINT ( 'NONE',  ( 5.637451635233869496, -2.088540497258955408, 0.9818693799023417990 ) ) ;
#154147 = CARTESIAN_POINT ( 'NONE',  ( 5.662465432362883355, 6.635239754958710989, 1.199719254218451159 ) ) ;
#154146 = B_SPLINE_CURVE_WITH_KNOTS ( 'NONE', 3,
 ( #24803, #89844, #36790, #7481, #119180, #168933 ),
 .UNSPECIFIED., .F., .F.,
 ( 4, 2, 4 ),
 ( 0.000000000000000000, 0.0003779448103413555527, 0.0007558896206827111055 ),
 .UNSPECIFIED. ) ;
#154148 = CARTESIAN_POINT ( 'NONE',  ( 0.9661734561289528900, 1.013198095218909245, 1.794397040888571437 ) ) ;
#154149 = CARTESIAN_POINT ( 'NONE',  ( 6.979750152936881058, 7.037463354714830643, 0.7998128361456341429 ) ) ;
#154150 = CARTESIAN_POINT ( 'NONE',  ( 0.4036724312478366938, 0.3418800534340654118, 1.986742826083332858 ) ) ;
#154151 = DIRECTION ( 'NONE',  ( 0.000000000000000000, 1.000000000000000000, 0.000000000000000000 ) ) ;
#154152 = CARTESIAN_POINT ( 'NONE',  ( -6.180537922983287302, 8.303989891604203422, -1.599625672291271394 ) ) ;
#154153 = CARTESIAN_POINT ( 'NONE',  ( 5.383624799460786647, 1.257121276536907750, 1.385457850027263182 ) ) ;
#154154 = AXIS2_PLACEMENT_3D ( 'NONE', #208851, #43205, #209917 ) ;
#154156 = CARTESIAN_POINT ( 'NONE',  ( -3.797165540279144214, 6.587721009371067638, 1.199719254218452935 ) ) ;
#154155 = CARTESIAN_POINT ( 'NONE',  ( 3.287273477832891366, 0.04233216220104508987, -1.912079899511004433 ) ) ;
#154157 = CARTESIAN_POINT ( 'NONE',  ( 5.496761087669068679, -0.5331231007881258588, -2.141394884921154151 ) ) ;
#154158 = CARTESIAN_POINT ( 'NONE',  ( 0.6124999999999707345, 1.729166667349485431, -1.060881119635955327 ) ) ;
#154159 = CARTESIAN_POINT ( 'NONE',  ( 5.153507786970260796, 7.105788066255672497, -1.443375672974078316 ) ) ;
#154160 = CARTESIAN_POINT ( 'NONE',  ( 5.031484404002889654, 6.003058238492422483, 1.082531754730549078 ) ) ;
#154161 = CIRCLE ( 'NONE', #181808, 6.249999999999995559 ) ;
#154162 = CARTESIAN_POINT ( 'NONE',  ( -4.706088717274938382, 6.583799151611112954, 1.443375672974058777 ) ) ;
#154163 = CARTESIAN_POINT ( 'NONE',  ( 6.217454246653871586, 1.762742247767977055, 1.178343227268910054 ) ) ;
#154164 = ADVANCED_FACE ( 'NONE', ( #23440 ), #113530, .T. ) ;
#154165 = CARTESIAN_POINT ( 'NONE',  ( 3.065757340968386035, 0.3400709678853690021, -2.282286004074239649 ) ) ;
#154166 = CARTESIAN_POINT ( 'NONE',  ( 4.158614545834369736, -0.6132839004606009947, -1.863630207987923004 ) ) ;
#154167 = CARTESIAN_POINT ( 'NONE',  ( 0.3034670832338138835, -1.512625156342655819, -1.248876549296701333 ) ) ;
#154168 = CARTESIAN_POINT ( 'NONE',  ( 3.145128448690309053, 4.692402494937224056, -1.443375672974057666 ) ) ;
#154169 = CARTESIAN_POINT ( 'NONE',  ( 4.634908411025333130, 6.500755460986618495, 1.599625672291268286 ) ) ;
#154170 = ORIENTED_EDGE ( 'NONE', *, *, #110743, .T. ) ;
#154171 = CARTESIAN_POINT ( 'NONE',  ( 5.946499988598237252, -1.422611626450220434, 1.429444749906971790 ) ) ;
#154172 = CARTESIAN_POINT ( 'NONE',  ( -8.136864746495904299, 12.64475930422059768, -0.7998128361456281477 ) ) ;
#154173 = CARTESIAN_POINT ( 'NONE',  ( 0.1988192939417210425, -0.4940924592915455493, 1.773541111592655373 ) ) ;
#154174 = CARTESIAN_POINT ( 'NONE',  ( 3.555704413576792788, 1.708454066091537493, 1.339533783212579099 ) ) ;
#154175 = CARTESIAN_POINT ( 'NONE',  ( 6.039231080244466199, 6.010467446565509242, 0.7998128361456350310 ) ) ;
#154176 = CARTESIAN_POINT ( 'NONE',  ( 0.2641366190093488164, 0.6592694798918593557, -2.015615888626711705 ) ) ;
#154177 = CARTESIAN_POINT ( 'NONE',  ( -0.7500000000000006661, 1.639583334016154970, -1.299038105676652011 ) ) ;
#154178 = CARTESIAN_POINT ( 'NONE',  ( 9.459838494033030898, 12.05956421450382088, 1.599625672291281386 ) ) ;
#154179 = CARTESIAN_POINT ( 'NONE',  ( 0.3999999999999758193, 3.000000000029069636, -2.023857702507768419 ) ) ;
#154180 = CARTESIAN_POINT ( 'NONE',  ( 5.770588788983777917, 7.358121641400980018, 1.301467365913897112 ) ) ;
#154181 = CARTESIAN_POINT ( 'NONE',  ( 0.7200824656817590430, -1.100121004815158177, -1.742362558145001294 ) ) ;
#154183 = CARTESIAN_POINT ( 'NONE',  ( -2.034713692888026060, 8.461455076002922127, -2.499999999999990230 ) ) ;
#154182 = FACE_OUTER_BOUND ( 'NONE', #129955, .T. ) ;
#154184 = CARTESIAN_POINT ( 'NONE',  ( 0.6823417656249882723, 0.9260416670080831025, -1.181850606188749264 ) ) ;
#154185 = DIRECTION ( 'NONE',  ( 0.000000000000000000, 0.000000000000000000, 1.000000000000000000 ) ) ;
#154186 = ORIENTED_EDGE ( 'NONE', *, *, #119166, .T. ) ;
#154187 = CARTESIAN_POINT ( 'NONE',  ( 2.842330330863319876, 1.060513762474508015, -1.591057744338888913 ) ) ;
#154188 = CARTESIAN_POINT ( 'NONE',  ( 5.805463146582474643, -0.4265672176911333713, 1.717519531449087866 ) ) ;
#154189 = CARTESIAN_POINT ( 'NONE',  ( 5.338878628731272613, 9.450718510153643948, -0.7998128361456481317 ) ) ;
#154190 = CARTESIAN_POINT ( 'NONE',  ( -5.199715606040888005, 6.025088614257851027, -1.199719254218446718 ) ) ;
#154191 = CARTESIAN_POINT ( 'NONE',  ( 0.1756362645438137582, 1.791864648875134636, -0.2657654445481233418 ) ) ;
#154193 = CARTESIAN_POINT ( 'NONE',  ( 0.6377201071205064187, 1.913410132493647442, -0.09706281964840141052 ) ) ;
#154192 = CARTESIAN_POINT ( 'NONE',  ( -6.725445687907775749, -7.162053774861877997, 6.710127771514615702 ) ) ;
#154194 = CARTESIAN_POINT ( 'NONE',  ( 2.084514231050747401, 1.193861083872927109, -1.691280048542340708 ) ) ;
#154195 = CARTESIAN_POINT ( 'NONE',  ( -1.402160292154681736E-14, 0.3843750003414230232, 1.575800808251672791 ) ) ;
#154196 = CARTESIAN_POINT ( 'NONE',  ( 6.034044788248046132, 0.9204803733943857091, -1.628451883209979689 ) ) ;
#154197 = CARTESIAN_POINT ( 'NONE',  ( 3.228933428962964758, 0.04559371896543929631, 1.825288036790246204 ) ) ;
#154198 = ADVANCED_FACE ( 'NONE', ( #125316 ), #157748, .T. ) ;
#154200 = CARTESIAN_POINT ( 'NONE',  ( 6.335378924966214242, 6.849830188997488634, 0.6565068261209184852 ) ) ;
#154199 = CARTESIAN_POINT ( 'NONE',  ( 0.3644775225865644619, 2.281660525247240834, -0.3449698035877246105 ) ) ;
#154201 = CARTESIAN_POINT ( 'NONE',  ( -0.6823417656250003738, -0.03229166632524871350, -1.181850606188749264 ) ) ;
#154202 = CARTESIAN_POINT ( 'NONE',  ( 4.123522620141695683, 0.2556129913668835907, -2.046733346555211330 ) ) ;
#154203 = CARTESIAN_POINT ( 'NONE',  ( -7.562750758324527922, 7.717630727667075696, 1.040834085586084257E-14 ) ) ;
#154204 = CARTESIAN_POINT ( 'NONE',  ( 6.805303039055573322, 10.02693841461847057, 1.199719254218460707 ) ) ;
#154205 = CARTESIAN_POINT ( 'NONE',  ( 5.840865249388944136, 5.708764300575555950, 0.7998128361456341429 ) ) ;
#154206 = CARTESIAN_POINT ( 'NONE',  ( 0.3511320849261707622, -1.736299752564632204, 1.287366282644891724 ) ) ;
#154207 = CARTESIAN_POINT ( 'NONE',  ( 6.742638474511262636, -2.029596885996234334, -0.4079607620106340260 ) ) ;
#154208 = CARTESIAN_POINT ( 'NONE',  ( -1.364683531250012516, 1.592708333674756727, 0.7879004041258379498 ) ) ;
#154209 = CARTESIAN_POINT ( 'NONE',  ( 4.183022562662654487, -0.2072598778708051315, -2.151613130492259440 ) ) ;
#154210 = CARTESIAN_POINT ( 'NONE',  ( 4.283856624473350472, 1.958454427565621048, -0.4929297443572661641 ) ) ;
#154213 = CARTESIAN_POINT ( 'NONE',  ( 7.456621297836082185, 7.801739057004660971, 0.7216878364870317197 ) ) ;
#154212 = CARTESIAN_POINT ( 'NONE',  ( 3.285556943749998737, -3.755208332855373587, -1.896917185911906500 ) ) ;
#154211 = CARTESIAN_POINT ( 'NONE',  ( 0.4499999999999677591, 3.999999999999961808, -0.8338124244296144516 ) ) ;
#154214 = CARTESIAN_POINT ( 'NONE',  ( -4.847922445338252118, 7.813604065273374921, -1.199719254218453823 ) ) ;
#154215 = CARTESIAN_POINT ( 'NONE',  ( 2.993375309983861143, -0.3886322325962355273, 1.978555244300662874 ) ) ;
#154216 = CARTESIAN_POINT ( 'NONE',  ( -6.364663046611467756, 9.512858423433634414, 1.199719254218452047 ) ) ;
#154218 = DIRECTION ( 'NONE',  ( 0.000000000000000000, 0.000000000000000000, -1.000000000000000000 ) ) ;
#154217 = CARTESIAN_POINT ( 'NONE',  ( -2.740719608256871442, 6.349256642941639051, 0.7998128361456341429 ) ) ;
#154219 = CARTESIAN_POINT ( 'NONE',  ( 3.809477975315520570, 7.388215371269448717, -0.7216878364869808715 ) ) ;
#154220 = CARTESIAN_POINT ( 'NONE',  ( 6.310809538426106258, -0.5167911955388967415, -1.841158844219364044 ) ) ;
#154221 = DIRECTION ( 'NONE',  ( 1.040834085586084257E-15, 1.000000000000000000, -4.622230424712076367E-32 ) ) ;
#154222 = CARTESIAN_POINT ( 'NONE',  ( 5.300874872818830852, 7.207439989753867238, 1.443375672974062551 ) ) ;
#154224 = CARTESIAN_POINT ( 'NONE',  ( 4.675407748274028386, 1.496063595514389943, 1.352143027241403450 ) ) ;
#154223 = CARTESIAN_POINT ( 'NONE',  ( -8.636180661780672452, 9.177891648273343250, -0.7216878364870267237 ) ) ;
#154225 = CARTESIAN_POINT ( 'NONE',  ( -1.500000000000011324, 5.129166666666691299, -0.8660254037844313801 ) ) ;
#154226 = CARTESIAN_POINT ( 'NONE',  ( -0.6823417656250039265, 14.88020833367473195, -1.181850606188755259 ) ) ;
#154227 = CARTESIAN_POINT ( 'NONE',  ( 6.211878148792838061, -1.711051158068075839, 0.2163953478501578487 ) ) ;
#154228 = CARTESIAN_POINT ( 'NONE',  ( 5.899733120602060232, 6.912052057904395141, -1.199719254218452047 ) ) ;
#154230 = CARTESIAN_POINT ( 'NONE',  ( -5.111060722671894929, 5.065251719313053513, 0.000000000000000000 ) ) ;
#154229 = CARTESIAN_POINT ( 'NONE',  ( 8.595506201384004896, 12.01154575404795466, 1.082531754730546636 ) ) ;
#154231 = CARTESIAN_POINT ( 'NONE',  ( -0.3728825314829262716, 3.227879828479837343, 0.5317689764002340169 ) ) ;
#154232 = CARTESIAN_POINT ( 'NONE',  ( 5.132044594934622062, 0.9627672477196843603, -1.603626212978970900 ) ) ;
#154233 =( BOUNDED_CURVE ( )  B_SPLINE_CURVE ( 2, ( #136278, #137349, #50740, #33422, #151458, #202298, #37699, #201234, #3030 ),
 .UNSPECIFIED., .F., .T. ) 
 B_SPLINE_CURVE_WITH_KNOTS ( ( 3, 2, 2, 2, 3 ),
 ( 0.5625000000000000000, 0.5654761904761904656, 0.5714285714285713969, 0.5773809523809523281, 0.5803571428571429047 ),
 .UNSPECIFIED. ) 
 CURVE ( )  GEOMETRIC_REPRESENTATION_ITEM ( )  RATIONAL_B_SPLINE_CURVE ( ( 0.9330127018922194093, 0.9330127018922194093, 1.000000000000000000, 0.8660254037844387076, 1.000000000000000000, 0.8660254037844387076, 1.000000000000000000, 0.9330127018922180770, 0.9330127018922194093 ) ) 
 REPRESENTATION_ITEM ( '' )  );
#154234 = CARTESIAN_POINT ( 'NONE',  ( 0.2584475630193752149, 2.007833436562710183, 0.1460894178599257687 ) ) ;
#154235 = CARTESIAN_POINT ( 'NONE',  ( -4.138282870000122848, 7.235124601197615135, 0.9996976134348694032 ) ) ;
#154236 = CARTESIAN_POINT ( 'NONE',  ( 1.991162705694597301, 0.1987741427678466344, 2.060657922996151914 ) ) ;
#154237 = CARTESIAN_POINT ( 'NONE',  ( -8.068510813464099485, 8.585886501895810596, 0.7216878364870317197 ) ) ;
#154238 = VERTEX_POINT ( 'NONE', #110119 ) ;
#154239 = CARTESIAN_POINT ( 'NONE',  ( 10.07334494482924292, 11.81495252613139257, -1.082531754730537088 ) ) ;
#154240 = CARTESIAN_POINT ( 'NONE',  ( 0.7203276360899166786, 1.987051886588153682, 0.3419113104980234241 ) ) ;
#154241 = CARTESIAN_POINT ( 'NONE',  ( 0.8436869049191192405, -1.150191864323051982, -1.399547552825676666 ) ) ;
#154242 = ADVANCED_FACE ( 'NONE', ( #159866 ), #11468, .F. ) ;
#154243 = CARTESIAN_POINT ( 'NONE',  ( 4.868786560638896255, 5.813244087901094481, 1.082531754730549078 ) ) ;
#154244 = CARTESIAN_POINT ( 'NONE',  ( -0.07933194154488912297, 7.849261790823902629, 9.499668754385634628 ) ) ;
#154245 = CARTESIAN_POINT ( 'NONE',  ( 7.497295758232718654, 9.769931022736756177, -1.443375672974058777 ) ) ;
#154246 = AXIS2_PLACEMENT_3D ( 'NONE', #16670, #46021, #82754 ) ;
#154247 = CARTESIAN_POINT ( 'NONE',  ( 6.238723240582662477, 10.43026088065513513, -0.7998128361456291469 ) ) ;
#154249 = CARTESIAN_POINT ( 'NONE',  ( 6.274997412412571585, 1.664062557780759066, -0.9488046768871650771 ) ) ;
#154248 = CARTESIAN_POINT ( 'NONE',  ( -6.880926654135487652, 7.986501503701545879, 1.199719254218450271 ) ) ;
#154250 = CARTESIAN_POINT ( 'NONE',  ( 11.04536101718726293, 13.40000000000000036, 1.099999999999996758 ) ) ;
#154251 = CARTESIAN_POINT ( 'NONE',  ( -2.769334607113469904, -3.219464545100549469, 1.817267084746972516 ) ) ;
#154252 = VECTOR ( 'NONE', #114418, 1000.000000000000000 ) ;
#154253 = CARTESIAN_POINT ( 'NONE',  ( -1.364683531250000748, -1.178124999658580752, 0.000000000000000000 ) ) ;
#154255 = VERTEX_POINT ( 'NONE', #190215 ) ;
#154254 = CARTESIAN_POINT ( 'NONE',  ( 5.016153647376217606, 4.954526798134778254, 0.7216878364870317197 ) ) ;
#154256 = CARTESIAN_POINT ( 'NONE',  ( -4.298098390732130625, 4.973201863064262263, 1.199719254218462483 ) ) ;
#154257 = CARTESIAN_POINT ( 'NONE',  ( -7.049876689426103127, 10.20831132343037062, -1.082531754730537976 ) ) ;
#154258 = CARTESIAN_POINT ( 'NONE',  ( 2.624079441566569582, -1.243859440641072123, -1.767801033134681843 ) ) ;
#154259 = CARTESIAN_POINT ( 'NONE',  ( -7.485510208520816278, 8.866088343763324886, 1.082531754730549078 ) ) ;
#154260 = EDGE_CURVE ( 'NONE', #212749, #190586, #107046, .T. ) ;
#154261 = CARTESIAN_POINT ( 'NONE',  ( 6.211043768836173484, 8.339580045099285854, 1.443375672974065660 ) ) ;
#154262 = CARTESIAN_POINT ( 'NONE',  ( 1.353939357992512305, -1.539690173578952770, -1.458446627980537480 ) ) ;
#154263 = CARTESIAN_POINT ( 'NONE',  ( 5.631824825758743991, -1.159798792365024145, -1.409841961918213427 ) ) ;
#154264 = CARTESIAN_POINT ( 'NONE',  ( 2.372288100061814564, -1.215664946315485606, 1.551802774678180619 ) ) ;
#154265 = CARTESIAN_POINT ( 'NONE',  ( 4.131050151015442928, 1.750605847248308145, 0.7702136748066327199 ) ) ;
#154266 = VERTEX_POINT ( 'NONE', #92757 ) ;
#154267 = FACE_OUTER_BOUND ( 'NONE', #81773, .T. ) ;
#154268 = CARTESIAN_POINT ( 'NONE',  ( 4.896905686981484429, 0.3346149513497528871, 1.940740247813901087 ) ) ;
#154269 = CARTESIAN_POINT ( 'NONE',  ( 0.5505969416323712728, -1.640064848914600804, -1.039604180477508688 ) ) ;
#154270 = ORIENTED_EDGE ( 'NONE', *, *, #153040, .T. ) ;
#154271 = CARTESIAN_POINT ( 'NONE',  ( -5.285699784481336927, 7.260012063351913625, 1.599625672291263179 ) ) ;
#154272 = CARTESIAN_POINT ( 'NONE',  ( -4.309512724297390740, 6.121127159803966933, 1.599625672291270506 ) ) ;
#154274 = CARTESIAN_POINT ( 'NONE',  ( 5.017926250389229459, 8.868348035513836436, 0.000000000000000000 ) ) ;
#154273 = CARTESIAN_POINT ( 'NONE',  ( 6.747154001095143627, 11.02343010125301959, -0.7998128361456291469 ) ) ;
#154276 = ORIENTED_EDGE ( 'NONE', *, *, #82451, .T. ) ;
#154275 = CARTESIAN_POINT ( 'NONE',  ( 4.863870654145381778, 0.5962773724161560818, -1.817021391602848812 ) ) ;
#154277 = CARTESIAN_POINT ( 'NONE',  ( 1.044295067165665669, 0.8929887407379887287, -2.018210024696056148 ) ) ;
#154278 = DIRECTION ( 'NONE',  ( -0.000000000000000000, -1.000000000000000000, -0.000000000000000000 ) ) ;
#154279 = CARTESIAN_POINT ( 'NONE',  ( 6.041657904462632622, -1.894779907254999118, 0.6802824325803021877 ) ) ;
#154280 = CARTESIAN_POINT ( 'NONE',  ( -0.02338929933905046013, 4.099262448077650944, -2.266018688142543258 ) ) ;
#154281 = CARTESIAN_POINT ( 'NONE',  ( 1.782949938078045138, -1.500000000000001332, -2.093702347113241657 ) ) ;
#154282 = DIRECTION ( 'NONE',  ( 0.000000000000000000, 0.000000000000000000, 1.000000000000000000 ) ) ;
#154283 = CARTESIAN_POINT ( 'NONE',  ( 2.629418614236479712, 0.1040367438073786233, -2.067886086930009970 ) ) ;
#154284 = CARTESIAN_POINT ( 'NONE',  ( -5.364222332501225488, 9.410009821226765325, 0.7998128361456481317 ) ) ;
#154285 = CARTESIAN_POINT ( 'NONE',  ( -4.613315975161869531, 8.372148359400446438, -0.1986654441144524719 ) ) ;
#154287 = CARTESIAN_POINT ( 'NONE',  ( 0.5148121308554790554, 1.489681748880047563, -1.566682057046255849 ) ) ;
#154286 = CARTESIAN_POINT ( 'NONE',  ( -3.307299406729781399, 5.945934176904983381, -1.199719254218452935 ) ) ;
#154288 = CARTESIAN_POINT ( 'NONE',  ( 4.584065335196261692, 7.401807753487379848, 1.082531754730549078 ) ) ;
#154289 = CARTESIAN_POINT ( 'NONE',  ( 0.07933194154487524519, -9.609467486116976431, 9.499668754385634628 ) ) ;
#154290 = CARTESIAN_POINT ( 'NONE',  ( -1.364683531250014514, 12.90104166700806232, -0.7879004041258335089 ) ) ;
#154292 = CARTESIAN_POINT ( 'NONE',  ( -4.118644803501354978, 8.027112380718707030, 0.7998128361456352531 ) ) ;
#154291 = CARTESIAN_POINT ( 'NONE',  ( 6.925078400183553029, 6.037155338232472523, 2.550556537725846340 ) ) ;
#154293 = CARTESIAN_POINT ( 'NONE',  ( 4.271880269886525916, 1.546599990029189575, -0.7845881139060503218 ) ) ;
#154294 = CARTESIAN_POINT ( 'NONE',  ( -4.790108344329849110, 4.482881244673243337, 0.7998128361456341429 ) ) ;
#154295 = CARTESIAN_POINT ( 'NONE',  ( 2.096617048772158487, 2.047133997803842753, 0.3078910663548983795 ) ) ;
#154296 = CARTESIAN_POINT ( 'NONE',  ( 5.027025340701954725, -1.815278874653761809, 1.089499710131608401 ) ) ;
#154297 = CARTESIAN_POINT ( 'NONE',  ( 6.252281394196331554, 10.44607872653774372, 1.040834085586084257E-14 ) ) ;
#154299 = EDGE_CURVE ( 'NONE', #66068, #12932, #77541, .T. ) ;
#154298 = CARTESIAN_POINT ( 'NONE',  ( -0.6823417656250212460, 5.301041667008086655, 1.181850606188767472 ) ) ;
#154300 = CARTESIAN_POINT ( 'NONE',  ( 2.219528804134728528, 0.3415968887231227713, -1.939435228410562484 ) ) ;
#154301 = CARTESIAN_POINT ( 'NONE',  ( 1.265713261412576562, 0.5522810963098608861, -1.830935845731461953 ) ) ;
#154302 = CARTESIAN_POINT ( 'NONE',  ( 4.945436657225622312, 0.7223393070586077158, -2.175551854680431330 ) ) ;
#154303 = CARTESIAN_POINT ( 'NONE',  ( 2.139018802738294589, -1.631172329757241801, 0.8201644002571031322 ) ) ;
#154304 = VECTOR ( 'NONE', #31797, 1000.000000000000114 ) ;
#154305 = EDGE_CURVE ( 'NONE', #111709, #88893, #25584, .T. ) ;
#154306 = CARTESIAN_POINT ( 'NONE',  ( 3.691562964670865199, 7.528850235416478576, -0.7998128361456362523 ) ) ;
#154307 = CARTESIAN_POINT ( 'NONE',  ( 4.311129659021211147, 7.973475668925984472, 1.040834085586084257E-14 ) ) ;
#154308 = CARTESIAN_POINT ( 'NONE',  ( -6.157374318900681764, 10.33535380535947290, 0.7998128361456481317 ) ) ;
#154309 = CARTESIAN_POINT ( 'NONE',  ( 3.252200647028923974, 0.9015175226297014177, -1.800113812977667038 ) ) ;
#154310 = CARTESIAN_POINT ( 'NONE',  ( 2.887496479553632422, -1.832211488775811414, 0.7015765724691159777 ) ) ;
#154311 = CARTESIAN_POINT ( 'NONE',  ( -7.147119532698295252, 11.49005655479003174, 0.000000000000000000 ) ) ;
#154312 = CARTESIAN_POINT ( 'NONE',  ( -6.261168011412601153, 6.199117522936475666, 1.040834085586084257E-14 ) ) ;
#154313 = DIRECTION ( 'NONE',  ( -0.8660254037844408170, -0.4999999999999962808, -1.110223024625157526E-16 ) ) ;
#154315 = CARTESIAN_POINT ( 'NONE',  ( 4.328786618740396719, 0.08755327933733339507, 1.767792532789840498 ) ) ;
#154314 = CARTESIAN_POINT ( 'NONE',  ( 5.859345120547017949, 2.059885262428410968, -0.3562953063034664525 ) ) ;
#154316 = CARTESIAN_POINT ( 'NONE',  ( -7.721398836998398352, -5.907420853759296264, -7.721398836998357496 ) ) ;
#154317 = CARTESIAN_POINT ( 'NONE',  ( 0.2874129202556953144, 1.626693421326959710, 1.468627725614686463 ) ) ;
#154318 = CARTESIAN_POINT ( 'NONE',  ( -0.1298852118744100725, 0.003815113116375101580, -1.726395881205537330 ) ) ;
#154319 = CARTESIAN_POINT ( 'NONE',  ( 6.938021921891177612, 9.117444880338284818, -1.599625672291262513 ) ) ;
#154320 = CARTESIAN_POINT ( 'NONE',  ( -5.763624699140887486, 5.896852701852046685, -0.7216878364870392693 ) ) ;
#154321 = CARTESIAN_POINT ( 'NONE',  ( 5.713622356042774797, 2.214598200325838206, 0.6159738146167788031 ) ) ;
#154322 = FACE_OUTER_BOUND ( 'NONE', #6385, .T. ) ;
#154323 = CARTESIAN_POINT ( 'NONE',  ( 6.274686883491842337, -1.720241393171379363, 0.2158021260532434760 ) ) ;
#154324 = CARTESIAN_POINT ( 'NONE',  ( 2.297764732281985633, 1.706874461811638044, 1.398895601573101111 ) ) ;
#154325 = CARTESIAN_POINT ( 'NONE',  ( 0.3038947965873342039, -1.677446906807459337, -1.377854473705003580 ) ) ;
#154326 = CARTESIAN_POINT ( 'NONE',  ( 0.000000000000000000, -0.9200000000000041478, -10.91999999999999105 ) ) ;
#154327 = CARTESIAN_POINT ( 'NONE',  ( 1.657563801924813784, 2.024516536105415820, -0.6199660602846206459 ) ) ;
#154328 = CARTESIAN_POINT ( 'NONE',  ( 4.312500000000001776, 1.451031289061289531, 1.451031289060941587 ) ) ;
#154329 = CARTESIAN_POINT ( 'NONE',  ( 6.727182134110200273, -0.004969159814478123736, 2.189081792362323586 ) ) ;
#154330 = CARTESIAN_POINT ( 'NONE',  ( 4.401339437636656804, 1.546884307994823793, 1.147896415085915667 ) ) ;
#154331 = EDGE_LOOP ( 'NONE', ( #204281, #142869, #107857, #63939, #134833 ) ) ;
#154333 = CARTESIAN_POINT ( 'NONE',  ( 0.6823417656249882723, -1.094791666325249713, 1.181850606188755259 ) ) ;
#154332 = CARTESIAN_POINT ( 'NONE',  ( 1.400361390298704656, -0.8304178796270310636, -2.136844513788013433 ) ) ;
#154334 = CARTESIAN_POINT ( 'NONE',  ( 4.985647801523278133, 6.839675073242382553, -1.599625672291256295 ) ) ;
#154335 = CARTESIAN_POINT ( 'NONE',  ( 4.971035877704902184, 8.951292290631053916, 1.040834085586084257E-14 ) ) ;
#154336 = CARTESIAN_POINT ( 'NONE',  ( 4.090652671443067767, -1.278631810133125546, 1.816222553172279319 ) ) ;
#154337 = CARTESIAN_POINT ( 'NONE',  ( -7.483737605063437215, 10.71448239167390604, 1.082531754730549967 ) ) ;
#154338 = CARTESIAN_POINT ( 'NONE',  ( 7.293923454472091450, 7.611924906413328529, 0.7216878364870317197 ) ) ;
#154339 = CARTESIAN_POINT ( 'NONE',  ( -8.066738210006693777, 10.43428054980638997, 1.443375672974090751 ) ) ;
#154340 = CARTESIAN_POINT ( 'NONE',  ( 6.726253606155519371, 7.019919760035800316, -0.7216878364870458196 ) ) ;
#154341 = CARTESIAN_POINT ( 'NONE',  ( 1.740861508391436274, 2.010826320759526720, -0.1511413081683593562 ) ) ;
#154343 = CARTESIAN_POINT ( 'NONE',  ( 6.461391904901197414, 1.712781507706350848, 1.149079448644703350 ) ) ;
#154342 = CARTESIAN_POINT ( 'NONE',  ( 7.884230021546724920, 9.157022099014721306, 1.199719254218462483 ) ) ;
#154344 = CARTESIAN_POINT ( 'NONE',  ( -10.99866081003794882, -6.614835951978810691, 0.2118258318329558909 ) ) ;
#154345 = CARTESIAN_POINT ( 'NONE',  ( 6.061904078641523697, 7.205214525570814210, -1.082531754730548412 ) ) ;
#154346 = CARTESIAN_POINT ( 'NONE',  ( 6.392160974223673797, -0.4739405955596608933, -1.674609590779071455 ) ) ;
#154347 = DIRECTION ( 'NONE',  ( 1.000000000000000000, 0.000000000000000000, 0.000000000000000000 ) ) ;
#154348 = CARTESIAN_POINT ( 'NONE',  ( -1.364683531250012516, 2.738541667008090208, -0.7879004041258289570 ) ) ;
#154349 = CARTESIAN_POINT ( 'NONE',  ( 1.598528592787134883, 1.450519685958560512, -1.013601284844565908 ) ) ;
#154350 = CARTESIAN_POINT ( 'NONE',  ( 6.604150274805285825, -0.1349072972122930258, 1.703313905121685456 ) ) ;
#154351 = CARTESIAN_POINT ( 'NONE',  ( 6.269106929289325336, 1.662610211318481301, -0.5146825814001282362 ) ) ;
#154352 = CARTESIAN_POINT ( 'NONE',  ( 3.966586032518903959, -2.139059804502403850, -0.8247178969851276520 ) ) ;
#154353 = CARTESIAN_POINT ( 'NONE',  ( 3.327899939431624876, 1.796474422365784029, 0.4023406486387756664 ) ) ;
#154354 = CARTESIAN_POINT ( 'NONE',  ( 7.422199028477372451, 10.74665040227725044, -1.199719254218441611 ) ) ;
#154355 = CARTESIAN_POINT ( 'NONE',  ( 3.909063277197013520, 1.565549990038747952, 0.9388121169797561949 ) ) ;
#154356 = CARTESIAN_POINT ( 'NONE',  ( 5.379529795981254914, -0.4926393568372189335, -1.955173248319847845 ) ) ;
#154357 = CARTESIAN_POINT ( 'NONE',  ( -10.32861409551237486, 10.94447128771960287, 1.040834085586084257E-14 ) ) ;
#154359 = CARTESIAN_POINT ( 'NONE',  ( -8.120407659942227241, 8.438506789546210030, 0.7998128361456341429 ) ) ;
#154358 = CARTESIAN_POINT ( 'NONE',  ( 3.098750496328426252, -0.6552482397011113457, -2.165565034296774272 ) ) ;
#154360 = CARTESIAN_POINT ( 'NONE',  ( 4.911209521004105127, 1.831006069304096373, 1.040297942642433249 ) ) ;
#154361 = FACE_OUTER_BOUND ( 'NONE', #80226, .T. ) ;
#154362 = CARTESIAN_POINT ( 'NONE',  ( 3.842288295254093100, -1.023014542950370975, 1.799900136785845817 ) ) ;
#154363 = CARTESIAN_POINT ( 'NONE',  ( 2.191614386903386613, 5.708633884695917260, -0.7998128361456281477 ) ) ;
#154365 = EDGE_CURVE ( 'NONE', #175139, #31187, #142582, .T. ) ;
#154364 = CARTESIAN_POINT ( 'NONE',  ( -1.360316468749998675, 1.442708333674736831, 0.7853790794158961308 ) ) ;
#154366 = CARTESIAN_POINT ( 'NONE',  ( 5.408877457991549065, -0.5154355754800541423, -2.056752310636372982 ) ) ;
#154368 = STYLED_ITEM ( 'NONE', ( #192294 ), #15528 ) ;
#154367 = ITEM_DEFINED_TRANSFORMATION ( 'NONE', 'NONE', #159309,  #200407 ) ;
#154370 = CARTESIAN_POINT ( 'NONE',  ( 2.420428029321282093, 1.258221797421785082, -1.458952285233440449 ) ) ;
#154369 = CARTESIAN_POINT ( 'NONE',  ( -10.47775378526269918, 11.11846759242831872, -0.7998128361456221525 ) ) ;
#154371 = DIRECTION ( 'NONE',  ( -0.1827044046890596851, 0.9634447193773951756, -0.1959422700976716503 ) ) ;
#154372 = CARTESIAN_POINT ( 'NONE',  ( 6.719592862238788378, 0.3399973502477529608, -1.939713583613829728 ) ) ;
#154373 = CARTESIAN_POINT ( 'NONE',  ( 3.390947816749319443, 6.970206529600588397, -1.734723475976807094E-15 ) ) ;
#154374 = CARTESIAN_POINT ( 'NONE',  ( 5.543269800280802073, 6.196057874731542015, 0.9238780061134096444 ) ) ;
#154375 = LINE ( 'NONE', #185779, #114980 ) ;
#154376 = CARTESIAN_POINT ( 'NONE',  ( -3.079673448598517549, 6.744702790006905424, 1.040834085586084257E-14 ) ) ;
#154377 = CARTESIAN_POINT ( 'NONE',  ( 0.8091801829576624749, -0.5468400522714472745, -2.152931845550176249 ) ) ;
#154378 = CARTESIAN_POINT ( 'NONE',  ( 2.485502531088045419, 1.925919180164997746, -0.8524081271456557252 ) ) ;
#154379 = CARTESIAN_POINT ( 'NONE',  ( -6.064239847062411926, 10.29697326487330500, 0.000000000000000000 ) ) ;
#154380 = CARTESIAN_POINT ( 'NONE',  ( 6.265839547809997079, 10.46189657242035587, 0.7998128361456462443 ) ) ;
#154381 = CARTESIAN_POINT ( 'NONE',  ( 0.3263015691194782741, -1.220318288589719913, 1.405194318597773329 ) ) ;
#154382 = CARTESIAN_POINT ( 'NONE',  ( 4.937140493670735708, 8.911747675924535983, -0.7998128361456281477 ) ) ;
#154383 = CARTESIAN_POINT ( 'NONE',  ( 11.97929049433705728, 9.719999999999998863, 0.7046979865771804130 ) ) ;
#154384 = CARTESIAN_POINT ( 'NONE',  ( -5.804299160426229953, 8.825413882922319431, -1.082531754730549967 ) ) ;
#154385 = CARTESIAN_POINT ( 'NONE',  ( -7.375272376154077492, 11.54830883891436422, -0.7216878364870267237 ) ) ;
#154386 = CARTESIAN_POINT ( 'NONE',  ( 1.143014088299774578, 2.045220145331683614, 0.5602274146137007360 ) ) ;
#154387 = CARTESIAN_POINT ( 'NONE',  ( -5.887983850084758330, 10.09134126839936840, 0.7998128361456291469 ) ) ;
#154389 = CARTESIAN_POINT ( 'NONE',  ( 3.824618516750320385, -1.319357783791510697, 1.452116237791359010 ) ) ;
#154388 = CARTESIAN_POINT ( 'NONE',  ( 0.6124999999999776179, 0.8333333333333594606, 1.060881119635894487 ) ) ;
#154390 = CARTESIAN_POINT ( 'NONE',  ( 1.797963993548271411, -0.7283430984801853025, 2.035426966748521860 ) ) ;
#154391 = CARTESIAN_POINT ( 'NONE',  ( 2.032514702046281485, -1.644074058028240692, 0.8291662819630771786 ) ) ;
#154393 = CARTESIAN_POINT ( 'NONE',  ( -5.486276195386677657, 6.266678140956847720, -0.9979454321464575894 ) ) ;
#154392 = CARTESIAN_POINT ( 'NONE',  ( -5.418418667316934112, 6.350518529071726981, -1.199719254218453823 ) ) ;
#154394 = CARTESIAN_POINT ( 'NONE',  ( 3.925522983587381276, 0.9287783018587884021, -1.471562914255954757 ) ) ;
#154395 = CARTESIAN_POINT ( 'NONE',  ( 4.500943810056890371, 8.194925511800951412, -0.7216878364870207285 ) ) ;
#154396 = CARTESIAN_POINT ( 'NONE',  ( -11.31088518949709965, 5.182344123437907513, 5.726584094856639773 ) ) ;
#154397 = CARTESIAN_POINT ( 'NONE',  ( 1.165152350680317195, -1.954565670758709128, -0.9236901323337529668 ) ) ;
#154398 = AXIS2_PLACEMENT_3D ( 'NONE', #50051, #186428, #36983 ) ;
#154399 = CARTESIAN_POINT ( 'NONE',  ( 3.673203737196802710, -0.8145011343782401214, -1.844427810980188820 ) ) ;
#154400 = LINE ( 'NONE', #138161, #68768 ) ;
#154401 = CARTESIAN_POINT ( 'NONE',  ( 0.4796413896344040029, 2.016494124141111399, -0.7793912508547717888 ) ) ;
#154402 = CARTESIAN_POINT ( 'NONE',  ( 2.623849442957484346, -1.133682707547468471, -1.612724008377570017 ) ) ;
#154403 = STYLED_ITEM ( 'NONE', ( #199875 ), #196354 ) ;
#154404 = CARTESIAN_POINT ( 'NONE',  ( 6.609000000000012420, 2.052634316153336691, 2.306727925381938604 ) ) ;
#154405 = CARTESIAN_POINT ( 'NONE',  ( 2.173291266613562644, 1.196360937402714875, 1.529712666019187761 ) ) ;
#154407 = EDGE_LOOP ( 'NONE', ( #50278, #146418, #48920, #88438 ) ) ;
#154406 = CARTESIAN_POINT ( 'NONE',  ( -4.584065335196305213, 6.441438539186039591, 1.443375672974058777 ) ) ;
#154408 = CARTESIAN_POINT ( 'NONE',  ( -5.112833325684920993, 6.097965313788082931, -1.082531754730549967 ) ) ;
#154409 = CARTESIAN_POINT ( 'NONE',  ( -0.2106854629475426177, 0.2415373081153374957, -2.031805921504933554 ) ) ;
#154410 = CARTESIAN_POINT ( 'NONE',  ( 4.362691568547328202, 8.311833606605697256, -0.7998128361456381397 ) ) ;
#154411 = CARTESIAN_POINT ( 'NONE',  ( -5.875479466675803231, 7.948088359245467416, -1.599625672291271394 ) ) ;
#154412 = CARTESIAN_POINT ( 'NONE',  ( -6.149505192250180663, 9.332117270003974951, -1.199719254218452047 ) ) ;
#154413 = CARTESIAN_POINT ( 'NONE',  ( -9.693716643646601128, 12.33242205571964512, 1.443375672974076540 ) ) ;
#154414 = CARTESIAN_POINT ( 'NONE',  ( 6.422925328166578574, 2.149888460833260684, 0.8388895797235284002 ) ) ;
#154415 = CARTESIAN_POINT ( 'NONE',  ( 6.725062055625550705, -1.793239977796506457, -0.7961783947641184467 ) ) ;
#154416 = CARTESIAN_POINT ( 'NONE',  ( 4.293769791895286403, -1.349757117914761384, -1.423854091114319598 ) ) ;
#154417 =( BOUNDED_CURVE ( )  B_SPLINE_CURVE ( 2, ( #128273, #196378, #77285 ),
 .UNSPECIFIED., .F., .T. ) 
 B_SPLINE_CURVE_WITH_KNOTS ( ( 3, 3 ),
 ( 0.000000000000000000, 0.002450381106065508980 ),
 .UNSPECIFIED. ) 
 CURVE ( )  GEOMETRIC_REPRESENTATION_ITEM ( )  RATIONAL_B_SPLINE_CURVE ( ( 1.000000000000000000, 0.9212106833777519155, 0.9350920161047693302 ) ) 
 REPRESENTATION_ITEM ( '' )  );
#154418 = CARTESIAN_POINT ( 'NONE',  ( 8.782984583554449998, 9.141236857102018831, 1.040834085586084257E-14 ) ) ;
#154419 = CARTESIAN_POINT ( 'NONE',  ( 2.197888892816081796, 1.802417619043535701, 0.9041091288993635677 ) ) ;
#154420 = VERTEX_POINT ( 'NONE', #60223 ) ;
#154421 = CARTESIAN_POINT ( 'NONE',  ( 1.991562931776114542, -0.4585136385713373675, 2.066967827372573563 ) ) ;
#154422 = CARTESIAN_POINT ( 'NONE',  ( -1.500000000000013101, 1.202083334016148974, 0.8660254037844403729 ) ) ;
#154424 = CARTESIAN_POINT ( 'NONE',  ( -6.718228810771495141, 7.796687353110217877, 1.199719254218450271 ) ) ;
#154423 = DIRECTION ( 'NONE',  ( -1.000000000000000000, 5.578564026256504688E-16, 0.000000000000000000 ) ) ;
#154425 = CARTESIAN_POINT ( 'NONE',  ( 2.747807751077631977, 0.6205313035267927546, 1.733543155639664990 ) ) ;
#154426 = ORIENTED_EDGE ( 'NONE', *, *, #12829, .F. ) ;
#154427 =( REPRESENTATION_RELATIONSHIP ('NONE','NONE', #84563, #40301 ) REPRESENTATION_RELATIONSHIP_WITH_TRANSFORMATION ( #210575 )SHAPE_REPRESENTATION_RELATIONSHIP( ) );
#154428 = CARTESIAN_POINT ( 'NONE',  ( -9.378489572351046633, 11.96465713920816043, -1.599625672291263179 ) ) ;
#154429 = CARTESIAN_POINT ( 'NONE',  ( -1.387358672531466386, 7.251968950356099342, 4.302625267141412913 ) ) ;
#154430 = CARTESIAN_POINT ( 'NONE',  ( 4.500305224345508393, -0.9970752094022590217, 1.871535012320741265 ) ) ;
#154431 = CARTESIAN_POINT ( 'NONE',  ( -0.01213283819992416745, -0.3988646234997471618, -1.803908381610368261 ) ) ;
#154432 = PLANE ( 'NONE',  #18103 ) ;
#154433 = CARTESIAN_POINT ( 'NONE',  ( 6.479907352327590964, 9.647310113435821677, 1.199719254218462483 ) ) ;
#154434 = CARTESIAN_POINT ( 'NONE',  ( 4.024726114628586870, 1.955573890245201785, 0.6501785607586229032 ) ) ;
#154436 = CARTESIAN_POINT ( 'NONE',  ( 1.012948470060770934, -1.796336717620912626, 0.4034172393945419377 ) ) ;
#154435 = CARTESIAN_POINT ( 'NONE',  ( -6.256197817702116026, 9.386315656372753224, -1.199719254218440723 ) ) ;
#154437 = CARTESIAN_POINT ( 'NONE',  ( 1.364683531249990311, 5.363541667008086655, 0.7879004041258500513 ) ) ;
#154438 = CARTESIAN_POINT ( 'NONE',  ( -5.574622267388016361, 7.504663849841638701, -1.387123747601160639 ) ) ;
#154439 = CARTESIAN_POINT ( 'NONE',  ( 1.214306433183764966E-14, 2.428612866367529932E-14, 1.500000000000001332 ) ) ;
#154440 = CIRCLE ( 'NONE', #47162, 0.04999999999999929501 ) ;
#154441 = CARTESIAN_POINT ( 'NONE',  ( 1.436444770134176485, 1.085300811998829662, -1.921501399296850821 ) ) ;
#154442 = CARTESIAN_POINT ( 'NONE',  ( 4.112777665030871610, 1.603588310063062794, -1.596181346845012117 ) ) ;
#154443 = CARTESIAN_POINT ( 'NONE',  ( -6.073689629242151611, 10.02979563418376685, -0.7216878364870278340 ) ) ;
#154444 = CARTESIAN_POINT ( 'NONE',  ( 3.041053801226344611, 0.04897401433806568977, 1.811106077260196345 ) ) ;
#154445 = CARTESIAN_POINT ( 'NONE',  ( 4.206187189226945122, 1.174002167177927713, -1.513781418528682643 ) ) ;
#154446 = EDGE_CURVE ( 'NONE', #14213, #176917, #105821, .T. ) ;
#154447 = CARTESIAN_POINT ( 'NONE',  ( 5.072747062355987602, 1.430223858385268665, -1.497173470029027120 ) ) ;
#154448 = CARTESIAN_POINT ( 'NONE',  ( -0.6823417656250212460, 4.363541667008085767, 1.181850606188767472 ) ) ;
#154449 = CIRCLE ( 'NONE', #9255, 0.08000000000000020983 ) ;
#154450 = CARTESIAN_POINT ( 'NONE',  ( 3.924654207020538355, 1.871676352785199393, 0.6194476946735865130 ) ) ;
#154451 = CARTESIAN_POINT ( 'NONE',  ( 1.307504913943892122, -0.4706295199745584301, 1.867897339068110618 ) ) ;
#154452 = CARTESIAN_POINT ( 'NONE',  ( 4.188257260935820625, -1.850246793840780279, -0.2747695030091561463 ) ) ;
#154453 = ADVANCED_FACE ( 'NONE', ( #193430 ), #129232, .T. ) ;
#154454 = CARTESIAN_POINT ( 'NONE',  ( 3.440313875665978127, 1.038139129215289946, -2.061066213440334582 ) ) ;
#154455 = CARTESIAN_POINT ( 'NONE',  ( 3.279601929513912939, -1.794223665640673593, 0.4940275889762090200 ) ) ;
#154456 = CARTESIAN_POINT ( 'NONE',  ( -1.364683531250012516, 4.738541667008091096, -0.7879004041258300672 ) ) ;
#154457 = CARTESIAN_POINT ( 'NONE',  ( -0.3000000000000380695, 3.975028841772282107, 0.9637995837462106641 ) ) ;
#154458 = CARTESIAN_POINT ( 'NONE',  ( 1.893330831959182836, 1.831869315246800189, -1.038985425167998633 ) ) ;
#154459 = CARTESIAN_POINT ( 'NONE',  ( 3.673896439178923057, 5.309298483840612093, 1.443375672974066548 ) ) ;
#154461 = CARTESIAN_POINT ( 'NONE',  ( 5.071913926361915514, 4.910694714577345188, 0.2269669051133595961 ) ) ;
#154460 = PLANE ( 'NONE',  #198025 ) ;
#154462 = CARTESIAN_POINT ( 'NONE',  ( 1.286813488861806354, 4.047007041464545374, -0.4595522011843541366 ) ) ;
#154463 = CARTESIAN_POINT ( 'NONE',  ( 3.252298345715322281, 0.9499829135306799843, -1.895951488860507128 ) ) ;
#154464 = LINE ( 'NONE', #201039, #131036 ) ;
#154465 = CARTESIAN_POINT ( 'NONE',  ( 1.213155585027906325, 1.648708085711389160, -1.166442415167892932 ) ) ;
#154466 = CARTESIAN_POINT ( 'NONE',  ( -1.364683531250012516, 0.5302083336747518416, 0.7879004041258379498 ) ) ;
#154467 = AXIS2_PLACEMENT_3D ( 'NONE', #46207, #163148, #47280 ) ;
#154468 = CARTESIAN_POINT ( 'NONE',  ( -3.795919822146289313, 5.451659097302528068, -1.443375672974053447 ) ) ;
#154469 = CARTESIAN_POINT ( 'NONE',  ( 3.649115900372475796, 7.409052317076538330, 1.040834085586084257E-14 ) ) ;
#154470 = ORIENTED_EDGE ( 'NONE', *, *, #151886, .F. ) ;
#154471 = CARTESIAN_POINT ( 'NONE',  ( 1.212450271513715094, -0.9707322288472041150, -1.931405299116681018 ) ) ;
#154472 = CARTESIAN_POINT ( 'NONE',  ( 6.609999999999995879, 0.01081285896096205283, 1.720159828161060833 ) ) ;
#154475 = CARTESIAN_POINT ( 'NONE',  ( 2.399429999938675007, 5.743159399996332404, 0.000000000000000000 ) ) ;
#154474 = DIRECTION ( 'NONE',  ( -1.000000000000000000, 0.000000000000000000, 0.000000000000000000 ) ) ;
#154473 = CARTESIAN_POINT ( 'NONE',  ( 4.712340909201580885, 7.655425606447271214, -1.199719254218452047 ) ) ;
#154476 = CARTESIAN_POINT ( 'NONE',  ( 9.612367721964607981, 12.23751498042398289, -1.443375672974058777 ) ) ;
#154477 = CARTESIAN_POINT ( 'NONE',  ( 5.788296071918774821, -0.7303023681345042206, -1.879805717804765353 ) ) ;
#154478 = CARTESIAN_POINT ( 'NONE',  ( -7.375272376154081932, 10.58793962461302485, -1.082531754730543971 ) ) ;
#154479 = CARTESIAN_POINT ( 'NONE',  ( 6.409723817861421757, -0.9859548438324974295, -1.843685114342674458 ) ) ;
#154480 = DIRECTION ( 'NONE',  ( 0.1664974550714444224, 0.9062754367152173751, 0.3885143887443222588 ) ) ;
#154482 = CARTESIAN_POINT ( 'NONE',  ( 1.364683531250000748, 12.00520833367472839, -0.7879004041258355073 ) ) ;
#154481 = CARTESIAN_POINT ( 'NONE',  ( 6.754756207809571755, -1.674487575904315406, 1.366813541845832924 ) ) ;
#154483 = CARTESIAN_POINT ( 'NONE',  ( -8.971744963941075568, 11.49012176272984931, 1.599625672291269396 ) ) ;
#154485 = CARTESIAN_POINT ( 'NONE',  ( 0.7377199025260212650, 1.913388251642001103, -0.09504988074141537679 ) ) ;
#154484 = CARTESIAN_POINT ( 'NONE',  ( -5.219525951136850139, 7.112532914458205013, -1.443375672974051449 ) ) ;
#154486 = CARTESIAN_POINT ( 'NONE',  ( 1.364683531249986537, 1.467708333674748289, -0.7879004041258239610 ) ) ;
#154487 = DIRECTION ( 'NONE',  ( -1.000000000000000000, 0.000000000000000000, 5.421010862427519212E-16 ) ) ;
#154488 = CARTESIAN_POINT ( 'NONE',  ( -1.500000000000015099, 9.729166666666669627, -0.8660254037844309360 ) ) ;
#154489 = CARTESIAN_POINT ( 'NONE',  ( 3.369487540355073030, 1.682505700701863338, -0.3791672619692722512 ) ) ;
#154490 = CARTESIAN_POINT ( 'NONE',  ( 3.705121118284530279, 7.544668081299086282, -1.734723475976807094E-15 ) ) ;
#154491 = CARTESIAN_POINT ( 'NONE',  ( 1.879799676208588899, -0.9517657123069392933, 1.491821474084076726 ) ) ;
#154492 = CARTESIAN_POINT ( 'NONE',  ( 5.825267882404531861, -0.05969703229705652925, 2.206138628428089277 ) ) ;
#154493 = ORIENTED_EDGE ( 'NONE', *, *, #82737, .T. ) ;
#154494 = CARTESIAN_POINT ( 'NONE',  ( 4.113539317574116616, 1.624649823752024824, 1.199838557982295217 ) ) ;
#154495 = CARTESIAN_POINT ( 'NONE',  ( -5.738844160334429567, 9.917344963690652548, 0.000000000000000000 ) ) ;
#154497 = CARTESIAN_POINT ( 'NONE',  ( 3.866814677988283044, -0.2004539179165897023, -2.006445418776988010 ) ) ;
#154496 = CARTESIAN_POINT ( 'NONE',  ( 4.072980787186268437, -1.570383936966279981, 1.425070900414181052 ) ) ;
#154499 = ORIENTED_EDGE ( 'NONE', *, *, #196828, .F. ) ;
#154498 = CARTESIAN_POINT ( 'NONE',  ( 4.500164564109310206, -0.8477707339301239209, 1.600948808527142386 ) ) ;
#154500 = CARTESIAN_POINT ( 'NONE',  ( 3.888156192069020634, 7.758209000714329839, 1.040834085586084257E-14 ) ) ;
#154501 = ORIENTED_EDGE ( 'NONE', *, *, #77263, .T. ) ;
#154502 = CARTESIAN_POINT ( 'NONE',  ( 1.902992089709685031, 1.553661375375714471, 1.041555772207984676 ) ) ;
#154503 = CARTESIAN_POINT ( 'NONE',  ( -10.91893890296302772, -9.990657656777852225, 0.1342453211083811382 ) ) ;
#154504 = CARTESIAN_POINT ( 'NONE',  ( 5.848286676205444401, 0.8867688175292733899, -1.579494629471886791 ) ) ;
#154505 = CARTESIAN_POINT ( 'NONE',  ( -2.415323921528888196, 5.969628341758991930, 0.7998128361456341429 ) ) ;
#154506 = CARTESIAN_POINT ( 'NONE',  ( -10.49139461985735977, 3.038394114823554482, -7.128631142076787164 ) ) ;
#154507 = CARTESIAN_POINT ( 'NONE',  ( -1.201851678989727383E-14, 3.009375000341419248, -1.575800808251660134 ) ) ;
#154508 = DIRECTION ( 'NONE',  ( 5.551115123125765446E-17, 0.000000000000000000, -1.000000000000000000 ) ) ;
#154509 = CARTESIAN_POINT ( 'NONE',  ( 6.211043768836173484, 8.339580045099285854, 1.443375672974065660 ) ) ;
#154510 = CARTESIAN_POINT ( 'NONE',  ( -5.153507786970285665, 5.185049637652990207, -0.7216878364870338292 ) ) ;
#154511 = ADVANCED_FACE ( 'NONE', ( #178263 ), #128524, .F. ) ;
#154512 = CARTESIAN_POINT ( 'NONE',  ( -4.827585214917754719, 7.789877296449459365, -1.199719254218453823 ) ) ;
#154513 = CARTESIAN_POINT ( 'NONE',  ( 4.465154236216789307, -1.701427117168831549, 1.265499569954648962 ) ) ;
#154515 = CARTESIAN_POINT ( 'NONE',  ( -10.52284959769361805, 5.420271152154175986, 5.071911021504272199 ) ) ;
#154514 = CARTESIAN_POINT ( 'NONE',  ( -0.1296875068448125057, 7.629137130509072939, -2.426516348560475933 ) ) ;
#154516 = CARTESIAN_POINT ( 'NONE',  ( 5.466080325957246799, 0.9693943247218398396, 1.716448534147915650 ) ) ;
#154517 = CARTESIAN_POINT ( 'NONE',  ( -1.364683531250000748, 0.7593750003414210248, 0.000000000000000000 ) ) ;
#154518 = CARTESIAN_POINT ( 'NONE',  ( 1.107682593029035711, 1.527310012579755183, 1.311747809748030846 ) ) ;
#154519 = ORIENTED_EDGE ( 'NONE', *, *, #80217, .T. ) ;
#154520 = AXIS2_PLACEMENT_3D ( 'NONE', #173453, #203767, #54354 ) ;
#154521 = CARTESIAN_POINT ( 'NONE',  ( 0.4920138693931704887, -2.106576347024671225, 0.2123275358263312096 ) ) ;
#154522 = DIRECTION ( 'NONE',  ( 0.000000000000000000, 1.000000000000000000, 0.000000000000000000 ) ) ;
#154523 = CARTESIAN_POINT ( 'NONE',  ( 1.398975865466948632, 0.4019745351953528112, 2.030794141931663521 ) ) ;
#154524 = CARTESIAN_POINT ( 'NONE',  ( 5.825163275726873202, 6.825053905550038991, 1.199719254218452047 ) ) ;
#154525 = CARTESIAN_POINT ( 'NONE',  ( 5.468734858265785093, 7.473552982767158070, 1.599625672291269396 ) ) ;
#154526 = ORIENTED_EDGE ( 'NONE', *, *, #79201, .F. ) ;
#154528 = CARTESIAN_POINT ( 'NONE',  ( 5.464099601507359516, 6.333536608968757697, 1.199719254218462483 ) ) ;
#154527 = CARTESIAN_POINT ( 'NONE',  ( 4.453126923439646667, 0.4583234712903122565, -2.039610397757870341 ) ) ;
#154531 = ORIENTED_EDGE ( 'NONE', *, *, #14021, .T. ) ;
#154530 = CARTESIAN_POINT ( 'NONE',  ( 1.295247000857565167, 1.673883212702592660, -0.6929762496888560719 ) ) ;
#154529 = CARTESIAN_POINT ( 'NONE',  ( 3.364083894888194592, 0.8197913233371353359, 1.631220078658943695 ) ) ;
#154532 = CARTESIAN_POINT ( 'NONE',  ( 6.252570086353132162, 0.6882034672392455255, 2.096894461246688213 ) ) ;
#154533 = CARTESIAN_POINT ( 'NONE',  ( 4.348781676370103710, 0.5853419563807431558, 2.127667884090424621 ) ) ;
#154534 = CARTESIAN_POINT ( 'NONE',  ( 7.527801604085637699, 9.805521176231838609, 1.599625672291281386 ) ) ;
#154535 = CARTESIAN_POINT ( 'NONE',  ( -8.012344526598182026E-15, 9.859375000341399797, -1.575800808251669460 ) ) ;
#154536 = EDGE_CURVE ( 'NONE', #138322, #147946, #89349, .T. ) ;
#154537 = CARTESIAN_POINT ( 'NONE',  ( 2.438023429326571456, -1.102505324871098757, -1.562262158393577405 ) ) ;
#154538 = CARTESIAN_POINT ( 'NONE',  ( 8.341290820905593151, 10.75459192918846618, 1.599625672291281386 ) ) ;
#154539 = CARTESIAN_POINT ( 'NONE',  ( 6.760220206081136496, -2.069995208266177666, 0.04663682477341198757 ) ) ;
#154540 = CARTESIAN_POINT ( 'NONE',  ( -7.511572993685796537E-15, 0.3593750003414037386, -1.570758158831792262 ) ) ;
#154541 = CARTESIAN_POINT ( 'NONE',  ( 5.460537066722415567, -1.980877156148381335, -0.9378266216248376530 ) ) ;
#154542 = DIRECTION ( 'NONE',  ( 0.000000000000000000, 0.000000000000000000, 1.000000000000000000 ) ) ;
#154543 = CARTESIAN_POINT ( 'NONE',  ( -3.090297434914522690, 15.44821197608033536, -11.55767568840040127 ) ) ;
#154544 = VERTEX_POINT ( 'NONE', #79677 ) ;
#154545 = ORIENTED_EDGE ( 'NONE', *, *, #111152, .F. ) ;
#154546 = CARTESIAN_POINT ( 'NONE',  ( 0.3999999999999758193, 3.000000000000047518, 2.023857702507768419 ) ) ;
#154547 = CARTESIAN_POINT ( 'NONE',  ( 3.725732288501612199, -1.111853074318921664, -1.504101509696729400 ) ) ;
#154548 = CARTESIAN_POINT ( 'NONE',  ( -1.642778471875000035, -1.655208332855377051, -2.845375778867859751 ) ) ;
#154549 = CIRCLE ( 'NONE', #119977, 0.09999999999999982514 ) ;
#154550 = LINE ( 'NONE', #87416, #119720 ) ;
#154551 = CARTESIAN_POINT ( 'NONE',  ( -8.242994207428740339, 9.679543332497402730, 1.082531754730558626 ) ) ;
#154553 = CARTESIAN_POINT ( 'NONE',  ( 5.435893244436359240, 5.306573304789342416, -0.7998128361456481317 ) ) ;
#154552 = AXIS2_PLACEMENT_3D ( 'NONE', #160166, #159097, #59461 ) ;
#154554 = CARTESIAN_POINT ( 'NONE',  ( 0.6023233765659050665, 1.963792105354182249, 0.1503755929508752975 ) ) ;
#154555 = CARTESIAN_POINT ( 'NONE',  ( 1.687125285987755019, 1.678019391100945779, 1.117813378161469418 ) ) ;
#154556 = CARTESIAN_POINT ( 'NONE',  ( -10.48453286206953727, 11.12637651536962125, 0.7998128361456462443 ) ) ;
#154557 = CARTESIAN_POINT ( 'NONE',  ( 4.004454267989866700, 5.765225627445230927, 1.599625672291262513 ) ) ;
#154559 = EDGE_CURVE ( 'NONE', #199252, #69312, #151896, .T. ) ;
#154558 =( LENGTH_UNIT ( ) NAMED_UNIT ( * ) SI_UNIT ( .MILLI., .METRE. ) );
#154560 = CARTESIAN_POINT ( 'NONE',  ( 1.131117939106265569, -1.979831898266545487, 0.9398196729281658168 ) ) ;
#154561 = CARTESIAN_POINT ( 'NONE',  ( 4.635264976507449397, -1.668059998867366778, 0.7425182445051290436 ) ) ;
#154562 = CARTESIAN_POINT ( 'NONE',  ( -3.086452525405351643, 6.752611712948207057, 0.7998128361456341429 ) ) ;
#154563 = ADVANCED_FACE ( 'NONE', ( #115440 ), #144726, .F. ) ;
#154564 = CARTESIAN_POINT ( 'NONE',  ( 4.394251184604957672, 8.140727125432173139, -0.7216878364870357165 ) ) ;
#154565 = CARTESIAN_POINT ( 'NONE',  ( 9.642873567817520808, 12.27310513391906532, 1.599625672291279388 ) ) ;
#154566 = CARTESIAN_POINT ( 'NONE',  ( -4.685224601974262271, 7.623789914682047808, -1.199719254218453823 ) ) ;
#154567 = CARTESIAN_POINT ( 'NONE',  ( 4.539282502477016479, 4.190251095844947926, 0.7998128361456341429 ) ) ;
#154568 = CARTESIAN_POINT ( 'NONE',  ( 4.740510986633625024, 5.559626234941203116, -1.199719254218450271 ) ) ;
#154569 = ORIENTED_EDGE ( 'NONE', *, *, #64259, .T. ) ;
#154571 = CARTESIAN_POINT ( 'NONE',  ( 0.01235793338260140865, -2.012684344489227062, -0.04732037452980299846 ) ) ;
#154570 = CARTESIAN_POINT ( 'NONE',  ( 2.419273308677453826, -1.061688697878185206, -1.504126257600538974 ) ) ;
#154572 = CARTESIAN_POINT ( 'NONE',  ( 1.494008433901512278, 2.215370577347621328, 0.6118545706256629524 ) ) ;
#154574 = CARTESIAN_POINT ( 'NONE',  ( 6.737165023268617325, -0.09304339776683606678, -1.959646862056351857 ) ) ;
#154573 = CARTESIAN_POINT ( 'NONE',  ( 3.470524135418292300, 5.072030796119872953, -1.443375672974057666 ) ) ;
#154575 = CARTESIAN_POINT ( 'NONE',  ( -5.603597561149804562, 5.431951997629870910, 0.7998128361456341429 ) ) ;
#154576 = CARTESIAN_POINT ( 'NONE',  ( 10.08385610902499963, -7.605490242282785474, -0.4645879755154048718 ) ) ;
#154577 = CARTESIAN_POINT ( 'NONE',  ( 3.761887187967042134, 0.6396200178584460216, -1.802413552503052463 ) ) ;
#154578 = CARTESIAN_POINT ( 'NONE',  ( -10.63367255181986160, 11.30037282007833532, 1.040834085586084257E-14 ) ) ;
#154579 = CARTESIAN_POINT ( 'NONE',  ( 6.385878362533466301, 6.816559200039058020, 0.5486352003098924346 ) ) ;
#154580 = CARTESIAN_POINT ( 'NONE',  ( -7.431277594066152403, 8.802816960232885179, -1.082531754730549967 ) ) ;
#154582 = CARTESIAN_POINT ( 'NONE',  ( 1.076777757339364205, -0.04213119042271313425, -1.870346338061685154 ) ) ;
#154581 = CARTESIAN_POINT ( 'NONE',  ( 3.069954157378000925, -1.243473088950231675, 1.680628819622100423 ) ) ;
#154583 = CARTESIAN_POINT ( 'NONE',  ( 1.722029606037442040, -1.727736752315935265, -1.038835718801443653 ) ) ;
#154584 = CARTESIAN_POINT ( 'NONE',  ( 9.408995418203975447, 10.07950886410055524, 0.7216878364870438212 ) ) ;
#154585 = CARTESIAN_POINT ( 'NONE',  ( 0.6823417656249899377, 4.488541667008086655, -1.181850606188754593 ) ) ;
#154586 = CARTESIAN_POINT ( 'NONE',  ( 3.473892794100913672, -1.678317346756386108, -0.4606119698754263525 ) ) ;
#154587 = CARTESIAN_POINT ( 'NONE',  ( 3.714044015139744914, 6.420469553383295391, 1.199719254218462483 ) ) ;
#154588 = DIRECTION ( 'NONE',  ( 0.000000000000000000, 0.000000000000000000, 1.000000000000000000 ) ) ;
#154589 = CARTESIAN_POINT ( 'NONE',  ( 3.896855043588220546, 1.455827857355775246, -0.9247512240674607975 ) ) ;
#154590 = CARTESIAN_POINT ( 'NONE',  ( 2.279091853667324141, 2.002311374866962979, -0.8913168663882904408 ) ) ;
#154591 = CARTESIAN_POINT ( 'NONE',  ( 5.567066847960510323, -1.993696164035433371, -0.9465883713010987410 ) ) ;
#154592 = CARTESIAN_POINT ( 'NONE',  ( -10.55260481140867235, 5.124873218919925755, -7.009574331923702495 ) ) ;
#154593 = MECHANICAL_DESIGN_GEOMETRIC_PRESENTATION_REPRESENTATION (  '', ( #16170 ), #106245 ) ;
#154594 = CARTESIAN_POINT ( 'NONE',  ( 4.100555696908855019, 2.160072011501934064, 0.2185761814032516903 ) ) ;
#154595 = CARTESIAN_POINT ( 'NONE',  ( 2.683998146737070378, -0.9385614705539682134, 1.565816405032012470 ) ) ;
#154596 = CARTESIAN_POINT ( 'NONE',  ( -2.788906526875773208E-15, 12.43750000000000000, -1.499999999999998446 ) ) ;
#154597 = CARTESIAN_POINT ( 'NONE',  ( 4.417270958439249107, -1.934380516720465959, 0.8614220525851381538 ) ) ;
#154598 = CARTESIAN_POINT ( 'NONE',  ( 6.539320575229250920, 3.702490941164796379, 2.411252750440337156 ) ) ;
#154599 = ORIENTED_EDGE ( 'NONE', *, *, #128228, .F. ) ;
#154601 = CARTESIAN_POINT ( 'NONE',  ( -1.201851678989727383E-14, 2.759375000341417916, -1.575800808251660134 ) ) ;
#154600 = CARTESIAN_POINT ( 'NONE',  ( 4.564210359040954401, -1.498010274845029244, 1.735314277699088858 ) ) ;
#154602 = CARTESIAN_POINT ( 'NONE',  ( 6.827182134110222123, -0.006956174471953178659, 2.188967759425272330 ) ) ;
#154603 = CARTESIAN_POINT ( 'NONE',  ( 9.459838494033030898, 12.05956421450382088, 1.599625672291281386 ) ) ;
#154604 = CARTESIAN_POINT ( 'NONE',  ( 0.1356056236470788157, -0.09959319089659908475, 2.118264760961988458 ) ) ;
#154605 = CARTESIAN_POINT ( 'NONE',  ( -4.772106882330223954, 8.511282429453158827, -0.7216878364870267237 ) ) ;
#154606 = CARTESIAN_POINT ( 'NONE',  ( 3.931501358282940117, 4.649468341827285300, -1.082531754730543083 ) ) ;
#154607 = CARTESIAN_POINT ( 'NONE',  ( -6.222829318548141586, 6.362315081168691044, 0.7216878364870317197 ) ) ;
#154608 = DIRECTION ( 'NONE',  ( -0.01641209967245726292, 0.005323139086630728802, -0.9998511425080263137 ) ) ;
#154609 = ORIENTED_EDGE ( 'NONE', *, *, #166617, .T. ) ;
#154610 = CARTESIAN_POINT ( 'NONE',  ( 5.326796142270829648, 0.8146286751641409474, -1.844708973168760924 ) ) ;
#154612 = CARTESIAN_POINT ( 'NONE',  ( 3.766515156912704665, -0.8315086482118605460, -1.887695802070661344 ) ) ;
#154611 = CARTESIAN_POINT ( 'NONE',  ( 6.484877546038077867, 6.460111979999551224, 1.040834085586084257E-14 ) ) ;
#154614 = CARTESIAN_POINT ( 'NONE',  ( -0.1411974294642046046, 7.629137130509075604, -2.500278959528269063 ) ) ;
#154613 = CARTESIAN_POINT ( 'NONE',  ( 5.657495238652423097, 9.822437888394988548, 0.000000000000000000 ) ) ;
#154615 = CARTESIAN_POINT ( 'NONE',  ( 6.200875153403774043, 8.327716660428123419, -1.599625672291283607 ) ) ;
#154616 = CARTESIAN_POINT ( 'NONE',  ( 3.285556943750000514, -1.363541666188709423, 1.896917185911906500 ) ) ;
#154617 = CARTESIAN_POINT ( 'NONE',  ( 0.000000000000000000, 13.49999999999999822, -1.500000000000000222 ) ) ;
#154618 = CARTESIAN_POINT ( 'NONE',  ( 6.035146784841348477, -1.584849238314169240, -1.513754250258770639 ) ) ;
#154619 = CARTESIAN_POINT ( 'NONE',  ( 3.252577435111691617, 1.966644794889659043, -0.4445022851852917234 ) ) ;
#154620 = CARTESIAN_POINT ( 'NONE',  ( 3.421284184235491743, -1.099380227797893905, -1.476844927387373163 ) ) ;
#154621 = CARTESIAN_POINT ( 'NONE',  ( 4.808338034340912337, 8.761478140039733020, 1.040834085586084257E-14 ) ) ;
#154622 = CARTESIAN_POINT ( 'NONE',  ( 0.1645217639845691082, -1.537023147574669402, -0.7826882907640534404 ) ) ;
#154623 = DIRECTION ( 'NONE',  ( 1.000000000000000000, 0.000000000000000000, 0.000000000000000000 ) ) ;
#154624 = CARTESIAN_POINT ( 'NONE',  ( 0.5812297525147345212, -0.8198687466959112546, 2.147686052911641497 ) ) ;
#154625 = CARTESIAN_POINT ( 'NONE',  ( -7.400052914960538963, 7.527816577075747695, 1.040834085586084257E-14 ) ) ;
#154626 = CARTESIAN_POINT ( 'NONE',  ( 0.6325467830279264403, 1.161941506187497364, -1.941124190868536603 ) ) ;
#154627 = CARTESIAN_POINT ( 'NONE',  ( 2.824945763694948653, 1.983238121251710950, 0.7091105908984902673 ) ) ;
#154628 = CARTESIAN_POINT ( 'NONE',  ( -3.474632506852224356, 7.275764701294714420, -0.7998128361456481317 ) ) ;
#154629 = CARTESIAN_POINT ( 'NONE',  ( 8.111855979677986994, 8.358253485912799263, 1.040834085586084257E-14 ) ) ;
#154630 = CARTESIAN_POINT ( 'NONE',  ( 6.672020991256494504, 6.956648375986938859, 0.000000000000000000 ) ) ;
#154631 = CARTESIAN_POINT ( 'NONE',  ( -6.738566041191992539, 7.820414121934134322, 1.199719254218450271 ) ) ;
#154632 = CARTESIAN_POINT ( 'NONE',  ( 6.277061933002774374, 9.306694107603160404, 1.082531754730558626 ) ) ;
#154633 = CARTESIAN_POINT ( 'NONE',  ( 4.291011075107065587, 7.468133931351726318, 1.062205608224401576 ) ) ;
#154634 = CARTESIAN_POINT ( 'NONE',  ( -5.274285450916075035, 6.112086766612214284, 1.199719254218450271 ) ) ;
#154636 = CARTESIAN_POINT ( 'NONE',  ( 4.236746486948286261, 1.365021424349493584, -1.752494286840690085 ) ) ;
#154635 = CARTESIAN_POINT ( 'NONE',  ( 2.197662576721173266, 1.936918166296027977, -0.8637449004969055544 ) ) ;
#154637 = CARTESIAN_POINT ( 'NONE',  ( 2.185716925580234449, -0.9354795820612994417, 1.981881815340847730 ) ) ;
#154638 = CARTESIAN_POINT ( 'NONE',  ( -7.088215381846223906, 7.164006121775713609, 0.7998128361456341429 ) ) ;
#154639 = CARTESIAN_POINT ( 'NONE',  ( -5.581116510680924847, 6.540332679663050541, -1.199719254218453823 ) ) ;
#154640 = CARTESIAN_POINT ( 'NONE',  ( 5.951606347324345236, 1.484592722905058393, 1.282605414028796353 ) ) ;
#154641 = CARTESIAN_POINT ( 'NONE',  ( -1.402160292154681736E-14, 1.446875000341420137, -1.575800808251659024 ) ) ;
#154642 = CARTESIAN_POINT ( 'NONE',  ( -4.394251184604987870, 5.259619482528146150, 1.082531754730549078 ) ) ;
#154643 = CARTESIAN_POINT ( 'NONE',  ( -6.900736999675794792, 7.153207375817628666, 1.040834085586084257E-14 ) ) ;
#154644 = CARTESIAN_POINT ( 'NONE',  ( 4.306960158517386894, -0.4675538901007176285, -2.068242682749166672 ) ) ;
#154645 = CARTESIAN_POINT ( 'NONE',  ( -5.307090785106547415, 5.156303768904543894, -0.7998128361456362523 ) ) ;
#154646 = ORIENTED_EDGE ( 'NONE', *, *, #88694, .F. ) ;
#154647 = CARTESIAN_POINT ( 'NONE',  ( 5.137646372127643524, -1.526005641499485810, -1.531359247741073570 ) ) ;
#154648 = CARTESIAN_POINT ( 'NONE',  ( 5.738125327081736060, 7.717565519727259904, 1.599625672291267398 ) ) ;
#154649 = CARTESIAN_POINT ( 'NONE',  ( 4.686955257832659427, 1.367739038236553295, 1.232883728221022990 ) ) ;
#154650 = CARTESIAN_POINT ( 'NONE',  ( -5.906232603126833958, 6.003624899985508634, 0.1331734367991978252 ) ) ;
#154651 = CARTESIAN_POINT ( 'NONE',  ( 1.364683531249986537, 0.9260416670080896528, 0.7879004041258500513 ) ) ;
#154652 = CARTESIAN_POINT ( 'NONE',  ( 0.4677839449492172674, -1.637930601595443125, -0.5889144675248291216 ) ) ;
#154653 = CARTESIAN_POINT ( 'NONE',  ( 6.727182134110201162, 0.003007720480356981373, 1.910970182385363092 ) ) ;
#154654 = CARTESIAN_POINT ( 'NONE',  ( 4.053524740805938720, 3.831459740469437936, 1.214306433183764966E-14 ) ) ;
#154655 = CARTESIAN_POINT ( 'NONE',  ( -2.905110965495596944E-15, 1.687500000000013101, -1.225000000000019851 ) ) ;
#154656 = CARTESIAN_POINT ( 'NONE',  ( 4.241217004700631676, -1.882188537963986219, 1.063020064016991117 ) ) ;
#154657 = CARTESIAN_POINT ( 'NONE',  ( -5.271422797614987665, 5.044414773505913274, -0.7998128361456221525 ) ) ;
#154658 = CARTESIAN_POINT ( 'NONE',  ( -7.497295758232724872, 9.769931022736756177, -1.443375672974058777 ) ) ;
#154659 = CARTESIAN_POINT ( 'NONE',  ( 3.924826023212550030, 2.051882857192890430, 0.6804245187241527715 ) ) ;
#154660 = CARTESIAN_POINT ( 'NONE',  ( 4.428955518335824237, 0.09376622492938446740, 1.969227427985324352 ) ) ;
#154661 = CARTESIAN_POINT ( 'NONE',  ( 3.514723022282209897, 1.734034291474368494, 0.002059465714070173124 ) ) ;
#154662 = CARTESIAN_POINT ( 'NONE',  ( 0.4510473619779230003, -1.854578567552306767, -1.167393260480112493 ) ) ;
#154663 = CARTESIAN_POINT ( 'NONE',  ( 1.009288123910282442, 1.745381235414251275, -1.509623180311530977 ) ) ;
#154664 = CARTESIAN_POINT ( 'NONE',  ( 3.497389175668437211, 1.622225323665491326, 1.270757995044344391 ) ) ;
#154665 = CARTESIAN_POINT ( 'NONE',  ( 5.970255158568685161, -1.845527328187264615, -0.6049325008806984982 ) ) ;
#154666 = CARTESIAN_POINT ( 'NONE',  ( -7.904040366642703930, 10.24446639921506552, 1.443375672974090751 ) ) ;
#154667 = CARTESIAN_POINT ( 'NONE',  ( -4.118644803501354978, 8.027112380718707030, 0.7998128361456352531 ) ) ;
#154668 = CARTESIAN_POINT ( 'NONE',  ( -11.78331023100045627, 12.30000000000000071, -1.800000000000001155 ) ) ;
#154670 = ORIENTED_EDGE ( 'NONE', *, *, #193087, .T. ) ;
#154669 = CARTESIAN_POINT ( 'NONE',  ( -1.814759087649988833, 3.975067388631688292, -0.4606438099578630818 ) ) ;
#154671 = CARTESIAN_POINT ( 'NONE',  ( -6.656690234185426824, 10.70996300661758660, 0.7216878364870458196 ) ) ;
#154672 = CARTESIAN_POINT ( 'NONE',  ( 3.311752114541001379, -0.4323003076652854881, 2.163846791405985570 ) ) ;
#154673 = CARTESIAN_POINT ( 'NONE',  ( -1.642778471875000035, -3.055208332855375630, -2.845375778867859751 ) ) ;
#154674 = VERTEX_POINT ( 'NONE', #29876 ) ;
#154675 = CARTESIAN_POINT ( 'NONE',  ( 0.4790722831046652641, -0.09921120595577682943, 1.858460205838560864 ) ) ;
#154676 = CARTESIAN_POINT ( 'NONE',  ( -0.02900071798685524560, 2.860900941590225344, -2.661937258840251008 ) ) ;
#154677 = CARTESIAN_POINT ( 'NONE',  ( -0.7500000000000215383, 5.472916667349482900, 1.299038105676671107 ) ) ;
#154678 = FILL_AREA_STYLE ('',( #24656 ) ) ;
#154681 = CIRCLE ( 'NONE', #109761, 1.500000000000005107 ) ;
#154680 = CARTESIAN_POINT ( 'NONE',  ( 6.825078400183577365, 2.023440267519378999, 2.448151054272352578 ) ) ;
#154679 = CARTESIAN_POINT ( 'NONE',  ( -6.117836340636773507, 7.096790560477957754, -1.125390141808879196 ) ) ;
#154682 = CARTESIAN_POINT ( 'NONE',  ( 6.474545096729184657, -0.09562278402284157819, -1.838781726270556582 ) ) ;
#154683 = ORIENTED_EDGE ( 'NONE', *, *, #82531, .F. ) ;
#154684 = CARTESIAN_POINT ( 'NONE',  ( 2.008734545381769543, 1.527802914727709016, -1.383344190003793495 ) ) ;
#154685 = CARTESIAN_POINT ( 'NONE',  ( -1.360316468750042862, -0.08854166632527044056, 0.7853790794158801436 ) ) ;
#154686 = CARTESIAN_POINT ( 'NONE',  ( -5.208303565944065738, 9.228104593576741621, -0.7998128361456231517 ) ) ;
#154687 = FACE_OUTER_BOUND ( 'NONE', #73490, .T. ) ;
#154688 = DIRECTION ( 'NONE',  ( 0.000000000000000000, 0.000000000000000000, -1.000000000000000000 ) ) ;
#154689 = CARTESIAN_POINT ( 'NONE',  ( 4.857899112398166075, 4.561970474086296079, 1.040834085586084257E-14 ) ) ;
#154690 = EDGE_CURVE ( 'NONE', #183276, #195372, #177591, .T. ) ;
#154691 = CARTESIAN_POINT ( 'NONE',  ( 0.7079729303958534059, -2.051031625230379074, 0.2011725655505970656 ) ) ;
#154693 = CARTESIAN_POINT ( 'NONE',  ( 4.722110844128335039, 1.763445737372179689, 0.5296355584529164329 ) ) ;
#154692 = CARTESIAN_POINT ( 'NONE',  ( 6.620655732516651071, -0.002413161512292844035, 2.173887093218453082 ) ) ;
#154694 = CARTESIAN_POINT ( 'NONE',  ( 5.900823170445728572, 7.907379670318584353, 1.599625672291267398 ) ) ;
#154695 = CARTESIAN_POINT ( 'NONE',  ( -5.631432701629818460, 7.663367133358481631, 1.599625672291263179 ) ) ;
#154696 = CARTESIAN_POINT ( 'NONE',  ( 2.609770642201841184, -0.3830433331901555993, 0.000000000000000000 ) ) ;
#154697 = CARTESIAN_POINT ( 'NONE',  ( 5.444034239667132624, 0.8972360612293399651, -2.016436982482258333 ) ) ;
#154698 = CARTESIAN_POINT ( 'NONE',  ( 0.5972264258897291844, 1.797487153981947916, -1.200333582630601637 ) ) ;
#154699 = CARTESIAN_POINT ( 'NONE',  ( -5.910991785878183080, 5.998504626387068051, -0.7216878364870278340 ) ) ;
#154700 = CARTESIAN_POINT ( 'NONE',  ( 0.5977379272000953314, 1.286164058678052946, 1.415416067018962165 ) ) ;
#154701 = CARTESIAN_POINT ( 'NONE',  ( 1.323454262349360144, -1.463929862531298198, -1.387097294446784090 ) ) ;
#154702 = ADVANCED_FACE ( 'NONE', ( #65531 ), #173435, .T. ) ;
#154703 = CARTESIAN_POINT ( 'NONE',  ( 6.441532379824158383, 9.568852638886589546, -1.082531754730548412 ) ) ;
#154704 = CARTESIAN_POINT ( 'NONE',  ( 1.458857794315861156, 1.741214688395021470, 1.500301734068248294 ) ) ;
#154705 = CARTESIAN_POINT ( 'NONE',  ( 6.928203230275524760, 15.51845925587262798, -9.797958971132702644 ) ) ;
#154706 = EDGE_CURVE ( 'NONE', #84297, #96508, #206993, .T. ) ;
#154707 = CARTESIAN_POINT ( 'NONE',  ( -11.92619526913699879, 13.40000000000000036, -1.328859060402686199 ) ) ;
#154708 = CARTESIAN_POINT ( 'NONE',  ( 1.410794581852807150, 1.648159533202856686, 0.8848386531258023435 ) ) ;
#154709 = CIRCLE ( 'NONE', #61316, 0.2000000000000005107 ) ;
#154710 = CARTESIAN_POINT ( 'NONE',  ( 2.782435679340321766, -0.5899881929209308540, -1.928257399728677601 ) ) ;
#154712 = CARTESIAN_POINT ( 'NONE',  ( -3.231779075379149546, 6.036511184309971689, -2.419999999999998597 ) ) ;
#154711 = CARTESIAN_POINT ( 'NONE',  ( -1.364683531250014514, 0.4885416670080875434, -0.7879004041258289570 ) ) ;
#154714 = CARTESIAN_POINT ( 'NONE',  ( 5.057299757384343231, -1.778698004947255162, -1.127411927216742216 ) ) ;
#154713 = CARTESIAN_POINT ( 'NONE',  ( -8.864333505236459132, 9.236143932397675727, 1.040834085586084257E-14 ) ) ;
#154715 = CARTESIAN_POINT ( 'NONE',  ( 7.259501185113382604, 10.55683625168592243, -1.199719254218441611 ) ) ;
#154717 = CARTESIAN_POINT ( 'NONE',  ( -8.259941899223614215, 10.65968485389279508, -1.599625672291263179 ) ) ;
#154716 = CARTESIAN_POINT ( 'NONE',  ( 4.278479993564246797, 7.149254538203735798, 1.199719254218452047 ) ) ;
#154718 = FACE_OUTER_BOUND ( 'NONE', #199654, .T. ) ;
#154719 = CARTESIAN_POINT ( 'NONE',  ( 4.113539317574116616, 1.624649823752024824, 1.199838557982295217 ) ) ;
#154720 = CARTESIAN_POINT ( 'NONE',  ( -0.6823417656250212460, 4.301041667008085767, 1.181850606188767472 ) ) ;
#154721 = CARTESIAN_POINT ( 'NONE',  ( 6.883263157960402445, -0.003972766660574957552, 2.046037087719229319 ) ) ;
#154722 = CARTESIAN_POINT ( 'NONE',  ( 7.944714827928033962, 12.21265836598400689, 0.7216878364870438212 ) ) ;
#154723 = CARTESIAN_POINT ( 'NONE',  ( 4.991577004318280331, 1.598001195387260154, 1.455802845438579407 ) ) ;
#154724 = CARTESIAN_POINT ( 'NONE',  ( 6.200875153403774043, 8.327716660428123419, -1.599625672291283607 ) ) ;
#154725 = CARTESIAN_POINT ( 'NONE',  ( -1.364683531250000748, -1.178124999658580752, 0.000000000000000000 ) ) ;
#154727 = CARTESIAN_POINT ( 'NONE',  ( -7.821934338880100590, -6.709380320845385270, 7.553974597844393735 ) ) ;
#154726 = CARTESIAN_POINT ( 'NONE',  ( 5.017399365509065845, 8.011327138806002779, -1.199719254218450271 ) ) ;
#154728 = CARTESIAN_POINT ( 'NONE',  ( 6.738039155867407537, 10.80487008191325771, -0.7216878364870267237 ) ) ;
#154730 = DIRECTION ( 'NONE',  ( -0.5773502691896238437, 0.000000000000000000, -0.8164965809277274778 ) ) ;
#154729 = CARTESIAN_POINT ( 'NONE',  ( 2.242849641980674491, -2.128998374728574117, -0.4250897845002408193 ) ) ;
#154732 = CARTESIAN_POINT ( 'NONE',  ( 1.487592393518050837, -1.832424703912252317, -0.1798031890194173865 ) ) ;
#154731 = CARTESIAN_POINT ( 'NONE',  ( -4.907688418466881863, 8.669460888279271416, 0.7216878364870458196 ) ) ;
#154733 = CARTESIAN_POINT ( 'NONE',  ( -1.201851678989727383E-14, 2.946875000341419248, -1.575800808251660134 ) ) ;
#154734 = CARTESIAN_POINT ( 'NONE',  ( 2.788834510562918645, 1.878274557074947948, -1.128960604485473862 ) ) ;
#154735 = DIRECTION ( 'NONE',  ( 1.000000000000000000, -0.000000000000000000, -0.000000000000000000 ) ) ;
#154736 = CARTESIAN_POINT ( 'NONE',  ( 3.327297708271567345, 0.05365531978675056046, 2.262033696468904065 ) ) ;
#154737 = CARTESIAN_POINT ( 'NONE',  ( -5.045605722580076780, 9.038290442985410067, -0.7998128361456231517 ) ) ;
#154738 = CARTESIAN_POINT ( 'NONE',  ( 1.364683531249992088, 5.446875000341417916, 1.214306433183764966E-14 ) ) ;
#154739 = CARTESIAN_POINT ( 'NONE',  ( 6.450676980830294838, 6.774405823990504949, -0.3487213023658369826 ) ) ;
#154740 = CARTESIAN_POINT ( 'NONE',  ( 0.7500000000000006661, 13.58333333333333570, 1.299038105676657340 ) ) ;
#154741 = CARTESIAN_POINT ( 'NONE',  ( 4.909461021924240498, 7.781436054670031410, 1.082531754730549078 ) ) ;
#154742 = CARTESIAN_POINT ( 'NONE',  ( 5.149538872483485186, 0.5550977867328189541, -1.680460614999980340 ) ) ;
#154743 = CARTESIAN_POINT ( 'NONE',  ( 3.580729931658500398, -1.350255368601901651, 1.493277094049742182 ) ) ;
#154744 = CARTESIAN_POINT ( 'NONE',  ( 7.262363838414439776, 11.62450824479221900, 0.7998128361456462443 ) ) ;
#154745 = CARTESIAN_POINT ( 'NONE',  ( 2.221831145078187575, -2.042928948074810069, 0.5108812299794410761 ) ) ;
#154747 = CARTESIAN_POINT ( 'NONE',  ( -0.7500000000000006661, 2.608333333333358262, -1.299038105676652011 ) ) ;
#154746 = CARTESIAN_POINT ( 'NONE',  ( 0.6823417656249969321, 10.27604166700806587, -1.181850606188757036 ) ) ;
#154748 = CARTESIAN_POINT ( 'NONE',  ( 1.433975083751269697, 1.170624227716898780, 1.583764482814524088 ) ) ;
#154749 = CARTESIAN_POINT ( 'NONE',  ( -4.604929450496978660, 5.401447776115099408, -1.199719254218453823 ) ) ;
#154750 = CARTESIAN_POINT ( 'NONE',  ( 0.3616705494772323726, -0.5269360983083425376, 1.889693748445469224 ) ) ;
#154752 = VERTEX_POINT ( 'NONE', #38383 ) ;
#154751 = CARTESIAN_POINT ( 'NONE',  ( 6.275650443109183740, 0.3000964294621047967, -1.786390703358155196 ) ) ;
#154753 = CARTESIAN_POINT ( 'NONE',  ( 4.677199807034550183, 8.400557508274889784, 1.040834085586084257E-14 ) ) ;
#154754 = CARTESIAN_POINT ( 'NONE',  ( 1.364683531249986537, -0.07395833299191513499, 0.7879004041258500513 ) ) ;
#154755 = CARTESIAN_POINT ( 'NONE',  ( 4.574985519202336981, -0.0001439422951596270033, -1.870836309977530920 ) ) ;
#154756 = EDGE_LOOP ( 'NONE', ( #16740, #98801, #158397, #20998 ) ) ;
#154757 = CARTESIAN_POINT ( 'NONE',  ( 5.155165671438199482, 1.724248240607465732, -1.145533019084030268 ) ) ;
#154758 = CARTESIAN_POINT ( 'NONE',  ( -2.153317591523261390E-14, 1.562499999999999334, 1.414508159514573427 ) ) ;
#154759 = CARTESIAN_POINT ( 'NONE',  ( -5.980555156959541208, 7.110307450275150210, 1.082531754730549078 ) ) ;
#154760 = CARTESIAN_POINT ( 'NONE',  ( 3.018384101681789389, -0.9522666703177655734, 1.551720975324444973 ) ) ;
#154761 = CARTESIAN_POINT ( 'NONE',  ( -1.500000000000001332, -1.099999999999976108, 0.000000000000000000 ) ) ;
#154762 = CARTESIAN_POINT ( 'NONE',  ( 6.401421083946654100, 10.62007503124645957, -0.7998128361456291469 ) ) ;
#154763 = CARTESIAN_POINT ( 'NONE',  ( -10.16591625214838679, 10.75465713712827487, 1.040834085586084257E-14 ) ) ;
#154764 = CARTESIAN_POINT ( 'NONE',  ( 5.318541398310776103, 9.426991741329731056, -0.7998128361456481317 ) ) ;
#154765 = CARTESIAN_POINT ( 'NONE',  ( 1.364683531249986537, 0.3635416670080869328, 0.7879004041258500513 ) ) ;
#154766 = TOROIDAL_SURFACE ( 'NONE', #102813, 0.8299999999999998490, 0.08000000000000000167 ) ;
#154767 = CARTESIAN_POINT ( 'NONE',  ( -1.201851678989727383E-14, 1.462500000000018119, 1.732050807568877637 ) ) ;
#154769 = CARTESIAN_POINT ( 'NONE',  ( 4.299907273828439180, 8.168308919441841454, 1.040834085586084257E-14 ) ) ;
#154768 = CARTESIAN_POINT ( 'NONE',  ( 5.037533845850875380, 1.831247050742194515, -0.7043679133837479345 ) ) ;
#154770 = CARTESIAN_POINT ( 'NONE',  ( 1.880232294074701604, -0.2495702131940503166, 2.000550610736756774 ) ) ;
#154771 = ADVANCED_FACE ( 'NONE', ( #50375 ), #153803, .F. ) ;
#154772 = CARTESIAN_POINT ( 'NONE',  ( 11.41381675112453387, 19.00000000000000000, -3.704697986577182522 ) ) ;
#154773 = CARTESIAN_POINT ( 'NONE',  ( 0.04676574305502100015, -1.756316032869180921, 1.310637071781264984 ) ) ;
#154774 = CARTESIAN_POINT ( 'NONE',  ( 1.499999999999990896, 5.306250000682820378, 1.214306433183764966E-14 ) ) ;
#154775 = CARTESIAN_POINT ( 'NONE',  ( 1.932664581101939838, 0.1784410483233467293, 1.861995071071875785 ) ) ;
#154776 = CARTESIAN_POINT ( 'NONE',  ( -1.364683531249997417, 5.509375000341417916, 1.214306433183764966E-14 ) ) ;
#154777 = CARTESIAN_POINT ( 'NONE',  ( 3.990493469460140830, -1.155612956054508977, 1.648335472937176194 ) ) ;
#154778 = CARTESIAN_POINT ( 'NONE',  ( -9.169391961543940539, 9.592045464756413509, 1.040834085586084257E-14 ) ) ;
#154780 = CARTESIAN_POINT ( 'NONE',  ( 3.198929712650464996, 1.915108447241938627, 0.9030302060772307238 ) ) ;
#154779 = CARTESIAN_POINT ( 'NONE',  ( -4.555176424511596878, 7.297827681030051750, 1.082531754730560403 ) ) ;
#154781 = CARTESIAN_POINT ( 'NONE',  ( -1.730579034767993219E-05, -9.953931234596399946, -9.500331159997283947 ) ) ;
#154782 = CARTESIAN_POINT ( 'NONE',  ( 5.002425025097493538, 2.064580399062130311, 0.1557331365308264881 ) ) ;
#154784 = CARTESIAN_POINT ( 'NONE',  ( 6.620655732516668834, 7.629137130509086262, 2.673739711112704143 ) ) ;
#154783 = CARTESIAN_POINT ( 'NONE',  ( 0.9078953525096540300, -0.9432727566685695786, -1.865958795489220723 ) ) ;
#154786 = ORIENTED_EDGE ( 'NONE', *, *, #11231, .T. ) ;
#154785 = CARTESIAN_POINT ( 'NONE',  ( 6.299803673773761936, -0.6120917497752301761, 1.720027978493202436 ) ) ;
#154787 = CARTESIAN_POINT ( 'NONE',  ( 8.101160479365381306, 9.410107633136481908, -1.199719254218446718 ) ) ;
#154788 = CARTESIAN_POINT ( 'NONE',  ( -9.587704862635016312, 4.026159954882873926, 6.671158199369250141 ) ) ;
#154789 = CARTESIAN_POINT ( 'NONE',  ( 8.080296363620359301, 8.529359967086321603, 1.040834085586084257E-14 ) ) ;
#154790 = CARTESIAN_POINT ( 'NONE',  ( 5.704304454332028484, 5.827645749575025569, -0.4508780309788811835 ) ) ;
#154791 = CARTESIAN_POINT ( 'NONE',  ( 5.918603479541379109, -0.6925943527147163659, -1.782627650866043911 ) ) ;
#154792 = CARTESIAN_POINT ( 'NONE',  ( -7.751511138711140170, 10.06651563329490529, -1.599625672291263179 ) ) ;
#154793 = CARTESIAN_POINT ( 'NONE',  ( 4.171104814498611368, 8.018039383557042044, 0.7998128361456321445 ) ) ;
#154794 = B_SPLINE_CURVE_WITH_KNOTS ( 'NONE', 3,
 ( #171592, #6934, #5864, #73014, #4786, #40549 ),
 .UNSPECIFIED., .F., .F.,
 ( 4, 2, 4 ),
 ( 0.000000000000000000, 0.0003097885599249449199, 0.0006195771198498898399 ),
 .UNSPECIFIED. ) ;
#154795 = FACE_OUTER_BOUND ( 'NONE', #92353, .T. ) ;
#154796 = CARTESIAN_POINT ( 'NONE',  ( 4.324687812634897988, 4.147816657603229373, 0.7216878364870317197 ) ) ;
#154797 = CARTESIAN_POINT ( 'NONE',  ( 3.225950485047770933, 5.851027101609320269, 1.199719254218450271 ) ) ;
#154798 = ORIENTED_EDGE ( 'NONE', *, *, #170324, .F. ) ;
#154799 = CARTESIAN_POINT ( 'NONE',  ( 6.116814581292481456, 0.2004514801264325186, 2.006445662566976651 ) ) ;
#154800 = DIRECTION ( 'NONE',  ( 0.000000000000000000, 0.000000000000000000, -1.000000000000000000 ) ) ;
#154801 = CARTESIAN_POINT ( 'NONE',  ( 2.494940289813108780, 3.447199233515649386, -11.73777120880564695 ) ) ;
#154802 = CARTESIAN_POINT ( 'NONE',  ( -0.1405533004718313439, 1.431097497908106808, -1.984188993888830632 ) ) ;
#154803 =( BOUNDED_CURVE ( )  B_SPLINE_CURVE ( 2, ( #165732, #163615, #96501, #31482, #16251, #132203, #210202, #179858, #62893 ),
 .UNSPECIFIED., .F., .T. ) 
 B_SPLINE_CURVE_WITH_KNOTS ( ( 3, 2, 2, 2, 3 ),
 ( 0.7410714285714286031, 0.7440476190476190688, 0.7500000000000000000, 0.7559523809523809312, 0.7589285714285713969 ),
 .UNSPECIFIED. ) 
 CURVE ( )  GEOMETRIC_REPRESENTATION_ITEM ( )  RATIONAL_B_SPLINE_CURVE ( ( 0.9330127018922194093, 0.9330127018922194093, 1.000000000000000000, 0.8660254037844387076, 1.000000000000000000, 0.8660254037844387076, 1.000000000000000000, 0.9330127018922194093, 0.9330127018922194093 ) ) 
 REPRESENTATION_ITEM ( '' )  );
#154804 = CARTESIAN_POINT ( 'NONE',  ( -4.772106882330227506, 7.550913215151819458, -1.082531754730549967 ) ) ;
#154805 = CARTESIAN_POINT ( 'NONE',  ( 10.24960094225127172, 11.06021530882240356, -0.7216878364870257245 ) ) ;
#154806 = CARTESIAN_POINT ( 'NONE',  ( 3.326963294591319009, -1.817917149290064982, -0.7580491890798303212 ) ) ;
#154807 = CARTESIAN_POINT ( 'NONE',  ( 4.060172857048785389, -1.158672032380179573, 1.650094836768666084 ) ) ;
#154808 = CARTESIAN_POINT ( 'NONE',  ( -7.881367368245678406, 8.089350105908421185, 0.7998128361456602331 ) ) ;
#154810 = EDGE_CURVE ( 'NONE', #95488, #11477, #51447, .T. ) ;
#154809 = CARTESIAN_POINT ( 'NONE',  ( -3.070003471035267939, 6.451017196056028524, -0.6895117023006979151 ) ) ;
#154811 = CARTESIAN_POINT ( 'NONE',  ( 4.646525747415945595, -1.761044916313101671, 1.304081410864160739 ) ) ;
#154812 = CARTESIAN_POINT ( 'NONE',  ( 9.574755730265700038, 4.231293077548122561, -7.158835739769526363 ) ) ;
#154813 = CARTESIAN_POINT ( 'NONE',  ( 3.522408793619712153, 1.222923848883204156, -1.488421986030899591 ) ) ;
#154814 = CARTESIAN_POINT ( 'NONE',  ( -6.333630315878337136, 10.54098580183340772, 0.000000000000000000 ) ) ;
#154815 = CARTESIAN_POINT ( 'NONE',  ( -0.1298852118743840378, 0.7651466308506644776, -1.811855282322960781 ) ) ;
#154816 = CARTESIAN_POINT ( 'NONE',  ( 0.4521680116954321371, 0.6883007682146925488, -2.096869779678663281 ) ) ;
#154817 = CARTESIAN_POINT ( 'NONE',  ( 0.07536363704235826688, -0.001874865094115066300, -2.144269471569634877 ) ) ;
#154818 = CARTESIAN_POINT ( 'NONE',  ( -1.364683531250014514, 13.33854166700806587, -0.7879004041258335089 ) ) ;
#154819 = CARTESIAN_POINT ( 'NONE',  ( 4.286349120214771879, 8.152491073559232859, -0.7998128361456221525 ) ) ;
#154820 = EDGE_LOOP ( 'NONE', ( #24035, #183776, #168522, #6047 ) ) ;
#154821 = CARTESIAN_POINT ( 'NONE',  ( 4.204437034013637664, 6.958908068774287692, -1.082531754730548412 ) ) ;
#154822 = ORIENTED_EDGE ( 'NONE', *, *, #137537, .T. ) ;
#154824 = CARTESIAN_POINT ( 'NONE',  ( 2.772137614628172653, 2.003179168937582855, -0.1996775111661793500 ) ) ;
#154823 = CARTESIAN_POINT ( 'NONE',  ( -0.1119450412391852639, -0.4286113830911059130, -1.901434273657340412 ) ) ;
#154825 = CARTESIAN_POINT ( 'NONE',  ( 5.202631756544580988, -1.620200680833181694, -1.630429044757361723 ) ) ;
#154827 = CARTESIAN_POINT ( 'NONE',  ( 3.238934005158759621, -0.1320712000743811398, -1.856290971584534377 ) ) ;
#154826 = CARTESIAN_POINT ( 'NONE',  ( -8.093291352714894415, 8.406871097780989288, -0.7998128361456362523 ) ) ;
#154828 = CARTESIAN_POINT ( 'NONE',  ( 7.014364370223726830, 9.276787413384745662, -1.599625672291269396 ) ) ;
#154830 = EDGE_CURVE ( 'NONE', #127020, #70402, #68595, .T. ) ;
#154829 = CARTESIAN_POINT ( 'NONE',  ( 11.48243876534946217, 13.79999999999998295, 3.199999999999997957 ) ) ;
#154831 = CARTESIAN_POINT ( 'NONE',  ( 6.240485052285455581, 1.095381943021833449, -1.567431287326017664 ) ) ;
#154832 = CARTESIAN_POINT ( 'NONE',  ( -7.366157530926372488, 7.488271962369228874, -0.7998128361456291469 ) ) ;
#154833 = CARTESIAN_POINT ( 'NONE',  ( -3.336715202739028552, 6.906935146588564223, 0.7216878364870338292 ) ) ;
#154834 = CARTESIAN_POINT ( 'NONE',  ( 5.741762370215764300, 2.088391581209507741, 0.1015199779932918489 ) ) ;
#154835 = CARTESIAN_POINT ( 'NONE',  ( 5.178851490740193242, 8.025448591630130579, 1.082531754730558626 ) ) ;
#154836 = VERTEX_POINT ( 'NONE', #102313 ) ;
#154837 = CARTESIAN_POINT ( 'NONE',  ( -11.89942855770814134, 13.79999999999999893, 0.6999999999999992895 ) ) ;
#154838 = CARTESIAN_POINT ( 'NONE',  ( -0.02319159430949970999, 0.003959926571647092407, -1.810968101872318714 ) ) ;
#154839 = CARTESIAN_POINT ( 'NONE',  ( -4.924636110261798372, 6.768494766770632332, 1.599625672291267398 ) ) ;
#154840 = CARTESIAN_POINT ( 'NONE',  ( 2.584235440824592001, -0.5423091454765850417, 1.647252552357024280 ) ) ;
#154841 = CYLINDRICAL_SURFACE ( 'NONE', #189177, 11.10000000000000320 ) ;
#154842 = DIRECTION ( 'NONE',  ( 0.000000000000000000, -0.000000000000000000, -1.000000000000000000 ) ) ;
#154843 = CARTESIAN_POINT ( 'NONE',  ( -6.205881626753225966, 8.263281202677319470, 1.599625672291283607 ) ) ;
#154844 = AXIS2_PLACEMENT_3D ( 'NONE', #68777, #167376, #87184 ) ;
#154845 = CARTESIAN_POINT ( 'NONE',  ( 0.000000000000000000, -3.600000000000005862, -4.899999999999999467 ) ) ;
#154846 = CARTESIAN_POINT ( 'NONE',  ( 0.5321919801732944988, 1.189095644551215525, 1.694524325727378322 ) ) ;
#154847 = CARTESIAN_POINT ( 'NONE',  ( 5.742758765878789085, 0.3605303665093100851, 1.789564367143759327 ) ) ;
#154848 = CARTESIAN_POINT ( 'NONE',  ( 3.696105151714265347, 0.8860871710942277435, -1.750347149911928968 ) ) ;
#154849 = CARTESIAN_POINT ( 'NONE',  ( -2.954552044183079750E-14, -0.1249999993171966028, 1.414508159514565433 ) ) ;
#154850 = CARTESIAN_POINT ( 'NONE',  ( -7.330154606482786050, 11.70359747420527619, 0.000000000000000000 ) ) ;
#154851 = CARTESIAN_POINT ( 'NONE',  ( 7.070740804726770357, 8.207951346058097286, 1.199719254218462483 ) ) ;
#154852 = CARTESIAN_POINT ( 'NONE',  ( 3.739029402251158984, 2.014021593674422572, 0.6637135986873595739 ) ) ;
#154853 = CARTESIAN_POINT ( 'NONE',  ( -2.494337075234348777, 5.853884321174607663, -0.7216878364870267237 ) ) ;
#154854 = CARTESIAN_POINT ( 'NONE',  ( -9.982881178363895103, 10.54111621771303753, 1.040834085586084257E-14 ) ) ;
#154855 = EDGE_CURVE ( 'NONE', #193391, #71097, #19983, .T. ) ;
#154856 = AXIS2_PLACEMENT_3D ( 'NONE', #44255, #176381, #94083 ) ;
#154857 = CARTESIAN_POINT ( 'NONE',  ( 2.202089267374872872, 0.7962392033929905910, -1.911209141678638090 ) ) ;
#154858 = CARTESIAN_POINT ( 'NONE',  ( 1.499999999999997113, 15.17708333401613352, -0.8660254037844378194 ) ) ;
#154860 = ORIENTED_EDGE ( 'NONE', *, *, #118886, .T. ) ;
#154859 = CARTESIAN_POINT ( 'NONE',  ( 4.090652671443067767, -1.278631810133125546, 1.816222553172279319 ) ) ;
#154861 = CARTESIAN_POINT ( 'NONE',  ( 2.057686432631794293, -1.410295276735703540, 1.815187820423395992 ) ) ;
#154863 = CARTESIAN_POINT ( 'NONE',  ( 6.244999159755385776, -0.2970413431409227312, -2.040939473721150144 ) ) ;
#154862 = CARTESIAN_POINT ( 'NONE',  ( 9.246297574839980271, 10.85006392781057905, 1.082531754730549967 ) ) ;
#154865 = CARTESIAN_POINT ( 'NONE',  ( 1.642778471875000035, -3.726041666188707691, -2.845375778867859751 ) ) ;
#154864 = CARTESIAN_POINT ( 'NONE',  ( 5.709392085130549077, 9.675058176045386205, 0.000000000000000000 ) ) ;
#154866 = FACE_OUTER_BOUND ( 'NONE', #113466, .T. ) ;
#154867 = CARTESIAN_POINT ( 'NONE',  ( 6.462460624273299814, -1.686435539877573220, -0.7394478613861471539 ) ) ;
#154868 = CARTESIAN_POINT ( 'NONE',  ( -5.718596324681298526, 6.117678329292076889, -0.7136201712047436363 ) ) ;
#154869 = CARTESIAN_POINT ( 'NONE',  ( 3.164218664783400747, 1.912571728330178855, -0.004505864839042527346 ) ) ;
#154870 = CARTESIAN_POINT ( 'NONE',  ( -0.2106725631050202496, 0.2307243749109839093, -2.036935839376171842 ) ) ;
#154871 = CARTESIAN_POINT ( 'NONE',  ( 3.961678648311004025, 1.711676862058534088, -0.2113787121680379411 ) ) ;
#154872 = CARTESIAN_POINT ( 'NONE',  ( 1.956267901341804283, -1.236798062192035363, 1.592663274815858676 ) ) ;
#154873 = CARTESIAN_POINT ( 'NONE',  ( 3.586856395851648394, -0.6656857563790157251, 2.200217309063193127 ) ) ;
#154874 = CARTESIAN_POINT ( 'NONE',  ( 3.638171750181828035, 1.021205778115843010, -2.018914226005202206 ) ) ;
#154875 = CARTESIAN_POINT ( 'NONE',  ( -0.01666059994226073634, -0.1612322585618740090, -2.171656592459796808 ) ) ;
#154876 = CARTESIAN_POINT ( 'NONE',  ( -4.814553946628611136, 8.631080347793099961, 0.000000000000000000 ) ) ;
#154877 = EDGE_LOOP ( 'NONE', ( #119174, #88116, #168234, #5476, #16811, #54282, #212825, #67111 ) ) ;
#154878 = CARTESIAN_POINT ( 'NONE',  ( 4.991328707773068807, 1.311207439723049317, 1.188721964340031301 ) ) ;
#154880 = CARTESIAN_POINT ( 'NONE',  ( 0.6742756655733075366, -1.268823270132292791, 1.908895542103898890 ) ) ;
#154879 = CARTESIAN_POINT ( 'NONE',  ( 5.338878628731272613, 9.450718510153643948, -0.7998128361456481317 ) ) ;
#154881 = CARTESIAN_POINT ( 'NONE',  ( 5.578019757025042047, -1.797138167560994759, -0.3993771437491022702 ) ) ;
#154882 = CARTESIAN_POINT ( 'NONE',  ( -3.972702704004144714, 4.593573561881607148, 1.199719254218462483 ) ) ;
#154883 = CARTESIAN_POINT ( 'NONE',  ( 6.158177532299373702, -1.552315630085840947, 1.547116483708823820 ) ) ;
#154884 = CARTESIAN_POINT ( 'NONE',  ( -3.983063267364693960, 7.868933921892603323, -0.7998128361456481317 ) ) ;
#154885 = DIRECTION ( 'NONE',  ( 0.000000000000000000, -1.000000000000000000, 0.000000000000000000 ) ) ;
#154886 = FACE_OUTER_BOUND ( 'NONE', #82668, .T. ) ;
#154887 = CARTESIAN_POINT ( 'NONE',  ( 6.215297738502283842, -1.773692237561547147, -1.067698627785176768 ) ) ;
#154888 = CARTESIAN_POINT ( 'NONE',  ( -0.1882626618336727398, -1.244567986390752390, -1.587255334073833790 ) ) ;
#154889 = B_SPLINE_CURVE_WITH_KNOTS ( 'NONE', 3,
 ( #968, #182942, #199170, #94536, #92410, #158449, #76125 ),
 .UNSPECIFIED., .F., .F.,
 ( 4, 3, 4 ),
 ( 4.755129718191212618E-15, 6.253302285471699906E-05, 0.0001620662963562105846 ),
 .UNSPECIFIED. ) ;
#154890 = STYLED_ITEM ( 'NONE', ( #5186 ), #105052 ) ;
#154891 =( BOUNDED_SURFACE ( )  B_SPLINE_SURFACE ( 3, 3, ( 
 ( #172867, #123139, #90549, #74288, #122053, #41809, #206402, #38584, #189097, #153399, #155541 ),
 ( #22293, #25520, #40730, #119900, #6052, #23376, #204244, #203188, #4970, #156613, #55896 ),
 ( #190154, #140383, #71048, #106836, #9278, #188017, #37510, #39645, #105753, #58027, #75349 ),
 ( #107922, #91628, #171780, #202107, #53767, #89486, #21228, #137164, #7120, #73193, #192272 ),
 ( #27657, #96959, #142512, #13537, #94817, #208521, #79607, #113253, #43933, #92688, #10329 ),
 ( #211726, #28732, #193357, #209583, #125250, #210669, #179258, #93753, #12462, #144654, #78537 ),
 ( #108982, #62297, #195500, #194424, #112186, #128456, #46065, #61229, #207471, #60156, #159791 ) ),
 .UNSPECIFIED., .T., .F., .F. ) 
 B_SPLINE_SURFACE_WITH_KNOTS ( ( 4, 3, 4 ),
 ( 4, 1, 1, 1, 1, 1, 1, 1, 4 ),
 ( 0.000000000000000000, 0.5000000000000000000, 1.000000000000000000 ),
 ( 0.000000000000000000, 0.2254179815473072723, 0.3971144120416517653, 0.5241699701252212629, 0.6156743509408303394, 0.6807935377546089351, 0.7289379548928518471, 0.7696256121123346006, 1.000000000000000000 ),
 .UNSPECIFIED. ) 
 GEOMETRIC_REPRESENTATION_ITEM ( )  RATIONAL_B_SPLINE_SURFACE ( (
 ( 1.000000000000000000, 1.000000000000000000, 1.000000000000000222, 0.9999999999999997780, 0.9999999999999997780, 1.000000000000000222, 0.9999999999999997780, 1.000000000000000222, 0.9999999999999992228, 1.000000000000000000, 1.000000000000000000),
 ( 0.3333333333333333703, 0.3333333333333334259, 0.3333333333333334259, 0.3333333333333332593, 0.3333333333333333703, 0.3333333333333334259, 0.3333333333333333703, 0.3333333333333334814, 0.3333333333333332038, 0.3333333333333333703, 0.3333333333333333703),
 ( 0.3333333333333333703, 0.3333333333333334259, 0.3333333333333334259, 0.3333333333333332593, 0.3333333333333333703, 0.3333333333333334259, 0.3333333333333333703, 0.3333333333333334814, 0.3333333333333332038, 0.3333333333333333703, 0.3333333333333333703),
 ( 1.000000000000000000, 1.000000000000000000, 1.000000000000000222, 0.9999999999999997780, 0.9999999999999997780, 1.000000000000000222, 0.9999999999999997780, 1.000000000000000222, 0.9999999999999992228, 1.000000000000000000, 1.000000000000000000),
 ( 0.3333333333333333703, 0.3333333333333334259, 0.3333333333333334259, 0.3333333333333332593, 0.3333333333333333703, 0.3333333333333334259, 0.3333333333333333703, 0.3333333333333334814, 0.3333333333333332038, 0.3333333333333333703, 0.3333333333333333703),
 ( 0.3333333333333333703, 0.3333333333333334259, 0.3333333333333334259, 0.3333333333333332593, 0.3333333333333333703, 0.3333333333333334259, 0.3333333333333333703, 0.3333333333333334814, 0.3333333333333332038, 0.3333333333333333703, 0.3333333333333333703),
 ( 1.000000000000000000, 1.000000000000000000, 1.000000000000000222, 0.9999999999999997780, 0.9999999999999997780, 1.000000000000000222, 0.9999999999999997780, 1.000000000000000222, 0.9999999999999992228, 1.000000000000000000, 1.000000000000000000) ) ) 
 REPRESENTATION_ITEM ( '' )  SURFACE ( )  );
#154892 = CARTESIAN_POINT ( 'NONE',  ( 0.6823417656249899377, 5.426041667008087543, -1.181850606188754593 ) ) ;
#154893 = CARTESIAN_POINT ( 'NONE',  ( 4.881433204766033818, 1.796953459403265674, -0.6949688560347905275 ) ) ;
#154894 = CARTESIAN_POINT ( 'NONE',  ( 1.364683531249997417, 10.98437500034139802, 2.602085213965210642E-15 ) ) ;
#154895 = CARTESIAN_POINT ( 'NONE',  ( 0.7037666293719077037, 1.955508453885120401, -1.053950084065604864 ) ) ;
#154897 = ORIENTED_EDGE ( 'NONE', *, *, #88561, .F. ) ;
#154896 = CARTESIAN_POINT ( 'NONE',  ( 2.854315967138055132, 6.433244981884085334, -0.2941531795266367211 ) ) ;
#154898 = PRESENTATION_STYLE_ASSIGNMENT (( #42227 ) ) ;
#154899 = CARTESIAN_POINT ( 'NONE',  ( 4.241003122976366058, 3.842258486427521103, -0.7998128361456211532 ) ) ;
#154900 = CARTESIAN_POINT ( 'NONE',  ( -0.4019237886467001974, 9.082585450998170273, 1.500000000000001998 ) ) ;
#154901 = DIRECTION ( 'NONE',  ( 0.7592566023652994600, -0.6507913734559651608, -0.000000000000000000 ) ) ;
#154902 = CARTESIAN_POINT ( 'NONE',  ( 11.95069383916873207, 7.566995367135784356, 0.4543839392838792124 ) ) ;
#154903 = CARTESIAN_POINT ( 'NONE',  ( 8.717529583462638954, 12.15390636647303069, 1.082531754730546636 ) ) ;
#154905 = CARTESIAN_POINT ( 'NONE',  ( 1.029656018189710309, 1.891699080040713410, -0.5197978237033786808 ) ) ;
#154904 = CIRCLE ( 'NONE', #168805, 0.07999999999999969635 ) ;
#154906 = CARTESIAN_POINT ( 'NONE',  ( 0.6823417656249899377, 2.655208333674753618, 1.181850606188767472 ) ) ;
#154907 = DIRECTION ( 'NONE',  ( 0.000000000000000000, -1.000000000000000000, 0.000000000000000000 ) ) ;
#154908 = CARTESIAN_POINT ( 'NONE',  ( 6.355910407107248083, -0.6622273607519140182, 1.846833223631501264 ) ) ;
#154909 = CARTESIAN_POINT ( 'NONE',  ( -7.309817376062285099, 11.67987070538135264, 0.000000000000000000 ) ) ;
#154910 = CARTESIAN_POINT ( 'NONE',  ( -4.406036734316890247, 7.123831375802920363, -1.082531754730548412 ) ) ;
#154911 = CARTESIAN_POINT ( 'NONE',  ( 0.6380306694902828646, -1.602208245511031803, -1.597717328844779239 ) ) ;
#154913 = ORIENTED_EDGE ( 'NONE', *, *, #106881, .F. ) ;
#154912 = CARTESIAN_POINT ( 'NONE',  ( -4.693093728624763372, 8.627026450037540428, 0.7998128361456481317 ) ) ;
#154914 = CARTESIAN_POINT ( 'NONE',  ( -0.6823417656249969321, 5.717708333674756283, -1.181850606188749264 ) ) ;
#154915 = CARTESIAN_POINT ( 'NONE',  ( 1.018573325691285003, 1.726041315240328444, 0.7214104187760682629 ) ) ;
#154916 = CARTESIAN_POINT ( 'NONE',  ( 0.1055823559395060729, -0.08803060671099156853, 1.732021048141555220 ) ) ;
#154918 = CARTESIAN_POINT ( 'NONE',  ( 4.247736854543925133, 2.191053489037126045, -0.05455935714590579716 ) ) ;
#154917 = CARTESIAN_POINT ( 'NONE',  ( 1.360316468749965590, 2.494791667008093849, 0.7853790794158861388 ) ) ;
#154919 = CARTESIAN_POINT ( 'NONE',  ( 4.594930786881223916, -0.5007672277346334466, -2.252456893713528530 ) ) ;
#154920 = CARTESIAN_POINT ( 'NONE',  ( 6.661407821810922947, 0.3568556019579691707, -2.029490769664368255 ) ) ;
#154921 = CARTESIAN_POINT ( 'NONE',  ( 2.343606807962240524, 1.941525774309307284, 0.04751797161560606525 ) ) ;
#154922 = CARTESIAN_POINT ( 'NONE',  ( -5.219525951136850139, 7.112532914458205013, -1.443375672974051449 ) ) ;
#154923 = FILL_AREA_STYLE_COLOUR ( '', #29842 ) ;
#154924 = CARTESIAN_POINT ( 'NONE',  ( 0.3282377607281097287, 2.823664549684629321, 1.224999999999951239 ) ) ;
#154925 = CARTESIAN_POINT ( 'NONE',  ( 3.727185537919291747, 2.006959858346604619, 0.1948421285040344286 ) ) ;
#154926 = CARTESIAN_POINT ( 'NONE',  ( -5.056828107772866510, 5.962349549565537643, -1.082531754730543971 ) ) ;
#154927 = CARTESIAN_POINT ( 'NONE',  ( -7.930593509350902792, 8.217056947189661287, -0.7998128361456362523 ) ) ;
#154928 = CARTESIAN_POINT ( 'NONE',  ( 7.899597058256738968, 12.36794700127490820, 1.040834085586084257E-14 ) ) ;
#154929 = CARTESIAN_POINT ( 'NONE',  ( 1.383131112650197281, 1.687622997524572677, -0.6969523973551354779 ) ) ;
#154930 = CARTESIAN_POINT ( 'NONE',  ( -5.101610940492132151, 9.173906207207963348, -0.7998128361456362523 ) ) ;
#154931 = CARTESIAN_POINT ( 'NONE',  ( -6.005335696210345020, 5.970922831858983315, 0.7998128361456282587 ) ) ;
#154932 = CARTESIAN_POINT ( 'NONE',  ( -10.32660017610915837, 5.019824769181640889, 7.354833152352289183 ) ) ;
#154933 = ORIENTED_EDGE ( 'NONE', *, *, #207563, .F. ) ;
#154934 = CARTESIAN_POINT ( 'NONE',  ( 5.225487584538335284, -1.957599804553040945, 0.6444962787128440951 ) ) ;
#154935 = CARTESIAN_POINT ( 'NONE',  ( -5.912764388891193157, 9.912325863766124456, 0.000000000000000000 ) ) ;
#154936 = UNCERTAINTY_MEASURE_WITH_UNIT (LENGTH_MEASURE( 1.000000000000000082E-05 ), #44739, 'distance_accuracy_value', 'NONE');
#154937 = CARTESIAN_POINT ( 'NONE',  ( 6.441532379824158383, 9.568852638886589546, -1.082531754730548412 ) ) ;
#154938 = CARTESIAN_POINT ( 'NONE',  ( -3.469997250093771246, 6.135748327496311383, -1.199719254218452935 ) ) ;
#154939 = CARTESIAN_POINT ( 'NONE',  ( -10.30827686509187835, 10.92074451889568643, 1.040834085586084257E-14 ) ) ;
#154940 = CARTESIAN_POINT ( 'NONE',  ( 5.707677564275420501, 1.530686452870811065, 1.317726828763097435 ) ) ;
#154942 = EDGE_LOOP ( 'NONE', ( #64741, #209768, #168348 ) ) ;
#154941 = CARTESIAN_POINT ( 'NONE',  ( 6.217462558288930019, 1.845152235743243052, 1.236491063047394201 ) ) ;
#154943 = CARTESIAN_POINT ( 'NONE',  ( -4.085803189671902480, 5.860132702740892263, -1.599625672291271394 ) ) ;
#154944 = CARTESIAN_POINT ( 'NONE',  ( 5.035963992472171746, 7.962709526937818083, 1.199719254218462483 ) ) ;
#154945 = CARTESIAN_POINT ( 'NONE',  ( 4.504794318429003575, 1.594258339665870938, -1.305997064384886830 ) ) ;
#154946 = CARTESIAN_POINT ( 'NONE',  ( 4.272111401563948085, 1.799923229630392640, -0.9091438646662284295 ) ) ;
#154947 = ORIENTED_EDGE ( 'NONE', *, *, #58935, .T. ) ;
#154948 = CARTESIAN_POINT ( 'NONE',  ( 0.1236583036082015280, 1.000000000000000888, -11.99936284241577233 ) ) ;
#154949 = CARTESIAN_POINT ( 'NONE',  ( 3.216308754939877446, 4.775446185561722956, -1.599625672291262513 ) ) ;
#154951 = ORIENTED_EDGE ( 'NONE', *, *, #52849, .T. ) ;
#154950 = CARTESIAN_POINT ( 'NONE',  ( -7.119966945832006289, 8.335658187339330283, 1.199719254218452047 ) ) ;
#154952 = CARTESIAN_POINT ( 'NONE',  ( 4.780342502845265074, 8.269896785439653897, -0.8296954209953393278 ) ) ;
#154953 = CARTESIAN_POINT ( 'NONE',  ( 3.796249832574852601, -1.863883295361246084, 0.7690029265580224926 ) ) ;
#154954 = CARTESIAN_POINT ( 'NONE',  ( 3.521284115754549582, -1.097709940230184200, -1.477957507169822104 ) ) ;
#154955 = CARTESIAN_POINT ( 'NONE',  ( 2.016686958704193344, -1.090287029490369930, -2.033897785187769536 ) ) ;
#154956 = CARTESIAN_POINT ( 'NONE',  ( 3.923105346307896202, 5.670318552149568703, -1.599625672291269396 ) ) ;
#154957 = CARTESIAN_POINT ( 'NONE',  ( 3.392016793147753617, -0.8794390384766533897, 1.974801309016629869 ) ) ;
#154958 = CARTESIAN_POINT ( 'NONE',  ( 6.760712154708803823, 11.03924794713562818, 1.040834085586084257E-14 ) ) ;
#154959 = VECTOR ( 'NONE', #16565, 1000.000000000000000 ) ;
#154960 = CARTESIAN_POINT ( 'NONE',  ( -5.274285450916075035, 6.112086766612214284, 1.199719254218450271 ) ) ;
#154961 = EDGE_CURVE ( 'NONE', #80044, #1738, #198729, .T. ) ;
#154962 = CARTESIAN_POINT ( 'NONE',  ( 3.638291363623618047, 0.06041265439583366065, -2.297745614018332105 ) ) ;
#154963 = CARTESIAN_POINT ( 'NONE',  ( 0.000000000000000000, 0.000000000000000000, 0.000000000000000000 ) ) ;
#154964 = CARTESIAN_POINT ( 'NONE',  ( 2.131529507118444133, -1.219933349377068099, -1.418231869465089057 ) ) ;
#154965 = CARTESIAN_POINT ( 'NONE',  ( 0.2101411907093185261, -0.8379918008738492796, -1.782380744178988285 ) ) ;
#154967 = CARTESIAN_POINT ( 'NONE',  ( -5.562588163356775972, 9.711712967216715953, 0.7998128361456291469 ) ) ;
#154966 = CARTESIAN_POINT ( 'NONE',  ( -1.364683531250012516, 4.738541667008091096, -0.7879004041258300672 ) ) ;
#154969 = CARTESIAN_POINT ( 'NONE',  ( 1.911028901235469313, 1.633884665098099598, -1.483674895440662667 ) ) ;
#154968 = CARTESIAN_POINT ( 'NONE',  ( -6.600121851754250812, 6.594563670001734046, 0.7998128361456341429 ) ) ;
#154970 = CARTESIAN_POINT ( 'NONE',  ( -3.805626687661477270, 7.453998545664736852, -0.4223333724091842267 ) ) ;
#154971 = CARTESIAN_POINT ( 'NONE',  ( 4.385172619016207918, 7.203452924572514959, 1.199719254218462483 ) ) ;
#154972 = CARTESIAN_POINT ( 'NONE',  ( -5.220052836461385404, 6.048815383081766583, -1.199719254218446718 ) ) ;
#154973 = CARTESIAN_POINT ( 'NONE',  ( 11.96533679318037890, 13.75246011186996498, 0.9151144679400620152 ) ) ;
#154974 = CARTESIAN_POINT ( 'NONE',  ( 6.543826718160733691, 0.7548084958455666404, -1.821436488709103019 ) ) ;
#154975 = CARTESIAN_POINT ( 'NONE',  ( 5.268348002110199602, 1.133478272989609348, 2.010090980756351176 ) ) ;
#154976 = CARTESIAN_POINT ( 'NONE',  ( 0.4144086874100678664, 0.7473079093508437909, 1.814158889769983185 ) ) ;
#154977 = CARTESIAN_POINT ( 'NONE',  ( 2.711848548736516040, 0.5542824208455496837, -1.986605816314121808 ) ) ;
#154978 = CARTESIAN_POINT ( 'NONE',  ( 7.619319141200072920, 7.991553207595983643, 0.7216878364870317197 ) ) ;
#154979 = EDGE_CURVE ( 'NONE', #170262, #110148, #124059, .T. ) ;
#154980 = CARTESIAN_POINT ( 'NONE',  ( 7.506374323821472849, 8.786466794993730289, -1.199719254218452047 ) ) ;
#154981 = CARTESIAN_POINT ( 'NONE',  ( 6.249945625775433555, 10.23542763013927726, -0.7216878364870267237 ) ) ;
#154982 = CARTESIAN_POINT ( 'NONE',  ( -1.364683531249997417, 3.071875000341423245, 1.214306433183764966E-14 ) ) ;
#154983 = CARTESIAN_POINT ( 'NONE',  ( 0.08058608058606961388, -6.134628647623513231, -10.99970480893079738 ) ) ;
#154984 = CARTESIAN_POINT ( 'NONE',  ( 4.433153041544209749, 7.155467067568137551, -1.082531754730548412 ) ) ;
#154985 = CARTESIAN_POINT ( 'NONE',  ( 5.775877569751362017, -2.119564319632438743, 0.4699819441058172842 ) ) ;
#154987 = CARTESIAN_POINT ( 'NONE',  ( 5.741722636381445533, 1.839460222191912964, 0.08393339073512617876 ) ) ;
#154986 = DIRECTION ( 'NONE',  ( 1.276756478318932585E-15, -1.000000000000000000, 1.665334536937738262E-16 ) ) ;
#154988 = CARTESIAN_POINT ( 'NONE',  ( 9.512045263456263555, -8.176568542494905500, -0.4655551865852067817 ) ) ;
#154989 = CARTESIAN_POINT ( 'NONE',  ( 4.570728514692611100, 8.499999999999511502, -0.1921259283747507873 ) ) ;
#154990 = CARTESIAN_POINT ( 'NONE',  ( 0.000000000000000000, -9.919999999999998153, 0.000000000000000000 ) ) ;
#154991 = CARTESIAN_POINT ( 'NONE',  ( 6.807534431281101028, -0.5077146954460194372, 2.213219090469565664 ) ) ;
#154992 = CARTESIAN_POINT ( 'NONE',  ( -4.331906098249381110, 7.414796467324478613, 1.153063172049747065 ) ) ;
#154993 = DIRECTION ( 'NONE',  ( 0.000000000000000000, 8.546850786086437571E-32, 1.000000000000000000 ) ) ;
#154994 = CARTESIAN_POINT ( 'NONE',  ( 6.569431593124095414, 6.790062804044275424, 0.3413723397009699734 ) ) ;
#154995 = CARTESIAN_POINT ( 'NONE',  ( -0.04057498839846879202, -1.478066481919372510, -1.213044814162365981 ) ) ;
#154996 = CARTESIAN_POINT ( 'NONE',  ( 1.393014870165907526, 1.336991634843522236, 1.159753417114619545 ) ) ;
#154998 = CARTESIAN_POINT ( 'NONE',  ( 6.287749749268194854, 1.925770139592613450, -0.5864224512089585284 ) ) ;
#154997 = TOROIDAL_SURFACE ( 'NONE', #168748, 12.17999999982603399, 0.5000000000000008882 ) ;
#155000 = CARTESIAN_POINT ( 'NONE',  ( 3.304201903042072175, 1.212927065539553206, -1.482701048864635496 ) ) ;
#154999 = CARTESIAN_POINT ( 'NONE',  ( -8.143643823302737061, 12.65266822716189843, 0.000000000000000000 ) ) ;
#155001 = CARTESIAN_POINT ( 'NONE',  ( -5.595925273716217951, 5.773232080116717846, -0.3509683264134528247 ) ) ;
#155002 = CARTESIAN_POINT ( 'NONE',  ( 4.123468233510577896, 0.2432657155154849538, -1.954413393957514788 ) ) ;
#155003 = CARTESIAN_POINT ( 'NONE',  ( 6.521752737896459706, -0.4354215942184087584, 1.979412122172687694 ) ) ;
#155004 = CARTESIAN_POINT ( 'NONE',  ( -2.272963308585411735, 5.803540959991587478, 0.7998128361456341429 ) ) ;
#155005 = CARTESIAN_POINT ( 'NONE',  ( 2.940157781200231746, 1.856316385841882965, 0.2306766016651334850 ) ) ;
#155007 = ORIENTED_EDGE ( 'NONE', *, *, #50194, .F. ) ;
#155006 = CARTESIAN_POINT ( 'NONE',  ( -0.005637892868452093476, -0.3948761927005627337, -1.788892068844874395 ) ) ;
#155009 = CARTESIAN_POINT ( 'NONE',  ( 4.378920427533921078, 4.211088041652093494, 1.214306433183764966E-14 ) ) ;
#155008 = CARTESIAN_POINT ( 'NONE',  ( 2.473496279428960776, 0.1070396533628548558, -2.204406164007084445 ) ) ;
#155010 = CARTESIAN_POINT ( 'NONE',  ( 0.6823417656249917140, 3.405208333674754506, 1.181850606188765695 ) ) ;
#155011 = CARTESIAN_POINT ( 'NONE',  ( 0.8892172652632176488, 0.1500229334146038762, 2.057259515242230830 ) ) ;
#155012 = CARTESIAN_POINT ( 'NONE',  ( 7.344766530301147789, 9.591980256816594164, 1.599625672291281386 ) ) ;
#155013 = FACE_OUTER_BOUND ( 'NONE', #99391, .T. ) ;
#155014 = CARTESIAN_POINT ( 'NONE',  ( -4.218316008240990271E-13, -9.350066838357692589, -9.500000000000001776 ) ) ;
#155015 = CARTESIAN_POINT ( 'NONE',  ( -5.576481253922474401, 5.400316305864649280, -0.7998128361456221525 ) ) ;
#155016 = DIRECTION ( 'NONE',  ( 1.000000000000000000, -0.000000000000000000, -0.000000000000000000 ) ) ;
#155018 = AXIS2_PLACEMENT_3D ( 'NONE', #75175, #109876, #42700 ) ;
#155017 = AXIS2_PLACEMENT_3D ( 'NONE', #132241, #146354, #129101 ) ;
#155019 = ORIENTED_EDGE ( 'NONE', *, *, #135163, .F. ) ;
#155020 = CARTESIAN_POINT ( 'NONE',  ( 2.611853368047814872, 0.5545374748289233491, -1.994631108499920646 ) ) ;
#155021 = CARTESIAN_POINT ( 'NONE',  ( 1.499999999999990896, 3.775000000000021227, 1.214306433183764966E-14 ) ) ;
#155022 = CARTESIAN_POINT ( 'NONE',  ( 3.825371897350130723, 7.614684313550482031, 0.7998128361456321445 ) ) ;
#155023 = CARTESIAN_POINT ( 'NONE',  ( -6.617491849531519144, 6.756558277422160863, -0.006230766683231955816 ) ) ;
#155024 = CARTESIAN_POINT ( 'NONE',  ( 1.365885014167470546, 0.5842608817006667010, -1.933330045775418116 ) ) ;
#155025 = CARTESIAN_POINT ( 'NONE',  ( 0.9486429539237110076, 2.913339070649072493, 1.028101543438982413 ) ) ;
#155026 = CARTESIAN_POINT ( 'NONE',  ( -1.201851678989727383E-14, 3.821875000341423689, 1.575800808251672791 ) ) ;
#155028 = CARTESIAN_POINT ( 'NONE',  ( 7.782016984564043227, 12.02284421539267356, 0.7216878364870438212 ) ) ;
#155027 = CARTESIAN_POINT ( 'NONE',  ( 0.1749903794560410675, 1.362372954287846882, -2.209288650253756536 ) ) ;
#155029 = CARTESIAN_POINT ( 'NONE',  ( 4.938827285099913311, 1.158512636183751665, 1.649828125244500843 ) ) ;
#155030 = CARTESIAN_POINT ( 'NONE',  ( 6.385945889491149607, -1.915137183225220197, 0.05458341080493907954 ) ) ;
#155031 = CARTESIAN_POINT ( 'NONE',  ( 6.539320575229278454, 2.035006821797652687, 2.408631514295301645 ) ) ;
#155032 = CARTESIAN_POINT ( 'NONE',  ( 3.790727848299980440, 1.850687065220711469, -1.173560875862532660 ) ) ;
#155033 = CARTESIAN_POINT ( 'NONE',  ( -1.500000000000013101, 1.410416667349486008, -0.8660254037844313801 ) ) ;
#155034 = CARTESIAN_POINT ( 'NONE',  ( 2.672007700615218528, 1.902801012812182169, -0.1915479950082218386 ) ) ;
#155035 = CARTESIAN_POINT ( 'NONE',  ( -4.717347382551060342, 7.590990148696470818, 1.199719254218464037 ) ) ;
#155036 = CARTESIAN_POINT ( 'NONE',  ( 3.646780131951580461, 7.198401220678078971, -0.7216878364870267237 ) ) ;
#155038 = CARTESIAN_POINT ( 'NONE',  ( 1.546500145565053108, -1.423948579484592747, 1.427951870166991544 ) ) ;
#155037 = CARTESIAN_POINT ( 'NONE',  ( -6.265276382846530545, 6.482112999508623297, 0.000000000000000000 ) ) ;
#155039 = CARTESIAN_POINT ( 'NONE',  ( 1.364683531249996529, 11.27604166700806410, 0.7879004041258405033 ) ) ;
#155041 = CARTESIAN_POINT ( 'NONE',  ( -5.173318132066234476, 8.193232366456022930, -1.199719254218453823 ) ) ;
#155040 = CARTESIAN_POINT ( 'NONE',  ( 5.882419586753742102, -0.3201050945752722532, -2.167950725039065052 ) ) ;
#155043 = ORIENTED_EDGE ( 'NONE', *, *, #1922, .T. ) ;
#155042 = CARTESIAN_POINT ( 'NONE',  ( 3.240908261985251837, -1.521742930289736728, 0.8118271961824756744 ) ) ;
#155044 = CARTESIAN_POINT ( 'NONE',  ( 6.064709079624690524, 0.6667526090060638122, 2.013086243192941716 ) ) ;
#155045 = CARTESIAN_POINT ( 'NONE',  ( 8.145751363712157911, 8.397798100619326078, -0.7998128361456281477 ) ) ;
#155046 = CARTESIAN_POINT ( 'NONE',  ( 3.974511587100456822, 7.788680618259193444, 1.040834085586084257E-14 ) ) ;
#155047 = CARTESIAN_POINT ( 'NONE',  ( -5.000000000000024869, 3.300000000000025135, 0.7750000000000238920 ) ) ;
#155048 = CARTESIAN_POINT ( 'NONE',  ( 0.3089402658475807195, -1.578002999302514642, 1.165503548361209063 ) ) ;
#155049 = FACE_OUTER_BOUND ( 'NONE', #100145, .T. ) ;
#155050 = CARTESIAN_POINT ( 'NONE',  ( 5.900823170445728572, 7.907379670318584353, 1.599625672291267398 ) ) ;
#155051 = DIRECTION ( 'NONE',  ( 5.578564026256490882E-16, 1.000000000000000000, 9.066213480720158442E-32 ) ) ;
#155052 = ORIENTED_EDGE ( 'NONE', *, *, #176811, .F. ) ;
#155053 = AXIS2_PLACEMENT_3D ( 'NONE', #181676, #48512, #100443 ) ;
#155054 = ORIENTED_EDGE ( 'NONE', *, *, #124593, .F. ) ;
#155055 = CARTESIAN_POINT ( 'NONE',  ( 2.367557981294612812, 0.4819373766774863177, -1.746117998840409191 ) ) ;
#155056 = ORIENTED_EDGE ( 'NONE', *, *, #45325, .F. ) ;
#155057 = CARTESIAN_POINT ( 'NONE',  ( 10.56588178375152864, 11.22128359066528169, -0.7998128361456281477 ) ) ;
#155058 = DIRECTION ( 'NONE',  ( 0.000000000000000000, 8.546850786086437571E-32, 1.000000000000000000 ) ) ;
#155059 = CARTESIAN_POINT ( 'NONE',  ( 3.826654739275455519, 1.278450958818643901, -1.283618901898140985 ) ) ;
#155060 = CARTESIAN_POINT ( 'NONE',  ( 6.143253000323500856, 10.18122924377050609, -0.7216878364870458196 ) ) ;
#155061 = CARTESIAN_POINT ( 'NONE',  ( -4.370663978927087356, 5.060324124126027279, 2.420000000000000373 ) ) ;
#155062 = CARTESIAN_POINT ( 'NONE',  ( 5.639205186016292615, 6.133955845365204773, 0.8069632701028349731 ) ) ;
#155063 = AXIS2_PLACEMENT_3D ( 'NONE', #36235, #183562, #35168 ) ;
#155065 = CARTESIAN_POINT ( 'NONE',  ( -1.402160292154681736E-14, 14.92187500034139980, 1.575800808251682339 ) ) ;
#155064 = CARTESIAN_POINT ( 'NONE',  ( 5.336322170104328855, -1.033901835001526104, 1.547212704913742520 ) ) ;
#155066 = CARTESIAN_POINT ( 'NONE',  ( 2.583477129321013255, -0.5985834622587657972, 1.819768813671450935 ) ) ;
#155067 = SURFACE_STYLE_FILL_AREA ( #121580 ) ;
#155068 = CARTESIAN_POINT ( 'NONE',  ( -11.52114515671133610, 8.081606464056415362, 2.192706985476595261 ) ) ;
#155069 = CARTESIAN_POINT ( 'NONE',  ( 5.187768293964614585, 7.852886447769140688, 1.258803494560766678 ) ) ;
#155070 = DIRECTION ( 'NONE',  ( -0.9632918427306580433, 0.000000000000000000, 0.2684563758389303945 ) ) ;
#155071 = CARTESIAN_POINT ( 'NONE',  ( 3.538314903486612817, 7.071858454135611538, 1.040834085586084257E-14 ) ) ;
#155072 = CARTESIAN_POINT ( 'NONE',  ( 6.426201623197458801, 9.480690412830290015, -1.082531754730537088 ) ) ;
#155073 = CARTESIAN_POINT ( 'NONE',  ( -4.090809663021341969, 5.795697244990093644, 1.599625672291267398 ) ) ;
#155075 = CARTESIAN_POINT ( 'NONE',  ( -1.249999999999963807, 8.500000000000000000, 10.85702537530424827 ) ) ;
#155074 = B_SPLINE_CURVE_WITH_KNOTS ( 'NONE', 3,
 ( #189713, #108540, #136718, #171330, #54394, #73839 ),
 .UNSPECIFIED., .F., .F.,
 ( 4, 2, 4 ),
 ( 0.0006305064395556263506, 0.0009448735008584378857, 0.001259240562161249421 ),
 .UNSPECIFIED. ) ;
#155076 = CARTESIAN_POINT ( 'NONE',  ( 0.9903105584966699348, -0.5097506344743455431, -2.027405242695742515 ) ) ;
#155077 = CARTESIAN_POINT ( 'NONE',  ( 7.178115983792402233, 7.339166500704784823, 0.7998128361456281477 ) ) ;
#155078 = CARTESIAN_POINT ( 'NONE',  ( 6.616243401494351417, -0.9090183210780745648, -1.698415751782512695 ) ) ;
#155079 = CARTESIAN_POINT ( 'NONE',  ( -4.904298879841297421, 6.744767997946721216, 1.599625672291267398 ) ) ;
#155080 = CARTESIAN_POINT ( 'NONE',  ( 2.080808903162992607, -0.08653491207171599975, -1.823647505904809174 ) ) ;
#155081 = CARTESIAN_POINT ( 'NONE',  ( 1.420000000000001039, 7.176846818246214177, -4.202462424328213153 ) ) ;
#155082 = CARTESIAN_POINT ( 'NONE',  ( 1.511816067030671729, -0.6413169068853613597, 1.801808535584384252 ) ) ;
#155083 =( BOUNDED_CURVE ( )  B_SPLINE_CURVE ( 2, ( #44384, #138689, #172249, #81135, #146164 ),
 .UNSPECIFIED., .F., .T. ) 
 B_SPLINE_CURVE_WITH_KNOTS ( ( 3, 2, 3 ),
 ( 0.2625000001274112593, 0.2666666666666666630, 0.2750000000000000222 ),
 .UNSPECIFIED. ) 
 CURVE ( )  GEOMETRIC_REPRESENTATION_ITEM ( )  RATIONAL_B_SPLINE_CURVE ( ( 0.9330127018922194093, 0.9330127039406037603, 1.000000000000000000, 0.8660254037844387076, 1.000000000000000000 ) ) 
 REPRESENTATION_ITEM ( '' )  );
#155084 = EDGE_CURVE ( 'NONE', #824, #123208, #203652, .T. ) ;
#155085 = CARTESIAN_POINT ( 'NONE',  ( 1.398812336859527550, 0.3809602064741451355, 1.932172009363951837 ) ) ;
#155086 = CARTESIAN_POINT ( 'NONE',  ( 3.808095655114822176, 1.371164123868431117, -1.375570907105559293 ) ) ;
#155087 = ORIENTED_EDGE ( 'NONE', *, *, #132620, .F. ) ;
#155088 = CARTESIAN_POINT ( 'NONE',  ( 0.000000000000000000, 0.5000000000000004441, 0.000000000000000000 ) ) ;
#155090 = CARTESIAN_POINT ( 'NONE',  ( 0.2208628207966298607, -1.659654761427356240, -0.8422171645118268213 ) ) ;
#155089 = CARTESIAN_POINT ( 'NONE',  ( -4.468294144155606773, 7.370704380560280100, 1.199719254218452935 ) ) ;
#155091 = CARTESIAN_POINT ( 'NONE',  ( 4.115782150200256950, 6.959440387612411349, 1.199719254218452047 ) ) ;
#155093 = EDGE_CURVE ( 'NONE', #195055, #198620, #61661, .T. ) ;
#155092 = CARTESIAN_POINT ( 'NONE',  ( 6.729185449012857312, -6.864242550357277040, 6.701130152864321232 ) ) ;
#155094 = CARTESIAN_POINT ( 'NONE',  ( 7.262363838414439776, 11.62450824479221900, 0.7998128361456462443 ) ) ;
#155095 = CARTESIAN_POINT ( 'NONE',  ( -5.088052786878465739, 9.158088361325352977, 0.000000000000000000 ) ) ;
#155096 = CARTESIAN_POINT ( 'NONE',  ( 0.7500000000000006661, 11.61458333401613174, 1.299038105676657340 ) ) ;
#155097 = EDGE_LOOP ( 'NONE', ( #106486, #61293, #127919, #165854 ) ) ;
#155098 = CIRCLE ( 'NONE', #196675, 0.08000000000000012657 ) ;
#155099 = CARTESIAN_POINT ( 'NONE',  ( 5.365994935958575240, 9.482354201918870018, 0.7998128361456341429 ) ) ;
#155100 = CARTESIAN_POINT ( 'NONE',  ( 0.3985077402206628205, -4.205987624083942222, 1.000000000000004441 ) ) ;
#155102 = CARTESIAN_POINT ( 'NONE',  ( 5.858611323429600226, -1.916351766245901977, -0.6279953093112633500 ) ) ;
#155101 = CARTESIAN_POINT ( 'NONE',  ( 3.650846181029033133, -1.491723252493650564, 1.052289205326197852 ) ) ;
#155103 = DIRECTION ( 'NONE',  ( 0.000000000000000000, -0.7766560405359869135, 0.6299249119529750640 ) ) ;
#155104 = CARTESIAN_POINT ( 'NONE',  ( -8.839552966430002101, 12.29626697993494666, -1.082531754730543971 ) ) ;
#155105 = CARTESIAN_POINT ( 'NONE',  ( -4.662743238902972820, 8.402825839448235357, 0.5650157067484343765 ) ) ;
#155106 = CARTESIAN_POINT ( 'NONE',  ( 11.84668730067608600, 13.39999999999998259, 1.399999999999998579 ) ) ;
#155107 = CARTESIAN_POINT ( 'NONE',  ( 4.592568387165754551, -0.4099775813008778025, -1.825014511474598589 ) ) ;
#155108 = CARTESIAN_POINT ( 'NONE',  ( 8.158255747121103241, 10.54105100977322174, 1.599625672291281386 ) ) ;
#155109 = CARTESIAN_POINT ( 'NONE',  ( 2.561056213344356181, -1.676160556340213992, -0.9495491084439124929 ) ) ;
#155110 = CARTESIAN_POINT ( 'NONE',  ( 6.543807102324334934, 1.350441955444921849, 1.423202910149905298 ) ) ;
#155111 = PRESENTATION_LAYER_ASSIGNMENT (  '', '', ( #44419 ) ) ;
#155112 = CARTESIAN_POINT ( 'NONE',  ( 1.364683531249996529, 9.276041667008062319, 0.7879004041258405033 ) ) ;
#155113 = CARTESIAN_POINT ( 'NONE',  ( -5.038826645773246682, 9.030381520044109322, 0.7998128361456481317 ) ) ;
#155114 = CARTESIAN_POINT ( 'NONE',  ( 5.522248639467795428, 5.337044922334209573, -0.7998128361456231517 ) ) ;
#155115 = CARTESIAN_POINT ( 'NONE',  ( -5.790741006368224753, 5.928488393617260321, 0.7216878364870257245 ) ) ;
#155116 = ADVANCED_FACE ( 'NONE', ( #150016 ), #111460, .T. ) ;
#155117 = CARTESIAN_POINT ( 'NONE',  ( 0.1052747227462194346, -0.09900681772390507174, 2.115024835901352596 ) ) ;
#155118 = FACE_OUTER_BOUND ( 'NONE', #103767, .T. ) ;
#155119 = CARTESIAN_POINT ( 'NONE',  ( 0.9311234436981579154, -2.203130369558480961, -3.474999999999996536 ) ) ;
#155120 = CARTESIAN_POINT ( 'NONE',  ( 5.330949937734919430, -1.947458545883517189, -0.7027056652011903770 ) ) ;
#155122 = CARTESIAN_POINT ( 'NONE',  ( -1.201851678989727383E-14, 2.634375000341417916, 1.575800808251672791 ) ) ;
#155121 = CARTESIAN_POINT ( 'NONE',  ( 0.08126746489400815676, -0.8690269180096841239, 1.623235155968821841 ) ) ;
#155123 = CARTESIAN_POINT ( 'NONE',  ( 4.940191063930403637, -1.940984743010031544, -1.231243198015237628 ) ) ;
#155124 = CARTESIAN_POINT ( 'NONE',  ( 6.263503779833467178, 9.290876262238963790, -1.082531754730537088 ) ) ;
#155126 = DIRECTION ( 'NONE',  ( -0.000000000000000000, -1.000000000000000000, -0.000000000000000000 ) ) ;
#155125 = CARTESIAN_POINT ( 'NONE',  ( 3.092668437693027794, 6.622213920701574885, -0.7216878364870338292 ) ) ;
#155127 = CARTESIAN_POINT ( 'NONE',  ( 0.8148889116572692881, 2.119938092393148565, 0.8724386107587696060 ) ) ;
#155128 = DIRECTION ( 'NONE',  ( 0.000000000000000000, 0.000000000000000000, 1.000000000000000000 ) ) ;
#155129 = CARTESIAN_POINT ( 'NONE',  ( -6.074935347375019390, 9.245119117649618801, 1.199719254218452047 ) ) ;
#155130 = CARTESIAN_POINT ( 'NONE',  ( 5.244061567092353826, 0.5653492691648214219, 1.857832877570769314 ) ) ;
#155131 = VERTEX_POINT ( 'NONE', #56773 ) ;
#155132 = CARTESIAN_POINT ( 'NONE',  ( 7.904040366642678173, 12.16520482781775137, 0.7216878364870438212 ) ) ;
#155133 = ORIENTED_EDGE ( 'NONE', *, *, #21155, .T. ) ;
#155134 = CARTESIAN_POINT ( 'NONE',  ( 5.801015586618943232, -0.2871438832755985326, -1.890612906794430614 ) ) ;
#155135 = CARTESIAN_POINT ( 'NONE',  ( 6.210172754313918908, 1.157103754073171675, -1.651340222398114843 ) ) ;
#155137 =( LENGTH_UNIT ( ) NAMED_UNIT ( * ) SI_UNIT ( .MILLI., .METRE. ) );
#155136 = CARTESIAN_POINT ( 'NONE',  ( -9.854078719034067291, 10.39084668182823634, 0.7998128361456462443 ) ) ;
#155138 = CARTESIAN_POINT ( 'NONE',  ( -1.642778471874998480, -2.588541666188707957, 2.845375778867863303 ) ) ;
#155140 = CARTESIAN_POINT ( 'NONE',  ( 1.691920373447815207, -1.760920987957525385, -0.1775098275408875104 ) ) ;
#155139 = CARTESIAN_POINT ( 'NONE',  ( 3.152369405254138446, -1.582674238129866184, 1.366072548952133259 ) ) ;
#155141 = CARTESIAN_POINT ( 'NONE',  ( 6.604150280000163242, -0.1430408514614608939, 1.983920101186954721 ) ) ;
#155142 = CARTESIAN_POINT ( 'NONE',  ( 4.312625044126452423, 2.094834666918590216, 0.9310453638207391025 ) ) ;
#155143 = CARTESIAN_POINT ( 'NONE',  ( 1.710509606392306647, -0.2150479285965025134, 1.726905287013901225 ) ) ;
#155144 = CARTESIAN_POINT ( 'NONE',  ( 4.813308228051395687, 5.574280006603454574, 1.199719254218462483 ) ) ;
#155145 = CARTESIAN_POINT ( 'NONE',  ( -2.666414593264807120, -0.4259009368094196502, -0.1247943508829715553 ) ) ;
#155146 = CARTESIAN_POINT ( 'NONE',  ( 2.459901920361181826, 1.337243170739129239, 1.103576756174700746 ) ) ;
#155147 = CARTESIAN_POINT ( 'NONE',  ( 1.360316468749997565, 2.067708333674723509, -0.7853790794159001276 ) ) ;
#155148 = CARTESIAN_POINT ( 'NONE',  ( 1.468971578825052804, 1.639158939101122758, 0.8813203298513817563 ) ) ;
#155149 = CARTESIAN_POINT ( 'NONE',  ( 2.910768570555821277, 0.7291657262279130913, 2.045214924614814578 ) ) ;
#155150 = CARTESIAN_POINT ( 'NONE',  ( 3.988069740714122791, 7.804498464141805592, 0.7998128361456321445 ) ) ;
#155151 = CARTESIAN_POINT ( 'NONE',  ( 4.505092375653735992, -0.09411930587044713137, 2.014432893821124004 ) ) ;
#155152 = CARTESIAN_POINT ( 'NONE',  ( 2.843750000000001332, 1.895863743164146298, 0.7852924748298368840 ) ) ;
#155153 = AXIS2_PLACEMENT_3D ( 'NONE', #72496, #93055, #10693 ) ;
#155154 = CARTESIAN_POINT ( 'NONE',  ( 0.7499999999999885647, 2.597916667349486897, -1.299038105676658228 ) ) ;
#155155 = CARTESIAN_POINT ( 'NONE',  ( 1.114139429068806919, -0.8636777455973219109, -1.721994443286285259 ) ) ;
#155156 = CARTESIAN_POINT ( 'NONE',  ( 1.364683531249997417, 14.73437500034140157, 2.602085213965210642E-15 ) ) ;
#155157 = CARTESIAN_POINT ( 'NONE',  ( 4.992532747203591192, -1.233408671777506349, 1.847344450390429937 ) ) ;
#155158 = VERTEX_POINT ( 'NONE', #155340 ) ;
#155159 = CARTESIAN_POINT ( 'NONE',  ( 1.499999999999987121, 0.2541666666666844154, 0.8660254037844524744 ) ) ;
#155160 = CARTESIAN_POINT ( 'NONE',  ( 6.265839547809997079, 10.46189657242035587, 0.7998128361456462443 ) ) ;
#155161 = CARTESIAN_POINT ( 'NONE',  ( 1.364683531249988757, -0.1156249996585798079, 0.000000000000000000 ) ) ;
#155162 = CARTESIAN_POINT ( 'NONE',  ( 0.9091800373960364778, -0.5448693228766487984, -2.153321320651789161 ) ) ;
#155163 = CARTESIAN_POINT ( 'NONE',  ( 6.285602425426498385, -1.847771260692541162, 0.6596951833430020340 ) ) ;
#155164 = CARTESIAN_POINT ( 'NONE',  ( 9.246297574839974942, 11.81043314211192019, 1.443375672974076540 ) ) ;
#155165 = DIRECTION ( 'NONE',  ( 0.000000000000000000, 0.000000000000000000, -1.000000000000000000 ) ) ;
#155166 = CARTESIAN_POINT ( 'NONE',  ( 5.800151253372650473, -2.262578822528161560, -0.008439264561578212892 ) ) ;
#155167 = VECTOR ( 'NONE', #4972, 1000.000000000000000 ) ;
#155168 = CARTESIAN_POINT ( 'NONE',  ( -3.851925040058333582, 7.508013290127760087, -0.7216878364870458196 ) ) ;
#155169 = CARTESIAN_POINT ( 'NONE',  ( 3.771981659335025938, -2.032644659601599457, 0.3498187521492699403 ) ) ;
#155170 = CARTESIAN_POINT ( 'NONE',  ( -7.067878151425722955, 7.140279352951794500, 0.7998128361456341429 ) ) ;
#155171 = CARTESIAN_POINT ( 'NONE',  ( -1.500000000000013101, 2.410416667349482456, -0.8660254037844313801 ) ) ;
#155172 = CARTESIAN_POINT ( 'NONE',  ( -1.001543065824772872E-14, 4.884375000341420581, 1.575800808251672791 ) ) ;
#155173 = CARTESIAN_POINT ( 'NONE',  ( 4.727732462671866642, -1.149354582003499159, -1.475719300151681512 ) ) ;
#155174 = CARTESIAN_POINT ( 'NONE',  ( 3.990606130280470509, -1.729166733334456030, 0.1323968765898491939 ) ) ;
#155175 = CARTESIAN_POINT ( 'NONE',  ( 3.614586527008158523, -0.1238012486478034802, 1.736083139875769676 ) ) ;
#155176 = CARTESIAN_POINT ( 'NONE',  ( 0.7148891103036036920, 2.120809155261915713, 0.8706237914077943341 ) ) ;
#155177 = CARTESIAN_POINT ( 'NONE',  ( -1.201851678989727383E-14, 3.759375000341422801, -1.575800808251660134 ) ) ;
#155178 = CARTESIAN_POINT ( 'NONE',  ( 5.003505698738024421, -2.080571448108500476, 0.2061593518874194064 ) ) ;
#155179 = CARTESIAN_POINT ( 'NONE',  ( 5.244061567092353826, 0.5653492691648214219, 1.857832877570769314 ) ) ;
#155181 = ORIENTED_EDGE ( 'NONE', *, *, #67497, .F. ) ;
#155180 = CARTESIAN_POINT ( 'NONE',  ( 8.939234941184713179, 14.72725019231858390, 8.009301753890152753 ) ) ;
#155182 =( NAMED_UNIT ( * ) SI_UNIT ( $, .STERADIAN. ) SOLID_ANGLE_UNIT ( ) );
#155183 = CARTESIAN_POINT ( 'NONE',  ( 0.9850002542920628379, -2.016597020373378513, 0.002813405579435435122 ) ) ;
#155184 = CARTESIAN_POINT ( 'NONE',  ( 1.266058358664986949, 0.6103625328083387425, -2.030891291126469600 ) ) ;
#155185 = CARTESIAN_POINT ( 'NONE',  ( -1.250000000000035749, 8.500000000000000000, -9.921567416492205638 ) ) ;
#155186 = CARTESIAN_POINT ( 'NONE',  ( -6.828502922777144768, 11.11833717654868892, 0.7998128361456481317 ) ) ;
#155187 = CARTESIAN_POINT ( 'NONE',  ( 5.957918438201454059, 9.038323046955323292, -1.199719254218440723 ) ) ;
#155188 = CARTESIAN_POINT ( 'NONE',  ( 2.051582899450168362, -1.892833867889589960, 0.9560217657286762538 ) ) ;
#155189 = CARTESIAN_POINT ( 'NONE',  ( 11.01135777277262306, 0.000000000000000000, 1.399999999999998579 ) ) ;
#155190 = CARTESIAN_POINT ( 'NONE',  ( 4.037589748876240670, -1.260430739550026269, -1.321009972365666307 ) ) ;
#155191 = ORIENTED_EDGE ( 'NONE', *, *, #101780, .T. ) ;
#155192 = CARTESIAN_POINT ( 'NONE',  ( -4.299344108864961989, 6.109263775132799168, -1.443375672974066548 ) ) ;
#155193 = LINE ( 'NONE', #71771, #12453 ) ;
#155194 = CARTESIAN_POINT ( 'NONE',  ( 1.642778471875000035, -1.013541666188708223, -2.845375778867859751 ) ) ;
#155195 = CARTESIAN_POINT ( 'NONE',  ( -8.044065211609668253, 8.279164256499745633, 0.7998128361456602331 ) ) ;
#155196 = CARTESIAN_POINT ( 'NONE',  ( 2.566670905829854021, 0.6845714803544473703, 1.900350667086497580 ) ) ;
#155197 = CARTESIAN_POINT ( 'NONE',  ( 5.860442804830619856, 0.8892231252738895808, 2.019869304780027353 ) ) ;
#155198 = CARTESIAN_POINT ( 'NONE',  ( -5.334207092333882017, 5.187939460669764635, 0.7998128361456281477 ) ) ;
#155199 = CARTESIAN_POINT ( 'NONE',  ( 3.168646232094144199, 1.351176984073151788, -1.279899388936973192 ) ) ;
#155200 = CARTESIAN_POINT ( 'NONE',  ( 2.920892028740289081, 5.495125569250587816, 1.199719254218452047 ) ) ;
#155201 = AXIS2_PLACEMENT_3D ( 'NONE', #21446, #1198, #120122 ) ;
#155202 = CYLINDRICAL_SURFACE ( 'NONE', #105891, 2.000000000000000000 ) ;
#155203 = CARTESIAN_POINT ( 'NONE',  ( -4.822949958159302497, 6.649860922651058992, -1.599625672291256295 ) ) ;
#155204 = CARTESIAN_POINT ( 'NONE',  ( -7.862839020921525091, 11.26073039346208660, -1.199719254218446718 ) ) ;
#155205 = CARTESIAN_POINT ( 'NONE',  ( 5.074738461036464088, -1.720261882950037124, -0.6118011564382742629 ) ) ;
#155207 = CARTESIAN_POINT ( 'NONE',  ( -4.233332884224245696, 7.524468121203685023, -1.021403520103405294 ) ) ;
#155206 = CARTESIAN_POINT ( 'NONE',  ( -6.994027139803241866, 9.253060644560830994, -1.599625672291271394 ) ) ;
#155208 = CARTESIAN_POINT ( 'NONE',  ( 5.763319317650291040, 7.363698819737331647, -1.304181885133362195 ) ) ;
#155209 = CARTESIAN_POINT ( 'NONE',  ( 1.018380972650875460, 1.732250818821230443, -0.07729615888975129023 ) ) ;
#155210 = CARTESIAN_POINT ( 'NONE',  ( -0.01232043299871990460, -0.3711077647031227333, -1.706071622908360119 ) ) ;
#155211 = CARTESIAN_POINT ( 'NONE',  ( 5.654963871297442601, -1.822634436652656342, 1.415334302069543027 ) ) ;
#155212 = CARTESIAN_POINT ( 'NONE',  ( 5.903649544107831382, 5.852288987739402870, -0.7998128361456481317 ) ) ;
#155213 = CARTESIAN_POINT ( 'NONE',  ( 0.2982115315293157320, -2.060280707965747027, -0.05303618902755858483 ) ) ;
#155214 = CARTESIAN_POINT ( 'NONE',  ( 5.469824908109481854, 8.468880595181346393, -1.199719254218446718 ) ) ;
#155215 = EDGE_CURVE ( 'NONE', #38980, #103298, #120653, .T. ) ;
#155216 = CARTESIAN_POINT ( 'NONE',  ( 5.729893540575130118, -2.074111880986319711, -0.9905765078317919636 ) ) ;
#155217 = CARTESIAN_POINT ( 'NONE',  ( -9.499668754385632852, -7.246166700194470067, -0.07933194154487524519 ) ) ;
#155218 = CARTESIAN_POINT ( 'NONE',  ( -7.584860592202423035, 7.813701877183096833, -0.7998128361456362523 ) ) ;
#155219 = CARTESIAN_POINT ( 'NONE',  ( 5.805500895539822181, -0.4530025297027094888, 1.814837910242727226 ) ) ;
#155221 = CARTESIAN_POINT ( 'NONE',  ( -6.116136693540540570, 10.14959355252370266, 0.000000000000000000 ) ) ;
#155220 = CARTESIAN_POINT ( 'NONE',  ( 3.814637755342592307, -0.6046605605216844870, -1.814329123173196834 ) ) ;
#155222 = CARTESIAN_POINT ( 'NONE',  ( 4.881566871873391555, 2.059980941486462047, -0.7921658822237286346 ) ) ;
#155223 = CARTESIAN_POINT ( 'NONE',  ( 5.014918053075636095, 0.1589874617720990202, 2.111459674661147368 ) ) ;
#155224 = CARTESIAN_POINT ( 'NONE',  ( 1.224999999999991207, 0.9166666673494643369, 0.7072540797572697269 ) ) ;
#155225 = CARTESIAN_POINT ( 'NONE',  ( -9.569358774149643310, 3.553052365627049625, 7.167287524840453727 ) ) ;
#155226 = CARTESIAN_POINT ( 'NONE',  ( 3.865483193227626124, 7.523831135491951372, -0.7216878364870338292 ) ) ;
#155227 = CARTESIAN_POINT ( 'NONE',  ( -4.285785955251283141, 8.014184357852876417, 0.000000000000000000 ) ) ;
#155228 = CARTESIAN_POINT ( 'NONE',  ( 5.461630201184114242, -1.671734486004393450, -1.304435072541964447 ) ) ;
#155229 = CARTESIAN_POINT ( 'NONE',  ( 2.239721530183640841, -2.061013379209011287, 1.037980457044695992 ) ) ;
#155230 = CARTESIAN_POINT ( 'NONE',  ( 3.350005920730843911, -0.7974703105717847462, 1.792663495558038056 ) ) ;
#155231 = CARTESIAN_POINT ( 'NONE',  ( -5.957882158562513908, 5.915560371269844353, -0.7998128361456361413 ) ) ;
#155232 = CARTESIAN_POINT ( 'NONE',  ( 6.930530977065029852, -1.274000060550171787, 1.622871787371343855 ) ) ;
#155233 = CARTESIAN_POINT ( 'NONE',  ( 4.039966587192267866, 4.776011108888172707, 1.082531754730560403 ) ) ;
#155234 = CARTESIAN_POINT ( 'NONE',  ( 4.203910148689107729, 7.062256385849379647, -1.199719254218448494 ) ) ;
#155235 = ORIENTED_EDGE ( 'NONE', *, *, #146492, .T. ) ;
#155236 = CARTESIAN_POINT ( 'NONE',  ( 5.489470343000498076, -0.4852711138302409077, 1.957169415941109047 ) ) ;
#155237 = CARTESIAN_POINT ( 'NONE',  ( -7.947050595904583403, 12.42330946186405249, 0.7998128361456481317 ) ) ;
#155238 = CARTESIAN_POINT ( 'NONE',  ( -10.71026998871754721, 6.055660674263378951, 4.667787751035539223 ) ) ;
#155239 = CARTESIAN_POINT ( 'NONE',  ( 2.993230899678362089, 0.2615320595270088644, 2.155169926569647565 ) ) ;
#155240 = DIRECTION ( 'NONE',  ( 0.000000000000000000, 0.000000000000000000, -1.000000000000000000 ) ) ;
#155241 = CARTESIAN_POINT ( 'NONE',  ( 0.2465380642357860586, 1.084720387836759725, -1.822023332652397354 ) ) ;
#155242 = CARTESIAN_POINT ( 'NONE',  ( 1.499999999999987121, 1.327083334016149641, -0.8660254037844253849 ) ) ;
#155243 = CARTESIAN_POINT ( 'NONE',  ( -6.730854013983878836, 14.55213468793103182, -9.890941155911500360 ) ) ;
#155244 = DIRECTION ( 'NONE',  ( -0.04529798058948674572, 1.504112749676232550E-16, -0.9989735196462989908 ) ) ;
#155245 = CARTESIAN_POINT ( 'NONE',  ( 4.941988244637107286, 8.095350367992509177, 1.064974588601754757 ) ) ;
#155246 = CIRCLE ( 'NONE', #210584, 0.07999999999999952982 ) ;
#155247 = CARTESIAN_POINT ( 'NONE',  ( 1.528665837207894285, 1.985218273788964316, 0.5525772030575173410 ) ) ;
#155249 = CYLINDRICAL_SURFACE ( 'NONE', #159047, 4.500000000000000000 ) ;
#155248 = CARTESIAN_POINT ( 'NONE',  ( -7.994504133552415404, 12.47867192245318435, -0.7998128361456281477 ) ) ;
#155250 = CARTESIAN_POINT ( 'NONE',  ( -0.6823417656250212460, 1.301041667008083547, 1.181850606188755259 ) ) ;
#155251 = CYLINDRICAL_SURFACE ( 'NONE', #70357, 0.04999999999999991257 ) ;
#155252 = ORIENTED_EDGE ( 'NONE', *, *, #161057, .T. ) ;
#155253 = CARTESIAN_POINT ( 'NONE',  ( 3.897043152223302886, -0.1904361752127527174, -1.902785305300330743 ) ) ;
#155254 = CARTESIAN_POINT ( 'NONE',  ( 5.155052684544634722, -1.496415494590461748, -0.9447146595812674352 ) ) ;
#155255 = CARTESIAN_POINT ( 'NONE',  ( 4.877901405866606588, 8.912911750144889567, 0.7998128361456341429 ) ) ;
#155256 = CARTESIAN_POINT ( 'NONE',  ( -2.930533758848195447, 6.570706485298192234, -0.7998128361456281477 ) ) ;
#155257 = CARTESIAN_POINT ( 'NONE',  ( 0.5447927104418804900, 0.1337802856970966847, 1.806726864048732173 ) ) ;
#155259 = CARTESIAN_POINT ( 'NONE',  ( 0.7080363470168028472, 1.138615994813133359, -1.540489816406021673 ) ) ;
#155258 = CARTESIAN_POINT ( 'NONE',  ( 0.000000000000000000, -7.473374494045017968, 9.579665964948883783 ) ) ;
#155260 = AXIS2_PLACEMENT_3D ( 'NONE', #201367, #148397, #168892 ) ;
#155261 = CARTESIAN_POINT ( 'NONE',  ( 2.172408243068229439, -0.9739482337229148357, -1.826950231780352762 ) ) ;
#155262 = CARTESIAN_POINT ( 'NONE',  ( -1.364683531250014514, 0.5510416670080878765, -0.7879004041258289570 ) ) ;
#155263 = CARTESIAN_POINT ( 'NONE',  ( 6.016445890116215445, 1.255022122864515310, -1.387330985440645037 ) ) ;
#155264 = CARTESIAN_POINT ( 'NONE',  ( 2.473051018021198200, 0.08991741065280876855, -1.823594477012622228 ) ) ;
#155266 = CARTESIAN_POINT ( 'NONE',  ( 5.794989345469916842, 7.230977472937116346, 1.182549002416101835 ) ) ;
#155265 = CARTESIAN_POINT ( 'NONE',  ( 5.391335350415090488, 1.947751002805158560, -1.037606470750504828 ) ) ;
#155267 = CARTESIAN_POINT ( 'NONE',  ( 1.364683531249988757, -0.3656249996585800299, 0.000000000000000000 ) ) ;
#155268 = CARTESIAN_POINT ( 'NONE',  ( 3.613784930257180950, 0.5038104997578238820, -2.000076687661219044 ) ) ;
#155269 = CARTESIAN_POINT ( 'NONE',  ( -8.362681821530818738, 8.650883634741092010, -0.7998128361456291469 ) ) ;
#155270 = CARTESIAN_POINT ( 'NONE',  ( 7.944187942603509356, 11.35563746875774882, 1.199719254218460707 ) ) ;
#155271 = CARTESIAN_POINT ( 'NONE',  ( 3.669453130792974971, 7.432779085900453886, 1.040834085586084257E-14 ) ) ;
#155272 = CARTESIAN_POINT ( 'NONE',  ( 0.3687372981288695728, -1.412185959430117821, 1.636573055046482983 ) ) ;
#155273 = ADVANCED_FACE ( 'NONE', ( #157492 ), #90551, .T. ) ;
#155274 = CARTESIAN_POINT ( 'NONE',  ( 6.092251258522619395, 1.023830597077223903, -1.799436568697235783 ) ) ;
#155275 = CARTESIAN_POINT ( 'NONE',  ( -1.402160292154681736E-14, 2.009375000341422801, -1.575800808251660134 ) ) ;
#155276 = CARTESIAN_POINT ( 'NONE',  ( 3.796290242343594024, -2.158924006851222988, -0.1102321833298808840 ) ) ;
#155278 = CARTESIAN_POINT ( 'NONE',  ( 2.365611650783586040, -0.4327418640146083462, 1.913375882425945917 ) ) ;
#155277 = CARTESIAN_POINT ( 'NONE',  ( 3.738929604108613969, 1.918458267904774806, 0.6316034170958833016 ) ) ;
#155279 = CARTESIAN_POINT ( 'NONE',  ( 6.224601922449876312, 6.434659462379210382, 0.000000000000000000 ) ) ;
#155282 = CARTESIAN_POINT ( 'NONE',  ( 6.697364695470787943, 7.876308901879812474, -1.082531754730543083 ) ) ;
#155281 = CARTESIAN_POINT ( 'NONE',  ( 3.285556943750000070, -3.084374999522042415, 0.000000000000000000 ) ) ;
#155280 = DIRECTION ( 'NONE',  ( -1.000000000000000000, 7.771561172376094797E-16, -3.330669073875481454E-16 ) ) ;
#155283 = CARTESIAN_POINT ( 'NONE',  ( -7.014364370223741929, 9.276787413384745662, -1.599625672291271394 ) ) ;
#155284 = CARTESIAN_POINT ( 'NONE',  ( 2.061732777098632230, 1.244387006429502396, 1.586668050434843158 ) ) ;
#155285 = CARTESIAN_POINT ( 'NONE',  ( -3.765413976293358278, 5.416068943807445635, 1.599625672291267398 ) ) ;
#155286 = CARTESIAN_POINT ( 'NONE',  ( 4.702146809683721784, 5.356480858934594025, 2.500000000000011102 ) ) ;
#155287 = CARTESIAN_POINT ( 'NONE',  ( 5.959226163113887864, -1.611951592244726950, 1.028742869173946861 ) ) ;
#155288 = CARTESIAN_POINT ( 'NONE',  ( -11.86145016429273014, 12.69999999999999929, 1.099999999999996980 ) ) ;
#155289 = CARTESIAN_POINT ( 'NONE',  ( 5.138177029454836564, 7.977995053463880382, 1.082531754730558626 ) ) ;
#155291 = CARTESIAN_POINT ( 'NONE',  ( 3.919546125582054508, -1.392558991000433011, -1.458545569310132350 ) ) ;
#155290 = CARTESIAN_POINT ( 'NONE',  ( -7.171900071504738072, 10.35067193585544665, -1.082531754730543083 ) ) ;
#155292 = CARTESIAN_POINT ( 'NONE',  ( -1.500000000000011324, 3.920833333333357817, 0.8660254037844403729 ) ) ;
#155293 = CARTESIAN_POINT ( 'NONE',  ( -1.364683531250000748, 8.359375000341396245, 0.000000000000000000 ) ) ;
#155294 = CARTESIAN_POINT ( 'NONE',  ( 6.616207624681263333, -0.8185094323158810248, -1.518158226148608625 ) ) ;
#155295 = CARTESIAN_POINT ( 'NONE',  ( 5.468734858265785093, 7.473552982767158070, 1.599625672291269396 ) ) ;
#155296 = CARTESIAN_POINT ( 'NONE',  ( 9.598809568795314107, 10.30095870645710754, -0.7216878364870257245 ) ) ;
#155297 = CARTESIAN_POINT ( 'NONE',  ( -6.717748655459638840, -7.246166700180801001, -6.717748655459603313 ) ) ;
#155298 = CARTESIAN_POINT ( 'NONE',  ( 4.042156614576187579, 1.861303109871172312, 0.1859210194900539903 ) ) ;
#155299 = CARTESIAN_POINT ( 'NONE',  ( 4.570507181582611267, 8.346359121906111511, 0.000000000000000000 ) ) ;
#155300 = CARTESIAN_POINT ( 'NONE',  ( 1.832961912758425349, -1.964510197511709189, -0.6532998099852762586 ) ) ;
#155301 = AXIS2_PLACEMENT_3D ( 'NONE', #201955, #70897, #38430 ) ;
#155302 = CARTESIAN_POINT ( 'NONE',  ( -5.899206235277530297, 9.896508017883515862, 0.7216878364870267237 ) ) ;
#155303 = ORIENTED_EDGE ( 'NONE', *, *, #38423, .T. ) ;
#155304 = CARTESIAN_POINT ( 'NONE',  ( 5.090160327287878594, 4.903218234782778850, -0.7998128361456481317 ) ) ;
#155305 = CARTESIAN_POINT ( 'NONE',  ( 0.3160300859305562593, 1.034144755472726995, -1.730879882831819705 ) ) ;
#155306 = CARTESIAN_POINT ( 'NONE',  ( 1.687489445765244289, 1.732788098368071461, -0.5283295289823899399 ) ) ;
#155307 = CARTESIAN_POINT ( 'NONE',  ( 3.567203813726958828, 6.215469311773181182, 1.082531754730549078 ) ) ;
#155308 = CARTESIAN_POINT ( 'NONE',  ( 6.116136693540529912, 10.14959355252369910, 1.530808498934192557E-16 ) ) ;
#155309 = CARTESIAN_POINT ( 'NONE',  ( 6.738039155867407537, 10.80487008191325771, -0.7216878364870267237 ) ) ;
#155310 = CARTESIAN_POINT ( 'NONE',  ( 7.079328764629950754, 11.41096732537697633, 0.7998128361456462443 ) ) ;
#155312 = CARTESIAN_POINT ( 'NONE',  ( 5.800374965758359203, 1.282846238547242557, -1.422814914302351852 ) ) ;
#155311 = CARTESIAN_POINT ( 'NONE',  ( -6.067437437315529536, 7.037430750744921859, 1.199719254218450271 ) ) ;
#155313 = CIRCLE ( 'NONE', #37645, 0.08000000000000061229 ) ;
#155314 = FACE_OUTER_BOUND ( 'NONE', #166442, .T. ) ;
#155315 = CARTESIAN_POINT ( 'NONE',  ( 1.364683531249984538, -1.032291666325247714, -0.7879004041258309554 ) ) ;
#155317 = VERTEX_POINT ( 'NONE', #105545 ) ;
#155316 = CARTESIAN_POINT ( 'NONE',  ( 3.823036129373602154, 6.443664003369091731, -1.082531754730548412 ) ) ;
#155318 = CARTESIAN_POINT ( 'NONE',  ( -6.534666852106790103, 10.56760239419251590, 0.7216878364870458196 ) ) ;
#155319 = CARTESIAN_POINT ( 'NONE',  ( 3.221700144506876917, -2.083771231579465866, 0.5749860669421111847 ) ) ;
#155320 = CARTESIAN_POINT ( 'NONE',  ( -4.442231607132987925, 5.211633625523774960, -1.199719254218453823 ) ) ;
#155321 = CARTESIAN_POINT ( 'NONE',  ( 7.363486825997814123, 7.763358516518489516, 0.000000000000000000 ) ) ;
#155322 = CARTESIAN_POINT ( 'NONE',  ( 1.301209403646291118, -0.3165094942152619772, -2.096747597609450953 ) ) ;
#155323 = CARTESIAN_POINT ( 'NONE',  ( 5.737271026523679041, -1.649412122839075234, 0.7826820710771440481 ) ) ;
#155324 = CARTESIAN_POINT ( 'NONE',  ( 1.686731049638652502, -0.2853660037422758866, -1.950466449893713428 ) ) ;
#155325 = CARTESIAN_POINT ( 'NONE',  ( 4.605663860560767375, 1.420894170025093439, 1.280184534114735095 ) ) ;
#155326 = ORIENTED_EDGE ( 'NONE', *, *, #183561, .F. ) ;
#155327 = FACE_OUTER_BOUND ( 'NONE', #37636, .T. ) ;
#155328 = CARTESIAN_POINT ( 'NONE',  ( 5.424252406547988237, 0.9690106866696795995, 1.714583495817107783 ) ) ;
#155329 = CARTESIAN_POINT ( 'NONE',  ( 0.005655660794708254786, -0.8285957215397036224, -1.754384556632330838 ) ) ;
#155330 = VERTEX_POINT ( 'NONE', #76218 ) ;
#155331 = CARTESIAN_POINT ( 'NONE',  ( -4.599959256786493533, 8.588645909551377855, 0.000000000000000000 ) ) ;
#155332 = CARTESIAN_POINT ( 'NONE',  ( -2.959422669532919326, 6.674686557755516780, 0.7998128361456352531 ) ) ;
#155333 = MANIFOLD_SOLID_BREP ( 'Sweep1[2]', #39627 ) ;
#155335 = ADVANCED_FACE ( 'NONE', ( #114918 ), #192083, .T. ) ;
#155334 = CARTESIAN_POINT ( 'NONE',  ( 5.682275777458846377, 7.722684055159064975, 1.443375672974064550 ) ) ;
#155337 = ORIENTED_EDGE ( 'NONE', *, *, #58229, .T. ) ;
#155336 = CARTESIAN_POINT ( 'NONE',  ( 4.688094572372190960, 1.103980140559155831, 1.561224650464939190 ) ) ;
#155338 = CARTESIAN_POINT ( 'NONE',  ( 0.6048602812970468312, -0.7454967350204609877, -2.077179305122120123 ) ) ;
#155339 = AXIS2_PLACEMENT_3D ( 'NONE', #27363, #30587, #146484 ) ;
#155340 = CARTESIAN_POINT ( 'NONE',  ( 4.363950690066983107, 4.004001632660354915, -0.1812806842866887536 ) ) ;
#155341 = CARTESIAN_POINT ( 'NONE',  ( 6.006499477249034769, -2.003593090125683762, -0.1951834861853833925 ) ) ;
#155342 = CARTESIAN_POINT ( 'NONE',  ( -1.500000000000001110, 8.770833333333337478, 0.8660254037844418162 ) ) ;
#155344 = CARTESIAN_POINT ( 'NONE',  ( 5.753138727196851043, 0.1435251449807967150, -2.011451301405759118 ) ) ;
#155343 = CARTESIAN_POINT ( 'NONE',  ( -6.326802395788107880, 6.950450678040672514, 0.9045734915664763731 ) ) ;
#155345 = CARTESIAN_POINT ( 'NONE',  ( 1.891162872569674080, 0.2007839719405466183, 2.060584128686280714 ) ) ;
#155346 = CARTESIAN_POINT ( 'NONE',  ( -6.250472511100020334, 7.250971670160158311, 1.199719254218450271 ) ) ;
#155347 = CARTESIAN_POINT ( 'NONE',  ( -4.820236115778962827, 8.125194398966316456, -0.8510355349711593576 ) ) ;
#155348 = CARTESIAN_POINT ( 'NONE',  ( 0.5851287433712646369, -0.2658872486876809327, -2.145209338178376335 ) ) ;
#155349 = CARTESIAN_POINT ( 'NONE',  ( 5.072158865288233009, 7.010880990960010273, 1.443375672974065660 ) ) ;
#155350 = CARTESIAN_POINT ( 'NONE',  ( 0.07933194154487524519, -9.746166700180788567, 9.499668754385634628 ) ) ;
#155351 = CARTESIAN_POINT ( 'NONE',  ( -8.012344526598182026E-15, 13.60937500034139447, -1.575800808251669460 ) ) ;
#155353 = CARTESIAN_POINT ( 'NONE',  ( -5.336015975430226099, 8.383046517047350932, -1.199719254218453823 ) ) ;
#155352 = CARTESIAN_POINT ( 'NONE',  ( 0.000000000000000000, 13.49999999999999822, 0.000000000000000000 ) ) ;
#155354 = CARTESIAN_POINT ( 'NONE',  ( 4.553154410594215662, -1.128159591824983377, 1.317121951208845454 ) ) ;
#155355 = CARTESIAN_POINT ( 'NONE',  ( -3.521367211247373508, 5.131347717920458962, -1.599625672291256295 ) ) ;
#155356 = CARTESIAN_POINT ( 'NONE',  ( 2.518496159030516601, 0.8812310945605882351, 1.873447404777649261 ) ) ;
#155357 = CARTESIAN_POINT ( 'NONE',  ( 4.728176305778284849, 2.111628383735635328, 0.1544883665849701437 ) ) ;
#155358 = CARTESIAN_POINT ( 'NONE',  ( 6.089583550832340819, 10.25626457594641749, 1.040834085586084257E-14 ) ) ;
#155359 = CARTESIAN_POINT ( 'NONE',  ( 0.08172171391242558092, -9.906619969460795261, 10.99969643042367018 ) ) ;
#155360 = CARTESIAN_POINT ( 'NONE',  ( 2.114047118560181016, 1.964524245714272643, -0.1396653253868378186 ) ) ;
#155361 = CARTESIAN_POINT ( 'NONE',  ( 6.058883744127357751, 6.050764970021646150, 0.4299300578466564993 ) ) ;
#155362 = CARTESIAN_POINT ( 'NONE',  ( 0.000000000000000000, 19.00000000000000000, -12.00000000000000178 ) ) ;
#155363 = CARTESIAN_POINT ( 'NONE',  ( 4.330218815260163723, 2.247629863848239040, 0.4493651543184833397 ) ) ;
#155364 = CARTESIAN_POINT ( 'NONE',  ( 1.629252094361890890, -1.719607636260962025, 0.6136192449261099746 ) ) ;
#155365 = CARTESIAN_POINT ( 'NONE',  ( 3.854260808034858155, 7.718664386007802136, -0.7998128361456362523 ) ) ;
#155366 = CARTESIAN_POINT ( 'NONE',  ( 5.626270559546814098, 7.587068290936515247, 1.443375672974062551 ) ) ;
#155367 = CARTESIAN_POINT ( 'NONE',  ( -8.193204901359996128, 8.453160561208463264, 1.040834085586084257E-14 ) ) ;
#155368 = CARTESIAN_POINT ( 'NONE',  ( 2.619392002094393490, 1.702953528017937090, 1.073460467912157101 ) ) ;
#155369 = CARTESIAN_POINT ( 'NONE',  ( 3.713678095275750657, 0.4809820416172749802, -1.901733992618503066 ) ) ;
#155370 = CARTESIAN_POINT ( 'NONE',  ( -8.453672473320708036, 9.821371626084353323, -1.199719254218446718 ) ) ;
#155371 = CARTESIAN_POINT ( 'NONE',  ( -7.386494761346872551, 7.511998731193139989, -0.7998128361456291469 ) ) ;
#155372 = DIRECTION ( 'NONE',  ( 0.000000000000000000, 1.000000000000000000, 0.000000000000000000 ) ) ;
#155374 = CARTESIAN_POINT ( 'NONE',  ( 4.258513496744737559, -1.310932089386746879, 1.189237179687177015 ) ) ;
#155373 = CARTESIAN_POINT ( 'NONE',  ( 6.404249610866886044, 1.549990571320001731, -1.403138301853884773 ) ) ;
#155375 = DIRECTION ( 'NONE',  ( 0.000000000000000000, 0.000000000000000000, -1.000000000000000000 ) ) ;
#155376 = CARTESIAN_POINT ( 'NONE',  ( 0.8498829323080080433, 2.188760582993890313, -0.1110106097068005726 ) ) ;
#155377 = CARTESIAN_POINT ( 'NONE',  ( 5.876847675788273939, 1.605460876287589045, -0.6722632963065499068 ) ) ;
#155378 =( GEOMETRIC_REPRESENTATION_CONTEXT ( 3 ) GLOBAL_UNCERTAINTY_ASSIGNED_CONTEXT ( ( #3806 ) ) GLOBAL_UNIT_ASSIGNED_CONTEXT ( ( #124958, #174717, #76120 ) ) REPRESENTATION_CONTEXT ( 'NONE', 'WORKASPACE' ) );
#155379 = CARTESIAN_POINT ( 'NONE',  ( 8.749089199520284410, 9.101692242395490240, 0.7998128361456481317 ) ) ;
#155380 = DIRECTION ( 'NONE',  ( 5.578564026256490882E-16, 1.000000000000000000, 9.066213480720158442E-32 ) ) ;
#155381 = CARTESIAN_POINT ( 'NONE',  ( 6.135373049470649320, 0.7166818055565070678, 2.184152129457237912 ) ) ;
#155382 = DIRECTION ( 'NONE',  ( 0.000000000000000000, -9.023263958591318651E-17, 1.000000000000000000 ) ) ;
#155383 = CARTESIAN_POINT ( 'NONE',  ( 5.501237755103592697, 1.708535605516453115, 0.2940088878824585472 ) ) ;
#155384 = CARTESIAN_POINT ( 'NONE',  ( 2.350463684150871035, 2.206416367115513477, 0.05273732197710182673 ) ) ;
#155385 = DIRECTION ( 'NONE',  ( -0.6483454320283789096, 0.000000000000000000, 0.7613463080411795314 ) ) ;
#155386 = CARTESIAN_POINT ( 'NONE',  ( 5.406739488685087025, 0.6250254011054052761, 2.079287783280135304 ) ) ;
#155387 = CARTESIAN_POINT ( 'NONE',  ( -1.500000000000015099, 11.22916666666666785, -0.8660254037844309360 ) ) ;
#155388 = CARTESIAN_POINT ( 'NONE',  ( 0.6732554233833996093, 1.864234297354839143, -1.003953180072956419 ) ) ;
#155389 = CARTESIAN_POINT ( 'NONE',  ( 4.187500000000002665, -1.451031289060945584, 1.451031289061284646 ) ) ;
#155390 = CARTESIAN_POINT ( 'NONE',  ( -0.3190191529056556341, 8.208688096292659608, -1.977123213039569727 ) ) ;
#155391 = CARTESIAN_POINT ( 'NONE',  ( 4.594702886556338406, -0.4214696541114425488, -1.879573207023744974 ) ) ;
#155392 = CARTESIAN_POINT ( 'NONE',  ( 1.541950133533489975, -2.090104109921666620, 0.7524221467923494222 ) ) ;
#155393 = VERTEX_POINT ( 'NONE', #180917 ) ;
#155394 = AXIS2_PLACEMENT_3D ( 'NONE', #89987, #71561, #137668 ) ;
#155395 = CARTESIAN_POINT ( 'NONE',  ( 1.499999999999989120, 3.754166666666685082, 0.8660254037844524744 ) ) ;
#155396 = CARTESIAN_POINT ( 'NONE',  ( 3.825371897350130723, 7.614684313550482031, 0.7998128361456321445 ) ) ;
#155397 = CARTESIAN_POINT ( 'NONE',  ( 5.686755365928134687, 8.721966129303114101, 1.199719254218462483 ) ) ;
#155398 = CARTESIAN_POINT ( 'NONE',  ( 3.510577332121900707, -2.218788133798971884, -0.1078075537720973032 ) ) ;
#155399 = CARTESIAN_POINT ( 'NONE',  ( -8.026063749610056419, 10.38682701267698150, -1.443375672974059665 ) ) ;
#155400 = VECTOR ( 'NONE', #143964, 1000.000000000000000 ) ;
#155401 = CARTESIAN_POINT ( 'NONE',  ( 5.341549334104176872, 9.175631956522799726, 0.7216878364870438212 ) ) ;
#155402 = CARTESIAN_POINT ( 'NONE',  ( -7.971831134711019118, 12.24429405723079967, 0.000000000000000000 ) ) ;
#155403 = CARTESIAN_POINT ( 'NONE',  ( 5.370438244788902971, 9.279612028980123384, -0.7216878364870458196 ) ) ;
#155404 = CARTESIAN_POINT ( 'NONE',  ( 1.969375177810539945, -1.978050944945686673, -0.3905967402937361443 ) ) ;
#155406 = CARTESIAN_POINT ( 'NONE',  ( 6.162562474744170515, -0.7388518307863629619, -1.925989236560563977 ) ) ;
#155405 = CARTESIAN_POINT ( 'NONE',  ( 9.088043039861931405, 9.497138389460751284, 1.040834085586084257E-14 ) ) ;
#155407 = CARTESIAN_POINT ( 'NONE',  ( -11.35605497252127449, 11.11418145951643943, 3.553547709190206128 ) ) ;
#155408 = CARTESIAN_POINT ( 'NONE',  ( 7.309254211098767051, 7.700087132469628948, 0.7216878364870267237 ) ) ;
#155409 = CARTESIAN_POINT ( 'NONE',  ( 6.614805129994690169, -0.1227637983064084892, 1.711830280531308812 ) ) ;
#155410 = CARTESIAN_POINT ( 'NONE',  ( -1.499999999999964029, 8.500000000000000000, 9.886859966642596476 ) ) ;
#155411 = CARTESIAN_POINT ( 'NONE',  ( -1.201851678989727383E-14, 2.571875000341417472, 1.575800808251672791 ) ) ;
#155412 = CARTESIAN_POINT ( 'NONE',  ( 1.897346677678591442, -0.6019946308016431713, 1.664328231202655273 ) ) ;
#155413 = CARTESIAN_POINT ( 'NONE',  ( 0.5807041986926939625, -0.7231374404764076003, 1.882475062126743204 ) ) ;
#155414 = CARTESIAN_POINT ( 'NONE',  ( 6.321804186586025942, 0.9940233051523542640, -1.428469917405380318 ) ) ;
#155415 = CARTESIAN_POINT ( 'NONE',  ( 4.335649905164426166, 0.9806507323757740480, -2.072138663387664614 ) ) ;
#155416 = CARTESIAN_POINT ( 'NONE',  ( 3.415785861374909249, 1.167101634185686576, -1.423959568491977912 ) ) ;
#155417 = CARTESIAN_POINT ( 'NONE',  ( 8.585337585951586803, 11.03931315507545108, -1.599625672291255185 ) ) ;
#155418 = CARTESIAN_POINT ( 'NONE',  ( 7.416489442564358825, 14.99999999999999467, 9.452688479263381183 ) ) ;
#155419 = CARTESIAN_POINT ( 'NONE',  ( 3.117977517195897441, -0.8984765085307615529, -1.589086709143338272 ) ) ;
#155420 = CARTESIAN_POINT ( 'NONE',  ( 3.621720349255663773, 0.2986264320336135536, 1.994071497604548382 ) ) ;
#155421 = CARTESIAN_POINT ( 'NONE',  ( -10.01677656239806247, 10.58066083241955901, 0.7998128361456462443 ) ) ;
#155423 = DIRECTION ( 'NONE',  ( 0.000000000000000000, 1.000000000000000000, 0.000000000000000000 ) ) ;
#155422 = CARTESIAN_POINT ( 'NONE',  ( 3.696369045748033155, -2.259781416529721643, -0.1137371904085457408 ) ) ;
#155424 = CARTESIAN_POINT ( 'NONE',  ( 5.210040546657988436, -2.096114648464560748, 0.2032773619186321323 ) ) ;
#155425 = CARTESIAN_POINT ( 'NONE',  ( 9.153107034568822797, 14.18422307519461789, 6.999546554107224594 ) ) ;
#155426 = CARTESIAN_POINT ( 'NONE',  ( 3.543477799061961253, 1.872898848466747479, -0.8826743078152868849 ) ) ;
#155427 = CARTESIAN_POINT ( 'NONE',  ( 10.16199982864259788, 11.81442020729326536, 1.199719254218452047 ) ) ;
#155428 = CARTESIAN_POINT ( 'NONE',  ( 0.6801582343749744686, 0.3385416670080923507, -1.178068619123886718 ) ) ;
#155429 = CARTESIAN_POINT ( 'NONE',  ( 6.006510593949522026, -2.110231943656666331, -0.2080817731764383061 ) ) ;
#155431 = CARTESIAN_POINT ( 'NONE',  ( 0.7680398806059639538, 0.9487340639210088966, 1.676631345724951982 ) ) ;
#155430 = CARTESIAN_POINT ( 'NONE',  ( -9.989660255170729641, 10.54902514065433827, -0.7998128361456291469 ) ) ;
#155432 = UNCERTAINTY_MEASURE_WITH_UNIT (LENGTH_MEASURE( 1.000000000000000082E-05 ), #174971, 'distance_accuracy_value', 'NONE');
#155433 = CARTESIAN_POINT ( 'NONE',  ( -3.709037541790315640, 6.484905011134099340, -1.199719254218450271 ) ) ;
#155434 = CARTESIAN_POINT ( 'NONE',  ( 8.503988664269582998, 10.94440607977979063, 1.599625672291281386 ) ) ;
#155435 = CARTESIAN_POINT ( 'NONE',  ( 6.360183458142179447, 6.592837920686898556, -0.7216878364870458196 ) ) ;
#155436 = CARTESIAN_POINT ( 'NONE',  ( 4.722716239034094876, 6.809985054512954328, 1.237095216770202954 ) ) ;
#155437 = CARTESIAN_POINT ( 'NONE',  ( -1.007075241936694399, 2.800000000000025135, -0.9723682818829901819 ) ) ;
#155438 = CARTESIAN_POINT ( 'NONE',  ( -5.264643720808155791, 5.036505850564608089, 0.000000000000000000 ) ) ;
#155439 = CARTESIAN_POINT ( 'NONE',  ( 0.6861347341944658007, 2.138861475627896080, -0.5996866306409093239 ) ) ;
#155440 = CARTESIAN_POINT ( 'NONE',  ( 2.696425475562960195, -2.100245048574858497, -0.1560501473716560672 ) ) ;
#155441 = CARTESIAN_POINT ( 'NONE',  ( -4.787964524281469458, 5.614988695530339413, -1.199719254218453823 ) ) ;
#155442 = CARTESIAN_POINT ( 'NONE',  ( 8.423693512792301163, 8.722063941212843119, 0.7998128361456481317 ) ) ;
#155443 = CARTESIAN_POINT ( 'NONE',  ( 6.754761327113334879, -0.4959639348531270642, -1.793591138363290316 ) ) ;
#155444 = CARTESIAN_POINT ( 'NONE',  ( 7.130698725783555680, 10.40656671580112658, 1.199719254218460707 ) ) ;
#155445 = PRESENTATION_STYLE_ASSIGNMENT (( #43858 ) ) ;
#155446 = CARTESIAN_POINT ( 'NONE',  ( -7.593975437430151132, 8.032261896522864930, -0.7216878364870338292 ) ) ;
#155447 = CARTESIAN_POINT ( 'NONE',  ( -9.219181267612684749, 10.81842823604534765, 1.082531754730558626 ) ) ;
#155449 = CARTESIAN_POINT ( 'NONE',  ( 0.5805319366703353134, 1.050441701016215923, 1.842106252469346117 ) ) ;
#155448 = CIRCLE ( 'NONE', #165804, 6.200000000000000178 ) ;
#155450 = LINE ( 'NONE', #7033, #185372 ) ;
#155452 = CARTESIAN_POINT ( 'NONE',  ( 3.033595934319989418, 1.863777508880835487, -0.6128360024686765328 ) ) ;
#155451 = CARTESIAN_POINT ( 'NONE',  ( 1.224999999999943023, -0.3958333333332818005, 0.7072540797572536286 ) ) ;
#155453 = CARTESIAN_POINT ( 'NONE',  ( 2.044033295145482043, 0.8276103948961744949, -1.997198329219296742 ) ) ;
#155454 = CARTESIAN_POINT ( 'NONE',  ( 1.048114208743459619, -1.451426956872736262, 1.132798186660122441 ) ) ;
#155456 = CARTESIAN_POINT ( 'NONE',  ( -4.553630449417391368, 6.998240405024593436, -1.173447104293420473 ) ) ;
#155455 = CARTESIAN_POINT ( 'NONE',  ( -5.496904935697871863, 5.377753611261092637, 0.7998128361456281477 ) ) ;
#155457 = ADVANCED_FACE ( 'NONE', ( #181969 ), #33599, .T. ) ;
#155458 = CARTESIAN_POINT ( 'NONE',  ( 3.784860527941535491, 1.262060850391345523, 1.198560274591720098 ) ) ;
#155459 = CARTESIAN_POINT ( 'NONE',  ( 5.477130870240836558, 9.333810415348903433, -0.7216878364870267237 ) ) ;
#155460 = CARTESIAN_POINT ( 'NONE',  ( -11.68287950975655676, 8.167437761341201252, 4.460353674290588266 ) ) ;
#155461 = CARTESIAN_POINT ( 'NONE',  ( 0.4620835240300471547, 2.137967531602209981, -0.3185850937674692407 ) ) ;
#155462 = EDGE_CURVE ( 'NONE', #48008, #185203, #61040, .T. ) ;
#155463 = CARTESIAN_POINT ( 'NONE',  ( 2.548203688163702463, 1.844428314090811538, -0.8144999995377337765 ) ) ;
#155464 = CARTESIAN_POINT ( 'NONE',  ( -7.015401035077384329, 6.062865449010541141, -2.437084766375293921 ) ) ;
#155465 = CARTESIAN_POINT ( 'NONE',  ( 2.553542074257345362, 0.5272840835596946940, -1.899572117879143596 ) ) ;
#155466 = B_SPLINE_CURVE_WITH_KNOTS ( 'NONE', 3,
 ( #43358, #173359, #26006, #11889 ),
 .UNSPECIFIED., .F., .F.,
 ( 4, 4 ),
 ( 0.000000000000000000, 0.0002908967400263835030 ),
 .UNSPECIFIED. ) ;
#155467 = CARTESIAN_POINT ( 'NONE',  ( 6.509000000000012776, 0.5843741663743782233, 2.053293374786519188 ) ) ;
#155470 = ORIENTED_EDGE ( 'NONE', *, *, #50541, .T. ) ;
#155469 = CARTESIAN_POINT ( 'NONE',  ( -3.499413046103020175, 7.096749297179887783, 0.7216878364870338292 ) ) ;
#155468 = FACE_OUTER_BOUND ( 'NONE', #165715, .T. ) ;
#155471 = CARTESIAN_POINT ( 'NONE',  ( -6.251718229232857915, 7.426664367927358512, -1.082531754730549967 ) ) ;
#155472 = CARTESIAN_POINT ( 'NONE',  ( -0.1110810684433168327, 2.049790377237853178, -2.213868588080004418 ) ) ;
#155473 = CARTESIAN_POINT ( 'NONE',  ( 6.235824307642648279, 6.239826211863360506, 0.000000000000000000 ) ) ;
#155474 = EDGE_CURVE ( 'NONE', #112831, #35502, #177841, .T. ) ;
#155475 = CARTESIAN_POINT ( 'NONE',  ( -4.782994330570982555, 8.802186828966616972, 0.000000000000000000 ) ) ;
#155476 = CARTESIAN_POINT ( 'NONE',  ( -7.228432174741334038, 8.462200954400218578, -1.199719254218452047 ) ) ;
#155477 = CARTESIAN_POINT ( 'NONE',  ( -10.61567108937589765, 11.48729714713446803, 0.7216878364870438212 ) ) ;
#155478 = CARTESIAN_POINT ( 'NONE',  ( 5.350698970897345141, 0.6634653876971875475, 2.210164229930264845 ) ) ;
#155479 = CARTESIAN_POINT ( 'NONE',  ( 6.672321430365630412, -0.9237476215336395402, -1.730755693189582667 ) ) ;
#155480 = CARTESIAN_POINT ( 'NONE',  ( 3.608209768781400761, 1.961936380018937331, 0.004537341891153179319 ) ) ;
#155481 = CARTESIAN_POINT ( 'NONE',  ( 9.121938423896107651, 9.536683004167278099, -0.7998128361456221525 ) ) ;
#155482 = CARTESIAN_POINT ( 'NONE',  ( 0.5279704824466545654, -1.728000714500482982, 1.038995864524896895 ) ) ;
#155483 = ORIENTED_EDGE ( 'NONE', *, *, #114444, .F. ) ;
#155484 = CARTESIAN_POINT ( 'NONE',  ( 2.395853177668628931, -2.093565527891564582, 0.3158384217898829727 ) ) ;
#155485 = CARTESIAN_POINT ( 'NONE',  ( -1.500000000000001332, 1.181250000682816603, 0.000000000000000000 ) ) ;
#155487 = CARTESIAN_POINT ( 'NONE',  ( -6.663996196316808174, 7.733415969579778171, -1.199719254218446718 ) ) ;
#155486 = CARTESIAN_POINT ( 'NONE',  ( -2.123823618835070537, 5.629544655282869847, 1.040834085586084257E-14 ) ) ;
#155488 = CARTESIAN_POINT ( 'NONE',  ( 3.697050842446505392, -0.5329721798031424873, 1.762307204009383454 ) ) ;
#155489 = ORIENTED_EDGE ( 'NONE', *, *, #209460, .T. ) ;
#155490 = CARTESIAN_POINT ( 'NONE',  ( -9.809487834687324437, 11.40315621434539395, 1.199719254218462483 ) ) ;
#155491 = CARTESIAN_POINT ( 'NONE',  ( 0.000000000000000000, 0.06547992991065912372, 0.000000000000000000 ) ) ;
#155492 = CARTESIAN_POINT ( 'NONE',  ( 3.603867943843573673, 1.538443694073919898, 1.459757404076333698 ) ) ;
#155493 = CARTESIAN_POINT ( 'NONE',  ( 0.05820987927622478519, -1.643049995186950829, -0.8308948761173093889 ) ) ;
#155494 = CARTESIAN_POINT ( 'NONE',  ( 1.499999999999989120, 5.327083334016152527, -0.8660254037844323793 ) ) ;
#155495 = CARTESIAN_POINT ( 'NONE',  ( 7.775764792637399836, 9.030479331953833011, -1.199719254218441611 ) ) ;
#155496 = CARTESIAN_POINT ( 'NONE',  ( 7.876360894896227371, 8.153785563659219804, -0.7998128361456341429 ) ) ;
#155497 = CARTESIAN_POINT ( 'NONE',  ( 4.042301887969748542, 2.050516515953205055, 0.2056252831919377910 ) ) ;
#155498 = STYLED_ITEM ( 'NONE', ( #156870 ), #25342 ) ;
#155500 = CARTESIAN_POINT ( 'NONE',  ( 1.557894219809667247, -1.301531972126177772, 1.302644501960325885 ) ) ;
#155499 = CARTESIAN_POINT ( 'NONE',  ( -6.877010230629689858, 9.046264573866535486, 1.599625672291283607 ) ) ;
#155501 = CARTESIAN_POINT ( 'NONE',  ( 1.364683531249988535, 4.363541667008090208, 0.7879004041258500513 ) ) ;
#155502 = FACE_BOUND ( 'NONE', #30560, .T. ) ;
#155503 =( BOUNDED_CURVE ( )  B_SPLINE_CURVE ( 2, ( #159453, #160522, #25181, #24795, #171053, #203529, #121329 ),
 .UNSPECIFIED., .F., .T. ) 
 B_SPLINE_CURVE_WITH_KNOTS ( ( 3, 2, 2, 3 ),
 ( 0.4499999999999995115, 0.4583333333333330373, 0.4666666666666666741, 0.4750000000000001998 ),
 .UNSPECIFIED. ) 
 CURVE ( )  GEOMETRIC_REPRESENTATION_ITEM ( )  RATIONAL_B_SPLINE_CURVE ( ( 1.000000000000007994, 0.8660254037844307140, 1.000000000000000000, 0.8660254037844387076, 1.000000000000000000, 0.8660254037844351549, 1.000000000000003553 ) ) 
 REPRESENTATION_ITEM ( '' )  );
#155504 = CARTESIAN_POINT ( 'NONE',  ( -9.499685679921610060, -9.917013740047297077, 0.07729799388535862903 ) ) ;
#155505 = CARTESIAN_POINT ( 'NONE',  ( 10.99665086521320845, -7.860092950639685938, -0.2746580110251511386 ) ) ;
#155506 = CARTESIAN_POINT ( 'NONE',  ( 0.7509353727821498348, 0.6442623716619542140, 2.110749664216593047 ) ) ;
#155507 = CARTESIAN_POINT ( 'NONE',  ( 3.515140014801207524, 2.043520737213794458, 0.9711500472536734874 ) ) ;
#155508 = CARTESIAN_POINT ( 'NONE',  ( -7.199016379176422120, 11.34267684244042584, 0.000000000000000000 ) ) ;
#155510 = EDGE_CURVE ( 'NONE', #60775, #128332, #9862, .T. ) ;
#155509 = CARTESIAN_POINT ( 'NONE',  ( 3.533306822026711647, -0.1277962806783480842, 1.807111865170844656 ) ) ;
#155511 = CARTESIAN_POINT ( 'NONE',  ( 3.749167220118687638, 0.2288279286139145163, -1.901904479094515210 ) ) ;
#155512 = CARTESIAN_POINT ( 'NONE',  ( 5.301260566756325510, -1.777534899005998481, 1.061244097098137606 ) ) ;
#155513 = CARTESIAN_POINT ( 'NONE',  ( 1.364683531249988535, 3.676041667008087099, 0.7879004041258500513 ) ) ;
#155514 = CARTESIAN_POINT ( 'NONE',  ( 2.799638878761875116, -0.6198165829789729075, 1.871555056500016745 ) ) ;
#155515 = CARTESIAN_POINT ( 'NONE',  ( 0.8856179577424825311, 1.291390466942985649, 1.429610664621896898 ) ) ;
#155516 = CARTESIAN_POINT ( 'NONE',  ( 3.819104250046548632, -0.1383300533824398659, 1.865606469731183825 ) ) ;
#155517 =( GEOMETRIC_REPRESENTATION_CONTEXT ( 3 ) GLOBAL_UNCERTAINTY_ASSIGNED_CONTEXT ( ( #29965 ) ) GLOBAL_UNIT_ASSIGNED_CONTEXT ( ( #78184, #160508, #133371 ) ) REPRESENTATION_CONTEXT ( 'NONE', 'WORKASPACE' ) );
#155518 = CARTESIAN_POINT ( 'NONE',  ( 3.475486094516122115, 0.05728489528775136674, -2.307140494302026390 ) ) ;
#155519 = CARTESIAN_POINT ( 'NONE',  ( 3.894834723524211118, 0.2711828204805393772, 1.841042229387960472 ) ) ;
#155520 = CARTESIAN_POINT ( 'NONE',  ( -1.201851678989727383E-14, 4.196875000341417028, -1.575800808251660134 ) ) ;
#155521 = CARTESIAN_POINT ( 'NONE',  ( -5.220052836461385404, 6.048815383081766583, -1.199719254218446718 ) ) ;
#155522 = CARTESIAN_POINT ( 'NONE',  ( 6.582647274634798151, 7.638508894284114170, 1.199719254218462483 ) ) ;
#155523 = CARTESIAN_POINT ( 'NONE',  ( 6.773846765307987461, -7.473374494058229622, 6.773846765307971474 ) ) ;
#155524 = CARTESIAN_POINT ( 'NONE',  ( 0.9792911203426227784, -0.05348914117170092131, -2.105562491362684252 ) ) ;
#155525 = ADVANCED_FACE ( 'NONE', ( #83407 ), #158244, .T. ) ;
#155526 = CARTESIAN_POINT ( 'NONE',  ( 4.487385655998888723, 4.337630808194552934, 0.7216878364870317197 ) ) ;
#155528 = CARTESIAN_POINT ( 'NONE',  ( 1.499999999999996891, 8.895833333333339255, -0.8660254037844378194 ) ) ;
#155527 = CARTESIAN_POINT ( 'NONE',  ( -1.364683531250010295, 5.801041667008088432, -0.7879004041258300672 ) ) ;
#155529 = CARTESIAN_POINT ( 'NONE',  ( -1.850900803405209905, 8.952907405788534945, -0.7749999999999996891 ) ) ;
#155530 = CARTESIAN_POINT ( 'NONE',  ( 1.758217466200185042, 0.8068918862002281145, -1.961288232260410380 ) ) ;
#155531 = CARTESIAN_POINT ( 'NONE',  ( 2.989549312115233004, 6.434947971831853408, -0.5153606499832382726 ) ) ;
#155532 = CARTESIAN_POINT ( 'NONE',  ( 1.002220075199202309, -0.9041908160717628817, 1.806139134770538002 ) ) ;
#155533 = CARTESIAN_POINT ( 'NONE',  ( -1.402160292154681736E-14, 0.3218750003414227456, 1.575800808251672791 ) ) ;
#155534 = CARTESIAN_POINT ( 'NONE',  ( -2.819732761962335577, 5.273143408055916304, -1.082531754730543971 ) ) ;
#155535 = EDGE_CURVE ( 'NONE', #70481, #176125, #89756, .T. ) ;
#155536 = CARTESIAN_POINT ( 'NONE',  ( 5.660692828905515839, 6.562895374266609849, -1.199719254218445830 ) ) ;
#155537 = ORIENTED_EDGE ( 'NONE', *, *, #48694, .T. ) ;
#155538 = CARTESIAN_POINT ( 'NONE',  ( 0.6499751493908960676, 0.6786997614584532323, -2.052318101833712660 ) ) ;
#155539 = CARTESIAN_POINT ( 'NONE',  ( 6.610000000000006537, 2.052567036419289614, 2.306714106643445561 ) ) ;
#155542 = CARTESIAN_POINT ( 'NONE',  ( 2.562127843302666186, 5.932973550587659517, 0.000000000000000000 ) ) ;
#155541 = CARTESIAN_POINT ( 'NONE',  ( 6.825078400183573812, 0.002648415797040087893, 1.855566311045192540 ) ) ;
#155540 = CARTESIAN_POINT ( 'NONE',  ( 5.896870467300973750, 5.844380064798101237, 0.7998128361456352531 ) ) ;
#155543 = CARTESIAN_POINT ( 'NONE',  ( -3.156015896931072540, 6.904045323053366268, 0.000000000000000000 ) ) ;
#155544 = CARTESIAN_POINT ( 'NONE',  ( 5.419157771004846857, -1.820987890746316173, 0.8666037247077316152 ) ) ;
#155545 = CARTESIAN_POINT ( 'NONE',  ( -9.164948653158003111, 9.794787638213568570, -0.7216878364870267237 ) ) ;
#155546 = CARTESIAN_POINT ( 'NONE',  ( -0.005964567173097347699, -2.191213315851054944, -0.04726126812268362232 ) ) ;
#155547 = FACE_OUTER_BOUND ( 'NONE', #47985, .T. ) ;
#155549 = CARTESIAN_POINT ( 'NONE',  ( -0.6823417656250039265, 10.56770833367473550, -1.181850606188755259 ) ) ;
#155548 = CARTESIAN_POINT ( 'NONE',  ( 0.8137758769373629741, -0.3292158159766758185, 2.238336236828967429 ) ) ;
#155550 = CARTESIAN_POINT ( 'NONE',  ( -8.435144125996554720, 12.99275191363802229, 0.7998128361456341429 ) ) ;
#155552 = CARTESIAN_POINT ( 'NONE',  ( 1.018978518071847583, -1.731272710380473923, 0.8202338080745846804 ) ) ;
#155551 = CARTESIAN_POINT ( 'NONE',  ( -4.378920427089552092, 8.052564898339037214, 0.7216878364870317197 ) ) ;
#155553 = CARTESIAN_POINT ( 'NONE',  ( -1.402160292154681736E-14, 0.1343750003414218575, 1.575800808251672791 ) ) ;
#155554 = CARTESIAN_POINT ( 'NONE',  ( 0.3282377607281101173, 2.738835450998162280, -1.225000000000008527 ) ) ;
#155555 = CARTESIAN_POINT ( 'NONE',  ( 1.499999999999993117, 10.10416666666667140, 0.8660254037844409281 ) ) ;
#155556 = CARTESIAN_POINT ( 'NONE',  ( 2.420142186669431705, 1.127438667474765621, -1.305497878543178336 ) ) ;
#155557 = CARTESIAN_POINT ( 'NONE',  ( 5.499767588998890844, 6.445425604367387429, 1.199719254218451159 ) ) ;
#155558 = CARTESIAN_POINT ( 'NONE',  ( 1.668863397688532091, 0.1364744985549205814, -1.764554890378322805 ) ) ;
#155559 = CARTESIAN_POINT ( 'NONE',  ( 1.858066033337543832, 0.7684160352657551929, -1.860855044080988785 ) ) ;
#155560 = CARTESIAN_POINT ( 'NONE',  ( 4.454274341225270994, 2.206355006892012138, -0.05062909709598743119 ) ) ;
#155561 = VERTEX_POINT ( 'NONE', #80419 ) ;
#155562 = CARTESIAN_POINT ( 'NONE',  ( 3.990493710177836828, -1.159536886187025440, 1.653596977174769833 ) ) ;
#155563 = CARTESIAN_POINT ( 'NONE',  ( -5.725286006720766707, 9.901527117808042178, 0.7998128361456291469 ) ) ;
#155565 = CARTESIAN_POINT ( 'NONE',  ( 3.620720401301917857, 0.2986476686686300175, 1.994069442355271615 ) ) ;
#155564 = CARTESIAN_POINT ( 'NONE',  ( 4.108145954595856075, -0.8103754143699601897, 1.959725966023172727 ) ) ;
#155567 = ORIENTED_EDGE ( 'NONE', *, *, #151365, .F. ) ;
#155566 = CARTESIAN_POINT ( 'NONE',  ( 3.972783152890049241, -1.338232477621086547, 1.221218810135711541 ) ) ;
#155568 = CARTESIAN_POINT ( 'NONE',  ( 5.737035277238070385, 6.722237907313067140, -1.199719254218452047 ) ) ;
#155569 = ORIENTED_EDGE ( 'NONE', *, *, #15404, .T. ) ;
#155570 = CARTESIAN_POINT ( 'NONE',  ( 1.586564105604048480, -0.2713065988851799393, -1.850747533123621391 ) ) ;
#155571 = CARTESIAN_POINT ( 'NONE',  ( -11.94105721237523099, 10.90000000000000036, -1.187919463087249827 ) ) ;
#155572 = CARTESIAN_POINT ( 'NONE',  ( -5.000000000000013323, 11.39843543023555661, -0.7749999999999996891 ) ) ;
#155573 = CARTESIAN_POINT ( 'NONE',  ( -10.19200560444942560, 4.477620260464512114, -5.707107691925500603 ) ) ;
#155574 =( NAMED_UNIT ( * ) SI_UNIT ( $, .STERADIAN. ) SOLID_ANGLE_UNIT ( ) );
#155575 = CARTESIAN_POINT ( 'NONE',  ( -0.6823417656250003738, 3.030208333674754062, -1.181850606188749264 ) ) ;
#155576 = CARTESIAN_POINT ( 'NONE',  ( 11.84668730067608600, 10.89999999999998259, 1.399999999999998579 ) ) ;
#155577 = EDGE_LOOP ( 'NONE', ( #39939, #32672, #156641, #200341 ) ) ;
#155578 = CARTESIAN_POINT ( 'NONE',  ( 6.861835142292143530, 8.138467433163244280, 1.082531754730549967 ) ) ;
#155579 = CARTESIAN_POINT ( 'NONE',  ( -5.004368097219957789, 5.011053332944274352, 0.000000000000000000 ) ) ;
#155580 = CARTESIAN_POINT ( 'NONE',  ( -5.261446130555064826, 8.296048364692991228, 1.199719254218452935 ) ) ;
#155581 = CARTESIAN_POINT ( 'NONE',  ( 4.605793411009856619, 1.573235607984494688, 1.422142093439874522 ) ) ;
#155582 = CARTESIAN_POINT ( 'NONE',  ( -10.05278092738192619, 5.876216011288541985, -5.831672646394378212 ) ) ;
#155583 = CARTESIAN_POINT ( 'NONE',  ( 5.237557467868056094, -1.392094792763297617, -1.396070155715684269 ) ) ;
#155584 = CARTESIAN_POINT ( 'NONE',  ( -1.402160292154681736E-14, 1.696875000341421469, -1.575800808251659024 ) ) ;
#155585 = CARTESIAN_POINT ( 'NONE',  ( 0.8615886222705991804, -1.589730513765170938, -1.235154978249096036 ) ) ;
#155586 = VERTEX_POINT ( 'NONE', #212536 ) ;
#155587 = CARTESIAN_POINT ( 'NONE',  ( 6.262923198102183342, -0.1061305018058098515, -2.114825283700927372 ) ) ;
#155588 = CARTESIAN_POINT ( 'NONE',  ( -0.3892891889261625438, 6.983571277091629170, -3.944761702788770474 ) ) ;
#155589 = CARTESIAN_POINT ( 'NONE',  ( 2.084514231050747401, 1.193861083872927109, -1.691280048542340708 ) ) ;
#155590 = CARTESIAN_POINT ( 'NONE',  ( 4.583538449871731757, 7.505156070562471804, 1.199719254218451159 ) ) ;
#155591 = CARTESIAN_POINT ( 'NONE',  ( 4.538947565524982686, 8.517465603079630299, 0.000000000000000000 ) ) ;
#155593 = CARTESIAN_POINT ( 'NONE',  ( 5.355634372598031767, 6.206993841907870291, -1.199719254218445830 ) ) ;
#155592 = CARTESIAN_POINT ( 'NONE',  ( 3.152369405254138446, -1.582674238129866184, 1.366072548952133259 ) ) ;
#155594 = CARTESIAN_POINT ( 'NONE',  ( 5.352436782344940802, 9.466536356036257871, 0.000000000000000000 ) ) ;
#155597 = ORIENTED_EDGE ( 'NONE', *, *, #98379, .F. ) ;
#155596 = CARTESIAN_POINT ( 'NONE',  ( 1.928074960669722504, -0.8543848903827315766, -1.597334059258429972 ) ) ;
#155595 = CARTESIAN_POINT ( 'NONE',  ( 2.625780896952558674, -1.049238153381076177, -1.493741879923994542 ) ) ;
#155598 = CARTESIAN_POINT ( 'NONE',  ( 5.760442859251142522, 0.8911043219209063837, 2.019162844794204048 ) ) ;
#155599 = DIRECTION ( 'NONE',  ( 0.000000000000000000, -1.000000000000000000, 0.000000000000000000 ) ) ;
#155600 = CARTESIAN_POINT ( 'NONE',  ( 4.630015379333586978, -1.354682855507854278, -1.741961856448564161 ) ) ;
#155601 = CARTESIAN_POINT ( 'NONE',  ( 7.202405917357655341, 9.425892875049191488, 1.599625672291281386 ) ) ;
#155602 = DIRECTION ( 'NONE',  ( -0.000000000000000000, -1.000000000000000000, -0.000000000000000000 ) ) ;
#155603 = CARTESIAN_POINT ( 'NONE',  ( 3.281800106729782840, 1.865104756965057620, -0.4213900744019505318 ) ) ;
#155604 =( GEOMETRIC_REPRESENTATION_CONTEXT ( 3 ) GLOBAL_UNCERTAINTY_ASSIGNED_CONTEXT ( ( #182605 ) ) GLOBAL_UNIT_ASSIGNED_CONTEXT ( ( #147972, #131752, #17923 ) ) REPRESENTATION_CONTEXT ( 'NONE', 'WORKASPACE' ) );
#155605 = CARTESIAN_POINT ( 'NONE',  ( 7.096803341749390981, 10.36702210109460154, -1.199719254218441611 ) ) ;
#155606 = CARTESIAN_POINT ( 'NONE',  ( 6.566853775770633561, 1.536883091774071453, -1.387433097640700774 ) ) ;
#155607 = CARTESIAN_POINT ( 'NONE',  ( -9.367496997608871112, 15.42330868759649043, 7.413898975919298806 ) ) ;
#155608 = CARTESIAN_POINT ( 'NONE',  ( 5.689076433642084041, 1.658752129386225516, 1.432425853890168188 ) ) ;
#155609 = CARTESIAN_POINT ( 'NONE',  ( 5.595231165798738360, 7.497995327707586810, -1.335214257040851615 ) ) ;
#155610 = ORIENTED_EDGE ( 'NONE', *, *, #170196, .F. ) ;
#155611 = ORIENTED_EDGE ( 'NONE', *, *, #118886, .F. ) ;
#155612 = FACE_OUTER_BOUND ( 'NONE', #201662, .T. ) ;
#155613 = CARTESIAN_POINT ( 'NONE',  ( 5.896870467300973750, 5.844380064798101237, 0.7998128361456352531 ) ) ;
#155614 = CARTESIAN_POINT ( 'NONE',  ( 3.285556943749998737, -1.392708332855375764, -1.896917185911906722 ) ) ;
#155615 = SURFACE_SIDE_STYLE ('',( #40813 ) ) ;
#155616 = CARTESIAN_POINT ( 'NONE',  ( -6.873620692448438874, 10.96304854125777695, 0.000000000000000000 ) ) ;
#155617 = CARTESIAN_POINT ( 'NONE',  ( 5.761288931164342486, 5.686201605971993978, -0.7998128361456481317 ) ) ;
#155618 = CARTESIAN_POINT ( 'NONE',  ( 5.330949937734919430, -1.947458545883517189, -0.7027056652011903770 ) ) ;
#155619 = CARTESIAN_POINT ( 'NONE',  ( 3.967344596728016093, 0.2348649212099394590, -1.912067515532820838 ) ) ;
#155620 = CARTESIAN_POINT ( 'NONE',  ( 1.388296234047466049, -0.7283980888908546669, -1.880428666220852696 ) ) ;
#155621 = CARTESIAN_POINT ( 'NONE',  ( -9.820183334999905256, 10.35130206712171130, 1.040834085586084257E-14 ) ) ;
#155622 = CARTESIAN_POINT ( 'NONE',  ( 6.047819040147648373, 9.213483425884394507, 1.199719254218452047 ) ) ;
#155623 = DIRECTION ( 'NONE',  ( 0.000000000000000000, -1.000000000000000000, 0.000000000000000000 ) ) ;
#155624 = CARTESIAN_POINT ( 'NONE',  ( 1.025618320672251560, -1.392776288830662512, -1.691927514038966907 ) ) ;
#155625 = CARTESIAN_POINT ( 'NONE',  ( 5.303274670167754223, 1.494737065598228165, 1.048009559513597866 ) ) ;
#155626 = CARTESIAN_POINT ( 'NONE',  ( 6.211043768836181478, 7.379210830797944709, 1.082531754730549967 ) ) ;
#155627 = CARTESIAN_POINT ( 'NONE',  ( 9.317477881089539338, 11.89347683273640932, 1.599625672291279388 ) ) ;
#155628 = CARTESIAN_POINT ( 'NONE',  ( -6.493429226302317225, 6.540365283632955773, 0.7998128361456341429 ) ) ;
#155629 = CARTESIAN_POINT ( 'NONE',  ( 3.506755287428983792, 7.242964935309132990, 1.040834085586084257E-14 ) ) ;
#155630 = CARTESIAN_POINT ( 'NONE',  ( 7.865138509703455405, 8.348618814175074121, -0.7216878364870317197 ) ) ;
#155631 = EDGE_LOOP ( 'NONE', ( #19692, #172372, #150681, #144464 ) ) ;
#155633 = CARTESIAN_POINT ( 'NONE',  ( 0.08268127059449237315, -1.313209137626596634, 1.525886470183013044 ) ) ;
#155632 = CARTESIAN_POINT ( 'NONE',  ( 2.401689157922583640, -0.7064633820979376866, -1.700523668893457296 ) ) ;
#155634 = CARTESIAN_POINT ( 'NONE',  ( 2.267358445155386981, -2.297842707097216053, 0.05573287391750710029 ) ) ;
#155635 = CARTESIAN_POINT ( 'NONE',  ( 6.789906393989944888, -1.279003670332454989, -1.487618534420580119 ) ) ;
#155636 = CARTESIAN_POINT ( 'NONE',  ( -4.706651882238427120, 8.642844295920152575, 1.040834085586084257E-14 ) ) ;
#155637 = DIRECTION ( 'NONE',  ( -0.9992060137953822085, 8.739303527495176105E-16, -0.03984146075563037293 ) ) ;
#155638 = CARTESIAN_POINT ( 'NONE',  ( 3.058751851047710080, 0.4689117840017149041, 1.853869267190631831 ) ) ;
#155639 = CARTESIAN_POINT ( 'NONE',  ( -10.13488352141530768, 11.78278451552804817, 1.199719254218462483 ) ) ;
#155640 = CARTESIAN_POINT ( 'NONE',  ( 0.9771079587245214970, 1.912259438035465386, 0.7939916666956441382 ) ) ;
#155641 = CARTESIAN_POINT ( 'NONE',  ( -4.659162064951642535, 5.464719159645540003, 1.199719254218452935 ) ) ;
#155643 = CARTESIAN_POINT ( 'NONE',  ( 1.024039198018782626, 1.117340804906666873, -1.500143343703803422 ) ) ;
#155642 = CARTESIAN_POINT ( 'NONE',  ( 2.085595224044423102, -0.8910886986466991511, 1.891471387866516585 ) ) ;
#155644 = CARTESIAN_POINT ( 'NONE',  ( 1.932970024460831882, 1.034005469613193062, 1.730602090182407959 ) ) ;
#155645 = CARTESIAN_POINT ( 'NONE',  ( 7.944714827928039291, 11.25228915168265864, 1.082531754730557072 ) ) ;
#155646 = ORIENTED_EDGE ( 'NONE', *, *, #113441, .F. ) ;
#155647 = CARTESIAN_POINT ( 'NONE',  ( -1.364683531249997417, 4.321875000341417028, 1.214306433183764966E-14 ) ) ;
#155648 = CARTESIAN_POINT ( 'NONE',  ( 2.243362625160577384, 1.740107689937436808, 0.04144568419049177860 ) ) ;
#155649 = TOROIDAL_SURFACE ( 'NONE', #210967, 7.374593666277937665, 0.08000000000000000167 ) ;
#155650 = CARTESIAN_POINT ( 'NONE',  ( 4.123651276850781144, 7.962676922967908411, -0.7998128361456221525 ) ) ;
#155652 = CARTESIAN_POINT ( 'NONE',  ( 0.1054570145121071778, 2.614151819895196294, -2.076146791065092145 ) ) ;
#155651 = CARTESIAN_POINT ( 'NONE',  ( -6.922231005658575853, -8.202869699938529990, 6.506745451169506644 ) ) ;
#155653 = CARTESIAN_POINT ( 'NONE',  ( 2.771755371404661439, 0.9226176164769549493, 1.457180633135872094 ) ) ;
#155654 = CARTESIAN_POINT ( 'NONE',  ( 2.718528139169604341, 2.064530135181973591, 0.7356957861901700646 ) ) ;
#155655 = CARTESIAN_POINT ( 'NONE',  ( 5.180388087185870738, -1.228261608319089149, 1.833297759731546073 ) ) ;
#155656 = CARTESIAN_POINT ( 'NONE',  ( -11.25372107582773396, 4.972923339538419363, -5.839092030517418763 ) ) ;
#155657 = CARTESIAN_POINT ( 'NONE',  ( 2.079201016916156330, 2.024566655493876155, 0.7844037353602287821 ) ) ;
#155658 = CARTESIAN_POINT ( 'NONE',  ( 2.103868193876055503, -1.825329726703457833, 0.04394198290156441783 ) ) ;
#155659 = DIRECTION ( 'NONE',  ( -1.000000000000000000, -0.000000000000000000, -0.000000000000000000 ) ) ;
#155660 = CARTESIAN_POINT ( 'NONE',  ( 5.050072346573388771, 1.046394516673061270, 1.840669678815173960 ) ) ;
#155661 = CARTESIAN_POINT ( 'NONE',  ( 6.639320575229294086, 0.5800432152290584398, 2.049144803211971233 ) ) ;
#155662 = VERTEX_POINT ( 'NONE', #116175 ) ;
#155664 = CARTESIAN_POINT ( 'NONE',  ( -1.201851678989727383E-14, 0.8843750003414173610, 1.575800808251672791 ) ) ;
#155663 = CARTESIAN_POINT ( 'NONE',  ( 5.337530604160453329, 0.9314408107504292822, -2.094771667654048208 ) ) ;
#155665 = DIRECTION ( 'NONE',  ( 0.6507913734559654939, -0.7592566023652992380, 0.000000000000000000 ) ) ;
#155666 = CARTESIAN_POINT ( 'NONE',  ( 9.541187415715040032, 12.15447128979948310, -1.599625672291262513 ) ) ;
#155667 = CARTESIAN_POINT ( 'NONE',  ( 0.4520119014386895229, -1.502510013782244025, -1.496567369470555020 ) ) ;
#155668 = CARTESIAN_POINT ( 'NONE',  ( -6.724481002698138532, 6.947575379343695623, -0.7216878364870278340 ) ) ;
#155670 = EDGE_CURVE ( 'NONE', #138555, #140464, #213584, .T. ) ;
#155669 = AXIS2_PLACEMENT_3D ( 'NONE', #74185, #91519, #24331 ) ;
#155671 = CARTESIAN_POINT ( 'NONE',  ( 3.497640442645619796, 6.064035702186436616, -1.082531754730543083 ) ) ;
#155672 = CARTESIAN_POINT ( 'NONE',  ( -5.043269954159181445, 8.827639346586952485, 1.214306433183764966E-14 ) ) ;
#155673 = CARTESIAN_POINT ( 'NONE',  ( 4.584065335196271462, 5.481069324884694005, 1.082531754730549078 ) ) ;
#155674 = ORIENTED_EDGE ( 'NONE', *, *, #43285, .F. ) ;
#155675 = CARTESIAN_POINT ( 'NONE',  ( 5.485000066852382616, -2.016597020608828839, 0.002808655738886777897 ) ) ;
#155677 = CARTESIAN_POINT ( 'NONE',  ( 2.993094585481168579, 0.2480512885563341541, 2.047511573040517341 ) ) ;
#155676 = CARTESIAN_POINT ( 'NONE',  ( 6.094553744542824170, 7.069066442510145265, 1.199719254218462483 ) ) ;
#155679 = CARTESIAN_POINT ( 'NONE',  ( -0.1408020194049965368, 5.721120576699901150, -2.694324532632543345 ) ) ;
#155678 = CARTESIAN_POINT ( 'NONE',  ( 5.643937085038755797, 9.806620042512378177, -0.7998128361456481317 ) ) ;
#155680 = CARTESIAN_POINT ( 'NONE',  ( 6.003228155800906407, 10.22579295840155744, 0.000000000000000000 ) ) ;
#155681 = CARTESIAN_POINT ( 'NONE',  ( 1.642778471875001811, -2.442708332855377140, 2.845375778867859751 ) ) ;
#155682 = DIRECTION ( 'NONE',  ( -8.638326563840814399E-31, 0.000000000000000000, -1.000000000000000000 ) ) ;
#155683 = CARTESIAN_POINT ( 'NONE',  ( 5.982419568921026887, -0.3181065885738461607, -2.168126298386578110 ) ) ;
#155684 = CARTESIAN_POINT ( 'NONE',  ( 3.973279856364997809, -1.994869694282218386, -0.2930714778977619450 ) ) ;
#155685 = CARTESIAN_POINT ( 'NONE',  ( 3.438839575862782549, -1.396446551253815782, -1.200180114512699792 ) ) ;
#155686 = CARTESIAN_POINT ( 'NONE',  ( 4.482942347612929979, 8.381849838857084123, 1.040834085586084257E-14 ) ) ;
#155687 = CARTESIAN_POINT ( 'NONE',  ( 6.405291383686446238, 1.519602032305459538, 1.011395407323860907 ) ) ;
#155688 =( BOUNDED_SURFACE ( )  B_SPLINE_SURFACE ( 3, 2, ( 
 ( #138837, #104196, #171311 ),
 ( #89022, #6663, #73818 ),
 ( #79144, #14119, #93297 ),
 ( #13065, #43478, #193957 ) ),
 .UNSPECIFIED., .F., .F., .T. ) 
 B_SPLINE_SURFACE_WITH_KNOTS ( ( 4, 4 ),
 ( 3, 3 ),
 ( 0.000000000000000000, 9.170893477967426329E-05 ),
 ( 0.000000000000000000, 1.000000000000000000 ),
 .UNSPECIFIED. ) 
 GEOMETRIC_REPRESENTATION_ITEM ( )  RATIONAL_B_SPLINE_SURFACE ( (
 ( 1.000000000000000000, 0.6787756258918241636, 1.000000000000000000),
 ( 1.000000000000000000, 0.6894756946173401513, 1.000000000000000000),
 ( 1.000000000000000000, 0.6998898451713442270, 1.000000000000000000),
 ( 1.000000000000000000, 0.7100530722072168066, 1.000000000000000000) ) ) 
 REPRESENTATION_ITEM ( '' )  SURFACE ( )  );
#155689 = CARTESIAN_POINT ( 'NONE',  ( -6.470265622219711688, 8.571729197388226140, -1.599625672291263179 ) ) ;
#155690 = CARTESIAN_POINT ( 'NONE',  ( 6.754744673581316583, -1.754229693457433736, 1.428470910521584036 ) ) ;
#155691 = CARTESIAN_POINT ( 'NONE',  ( 2.367922061077184726, 2.065251240347278472, -0.4117205849265455075 ) ) ;
#155692 = CARTESIAN_POINT ( 'NONE',  ( -5.529746549527323474, 7.544733289238903851, -1.599625672291271394 ) ) ;
#155693 =( REPRESENTATION_RELATIONSHIP ('NONE','NONE', #84563, #121983 ) REPRESENTATION_RELATIONSHIP_WITH_TRANSFORMATION ( #38482 )SHAPE_REPRESENTATION_RELATIONSHIP( ) );
#155694 = CARTESIAN_POINT ( 'NONE',  ( 7.962716289927667113, 8.184257181204083409, -0.7998128361456291469 ) ) ;
#155695 = CARTESIAN_POINT ( 'NONE',  ( 7.010974831598141499, 7.352094523052197239, -0.7216878364870317197 ) ) ;
#155696 = CARTESIAN_POINT ( 'NONE',  ( -5.554036483092550824, 9.631459663583308739, -0.7998128361456231517 ) ) ;
#155697 = EDGE_CURVE ( 'NONE', #99612, #98321, #46878, .T. ) ;
#155698 = CARTESIAN_POINT ( 'NONE',  ( 5.273758565591489145, 9.096542726591325234, -0.7216878364870267237 ) ) ;
#155699 = CARTESIAN_POINT ( 'NONE',  ( 4.595133766160131472, 7.156059413716462814, 1.333087067838649720 ) ) ;
#155700 = CARTESIAN_POINT ( 'NONE',  ( -5.545448523189368650, 6.428443684264421698, -1.199719254218446718 ) ) ;
#155702 = CARTESIAN_POINT ( 'NONE',  ( 3.885193193976806292, -2.073655658835142024, -0.7971110592776513570 ) ) ;
#155701 = CARTESIAN_POINT ( 'NONE',  ( 2.267978396857213585, 0.5610993688725562922, -2.044979925899123252 ) ) ;
#155703 = CARTESIAN_POINT ( 'NONE',  ( 2.115410589380119610, -2.125216164159982046, 0.5342070311455533460 ) ) ;
#155704 = CARTESIAN_POINT ( 'NONE',  ( -4.876128802409253282, 8.840567369452784874, 0.7998128361456481317 ) ) ;
#155705 = CARTESIAN_POINT ( 'NONE',  ( 6.883263157960391787, -0.001104538646235289417, 1.946037152736757925 ) ) ;
#155706 = CARTESIAN_POINT ( 'NONE',  ( -5.798046968499580345, 6.793418213784815585, 1.199719254218452935 ) ) ;
#155707 = CARTESIAN_POINT ( 'NONE',  ( 5.723093114104088386, -1.772945450647535948, -0.8403097561825512152 ) ) ;
#155708 = CARTESIAN_POINT ( 'NONE',  ( -1.237941840313982578, 1.374772708486763806, 1.500000000000001332 ) ) ;
#155709 = CARTESIAN_POINT ( 'NONE',  ( -1.364683531250012516, 2.238541667008087988, -0.7879004041258289570 ) ) ;
#155710 = CARTESIAN_POINT ( 'NONE',  ( 6.610000000000030518, 1.266345627986571021, 2.115470293623383569 ) ) ;
#155711 = CARTESIAN_POINT ( 'NONE',  ( -6.236387472606153892, 8.298871356172400127, -1.443375672974059665 ) ) ;
#155712 = CARTESIAN_POINT ( 'NONE',  ( 3.621431001533811589, 1.820626359085864454, 1.087046460333654485 ) ) ;
#155713 = CARTESIAN_POINT ( 'NONE',  ( -3.363304624641834106, 6.081549941127532222, -1.199719254218452047 ) ) ;
#155714 = CARTESIAN_POINT ( 'NONE',  ( 5.664953204072169513, -1.952404353424816774, -0.9282482345986733385 ) ) ;
#155715 = CARTESIAN_POINT ( 'NONE',  ( 6.144869935491714230, 8.192100896205568361, -1.599625672291262513 ) ) ;
#155716 = CARTESIAN_POINT ( 'NONE',  ( 5.565905774130330386, -1.163279849954502287, 1.427249551226833502 ) ) ;
#155717 = CARTESIAN_POINT ( 'NONE',  ( -5.877243123607416742, 6.020912620514094371, 0.3151507616369741416 ) ) ;
#155718 = CARTESIAN_POINT ( 'NONE',  ( -1.364683531250012516, 1.592708333674756727, 0.7879004041258379498 ) ) ;
#155719 = CARTESIAN_POINT ( 'NONE',  ( 0.04591871184063747030, -1.399829139283098822, 1.033961902999945170 ) ) ;
#155720 = CARTESIAN_POINT ( 'NONE',  ( 6.827182134110227452, 2.468179810210658687, 2.195371296381436022 ) ) ;
#155721 = CARTESIAN_POINT ( 'NONE',  ( 3.307826292054301121, 4.882216645528547616, -1.443375672974057666 ) ) ;
#155722 = CARTESIAN_POINT ( 'NONE',  ( 0.4019237886466778820, 11.82366454968463110, 1.500000000000001554 ) ) ;
#155723 = AXIS2_PLACEMENT_3D ( 'NONE', #30703, #127211, #94645 ) ;
#155724 = CARTESIAN_POINT ( 'NONE',  ( 4.311504812833309330, -0.3723461477018601973, 2.129241309423899775 ) ) ;
#155725 = CARTESIAN_POINT ( 'NONE',  ( -5.447678794592645701, 5.250046769979851646, 0.000000000000000000 ) ) ;
#155726 = CARTESIAN_POINT ( 'NONE',  ( 0.3504316985127345907, -0.8248687954017698276, 1.525068808560197109 ) ) ;
#155727 = CARTESIAN_POINT ( 'NONE',  ( -7.605760987142072160, 10.85684300409898384, 1.082531754730549967 ) ) ;
#155728 = CARTESIAN_POINT ( 'NONE',  ( 3.731458613173586514, -1.998165266068991253, 0.8252760040215676440 ) ) ;
#155729 = CARTESIAN_POINT ( 'NONE',  ( 4.815676612163926507, -1.933897303736350270, 0.3816649536505806184 ) ) ;
#155730 = CARTESIAN_POINT ( 'NONE',  ( 3.743219424636199832, -1.670416500854546626, -0.4642454339297346078 ) ) ;
#155731 = CARTESIAN_POINT ( 'NONE',  ( 1.365048776756357940, 0.1565470504056795942, -2.186014887712848243 ) ) ;
#155732 = CARTESIAN_POINT ( 'NONE',  ( 1.396046310939329738, 1.748920304266964543, 1.505474166573782968 ) ) ;
#155733 = CARTESIAN_POINT ( 'NONE',  ( 3.198563317047153465, -0.5950029230564283234, -1.973035911149529698 ) ) ;
#155734 = CARTESIAN_POINT ( 'NONE',  ( 5.513211315966105808, -1.893842782867664054, 0.4293952855863486517 ) ) ;
#155735 = CARTESIAN_POINT ( 'NONE',  ( -8.500599125644013654, 9.019713189447241319, 0.7216878364870438212 ) ) ;
#155736 = CARTESIAN_POINT ( 'NONE',  ( -4.633854640820660009, 8.628190524257904670, -0.7998128361456362523 ) ) ;
#155737 = DIRECTION ( 'NONE',  ( 0.7592566023653005702, 0.6507913734559639396, 0.000000000000000000 ) ) ;
#155738 = ADVANCED_FACE ( 'NONE', ( #32730 ), #196307, .F. ) ;
#155740 = EDGE_LOOP ( 'NONE', ( #38271, #152723, #6188 ) ) ;
#155739 = CARTESIAN_POINT ( 'NONE',  ( -3.709037541790315640, 6.484905011134099340, -1.199719254218450271 ) ) ;
#155741 = CARTESIAN_POINT ( 'NONE',  ( -6.846504384776755714, 9.971043634672792422, -1.082531754730537088 ) ) ;
#155742 = CARTESIAN_POINT ( 'NONE',  ( 2.696532018272995490, -2.200798769047443759, -0.1632673417703081331 ) ) ;
#155743 = CARTESIAN_POINT ( 'NONE',  ( 3.285556943750000514, -3.551041666188707424, 1.896917185911906500 ) ) ;
#155744 = ORIENTED_EDGE ( 'NONE', *, *, #196345, .T. ) ;
#155745 = CARTESIAN_POINT ( 'NONE',  ( 1.076741303291447460, 1.716668495539741324, 0.7189669686299257068 ) ) ;
#155746 = CARTESIAN_POINT ( 'NONE',  ( -0.02900071798685177615, 6.946858727649162901, -2.768864135414349281 ) ) ;
#155747 = CARTESIAN_POINT ( 'NONE',  ( -1.500000000000011324, 5.660416667349481123, -0.8660254037844313801 ) ) ;
#155748 = CARTESIAN_POINT ( 'NONE',  ( 4.675513026854819287, 7.080785086760167601, -1.371149936167876282 ) ) ;
#155750 = CARTESIAN_POINT ( 'NONE',  ( -4.072997184480262156, 7.271224798513709509, -0.8443910950608760624 ) ) ;
#155749 = CARTESIAN_POINT ( 'NONE',  ( -1.500000000000001110, 5.160416667349487341, -0.8660254037844372643 ) ) ;
#155751 = CARTESIAN_POINT ( 'NONE',  ( 4.529832720297257254, 8.298905583739861314, 0.000000000000000000 ) ) ;
#155752 = ORIENTED_EDGE ( 'NONE', *, *, #17772, .T. ) ;
#155753 = CARTESIAN_POINT ( 'NONE',  ( 2.729428266803469061, -1.923432490405907247, 0.7405405203823824944 ) ) ;
#155754 = CARTESIAN_POINT ( 'NONE',  ( -1.360316468750002894, 0.4114583336747319464, 0.7853790794158961308 ) ) ;
#155755 = CARTESIAN_POINT ( 'NONE',  ( -5.520141099058386125, 9.591915048876776595, 0.000000000000000000 ) ) ;
#155756 = CARTESIAN_POINT ( 'NONE',  ( 11.04536101718726293, 13.40000000000000036, -1.100000000000002087 ) ) ;
#155757 = CARTESIAN_POINT ( 'NONE',  ( 11.94105721237523277, 10.90000000000000036, 1.187919463087245386 ) ) ;
#155758 = CARTESIAN_POINT ( 'NONE',  ( 5.007038802148489509, 4.735966778795008381, 0.7998128361456341429 ) ) ;
#155759 = CARTESIAN_POINT ( 'NONE',  ( 1.147419824990800752, -1.624031055642958243, -1.268641727334917313 ) ) ;
#155760 = EDGE_CURVE ( 'NONE', #24541, #85130, #16456, .T. ) ;
#155762 = CARTESIAN_POINT ( 'NONE',  ( 4.968220237687512864, -1.735557695065930606, -0.6152675618510683453 ) ) ;
#155761 = CARTESIAN_POINT ( 'NONE',  ( -4.318600669050610463, 4.999583595936801572, 2.420000000000000373 ) ) ;
#155763 = CARTESIAN_POINT ( 'NONE',  ( 7.806797523370503811, 8.002351953554066810, 1.040834085586084257E-14 ) ) ;
#155764 = CARTESIAN_POINT ( 'NONE',  ( -5.010620288702242853, 8.003418215864698482, -1.199719254218453823 ) ) ;
#155765 = CARTESIAN_POINT ( 'NONE',  ( 6.132223229334005765, 5.371873414694337434, 2.500000000000000444 ) ) ;
#155766 = CARTESIAN_POINT ( 'NONE',  ( 4.512475528931441104, -0.9420208833846724916, -1.995868093903986118 ) ) ;
#155767 = CARTESIAN_POINT ( 'NONE',  ( 6.749321564901560322, -1.811022791033944257, -1.355814775124731808 ) ) ;
#155768 = CARTESIAN_POINT ( 'NONE',  ( -6.900736999675794792, 7.153207375817628666, 1.040834085586084257E-14 ) ) ;
#155769 = CARTESIAN_POINT ( 'NONE',  ( -0.03509584499547176162, -1.534781374734139670, 1.140672443274578729 ) ) ;
#155770 = CARTESIAN_POINT ( 'NONE',  ( 1.288296401830712368, -0.7303101666344159471, -1.879802715551846859 ) ) ;
#155771 = LINE ( 'NONE', #124424, #126859 ) ;
#155772 = CARTESIAN_POINT ( 'NONE',  ( 1.652187889876779892, -0.3379717360396676806, -2.273286007567467237 ) ) ;
#155773 = CARTESIAN_POINT ( 'NONE',  ( -2.428612866367529932E-14, 2.999999999999999112, 2.500000000000000444 ) ) ;
#155774 = CARTESIAN_POINT ( 'NONE',  ( 6.604189988765333474, -0.8127675640051763573, 1.729262449380222444 ) ) ;
#155775 = CARTESIAN_POINT ( 'NONE',  ( -3.023105066167347310, 5.702484939155337607, 2.420000000000010587 ) ) ;
#155776 = CARTESIAN_POINT ( 'NONE',  ( 1.955717210371358483, 1.865846021326333926, -0.1348392221205765851 ) ) ;
#155777 = CARTESIAN_POINT ( 'NONE',  ( 2.589077643123653072, 1.706113014995232380, 1.074661422923957055 ) ) ;
#155779 = CARTESIAN_POINT ( 'NONE',  ( -5.865261586769421776, 6.278966368068457093, 0.6541898161073615992 ) ) ;
#155778 = CARTESIAN_POINT ( 'NONE',  ( -1.402160292154681736E-14, 0.6968750003414164729, -1.575800808251659024 ) ) ;
#155781 = CARTESIAN_POINT ( 'NONE',  ( 3.668672709498523865, -1.414518211590541252, 1.560516469030509334 ) ) ;
#155780 = CARTESIAN_POINT ( 'NONE',  ( -7.853197290813634268, 10.18514947741448573, 1.599625672291295375 ) ) ;
#155782 = EDGE_CURVE ( 'NONE', #60268, #89693, #53663, .T. ) ;
#155783 = CARTESIAN_POINT ( 'NONE',  ( 7.853197290813620945, 10.18514947741448573, 1.599625672291281386 ) ) ;
#155785 = CARTESIAN_POINT ( 'NONE',  ( -7.503547950159405566, 10.84155747757291266, 1.199719254218453823 ) ) ;
#155784 = CARTESIAN_POINT ( 'NONE',  ( 4.736594563127852098, 6.619389305106191834, -1.599625672291273171 ) ) ;
#155786 = CARTESIAN_POINT ( 'NONE',  ( 3.885024839820313325, -1.886105071096555230, -0.7231171000243222791 ) ) ;
#155787 = CARTESIAN_POINT ( 'NONE',  ( -0.6823417656249969321, 4.717708333674755394, -1.181850606188749264 ) ) ;
#155788 = ADVANCED_FACE ( 'NONE', ( #3946, #70013 ), #103625, .F. ) ;
#155789 = CARTESIAN_POINT ( 'NONE',  ( 6.865701141133224716, -0.4594653659172152071, 2.018469443450424894 ) ) ;
#155790 = CARTESIAN_POINT ( 'NONE',  ( 8.839552966430002101, 11.33589776563360019, -1.443375672974052559 ) ) ;
#155791 = CARTESIAN_POINT ( 'NONE',  ( 4.780646861661003832, -2.095393720161139228, -0.5303334973314683953 ) ) ;
#155792 = CARTESIAN_POINT ( 'NONE',  ( 5.515134625708930649, 9.656350506627580543, 0.000000000000000000 ) ) ;
#155793 = CARTESIAN_POINT ( 'NONE',  ( 0.6823417656249882723, -1.094791666325249713, 1.181850606188755259 ) ) ;
#155795 = CARTESIAN_POINT ( 'NONE',  ( -9.481348452320357723, -9.199999999999983302, 0.5950054837414385789 ) ) ;
#155794 = CARTESIAN_POINT ( 'NONE',  ( 7.178115983792402233, 7.339166500704784823, 0.7998128361456281477 ) ) ;
#155796 = CARTESIAN_POINT ( 'NONE',  ( 8.419250203962011625, 8.924806114151579095, -0.7216878364870267237 ) ) ;
#155798 = LINE ( 'NONE', #205590, #24462 ) ;
#155797 = CARTESIAN_POINT ( 'NONE',  ( 2.102231420249685456, 0.8322404413585123839, -2.005527090382641653 ) ) ;
#155800 = CARTESIAN_POINT ( 'NONE',  ( 1.645803748337611783, 0.5784278848013635344, 1.748079663633335334 ) ) ;
#155799 = CARTESIAN_POINT ( 'NONE',  ( -5.097502569058215194, 6.970172302033127210, -1.443375672974053447 ) ) ;
#155801 = B_SPLINE_CURVE_WITH_KNOTS ( 'NONE', 3,
 ( #196353, #147610, #33838, #199523, #35969, #102047, #17563 ),
 .UNSPECIFIED., .F., .F.,
 ( 4, 3, 4 ),
 ( 0.002201685690204605809, 0.002395020826490573771, 0.002952547457960620625 ),
 .UNSPECIFIED. ) ;
#155802 = CARTESIAN_POINT ( 'NONE',  ( -1.364683531250000748, 1.509375000341421691, 0.000000000000000000 ) ) ;
#155803 = CARTESIAN_POINT ( 'NONE',  ( 3.070069520051089906, -1.303570237086741024, 1.761582097007891923 ) ) ;
#155804 = CARTESIAN_POINT ( 'NONE',  ( 0.6311622855796270581, 3.199999999999994404, 0.3999999999999819811 ) ) ;
#155805 = CARTESIAN_POINT ( 'NONE',  ( 3.661208364039827856, -1.994111792441630726, -1.068896079077549910 ) ) ;
#155806 = CARTESIAN_POINT ( 'NONE',  ( -6.230135280679522936, 7.227244901336242755, 1.199719254218450271 ) ) ;
#155807 = LINE ( 'NONE', #153672, #87174 ) ;
#155808 = CARTESIAN_POINT ( 'NONE',  ( 6.463930056324285189, 6.765849701160138174, -0.2895399612845122039 ) ) ;
#155809 = CARTESIAN_POINT ( 'NONE',  ( 1.500000000000001332, 13.12499999999999822, 0.000000000000000000 ) ) ;
#155810 = CARTESIAN_POINT ( 'NONE',  ( 6.211043768836181478, 7.379210830797944709, 1.082531754730549967 ) ) ;
#155811 = CARTESIAN_POINT ( 'NONE',  ( 5.026482010321593030, 1.693441115147217291, 0.5138918105389718161 ) ) ;
#155812 = CARTESIAN_POINT ( 'NONE',  ( 6.988338112840064120, 10.24047933403371502, 1.199719254218460707 ) ) ;
#155813 = CARTESIAN_POINT ( 'NONE',  ( 2.309725134170067307, -0.4624151122551781179, 2.054391039957529586 ) ) ;
#155815 = CARTESIAN_POINT ( 'NONE',  ( -1.499999999999997780, 1.900000000000019673, 0.000000000000000000 ) ) ;
#155814 = CARTESIAN_POINT ( 'NONE',  ( 1.364683531249997417, 10.73437500034139802, 2.602085213965210642E-15 ) ) ;
#155816 = CARTESIAN_POINT ( 'NONE',  ( 1.152721088564850671, -0.4753370964276568134, -1.911210599630641882 ) ) ;
#155817 = DIRECTION ( 'NONE',  ( -0.000000000000000000, 1.000000000000000000, -0.000000000000000000 ) ) ;
#155818 = CARTESIAN_POINT ( 'NONE',  ( 0.3000000000000016542, 3.322650755865477645, 0.5865692111442620815 ) ) ;
#155820 = VERTEX_POINT ( 'NONE', #87370 ) ;
#155819 = CARTESIAN_POINT ( 'NONE',  ( 5.502179438505619302, -0.8068474266363240277, 1.622048611428918319 ) ) ;
#155821 = CARTESIAN_POINT ( 'NONE',  ( 6.155038550924133212, 10.12470270947942730, 0.7216878364870438212 ) ) ;
#155822 = CARTESIAN_POINT ( 'NONE',  ( 4.733189744967194024, -1.710186631362722309, 0.7584244158565583982 ) ) ;
#155823 = CARTESIAN_POINT ( 'NONE',  ( 3.999819011231439347, 4.625209253646830554, 1.199719254218464037 ) ) ;
#155824 = ORIENTED_EDGE ( 'NONE', *, *, #200474, .T. ) ;
#155825 = CARTESIAN_POINT ( 'NONE',  ( 4.416890754593222113, -1.537527071031305814, 1.386575359339572877 ) ) ;
#155826 = CARTESIAN_POINT ( 'NONE',  ( -1.225000000000012523, 2.000000000000001776, -1.214306433183764966E-14 ) ) ;
#155827 = CARTESIAN_POINT ( 'NONE',  ( -5.926322542504884439, 6.086666852443364029, -0.7216878364870338292 ) ) ;
#155828 = SURFACE_STYLE_USAGE ( .BOTH. , #27950 ) ;
#155829 = CARTESIAN_POINT ( 'NONE',  ( 8.260995669428309540, 8.532249790621511565, 0.7998128361456481317 ) ) ;
#155830 = CARTESIAN_POINT ( 'NONE',  ( -9.938290294017125603, 11.55342575023019691, -1.199719254218441611 ) ) ;
#155831 = CARTESIAN_POINT ( 'NONE',  ( 9.533882724342092274, 4.462909762398312274, 7.287958407156895468 ) ) ;
#155832 = CARTESIAN_POINT ( 'NONE',  ( 3.469446951953614189E-15, 6.120000000000021423, 1.214306433183764966E-14 ) ) ;
#155833 = CARTESIAN_POINT ( 'NONE',  ( 1.364683531249986537, -0.6364583329919177856, 0.7879004041258500513 ) ) ;
#155834 = CARTESIAN_POINT ( 'NONE',  ( 1.499999999999987121, 1.545833333333354487, -0.8660254037844253849 ) ) ;
#155836 = CARTESIAN_POINT ( 'NONE',  ( 6.145923705696426431, 6.064665832934283962, 0.7998128361456341429 ) ) ;
#155835 = CARTESIAN_POINT ( 'NONE',  ( 3.420314466093795414, 0.8798059112791326575, 1.753580237611163994 ) ) ;
#155837 = CARTESIAN_POINT ( 'NONE',  ( 2.056017322730230301, 1.755501262438976751, -0.9912458455646618871 ) ) ;
#155838 = CARTESIAN_POINT ( 'NONE',  ( 11.41381675112460847, 13.53016735491475941, -3.704697986577268232 ) ) ;
#155839 = CARTESIAN_POINT ( 'NONE',  ( 0.4626273691814064004, 3.108307088186316403, 0.4053073865230037987 ) ) ;
#155840 = CARTESIAN_POINT ( 'NONE',  ( -11.84103413958623818, 9.989955215268501831, 1.443924719788817423 ) ) ;
#155841 = CARTESIAN_POINT ( 'NONE',  ( 1.950266909631480861, 0.5821006739541793040, 1.777759251391328732 ) ) ;
#155842 = CARTESIAN_POINT ( 'NONE',  ( -1.364683531249997417, 4.509375000341424133, 1.214306433183764966E-14 ) ) ;
#155843 = CARTESIAN_POINT ( 'NONE',  ( -7.323375529675950624, 11.69568855126397011, -0.7998128361456291469 ) ) ;
#155845 = CARTESIAN_POINT ( 'NONE',  ( 3.796581652666820350, 1.495729193744433028, -1.498731062137735437 ) ) ;
#155844 = CARTESIAN_POINT ( 'NONE',  ( -4.446711195602239819, 8.131654128270509929, -0.7216878364870267237 ) ) ;
#155846 = CARTESIAN_POINT ( 'NONE',  ( 5.107906530550561541, 0.6527686194882609261, -1.964817160181751010 ) ) ;
#155847 = CARTESIAN_POINT ( 'NONE',  ( 6.261886844665240481, 8.398896966899865646, 1.599625672291268286 ) ) ;
#155849 = CARTESIAN_POINT ( 'NONE',  ( 6.720655732516647163, -0.007268404184145297979, 2.273772995263834140 ) ) ;
#155848 = CARTESIAN_POINT ( 'NONE',  ( 1.118821681092090126, -0.04763362108583040627, 2.090370170816723494 ) ) ;
#155851 = ORIENTED_EDGE ( 'NONE', *, *, #212155, .T. ) ;
#155850 = CARTESIAN_POINT ( 'NONE',  ( 6.370122744524995717, 0.9412729668686821149, 1.564051812004362940 ) ) ;
#155852 = CARTESIAN_POINT ( 'NONE',  ( 6.103141704446003679, 10.27208242182903142, 0.7998128361456462443 ) ) ;
#155853 = CARTESIAN_POINT ( 'NONE',  ( -3.904385050611244079, 7.498940292447679568, 1.040834085586084257E-14 ) ) ;
#155854 = CARTESIAN_POINT ( 'NONE',  ( -11.94980361490430099, 13.50332124735869854, 1.099999952233555955 ) ) ;
#155855 = AXIS2_PLACEMENT_3D ( 'NONE', #4785, #85010, #148953 ) ;
#155856 = CARTESIAN_POINT ( 'NONE',  ( -10.22583553578405358, 2.999999999999999556, 7.498742284419905424 ) ) ;
#155857 = CARTESIAN_POINT ( 'NONE',  ( 6.439759776366758892, 10.45687747249582955, 0.7216878364870438212 ) ) ;
#155858 = CARTESIAN_POINT ( 'NONE',  ( 0.6823417656249934904, 13.00520833367473017, 1.181850606188764807 ) ) ;
#155859 = CARTESIAN_POINT ( 'NONE',  ( 6.024064539286675846, -1.897261554996135802, 0.2387622092476364699 ) ) ;
#155860 = CARTESIAN_POINT ( 'NONE',  ( -9.182950115157607840, 9.607863310639020327, 0.7998128361456462443 ) ) ;
#155861 = CARTESIAN_POINT ( 'NONE',  ( 6.114890974963323345, 7.092793211334054604, 1.199719254218462483 ) ) ;
#155862 = CARTESIAN_POINT ( 'NONE',  ( 0.2970643657731242282, -6.863149499369272988, 10.99622371251743225 ) ) ;
#155863 = CARTESIAN_POINT ( 'NONE',  ( 0.000000000000000000, 0.000000000000000000, -5.732590180780448463 ) ) ;
#155864 = CARTESIAN_POINT ( 'NONE',  ( 4.356247428692526569, 3.976710176429713250, 0.7998128361456341429 ) ) ;
#155865 = ORIENTED_EDGE ( 'NONE', *, *, #210252, .T. ) ;
#155866 = CIRCLE ( 'NONE', #7095, 0.07999999999999972411 ) ;
#155867 = CARTESIAN_POINT ( 'NONE',  ( 6.485953897545715385, -2.015913262743720402, 0.05231248585663844652 ) ) ;
#155868 = CARTESIAN_POINT ( 'NONE',  ( -1.958975448762383504E-15, -9.746166700180790343, -9.500331257164614129 ) ) ;
#155869 = CARTESIAN_POINT ( 'NONE',  ( 10.94228617828407124, -8.109732095436330113, -0.2200370843778234053 ) ) ;
#155870 = CARTESIAN_POINT ( 'NONE',  ( 0.1399997263886003374, 7.629137130509076492, -2.599723212958489516 ) ) ;
#155871 = B_SPLINE_CURVE_WITH_KNOTS ( 'NONE', 3,
 ( #94528, #196272, #47919, #131329, #114031, #180025, #48963, #199441, #169088, #35887 ),
 .UNSPECIFIED., .F., .F.,
 ( 4, 3, 3, 4 ),
 ( 2.434915676126017810E-15, 3.125147921016584851E-05, 5.470111457697502723E-05, 7.815590336363350394E-05 ),
 .UNSPECIFIED. ) ;
#155872 = CARTESIAN_POINT ( 'NONE',  ( -3.782361668532609134, 7.356579680022602652, 1.040834085586084257E-14 ) ) ;
#155873 = CARTESIAN_POINT ( 'NONE',  ( 8.432808358020004391, 12.78210081775797669, 0.7216878364870438212 ) ) ;
#155874 = CARTESIAN_POINT ( 'NONE',  ( 2.817198160248539196, -1.711224680871022086, -0.9748066430285988737 ) ) ;
#155875 = CARTESIAN_POINT ( 'NONE',  ( 4.007435537932837910, -1.928747227692016564, 0.5880391185724976877 ) ) ;
#155876 = CARTESIAN_POINT ( 'NONE',  ( -7.542413527904030524, 7.693903958843159252, 1.040834085586084257E-14 ) ) ;
#155877 = CARTESIAN_POINT ( 'NONE',  ( -10.94228617828407302, -8.109732095436331889, 0.2200370843778256258 ) ) ;
#155878 = CARTESIAN_POINT ( 'NONE',  ( 5.191441776010862874, -0.7909675746368143301, 2.043907961996515699 ) ) ;
#155879 = CARTESIAN_POINT ( 'NONE',  ( -8.103009739377986520, -6.893137084989842123, 7.439168848974023973 ) ) ;
#155880 = CARTESIAN_POINT ( 'NONE',  ( 3.118101180835719521, -0.9482820236139007930, -1.676744857821835355 ) ) ;
#155881 = CARTESIAN_POINT ( 'NONE',  ( -9.267161690140662600, 10.77044237904097734, -1.199719254218441611 ) ) ;
#155882 = CARTESIAN_POINT ( 'NONE',  ( -0.1298852118744100725, 6.948705093303869873, -2.321530996463050389 ) ) ;
#155883 = CARTESIAN_POINT ( 'NONE',  ( 0.1331565106231571705, 4.092041177288479048, -2.500854978060399691 ) ) ;
#155884 = CARTESIAN_POINT ( 'NONE',  ( -8.171050021823464959, 15.51987628352802417, -8.834037178151259440 ) ) ;
#155885 = CARTESIAN_POINT ( 'NONE',  ( -1.364683531250004522, 13.36700584430852068, 0.2885925621847857947 ) ) ;
#155886 = CARTESIAN_POINT ( 'NONE',  ( 5.066996723205273057, 6.934582148538044777, 1.599625672291267398 ) ) ;
#155887 = CARTESIAN_POINT ( 'NONE',  ( -6.922777049148908013, -8.203199116536525892, 6.506163559800182128 ) ) ;
#155888 = CARTESIAN_POINT ( 'NONE',  ( 5.397554552016226914, 6.430140077841320689, 1.082531754730549078 ) ) ;
#155889 = ORIENTED_EDGE ( 'NONE', *, *, #156113, .T. ) ;
#155891 = CARTESIAN_POINT ( 'NONE',  ( 3.000642180831034622, -1.983674057915509881, -0.3420062109290455954 ) ) ;
#155890 = CARTESIAN_POINT ( 'NONE',  ( 5.776868925826902590, 1.698781319366513998, -0.7106697882480541573 ) ) ;
#155892 = CARTESIAN_POINT ( 'NONE',  ( 4.851052417537679240, -1.089491736270932432, 2.023782222440795753 ) ) ;
#155894 = CARTESIAN_POINT ( 'NONE',  ( 2.922522432510234136, -1.287038294151692241, 1.344341647096161996 ) ) ;
#155893 = FACE_OUTER_BOUND ( 'NONE', #150756, .T. ) ;
#155895 = CARTESIAN_POINT ( 'NONE',  ( 1.642778471875000035, -0.2260416661887081069, -2.845375778867859751 ) ) ;
#155896 = DIRECTION ( 'NONE',  ( 0.000000000000000000, 1.000000000000000000, 0.000000000000000000 ) ) ;
#155897 = SURFACE_SIDE_STYLE ('',( #140748 ) ) ;
#155898 = CARTESIAN_POINT ( 'NONE',  ( -6.880926654135487652, 7.986501503701545879, 1.199719254218450271 ) ) ;
#155899 = CARTESIAN_POINT ( 'NONE',  ( -4.340018570150318666, 6.156717313299049366, -1.443375672974066548 ) ) ;
#155900 = CARTESIAN_POINT ( 'NONE',  ( 6.550343146927733784, -1.615745695573450824, 1.326605865911892002 ) ) ;
#155901 = CARTESIAN_POINT ( 'NONE',  ( 6.643132081016125845, 6.852668304048034287, 0.7216878364870317197 ) ) ;
#155902 = ORIENTED_EDGE ( 'NONE', *, *, #103930, .F. ) ;
#155903 = ADVANCED_FACE ( 'NONE', ( #5011 ), #71084, .T. ) ;
#155904 = CARTESIAN_POINT ( 'NONE',  ( 10.39398850336073643, -8.287668210030899374, -0.6181847325714995289 ) ) ;
#155905 = CARTESIAN_POINT ( 'NONE',  ( 4.760662214969796580, 8.263722922863950160, 0.7838479752697187219 ) ) ;
#155906 = CARTESIAN_POINT ( 'NONE',  ( 6.129511981615775262, -1.621618681806114459, 0.5882815792577487102 ) ) ;
#155907 = CARTESIAN_POINT ( 'NONE',  ( -6.423865854776591000, 6.388931673527803667, 1.040834085586084257E-14 ) ) ;
#155908 = CARTESIAN_POINT ( 'NONE',  ( 1.353744004007218615, 0.1277301157788513497, -1.729473920685227428 ) ) ;
#155909 = CARTESIAN_POINT ( 'NONE',  ( 1.387778780781441485E-16, 3.900000000000000799, -2.500000000000000000 ) ) ;
#155910 = CARTESIAN_POINT ( 'NONE',  ( 0.000000000000000000, -3.499999999999999556, 0.000000000000000000 ) ) ;
#155911 = CARTESIAN_POINT ( 'NONE',  ( -7.393273838153706201, 7.519907654134449615, 0.7998128361456341429 ) ) ;
#155912 = CARTESIAN_POINT ( 'NONE',  ( -5.824764126078942006, 6.052491103662449135, 0.4936746899740264150 ) ) ;
#155913 = CARTESIAN_POINT ( 'NONE',  ( 0.3564121386029559524, -2.069725681613205470, -0.05427943458365809548 ) ) ;
#155914 = CARTESIAN_POINT ( 'NONE',  ( 5.637271085457097541, -1.648663388651723460, 0.7845467231081537651 ) ) ;
#155915 = CARTESIAN_POINT ( 'NONE',  ( 3.801568999928582659, -1.482573837031101016, -1.284759613706359271 ) ) ;
#155916 = ADVANCED_FACE ( 'NONE', ( #60196 ), #72158, .F. ) ;
#155917 = CARTESIAN_POINT ( 'NONE',  ( -3.355169270512988773E-14, -0.8749999993172000723, 1.414508159514567431 ) ) ;
#155918 = CARTESIAN_POINT ( 'NONE',  ( -1.500000000000005773, 5.629166666666694852, -0.8660254037844342667 ) ) ;
#155919 = CARTESIAN_POINT ( 'NONE',  ( 7.623762449586013901, 7.788811034138823253, 1.040834085586084257E-14 ) ) ;
#155920 = CARTESIAN_POINT ( 'NONE',  ( 3.668700845920089826, 0.7647225481513253431, 1.977962425194310203 ) ) ;
#155921 = DIRECTION ( 'NONE',  ( 0.000000000000000000, 1.485208455481716443E-16, -1.000000000000000000 ) ) ;
#155922 = EDGE_CURVE ( 'NONE', #25107, #191425, #143378, .T. ) ;
#155923 = CARTESIAN_POINT ( 'NONE',  ( 0.4370080631058587683, -8.003595416197011758, -10.68747925529770271 ) ) ;
#155924 = CARTESIAN_POINT ( 'NONE',  ( 1.674760025662187735, 1.393346669028448392, -1.531324272915953744 ) ) ;
#155926 = CARTESIAN_POINT ( 'NONE',  ( 0.7500000000000006661, 15.11458333401612819, 1.299038105676657340 ) ) ;
#155925 = CARTESIAN_POINT ( 'NONE',  ( -11.95360554405587017, 11.10444996502583237, 1.059413164304700006 ) ) ;
#155928 = ORIENTED_EDGE ( 'NONE', *, *, #3914, .T. ) ;
#155927 = CARTESIAN_POINT ( 'NONE',  ( 3.370003599138057471, 0.5381768412672756074, -2.155016279732512974 ) ) ;
#155929 = CARTESIAN_POINT ( 'NONE',  ( 1.811588643561705680, 1.319210623403826110, -1.882327697243087350 ) ) ;
#155931 = CARTESIAN_POINT ( 'NONE',  ( 6.649293052619501765, 1.797374026962361482, -1.011582863395175114 ) ) ;
#155930 = CARTESIAN_POINT ( 'NONE',  ( 10.07334494527360569, 10.85458331234846696, 0.000000000000000000 ) ) ;
#155933 = CARTESIAN_POINT ( 'NONE',  ( -3.475000000000000533, -0.7291666666666675178, -2.006292185433948827 ) ) ;
#155932 = CARTESIAN_POINT ( 'NONE',  ( 4.797606254389322089, 6.690569611577942943, 1.599625672291268286 ) ) ;
#155934 = CARTESIAN_POINT ( 'NONE',  ( -3.929058411375401683, -1.000000000000000888, -0.7500000000000006661 ) ) ;
#155935 = CARTESIAN_POINT ( 'NONE',  ( 6.128435733830499998, 0.1874100934057248424, 1.831705376836203936 ) ) ;
#155936 = CARTESIAN_POINT ( 'NONE',  ( -1.815167269671988270, -0.3943365573012030945, 0.6613654005181992535 ) ) ;
#155937 = CARTESIAN_POINT ( 'NONE',  ( 3.129067941553372645, 1.730785544086024696, 0.8136490247460312908 ) ) ;
#155938 = CARTESIAN_POINT ( 'NONE',  ( -0.2102771530458276972, 0.6786276403282426317, -2.283427277113641019 ) ) ;
#155939 = CARTESIAN_POINT ( 'NONE',  ( 4.032037319687285404, 0.9221689259152658913, -1.457338292308225869 ) ) ;
#155940 = CARTESIAN_POINT ( 'NONE',  ( 2.096888995370162156, 1.803417055948232983, 0.9023429676050932491 ) ) ;
#155941 = CARTESIAN_POINT ( 'NONE',  ( 3.885566394551481562, -0.7213347477983514944, -2.182621754721993490 ) ) ;
#155942 = CARTESIAN_POINT ( 'NONE',  ( 3.146068640573984165, 0.8174054641026907708, -2.109740015476600838 ) ) ;
#155943 = CARTESIAN_POINT ( 'NONE',  ( 5.162764661449575243, -1.526107291725445236, 1.451632374922463553 ) ) ;
#155944 = CARTESIAN_POINT ( 'NONE',  ( -5.478903473698247595, 8.445785581739666981, -1.082531754730549967 ) ) ;
#155945 = ORIENTED_EDGE ( 'NONE', *, *, #20664, .T. ) ;
#155946 = CARTESIAN_POINT ( 'NONE',  ( 4.762845401903825326, -1.580659612885275012, -0.7961057336023872333 ) ) ;
#155948 = CARTESIAN_POINT ( 'NONE',  ( 1.201600019185744994, -0.5526092242729553350, 2.224544611104557035 ) ) ;
#155947 = CARTESIAN_POINT ( 'NONE',  ( 6.282224075085741433, 8.422623735723785643, 1.599625672291268286 ) ) ;
#155949 = CARTESIAN_POINT ( 'NONE',  ( 5.718664505737725001, -0.04093049815006092468, 1.840854889930729765 ) ) ;
#155950 = CARTESIAN_POINT ( 'NONE',  ( -5.108724954250998707, 4.854600622914589714, -0.7998128361456221525 ) ) ;
#155951 = UNCERTAINTY_MEASURE_WITH_UNIT (LENGTH_MEASURE( 1.000000000000000082E-05 ), #39291, 'distance_accuracy_value', 'NONE');
#155952 = CARTESIAN_POINT ( 'NONE',  ( 5.912113082354765403, 1.474260358680115290, -1.621598248542432064 ) ) ;
#155953 = CARTESIAN_POINT ( 'NONE',  ( -2.598358995313378550, 6.183169261174235487, 0.7998128361456341429 ) ) ;
#155954 = CARTESIAN_POINT ( 'NONE',  ( -4.353222949258705121, 15.46947200944509682, 11.19154526970763364 ) ) ;
#155955 = CARTESIAN_POINT ( 'NONE',  ( 5.916483165358986440, 0.8355632440216669288, 1.894440869009452300 ) ) ;
#155956 = CARTESIAN_POINT ( 'NONE',  ( 0.2687680251878405424, -0.2516378192510167477, -2.000730910237565663 ) ) ;
#155957 = CARTESIAN_POINT ( 'NONE',  ( -1.500000000000015099, -0.5895833326505155458, -0.8660254037844383745 ) ) ;
#155958 = CARTESIAN_POINT ( 'NONE',  ( 4.723225685987796574, -0.09301374627979085152, 1.924373785979951013 ) ) ;
#155959 = CARTESIAN_POINT ( 'NONE',  ( 0.6823417656249969321, 10.27604166700806587, -1.181850606188757036 ) ) ;
#155960 = FACE_OUTER_BOUND ( 'NONE', #208193, .T. ) ;
#155961 = CARTESIAN_POINT ( 'NONE',  ( 1.389269710167878369, -2.111442789942123088, -0.6905784607170639688 ) ) ;
#155963 = EDGE_LOOP ( 'NONE', ( #169113, #132324, #124663, #158871 ) ) ;
#155962 = CARTESIAN_POINT ( 'NONE',  ( -0.7655046440382844430, 13.24001401857275440, -1.290086495267464883 ) ) ;
#155965 = CARTESIAN_POINT ( 'NONE',  ( -1.304512053934558738E-16, 4.000000000000001776, 2.350000000000007194 ) ) ;
#155964 = CARTESIAN_POINT ( 'NONE',  ( -4.095971805104331231, 5.871996087412059140, 1.443375672974065660 ) ) ;
#155966 = CARTESIAN_POINT ( 'NONE',  ( 10.16199982864259788, 11.81442020729326536, 1.199719254218452047 ) ) ;
#155967 = CARTESIAN_POINT ( 'NONE',  ( -0.9311234436981496998, -2.378130369558483004, 3.475000000000000977 ) ) ;
#155968 = CARTESIAN_POINT ( 'NONE',  ( 5.346851039111029991, 6.199209027673978412, 7.500000000000000000 ) ) ;
#155969 = CARTESIAN_POINT ( 'NONE',  ( 10.80647848125409993, 9.579244470042894477, -5.114164611927699333 ) ) ;
#155970 = CARTESIAN_POINT ( 'NONE',  ( -1.423205080756851260, 7.980384757729337863, 10.65537363484302524 ) ) ;
#155971 = CARTESIAN_POINT ( 'NONE',  ( 1.223018651738450480, -1.772137153356953432, -0.8420139538000551704 ) ) ;
#155972 = CARTESIAN_POINT ( 'NONE',  ( -1.364683531250000748, 2.071875000341422357, 1.214306433183764966E-14 ) ) ;
#155973 = CARTESIAN_POINT ( 'NONE',  ( 6.144970055084349347, -0.2864424343173576082, -1.940704187532462210 ) ) ;
#155974 = CARTESIAN_POINT ( 'NONE',  ( -7.147119532698295252, 11.49005655479003174, 0.000000000000000000 ) ) ;
#155975 = CARTESIAN_POINT ( 'NONE',  ( -4.555176424067209240, 8.258196894812975586, 1.040834085586084257E-14 ) ) ;
#155976 = CARTESIAN_POINT ( 'NONE',  ( 0.3392369075362114961, 0.3904986559340599128, 2.228413801644222758 ) ) ;
#155978 = EDGE_LOOP ( 'NONE', ( #98384, #32650 ) ) ;
#155977 = CARTESIAN_POINT ( 'NONE',  ( -6.392833124043511894, 7.417059051927569868, 1.199719254218450271 ) ) ;
#155979 = CARTESIAN_POINT ( 'NONE',  ( -0.7500000000000249800, -1.277083332650516656, 1.299038105676659116 ) ) ;
#155980 = CARTESIAN_POINT ( 'NONE',  ( 0.9306671693925671063, 0.1315677519515070781, 1.865966016356377821 ) ) ;
#155981 = CARTESIAN_POINT ( 'NONE',  ( 0.5801786448705691379, -0.6264061342569470225, 1.617264071341844245 ) ) ;
#155983 = CARTESIAN_POINT ( 'NONE',  ( 3.984055765753656164, -2.167877601896048390, -0.3204034371554059235 ) ) ;
#155982 = CARTESIAN_POINT ( 'NONE',  ( 0.6801582343749796866, 1.473958333674751930, 1.178068619123789462 ) ) ;
#155984 = CARTESIAN_POINT ( 'NONE',  ( 3.979734726549417623, 2.174020839304124042, -0.7740601867209749853 ) ) ;
#155985 = CARTESIAN_POINT ( 'NONE',  ( 6.925078400183531713, -0.004750840071900476122, 2.044148492825672569 ) ) ;
#155986 = CARTESIAN_POINT ( 'NONE',  ( 2.431497994139957264, 0.9153433635570235039, -1.712687122320022626 ) ) ;
#155987 = CARTESIAN_POINT ( 'NONE',  ( -4.555176424067209240, 8.258196894812975586, 1.040834085586084257E-14 ) ) ;
#155988 = DIRECTION ( 'NONE',  ( 0.7592566023653005702, -0.6507913734559639396, 0.000000000000000000 ) ) ;
#155989 = EDGE_CURVE ( 'NONE', #68973, #61933, #7159, .T. ) ;
#155990 = CARTESIAN_POINT ( 'NONE',  ( 5.467072749063267345, -1.670387955228332277, 1.306269166133757986 ) ) ;
#155991 = SURFACE_SIDE_STYLE ('',( #89940 ) ) ;
#155992 = CARTESIAN_POINT ( 'NONE',  ( 3.498672800139957406, -1.986100699840901651, 0.3474671148789992836 ) ) ;
#155993 = CARTESIAN_POINT ( 'NONE',  ( -4.053524740361572398, 7.672936597156388316, 0.7216878364870317197 ) ) ;
#155994 = CARTESIAN_POINT ( 'NONE',  ( -5.582925393777276035, 9.735439736040634173, 0.7998128361456291469 ) ) ;
#155995 = CARTESIAN_POINT ( 'NONE',  ( 9.154780037725547714, 11.70366268214508487, 1.599625672291279388 ) ) ;
#155996 = CARTESIAN_POINT ( 'NONE',  ( 0.5041868517345666767, -0.6120625888205477594, -1.720162557568189809 ) ) ;
#155997 = CARTESIAN_POINT ( 'NONE',  ( -5.692444392891315097, 7.734547439830227411, -1.599625672291271394 ) ) ;
#155998 = CARTESIAN_POINT ( 'NONE',  ( -0.06005734137062879868, 15.49847999378906138, 11.99783618803943241 ) ) ;
#155999 = CARTESIAN_POINT ( 'NONE',  ( -9.748179543381699119, 3.057003318903428912, 6.445181705109019887 ) ) ;
#156000 = ORIENTED_EDGE ( 'NONE', *, *, #52471, .T. ) ;
#156001 = CARTESIAN_POINT ( 'NONE',  ( 5.735248378139378822, -1.864208485850331609, 0.8789154904798938128 ) ) ;
#156002 = CARTESIAN_POINT ( 'NONE',  ( -5.736508391913536897, 9.706693867292189637, 0.7216878364870267237 ) ) ;
#156003 = CARTESIAN_POINT ( 'NONE',  ( 7.065207446052794715, 9.336104335185329006, -1.443375672974064550 ) ) ;
#156004 = CARTESIAN_POINT ( 'NONE',  ( -2.591579918506545344, 6.175260338232929413, 1.040834085586084257E-14 ) ) ;
#156005 = CARTESIAN_POINT ( 'NONE',  ( -10.45741655484220267, 11.09474082360439873, -0.7998128361456221525 ) ) ;
#156006 = CARTESIAN_POINT ( 'NONE',  ( 4.951822102061871789, -1.429791030739693047, -1.426725901824247078 ) ) ;
#156007 = CARTESIAN_POINT ( 'NONE',  ( 5.531947820799793192, -2.167606221786242848, 0.4847573843902542312 ) ) ;
#156009 = CARTESIAN_POINT ( 'NONE',  ( 7.104109303880752790, 11.23195192126214970, -0.7216878364870267237 ) ) ;
#156008 = CARTESIAN_POINT ( 'NONE',  ( -2.844178363816758814, 6.540234867753325076, -0.7998128361456481317 ) ) ;
#156010 = CARTESIAN_POINT ( 'NONE',  ( 6.169123589417988995, 7.156064594864501416, -1.199719254218445830 ) ) ;
#156011 = STYLED_ITEM ( 'NONE', ( #41845 ), #170365 ) ;
#156012 = CARTESIAN_POINT ( 'NONE',  ( 4.680574674004650326, -1.998471466470305602, -0.5028169189831372954 ) ) ;
#156013 = CARTESIAN_POINT ( 'NONE',  ( 3.955704058034177351, -1.882473782773282700, -0.7231407674024927790 ) ) ;
#156014 = ORIENTED_EDGE ( 'NONE', *, *, #104484, .T. ) ;
#156015 = EDGE_CURVE ( 'NONE', #105092, #146253, #208561, .T. ) ;
#156016 = CARTESIAN_POINT ( 'NONE',  ( 3.837121167867449945, 4.435395103055503441, 1.199719254218464037 ) ) ;
#156018 = EDGE_LOOP ( 'NONE', ( #167844, #76479, #196118, #176337, #39064, #139250, #10636, #207567, #3963, #143002, #35387 ) ) ;
#156017 = CARTESIAN_POINT ( 'NONE',  ( -7.014364370223741929, 9.276787413384745662, -1.599625672291271394 ) ) ;
#156019 = CARTESIAN_POINT ( 'NONE',  ( 5.273189713885392926, 7.658326211947664497, -1.220946906274408494 ) ) ;
#156020 = CARTESIAN_POINT ( 'NONE',  ( 3.708361104356564297, -1.524809962200252444, -1.319026932540816599 ) ) ;
#156021 = CARTESIAN_POINT ( 'NONE',  ( 3.134520880496123318, -1.623366475481220261, 0.8686021547102340534 ) ) ;
#156022 = CARTESIAN_POINT ( 'NONE',  ( 6.343417644181545967, 6.506394916570013898, 2.500000000000000444 ) ) ;
#156023 = CARTESIAN_POINT ( 'NONE',  ( 0.6280632297508845774, -2.189494644770412890, 0.7293192972532935858 ) ) ;
#156024 = CARTESIAN_POINT ( 'NONE',  ( 4.543917759235442944, 5.330267469643351852, 1.199719254218452935 ) ) ;
#156025 = CARTESIAN_POINT ( 'NONE',  ( 3.813887338145681927, -2.130327034543195275, 0.3653767458386343314 ) ) ;
#156026 = CARTESIAN_POINT ( 'NONE',  ( -5.599681137644054729, 6.491715067794862293, 1.199719254218450271 ) ) ;
#156027 = CARTESIAN_POINT ( 'NONE',  ( 0.07538891330675548397, -7.154544010627095219, -9.499700864329911454 ) ) ;
#156028 = CARTESIAN_POINT ( 'NONE',  ( 1.973319494866377699, 1.790917844098998124, -0.5403536831049270406 ) ) ;
#156029 = CARTESIAN_POINT ( 'NONE',  ( 0.5441301207207068780, 1.965759916638841309, 0.1495998195316684265 ) ) ;
#156031 = CARTESIAN_POINT ( 'NONE',  ( 10.90207482560801999, -7.666862915010147717, -0.6254314485565921622 ) ) ;
#156030 = CARTESIAN_POINT ( 'NONE',  ( 1.364683531249990311, 4.134375000341417028, 1.214306433183764966E-14 ) ) ;
#156033 = CARTESIAN_POINT ( 'NONE',  ( 1.875870136999336246, 2.111227540014638304, -0.6426800678154330759 ) ) ;
#156032 = CARTESIAN_POINT ( 'NONE',  ( -5.250031796989778066, 7.148123067953287446, 1.599625672291267398 ) ) ;
#156034 = EDGE_CURVE ( 'NONE', #181416, #82411, #209023, .T. ) ;
#156035 = CARTESIAN_POINT ( 'NONE',  ( 0.000000000000000000, 12.31951671548121219, 10.25000000000000000 ) ) ;
#156036 = CARTESIAN_POINT ( 'NONE',  ( 5.355634372598031767, 6.206993841907870291, -1.199719254218445830 ) ) ;
#156037 = CARTESIAN_POINT ( 'NONE',  ( -3.913499895838973508, 7.717500311787445000, 1.040834085586084257E-14 ) ) ;
#156038 = CARTESIAN_POINT ( 'NONE',  ( 11.97297122925952273, 13.79874920673088745, 0.8121202983519189011 ) ) ;
#156039 = CARTESIAN_POINT ( 'NONE',  ( 5.647334207030327846, -1.553848685622709835, -1.213239188487026166 ) ) ;
#156040 = CARTESIAN_POINT ( 'NONE',  ( 5.865930957382810895, 2.274600175340906638, -0.3886535673101945143 ) ) ;
#156041 = CARTESIAN_POINT ( 'NONE',  ( 0.8187140321147531319, -1.423520202335259999, 1.350257566363553208 ) ) ;
#156042 = EDGE_CURVE ( 'NONE', #62806, #173456, #105794, .T. ) ;
#156043 = CARTESIAN_POINT ( 'NONE',  ( 2.500897397093455155, 0.4475292293845704594, 2.013297154094250807 ) ) ;
#156044 = CARTESIAN_POINT ( 'NONE',  ( 6.480434237652132445, 7.623223367758051872, 1.082531754730558626 ) ) ;
#156045 = CARTESIAN_POINT ( 'NONE',  ( 7.842465510862060896, 8.114240948952696542, 0.000000000000000000 ) ) ;
#156046 = CARTESIAN_POINT ( 'NONE',  ( 6.846504384776753049, 9.010674420371453053, -1.443375672974058777 ) ) ;
#156047 = CARTESIAN_POINT ( 'NONE',  ( 1.364683531249990311, 3.446875000341416584, 1.214306433183764966E-14 ) ) ;
#156048 = CARTESIAN_POINT ( 'NONE',  ( -9.864361085393147377, 3.580476348100011919, -6.759752543078383802 ) ) ;
#156049 = CARTESIAN_POINT ( 'NONE',  ( 5.951666246274807115, 6.045958163516475636, 0.7216878364870317197 ) ) ;
#156050 = CARTESIAN_POINT ( 'NONE',  ( 5.178266966923749770, -1.157238278732542369, -1.836894593069735793 ) ) ;
#156052 = CARTESIAN_POINT ( 'NONE',  ( 4.897927690869709139, -0.6253142351902387652, -1.731941863025769246 ) ) ;
#156051 = CARTESIAN_POINT ( 'NONE',  ( 2.680403734646828351, 0.4910177078051911614, -0.09999999999999592548 ) ) ;
#156053 = B_SPLINE_CURVE_WITH_KNOTS ( 'NONE', 3,
 ( #161025, #132815, #212950, #46226 ),
 .UNSPECIFIED., .F., .F.,
 ( 4, 4 ),
 ( 0.000000000000000000, 0.0001591186035317672907 ),
 .UNSPECIFIED. ) ;
#156054 = MANIFOLD_SOLID_BREP ( 'Fillet7', #146810 ) ;
#156056 = CARTESIAN_POINT ( 'NONE',  ( 6.620655732516644854, 4.701125524277991907, 2.388986273831222640 ) ) ;
#156055 = CARTESIAN_POINT ( 'NONE',  ( -11.92619526913699879, 10.89999999999998259, 1.328859060402682868 ) ) ;
#156057 = CARTESIAN_POINT ( 'NONE',  ( 6.720655732516647163, -0.007268404184145290173, 2.273772995263834584 ) ) ;
#156058 = CARTESIAN_POINT ( 'NONE',  ( 0.5791066246769066561, 1.747692025923882841, -0.6672336632058752937 ) ) ;
#156059 = CARTESIAN_POINT ( 'NONE',  ( 0.6150082408139592172, 1.559066714514239393, -1.639647465354547196 ) ) ;
#156060 = CARTESIAN_POINT ( 'NONE',  ( -5.139172151939493283, 6.684247474441955106, 1.432371535143169394 ) ) ;
#156061 = DIRECTION ( 'NONE',  ( -0.9980366791916180924, 0.000000000000000000, 0.06263215618328135670 ) ) ;
#156062 = CARTESIAN_POINT ( 'NONE',  ( 6.589288424369031283, 6.777081280454712697, 0.2339771526987007022 ) ) ;
#156063 = CARTESIAN_POINT ( 'NONE',  ( -3.973948422136968084, 7.650373902552835226, -0.7216878364870458196 ) ) ;
#156064 = CARTESIAN_POINT ( 'NONE',  ( 11.33772463945036790, 13.40000000000000036, -3.600000000000002309 ) ) ;
#156065 = CARTESIAN_POINT ( 'NONE',  ( 6.159198499077391808, -1.652456008184695735, -0.9899348748576908275 ) ) ;
#156066 = CARTESIAN_POINT ( 'NONE',  ( 2.166550811918485753, -1.616863761265506794, -0.7202261968358366628 ) ) ;
#156067 = CIRCLE ( 'NONE', #138759, 2.000000000000000000 ) ;
#156068 = CARTESIAN_POINT ( 'NONE',  ( 6.182294962360654900, 1.036951722903585837, 1.725357817989848996 ) ) ;
#156070 = CARTESIAN_POINT ( 'NONE',  ( 3.585460515032745210, -0.5529844701629010872, 1.834067302312661241 ) ) ;
#156069 = CARTESIAN_POINT ( 'NONE',  ( -9.938290294017125603, 11.55342575023019691, -1.199719254218441611 ) ) ;
#156071 = AXIS2_PLACEMENT_3D ( 'NONE', #194838, #164477, #81091 ) ;
#156072 = CARTESIAN_POINT ( 'NONE',  ( 2.184835310096557404, 5.700724961754617404, 1.040834085586084257E-14 ) ) ;
#156073 = CARTESIAN_POINT ( 'NONE',  ( 4.035575377323636026, 1.855309441653162139, -0.6614512482757756162 ) ) ;
#156074 = CARTESIAN_POINT ( 'NONE',  ( 6.451426753955883164, -1.802380967894920527, 0.9117540809469369956 ) ) ;
#156075 = CARTESIAN_POINT ( 'NONE',  ( -1.777638883463123598, -0.9165151389911724289, 1.199999999999999734 ) ) ;
#156076 = CARTESIAN_POINT ( 'NONE',  ( 2.500682550815761740, 1.503739811390795378, -1.112508705057350999 ) ) ;
#156078 = ORIENTED_EDGE ( 'NONE', *, *, #142903, .T. ) ;
#156077 = CARTESIAN_POINT ( 'NONE',  ( 6.252575197229738535, 0.5485693247098271108, 1.635415954441843844 ) ) ;
#156080 = CARTESIAN_POINT ( 'NONE',  ( 2.873965376416980355, 6.296784005887697155, -0.7216878364870267237 ) ) ;
#156079 = CARTESIAN_POINT ( 'NONE',  ( 1.998912159191484905, -0.5904864226158462737, -2.126349760018491963 ) ) ;
#156081 = CARTESIAN_POINT ( 'NONE',  ( 0.6823417656249899377, 3.738541667008085767, -1.181850606188754593 ) ) ;
#156082 = CARTESIAN_POINT ( 'NONE',  ( 6.566857081534598350, 1.454584517406570132, -1.316677807353151097 ) ) ;
#156083 = CARTESIAN_POINT ( 'NONE',  ( 6.889514614038635187, 11.18951748302043114, -0.7998128361456291469 ) ) ;
#156084 = CARTESIAN_POINT ( 'NONE',  ( -8.967828540435322182, 12.54988483289483980, 1.199719254218462483 ) ) ;
#156085 = CARTESIAN_POINT ( 'NONE',  ( -8.845566791370137238, 3.603011019375353285, -7.955782632700151069 ) ) ;
#156086 = CARTESIAN_POINT ( 'NONE',  ( 0.1747926744264451659, 0.2546335194838904581, -1.890750172325323275 ) ) ;
#156087 = EDGE_CURVE ( 'NONE', #180510, #22857, #198271, .T. ) ;
#156088 = CARTESIAN_POINT ( 'NONE',  ( 0.000000000000000000, 12.30000000000000071, 0.000000000000000000 ) ) ;
#156089 =( BOUNDED_CURVE ( )  B_SPLINE_CURVE ( 2, ( #6483, #72560, #138658, #204679, #189518, #122489, #53120 ),
 .UNSPECIFIED., .F., .T. ) 
 B_SPLINE_CURVE_WITH_KNOTS ( ( 3, 2, 2, 3 ),
 ( 0.1749999999999997669, 0.1791666666666665020, 0.1833333333333332371, 0.1874999999999999722 ),
 .UNSPECIFIED. ) 
 CURVE ( )  GEOMETRIC_REPRESENTATION_ITEM ( )  RATIONAL_B_SPLINE_CURVE ( ( 1.000000000000007105, 0.8660254037844316022, 1.000000000000000000, 0.8660254037844387076, 1.000000000000000000, 0.8660254037844395958, 0.9999999999999991118 ) ) 
 REPRESENTATION_ITEM ( '' )  );
#156090 = ORIENTED_EDGE ( 'NONE', *, *, #113251, .T. ) ;
#156091 = CARTESIAN_POINT ( 'NONE',  ( 2.189971326302230903, -1.350648006375281929, -1.569233719104834890 ) ) ;
#156092 = CARTESIAN_POINT ( 'NONE',  ( -1.499999999999997780, 3.650000000000021227, 1.214306433183764966E-14 ) ) ;
#156093 = CARTESIAN_POINT ( 'NONE',  ( 4.299907273828439180, 8.168308919441841454, 1.040834085586084257E-14 ) ) ;
#156094 = CARTESIAN_POINT ( 'NONE',  ( 7.512626515748109135, 8.897724035528543851, 1.082531754730549967 ) ) ;
#156095 = CARTESIAN_POINT ( 'NONE',  ( 6.340501840829311675, 1.221348521443364366, -1.733245716811770309 ) ) ;
#156096 = CARTESIAN_POINT ( 'NONE',  ( 1.438721403194116233, 7.870009100115498590, 3.684356824108467876 ) ) ;
#156097 = CARTESIAN_POINT ( 'NONE',  ( 0.6823417656249917140, 3.592708333674754506, 1.181850606188765695 ) ) ;
#156099 = CARTESIAN_POINT ( 'NONE',  ( 8.703971430293332645, 12.13808852110884118, -1.082531754730543083 ) ) ;
#156098 = CARTESIAN_POINT ( 'NONE',  ( 0.07479286986305369589, 1.387406912293275729, -2.112587013352088317 ) ) ;
#156100 = CARTESIAN_POINT ( 'NONE',  ( 5.571638683613604037, 1.528505562557905595, -1.314797328242120367 ) ) ;
#156101 = CARTESIAN_POINT ( 'NONE',  ( 6.280494692369203769, -0.5183099952858164494, -1.844178102243919870 ) ) ;
#156102 = CARTESIAN_POINT ( 'NONE',  ( 6.539320575229223387, 6.036367980355456631, 2.598156967962389263 ) ) ;
#156103 = CARTESIAN_POINT ( 'NONE',  ( 3.386445149735781257, -0.4294187885149694517, -2.148908265708626697 ) ) ;
#156104 =( BOUNDED_SURFACE ( )  B_SPLINE_SURFACE ( 3, 3, ( 
 ( #124089, #141361, #5940, #24333, #206299, #88300, #158637, #207374, #139187, #191108, #72011, #58994, #26485, #123033, #187909, #188984, #172758, #76309 ),
 ( #192176, #55786, #104554, #157580, #190052, #92595, #60059, #57924, #42776, #125150, #142416, #9173, #174906, #121943, #105640, #10234, #208425, #126214 ),
 ( #22184, #106731, #8098, #107814, #23264, #89376, #155425, #74187, #41704, #173839, #25416, #7010, #91521, #73086, #56859, #90441, #156509, #11296 ),
 ( #61128, #144560, #28636, #146679, #63262, #30782, #45970, #44906, #211627, #130477, #79512, #127288, #145630, #43837, #209487, #143490, #14491, #160766 ),
 ( #129424, #114222, #62204, #111014, #195407, #94723, #95791, #212694, #77375, #47037, #193259, #109953, #177019, #12361, #80581, #178092, #113152, #13436 ),
 ( #175963, #179158, #96861, #194328, #27558, #159697, #162909, #64336, #93654, #196468, #48110, #112091, #78440, #210570, #128360, #29710, #161848, #109590 ),
 ( #191807, #23980, #140993, #90083, #208063, #57569, #74885, #157210, #60758, #40257, #123727, #175596, #138832, #106369, #56502, #207001, #7728, #43472 ) ),
 .UNSPECIFIED., .T., .F., .T. ) 
 B_SPLINE_SURFACE_WITH_KNOTS ( ( 4, 3, 4 ),
 ( 4, 2, 2, 2, 2, 2, 2, 2, 4 ),
 ( 0.000000000000000000, 0.5000000000000000000, 1.000000000000000000 ),
 ( 0.7548633226336768365, 0.7573624263556413272, 0.7598615300776057069, 0.7648597375215344663, 0.7748561524093919850, 0.7948489821851072445, 0.8148337662062091757, 0.8248261582167601969, 0.8348185502273111069 ),
 .UNSPECIFIED. ) 
 GEOMETRIC_REPRESENTATION_ITEM ( )  RATIONAL_B_SPLINE_SURFACE ( (
 ( 1.000000000000000000, 1.000000000000000000, 1.000000000000000000, 1.000000000000000000, 1.000000000000000000, 1.000000000000000000, 1.000000000000000000, 1.000000000000000000, 1.000000000000000000, 1.000000000000000000, 1.000000000000000000, 1.000000000000000000, 1.000000000000000000, 1.000000000000000000, 1.000000000000000000, 1.000000000000000000, 1.000000000000000000, 1.000000000000000000),
 ( 0.3333333333333333703, 0.3333333333333333703, 0.3333333333333333703, 0.3333333333333333703, 0.3333333333333333703, 0.3333333333333333703, 0.3333333333333333703, 0.3333333333333333703, 0.3333333333333333703, 0.3333333333333333703, 0.3333333333333333703, 0.3333333333333333703, 0.3333333333333333703, 0.3333333333333333703, 0.3333333333333333703, 0.3333333333333333703, 0.3333333333333333703, 0.3333333333333333703),
 ( 0.3333333333333333703, 0.3333333333333333703, 0.3333333333333333703, 0.3333333333333333703, 0.3333333333333333703, 0.3333333333333333703, 0.3333333333333333703, 0.3333333333333333703, 0.3333333333333333703, 0.3333333333333333703, 0.3333333333333333703, 0.3333333333333333703, 0.3333333333333333703, 0.3333333333333333703, 0.3333333333333333703, 0.3333333333333333703, 0.3333333333333333703, 0.3333333333333333703),
 ( 1.000000000000000000, 1.000000000000000000, 1.000000000000000000, 1.000000000000000000, 1.000000000000000000, 1.000000000000000000, 1.000000000000000000, 1.000000000000000000, 1.000000000000000000, 1.000000000000000000, 1.000000000000000000, 1.000000000000000000, 1.000000000000000000, 1.000000000000000000, 1.000000000000000000, 1.000000000000000000, 1.000000000000000000, 1.000000000000000000),
 ( 0.3333333333333333703, 0.3333333333333333703, 0.3333333333333333703, 0.3333333333333333703, 0.3333333333333333703, 0.3333333333333333703, 0.3333333333333333703, 0.3333333333333333703, 0.3333333333333333703, 0.3333333333333333703, 0.3333333333333333703, 0.3333333333333333703, 0.3333333333333333703, 0.3333333333333333703, 0.3333333333333333703, 0.3333333333333333703, 0.3333333333333333703, 0.3333333333333333703),
 ( 0.3333333333333333703, 0.3333333333333333703, 0.3333333333333333703, 0.3333333333333333703, 0.3333333333333333703, 0.3333333333333333703, 0.3333333333333333703, 0.3333333333333333703, 0.3333333333333333703, 0.3333333333333333703, 0.3333333333333333703, 0.3333333333333333703, 0.3333333333333333703, 0.3333333333333333703, 0.3333333333333333703, 0.3333333333333333703, 0.3333333333333333703, 0.3333333333333333703),
 ( 1.000000000000000000, 1.000000000000000000, 1.000000000000000000, 1.000000000000000000, 1.000000000000000000, 1.000000000000000000, 1.000000000000000000, 1.000000000000000000, 1.000000000000000000, 1.000000000000000000, 1.000000000000000000, 1.000000000000000000, 1.000000000000000000, 1.000000000000000000, 1.000000000000000000, 1.000000000000000000, 1.000000000000000000, 1.000000000000000000) ) ) 
 REPRESENTATION_ITEM ( '' )  SURFACE ( )  );
#156105 = CARTESIAN_POINT ( 'NONE',  ( 0.7499999999999902300, 1.514583334016148086, 1.299038105676657340 ) ) ;
#156106 = CARTESIAN_POINT ( 'NONE',  ( 2.865378420500460432, -1.565876230000915470, -1.097592462808501645 ) ) ;
#156107 = ADVANCED_BREP_SHAPE_REPRESENTATION ( '', ( #85152, #200407 ), #141734 ) ;
#156108 = CARTESIAN_POINT ( 'NONE',  ( -6.067437437315529536, 7.037430750744921859, 1.199719254218450271 ) ) ;
#156109 = CARTESIAN_POINT ( 'NONE',  ( 5.300874872818840622, 6.247070775452521652, 1.082531754730560403 ) ) ;
#156111 = CARTESIAN_POINT ( 'NONE',  ( 6.591443028821331040, -0.4675721919094841250, 2.072835713318227135 ) ) ;
#156110 = CARTESIAN_POINT ( 'NONE',  ( 6.925078400183515726, -0.002206826874838823185, 1.955452213090567160 ) ) ;
#156112 = CARTESIAN_POINT ( 'NONE',  ( -1.364683531250010295, 9.442708333674733723, 0.7879004041258445001 ) ) ;
#156113 = EDGE_CURVE ( 'NONE', #55184, #206199, #105329, .T. ) ;
#156115 = CARTESIAN_POINT ( 'NONE',  ( -6.089547271193396227, 7.133501900260939443, -1.199719254218453823 ) ) ;
#156114 = CARTESIAN_POINT ( 'NONE',  ( 6.093348126157794198, -0.7399906200981146709, 2.062998119606203939 ) ) ;
#156117 = VERTEX_POINT ( 'NONE', #191249 ) ;
#156116 = CARTESIAN_POINT ( 'NONE',  ( 3.100334465813825435, -0.4993057154734497072, -1.650917527159057707 ) ) ;
#156118 = CARTESIAN_POINT ( 'NONE',  ( 6.398696098476772676, -2.079943653215409416, -0.4123558718646391785 ) ) ;
#156119 = CARTESIAN_POINT ( 'NONE',  ( 7.365103760721646076, 9.615707025640515937, 1.599625672291281386 ) ) ;
#156120 = CARTESIAN_POINT ( 'NONE',  ( 5.684946482831785275, 5.526859072925533134, -0.7998128361456231517 ) ) ;
#156121 = FACE_OUTER_BOUND ( 'NONE', #93662, .T. ) ;
#156122 = CARTESIAN_POINT ( 'NONE',  ( 0.1858947801188018389, -1.204007190563995078, -1.549573762531175625 ) ) ;
#156123 =( BOUNDED_SURFACE ( )  B_SPLINE_SURFACE ( 3, 2, ( 
 ( #9588, #11711, #10638 ),
 ( #128756, #95130, #29047 ),
 ( #161179, #12765, #79909 ),
 ( #125562, #78840, #77785 ),
 ( #91939, #142830, #141771 ),
 ( #143906, #209899, #61537 ),
 ( #207779, #93001, #59406 ),
 ( #146017, #62593, #208837 ) ),
 .UNSPECIFIED., .F., .F., .T. ) 
 B_SPLINE_SURFACE_WITH_KNOTS ( ( 4, 2, 2, 4 ),
 ( 3, 3 ),
 ( 0.000000000000000000, 0.003001918495469458117, 0.004502877743204187176, 0.006003836990938916235 ),
 ( 0.000000000000000000, 1.000000000000000000 ),
 .UNSPECIFIED. ) 
 GEOMETRIC_REPRESENTATION_ITEM ( )  RATIONAL_B_SPLINE_SURFACE ( (
 ( 1.000000000000000000, 0.7835651598521251593, 1.000000000000000000),
 ( 1.000000000000000000, 0.7913519369926046432, 1.000000000000000000),
 ( 1.000000000000000000, 0.8009496234817151672, 1.000000000000000000),
 ( 1.000000000000000000, 0.8230981486296959915, 1.000000000000000000),
 ( 1.000000000000000000, 0.8318333311016131715, 1.000000000000000000),
 ( 1.000000000000000000, 0.8529518727576285153, 1.000000000000000000),
 ( 1.000000000000000000, 0.8654984584225093869, 1.000000000000000000),
 ( 1.000000000000000000, 0.8789000212895426989, 1.000000000000000000) ) ) 
 REPRESENTATION_ITEM ( '' )  SURFACE ( )  );
#156124 = CARTESIAN_POINT ( 'NONE',  ( 5.591005849568446706, 5.791977450266268868, -0.7139200525481930182 ) ) ;
#156125 = CARTESIAN_POINT ( 'NONE',  ( 4.143988507271280319, 7.986403691791820414, -0.7998128361456221525 ) ) ;
#156126 = FACE_OUTER_BOUND ( 'NONE', #167467, .T. ) ;
#156127 = EDGE_LOOP ( 'NONE', ( #77056, #153200, #135601, #5439, #123701 ) ) ;
#156128 = CARTESIAN_POINT ( 'NONE',  ( -11.78331023100045627, 13.79999999999999893, -1.800000000000001155 ) ) ;
#156129 = ORIENTED_EDGE ( 'NONE', *, *, #6013, .F. ) ;
#156130 = CARTESIAN_POINT ( 'NONE',  ( 2.965264322261091934, -1.482184020574893069, -1.041122702216127571 ) ) ;
#156131 = VERTEX_POINT ( 'NONE', #42914 ) ;
#156132 = CARTESIAN_POINT ( 'NONE',  ( 8.055515824813896941, 12.54985222892493368, 0.7998128361456462443 ) ) ;
#156133 = CARTESIAN_POINT ( 'NONE',  ( 3.400062661977048428, 7.188766548940353829, -1.734723475976807094E-15 ) ) ;
#156134 = CARTESIAN_POINT ( 'NONE',  ( 3.580526426040127941, -1.214262702978758712, 1.344428254631929276 ) ) ;
#156135 = CARTESIAN_POINT ( 'NONE',  ( 7.824464048418096951, 8.301165276008827476, -0.7216878364870317197 ) ) ;
#156136 = CARTESIAN_POINT ( 'NONE',  ( 0.4019237886466816012, 9.207585450998170273, -1.499999999999998668 ) ) ;
#156137 = CARTESIAN_POINT ( 'NONE',  ( 4.943270704524102221, 6.626842455454077907, 1.245637569283185586 ) ) ;
#156139 = CARTESIAN_POINT ( 'NONE',  ( -0.6823417656250039265, 14.06770833367473195, -1.181850606188755259 ) ) ;
#156138 = CARTESIAN_POINT ( 'NONE',  ( 4.896841239116665356, 0.3175000240179836619, 1.833586397851859839 ) ) ;
#156140 = CARTESIAN_POINT ( 'NONE',  ( 2.794441263998331149, 1.385543030692138133, -1.323043162562879349 ) ) ;
#156141 = CARTESIAN_POINT ( 'NONE',  ( 0.9908991873810431006, 1.612194894691898250, -0.8564790819722142290 ) ) ;
#156142 = CARTESIAN_POINT ( 'NONE',  ( 4.754915986029614849, 8.180161719226850536, 0.7478464228280010673 ) ) ;
#156143 = CARTESIAN_POINT ( 'NONE',  ( -10.78237064342727791, 6.270194388237658956, -4.501389708959286473 ) ) ;
#156144 = AXIS2_PLACEMENT_3D ( 'NONE', #69729, #188838, #139043 ) ;
#156145 = CARTESIAN_POINT ( 'NONE',  ( 5.654245663017247736, 7.339362581565530341, 1.229167601055790815 ) ) ;
#156146 = CARTESIAN_POINT ( 'NONE',  ( -11.48243876534946217, 9.799999999999982947, 3.199999999999997957 ) ) ;
#156147 = CARTESIAN_POINT ( 'NONE',  ( -3.704603422706345572, 7.358260162494655532, -0.4639270913322328105 ) ) ;
#156148 = CARTESIAN_POINT ( 'NONE',  ( 7.100579091573050228, -6.583980363594990948, -6.484567079770450881 ) ) ;
#156149 = CARTESIAN_POINT ( 'NONE',  ( 7.470179451449751262, 7.817556902887268677, 1.040834085586084257E-14 ) ) ;
#156150 = CARTESIAN_POINT ( 'NONE',  ( -4.765854690403601879, 5.518917546014321829, 1.199719254218462483 ) ) ;
#156151 = FACE_OUTER_BOUND ( 'NONE', #95694, .T. ) ;
#156152 = CARTESIAN_POINT ( 'NONE',  ( 1.728581982081365265, 0.2060769881795926906, 2.080452860985905428 ) ) ;
#156153 = CARTESIAN_POINT ( 'NONE',  ( 6.211935731971203190, -1.911736917912661537, 0.2365620046330171311 ) ) ;
#156154 = CARTESIAN_POINT ( 'NONE',  ( -6.552668314106420588, 6.539201209412602189, -0.7998128361456291469 ) ) ;
#156155 = CARTESIAN_POINT ( 'NONE',  ( 2.186296784933777992, -1.789763940591000191, -0.3589617604915079085 ) ) ;
#156156 = CARTESIAN_POINT ( 'NONE',  ( 3.422699507934780616, 1.400174360247144589, -1.705827624971032686 ) ) ;
#156157 = EDGE_CURVE ( 'NONE', #131570, #157711, #188053, .T. ) ;
#156158 = FACE_OUTER_BOUND ( 'NONE', #199234, .T. ) ;
#156159 = CARTESIAN_POINT ( 'NONE',  ( 1.476665317443916603, -1.350161712199383413, 1.354623164920423450 ) ) ;
#156160 = CARTESIAN_POINT ( 'NONE',  ( 1.785543415971390102, -1.855581397249297382, 0.6606886831301524987 ) ) ;
#156161 = CARTESIAN_POINT ( 'NONE',  ( 2.876435298317912004, -0.1456031558026495976, -1.936675272211895837 ) ) ;
#156162 = ORIENTED_EDGE ( 'NONE', *, *, #103675, .T. ) ;
#156163 = DIRECTION ( 'NONE',  ( 0.000000000000000000, -0.3940140829290779689, -0.9191044023687177100 ) ) ;
#156165 = CARTESIAN_POINT ( 'NONE',  ( 6.385601346537729484, -1.752585461374029929, 0.6262014864842447848 ) ) ;
#156164 = CARTESIAN_POINT ( 'NONE',  ( -5.666381855868691808, 5.575476684793721383, 0.000000000000000000 ) ) ;
#156166 = CARTESIAN_POINT ( 'NONE',  ( 4.064412189046650248, 7.963840997188264659, 0.7998128361456271485 ) ) ;
#156167 = FACE_OUTER_BOUND ( 'NONE', #41839, .T. ) ;
#156168 = CARTESIAN_POINT ( 'NONE',  ( 9.748476143425788720, 11.33197590787365172, -1.199719254218440723 ) ) ;
#156169 = CARTESIAN_POINT ( 'NONE',  ( -6.961185525973791144, 7.086080966583015339, 0.7998128361456341429 ) ) ;
#156170 = CARTESIAN_POINT ( 'NONE',  ( 2.683357600500847262, 1.551837136583393839, 1.547750905674146971 ) ) ;
#156171 = FACE_OUTER_BOUND ( 'NONE', #197356, .T. ) ;
#156172 = ORIENTED_EDGE ( 'NONE', *, *, #208381, .F. ) ;
#156173 = AXIS2_PLACEMENT_3D ( 'NONE', #90764, #205541, #56113 ) ;
#156174 = CARTESIAN_POINT ( 'NONE',  ( 5.027041095616958444, 9.086908054853605421, 0.000000000000000000 ) ) ;
#156175 = CARTESIAN_POINT ( 'NONE',  ( -7.065207446497166366, 9.336104335703744539, 0.000000000000000000 ) ) ;
#156176 = CARTESIAN_POINT ( 'NONE',  ( 4.072732355924274295, -1.704239406772959153, -0.6552279023967976235 ) ) ;
#156177 =( LENGTH_UNIT ( ) NAMED_UNIT ( * ) SI_UNIT ( .MILLI., .METRE. ) );
#156178 = CARTESIAN_POINT ( 'NONE',  ( -2.266184231778562541, 5.795632037050281404, 1.040834085586084257E-14 ) ) ;
#156179 =( BOUNDED_CURVE ( )  B_SPLINE_CURVE ( 2, ( #163261, #194675, #112435, #14843, #100377 ),
 .UNSPECIFIED., .F., .T. ) 
 B_SPLINE_CURVE_WITH_KNOTS ( ( 3, 2, 3 ),
 ( 0.5171743412319206312, 0.5250000000000000222, 0.5287935031110296835 ),
 .UNSPECIFIED. ) 
 CURVE ( )  GEOMETRIC_REPRESENTATION_ITEM ( )  RATIONAL_B_SPLINE_CURVE ( ( 0.9846707376464753914, 0.8741872631710951858, 1.000000000000000000, 0.9390120342948788945, 0.9335499976228173180 ) ) 
 REPRESENTATION_ITEM ( '' )  );
#156180 = CARTESIAN_POINT ( 'NONE',  ( -4.839158742459761520, 8.201312040681516535, -0.9517655008395020655 ) ) ;
#156181 = DIRECTION ( 'NONE',  ( -0.000000000000000000, -1.000000000000000000, -0.000000000000000000 ) ) ;
#156182 = CARTESIAN_POINT ( 'NONE',  ( 8.925345196497941558, 9.307324238869423283, 1.040834085586084257E-14 ) ) ;
#156183 = CARTESIAN_POINT ( 'NONE',  ( 2.420428029321282093, 1.258221797421785082, -1.458952285233440449 ) ) ;
#156184 = CARTESIAN_POINT ( 'NONE',  ( 6.526224699197019419, 1.005635830909179074, 1.684226478273798788 ) ) ;
#156185 = EDGE_CURVE ( 'NONE', #168244, #78493, #136548, .T. ) ;
#156186 = CARTESIAN_POINT ( 'NONE',  ( 0.7500000000000006661, 14.41666666666666785, -1.299038105676657340 ) ) ;
#156187 = CARTESIAN_POINT ( 'NONE',  ( -5.201524489137236529, 9.220195670635433771, 0.7998128361456481317 ) ) ;
#156188 = CARTESIAN_POINT ( 'NONE',  ( 3.486418057008484617, 7.219238166485217434, 1.040834085586084257E-14 ) ) ;
#156189 = CARTESIAN_POINT ( 'NONE',  ( -6.102578539482539810, 6.292298848917299736, 0.000000000000000000 ) ) ;
#156190 = CARTESIAN_POINT ( 'NONE',  ( -0.1232448511370512201, -0.4725888426768353190, -2.071762565325820038 ) ) ;
#156191 = CARTESIAN_POINT ( 'NONE',  ( 9.297140650669039275, 11.86975006391249643, 1.599625672291281386 ) ) ;
#156192 = CARTESIAN_POINT ( 'NONE',  ( -1.355395447572484535, 3.935140844187386744, -0.6425755019599873608 ) ) ;
#156193 = CARTESIAN_POINT ( 'NONE',  ( 5.032118066406459533, 1.187563481491529460, 1.695602288408842417 ) ) ;
#156195 = CARTESIAN_POINT ( 'NONE',  ( -1.364683531250012516, 2.842708333674754506, 0.7879004041258379498 ) ) ;
#156194 = CARTESIAN_POINT ( 'NONE',  ( 0.1164230846485321547, -0.09151219166612066525, 1.839079034809627755 ) ) ;
#156196 = ORIENTED_EDGE ( 'NONE', *, *, #56646, .F. ) ;
#156197 = CARTESIAN_POINT ( 'NONE',  ( 5.326872488440856479, 0.9340183262317149904, -2.100526973934746522 ) ) ;
#156198 = CARTESIAN_POINT ( 'NONE',  ( 6.982085921357777281, 7.248114451113292667, 1.040834085586084257E-14 ) ) ;
#156200 = CARTESIAN_POINT ( 'NONE',  ( 1.836970198721030181E-16, 13.49999999999999822, 1.500000000000000222 ) ) ;
#156199 = CARTESIAN_POINT ( 'NONE',  ( 5.750066545971570520, 5.881034856487848295, -0.7216878364870458196 ) ) ;
#156201 = CARTESIAN_POINT ( 'NONE',  ( 0.3754557147975129960, 2.136610487456944263, -0.8307393200860619942 ) ) ;
#156202 = DIRECTION ( 'NONE',  ( -0.5000000000000001110, 0.000000000000000000, 0.8660254037844385966 ) ) ;
#156203 = CARTESIAN_POINT ( 'NONE',  ( -7.747558435566414659, 8.003516027774422170, -0.7998128361456362523 ) ) ;
#156204 = CARTESIAN_POINT ( 'NONE',  ( 4.558499613049934673, -1.735246752265024561, -0.8719658702049468690 ) ) ;
#156205 = VERTEX_POINT ( 'NONE', #8243 ) ;
#156206 = CARTESIAN_POINT ( 'NONE',  ( 7.876924059415351564, 12.13356913605253240, -0.7216878364870267237 ) ) ;
#156207 = EDGE_CURVE ( 'NONE', #69840, #26075, #70789, .T. ) ;
#156208 = ORIENTED_EDGE ( 'NONE', *, *, #62427, .F. ) ;
#156209 = CARTESIAN_POINT ( 'NONE',  ( 6.363533315466952445, -1.540175188624912650, -1.133462061071670579 ) ) ;
#156210 = CARTESIAN_POINT ( 'NONE',  ( 0.2402810872906081530, 0.2891477966728701610, 1.700304936625576024 ) ) ;
#156211 = CARTESIAN_POINT ( 'NONE',  ( 6.227749967195367553, 0.7672974224810540367, -1.865044430435198519 ) ) ;
#156213 = CARTESIAN_POINT ( 'NONE',  ( -1.313174662617493382, 8.310476012147637093, -10.86148356754322819 ) ) ;
#156212 = CARTESIAN_POINT ( 'NONE',  ( -8.642432853707342488, 12.17025653171218558, 1.199719254218462483 ) ) ;
#156214 = CARTESIAN_POINT ( 'NONE',  ( 1.001543065824772753E-15, -0.8093749995220410609, 3.793834371823811669 ) ) ;
#156216 = CARTESIAN_POINT ( 'NONE',  ( 0.6898892245524823608, -1.755727311204742680, -0.2225690630779184609 ) ) ;
#156215 = CARTESIAN_POINT ( 'NONE',  ( 2.976600611693449139, -0.1542612496043833104, -2.085005227243463821 ) ) ;
#156217 = CARTESIAN_POINT ( 'NONE',  ( 0.08053691275167890185, 14.48153890507870223, 11.99972973886013961 ) ) ;
#156219 = CARTESIAN_POINT ( 'NONE',  ( 3.943561162899355654, 0.7735357226616009774, -2.157932208606289759 ) ) ;
#156218 = SURFACE_STYLE_USAGE ( .BOTH. , #204921 ) ;
#156220 = CARTESIAN_POINT ( 'NONE',  ( 2.448798285840974476, 0.4648185774855151942, -1.677030037339591217 ) ) ;
#156221 = CARTESIAN_POINT ( 'NONE',  ( 3.734381245560244089, 6.444196322207211836, 1.199719254218462483 ) ) ;
#156222 = CARTESIAN_POINT ( 'NONE',  ( 0.6124999999999707345, 0.7291666673494984208, -1.060881119635972647 ) ) ;
#156223 = CARTESIAN_POINT ( 'NONE',  ( 1.651252135258261422, -0.2480751513778757522, -1.715843305285965403 ) ) ;
#156224 = CARTESIAN_POINT ( 'NONE',  ( -1.360316468750006669, 2.442708333674733723, 0.7853790794158861388 ) ) ;
#156225 = CARTESIAN_POINT ( 'NONE',  ( 1.855673809551155795, -0.6311025070286357952, 1.750906552266822569 ) ) ;
#156226 = CARTESIAN_POINT ( 'NONE',  ( 2.611994278460927799, 0.5808993838645438723, -2.091943403374715515 ) ) ;
#156227 = CARTESIAN_POINT ( 'NONE',  ( 5.124091990960999432, 8.065525525174782828, -1.199719254218452047 ) ) ;
#156228 = CARTESIAN_POINT ( 'NONE',  ( 3.661342437515973547, 1.897110692972364454, -0.6839366698164971448 ) ) ;
#156229 = CARTESIAN_POINT ( 'NONE',  ( 1.843750000000001332, 1.895863743164127868, 0.7852924748298895086 ) ) ;
#156230 = CARTESIAN_POINT ( 'NONE',  ( 1.499999999999989120, 3.035416667349485564, 0.8660254037844524744 ) ) ;
#156231 = CARTESIAN_POINT ( 'NONE',  ( 0.8856179577424825311, 1.291390466942985649, 1.429610664621896898 ) ) ;
#156232 = CARTESIAN_POINT ( 'NONE',  ( 1.364683531249997417, 13.73437500034139980, 2.602085213965210642E-15 ) ) ;
#156233 = CARTESIAN_POINT ( 'NONE',  ( 4.957398421247804166, -1.904820672624758515, 1.142771788014641743 ) ) ;
#156234 = ORIENTED_EDGE ( 'NONE', *, *, #61552, .F. ) ;
#156235 = CARTESIAN_POINT ( 'NONE',  ( 0.3282377607281116716, 2.488835450998179599, -1.225000000000015410 ) ) ;
#156236 = CARTESIAN_POINT ( 'NONE',  ( 1.499999999999987121, 0.5041666666666856367, 0.8660254037844524744 ) ) ;
#156237 = CARTESIAN_POINT ( 'NONE',  ( 7.613066949273408213, 8.840665181362512115, -1.199719254218441611 ) ) ;
#156238 = CARTESIAN_POINT ( 'NONE',  ( -1.364683531250014514, -0.01145833299191483488, -0.7879004041258359514 ) ) ;
#156239 = CARTESIAN_POINT ( 'NONE',  ( 5.748318879583719010, 1.095320496750437966, -1.932492775422405717 ) ) ;
#156240 = CARTESIAN_POINT ( 'NONE',  ( 4.545333077707183200, 1.753367681936630840, -0.8802267832125689750 ) ) ;
#156241 = CARTESIAN_POINT ( 'NONE',  ( 8.676855123066012254, 11.14608361504227574, -1.443375672974052559 ) ) ;
#156242 = DIRECTION ( 'NONE',  ( 1.000000000000000000, -0.000000000000000000, -0.000000000000000000 ) ) ;
#156243 = CARTESIAN_POINT ( 'NONE',  ( 5.255258077898470326, -1.907309223944063437, -1.216589440439620695 ) ) ;
#156244 = CARTESIAN_POINT ( 'NONE',  ( -6.482206841109545259, 6.735198534148810090, 0.7216878364870257245 ) ) ;
#156245 = CARTESIAN_POINT ( 'NONE',  ( 3.104023224481029519, 0.7448178976848550681, -1.923671348419103921 ) ) ;
#156246 = CARTESIAN_POINT ( 'NONE',  ( -4.557512192488103686, 8.468847991211438497, -0.7998128361456281477 ) ) ;
#156247 = CARTESIAN_POINT ( 'NONE',  ( 0.7499999999999902300, 2.264583334016148530, 1.299038105676669330 ) ) ;
#156248 = CARTESIAN_POINT ( 'NONE',  ( -1.201851678989727383E-14, 5.759375000341417028, -1.575800808251660801 ) ) ;
#156249 = CARTESIAN_POINT ( 'NONE',  ( 5.008994926481016741, 1.626754543590884561, 0.9232732976792232815 ) ) ;
#156250 = CARTESIAN_POINT ( 'NONE',  ( 4.043420308529748652, -1.281227996783333989, 1.168826672502675912 ) ) ;
#156251 = CARTESIAN_POINT ( 'NONE',  ( 2.858654643706417975, 0.2527927160936989659, -1.721832920378673748 ) ) ;
#156252 = CARTESIAN_POINT ( 'NONE',  ( 0.6445460132639491135, 0.6724220840489106843, 2.191533042908066165 ) ) ;
#156253 = CARTESIAN_POINT ( 'NONE',  ( 0.8685540286928781217, 1.089157903960279672, 1.919174906450902274 ) ) ;
#156254 = CARTESIAN_POINT ( 'NONE',  ( 4.370703248089922610, -0.001752428395085294443, -2.090933975693793911 ) ) ;
#156255 = CARTESIAN_POINT ( 'NONE',  ( 5.542900022196344700, -1.532237948119744342, -1.192973588722973100 ) ) ;
#156257 = ORIENTED_EDGE ( 'NONE', *, *, #160015, .T. ) ;
#156256 = CARTESIAN_POINT ( 'NONE',  ( 7.189988563920103104, 15.44736672437920433, 9.558790995692916681 ) ) ;
#156258 = CARTESIAN_POINT ( 'NONE',  ( 0.3697678102792775756, -0.2496098759999023087, -2.000856779379902139 ) ) ;
#156259 = EDGE_CURVE ( 'NONE', #135468, #71711, #56367, .T. ) ;
#156260 = CARTESIAN_POINT ( 'NONE',  ( 0.000000000000000000, -9.746166700180788567, 9.579665964948883783 ) ) ;
#156261 = CARTESIAN_POINT ( 'NONE',  ( 6.522112240665402183, -1.799906897009293738, 0.9091900463213120620 ) ) ;
#156262 = CARTESIAN_POINT ( 'NONE',  ( -10.15235809853472126, 10.73883929124566983, -0.7998128361456291469 ) ) ;
#156263 = CARTESIAN_POINT ( 'NONE',  ( 5.608269097547198712, 9.694731047113750222, -0.7998128361456281477 ) ) ;
#156264 = PRESENTATION_STYLE_ASSIGNMENT (( #141111 ) ) ;
#156265 = CARTESIAN_POINT ( 'NONE',  ( 3.879382553896340013, 1.718498013671100777, -0.6167319420108534622 ) ) ;
#156266 = ORIENTED_EDGE ( 'NONE', *, *, #188595, .F. ) ;
#156267 = CARTESIAN_POINT ( 'NONE',  ( -4.217995187182965289, 6.014356699837137832, 1.443375672974065660 ) ) ;
#156268 = CARTESIAN_POINT ( 'NONE',  ( -3.923105346307911745, 5.670318552149568703, -1.599625672291283607 ) ) ;
#156269 = CARTESIAN_POINT ( 'NONE',  ( -3.285556943750000070, -1.946874999522042682, 0.000000000000000000 ) ) ;
#156270 = CARTESIAN_POINT ( 'NONE',  ( -5.682838942422375084, 9.781729199468104596, 0.000000000000000000 ) ) ;
#156271 = CARTESIAN_POINT ( 'NONE',  ( 2.426041109754235592, -1.997208190617974166, 0.3004318525065238776 ) ) ;
#156272 = CARTESIAN_POINT ( 'NONE',  ( -4.176793841461789114, 7.030620694084159794, -1.199719254218455378 ) ) ;
#156273 = CARTESIAN_POINT ( 'NONE',  ( 3.432308073483012922, -1.112138214925220803, 1.491878268611693814 ) ) ;
#156274 = CARTESIAN_POINT ( 'NONE',  ( 8.353795204314554468, 12.89784483834236184, -0.7998128361456352531 ) ) ;
#156275 = FACE_OUTER_BOUND ( 'NONE', #12368, .T. ) ;
#156276 = EDGE_LOOP ( 'NONE', ( #132069, #33372, #98820, #47485, #179907, #90324, #127529, #186353, #24470, #98614, #141163, #134995, #131880, #49210, #48927, #38609, #47087, #94505, #42225, #151703, #209664 ) ) ;
#156277 = CARTESIAN_POINT ( 'NONE',  ( -4.904298879841297421, 6.744767997946721216, 1.599625672291267398 ) ) ;
#156278 = CARTESIAN_POINT ( 'NONE',  ( -9.494787648271923786, 9.971673765939062406, 1.040834085586084257E-14 ) ) ;
#156279 = CARTESIAN_POINT ( 'NONE',  ( 5.338443970399977978, 1.799313579390570128, 0.3082849261525285600 ) ) ;
#156281 = CARTESIAN_POINT ( 'NONE',  ( -4.597746731904842399, 7.146551969360384504, -1.363588915232381904 ) ) ;
#156280 = CARTESIAN_POINT ( 'NONE',  ( -3.006876207180748217, 6.730049018344652190, -0.7998128361456481317 ) ) ;
#156282 = CARTESIAN_POINT ( 'NONE',  ( 6.374094191309353619, 6.920300110170956032, -0.8184029421815092187 ) ) ;
#156283 = CARTESIAN_POINT ( 'NONE',  ( 0.6317059331818836165, 0.1778517408326604765, -1.724704385026996079 ) ) ;
#156284 = CARTESIAN_POINT ( 'NONE',  ( 6.703072984701052839, -0.3981723446819797063, 1.804146177254343009 ) ) ;
#156285 = CARTESIAN_POINT ( 'NONE',  ( 5.198025161738785371, -0.8347013672818380803, 2.151627338387426036 ) ) ;
#156286 = CARTESIAN_POINT ( 'NONE',  ( 3.366167277942881064, 7.149221934233827014, -0.7998128361456362523 ) ) ;
#156287 = CARTESIAN_POINT ( 'NONE',  ( 0.3157904346527000139, -2.021491663516309156, 0.3995350904514202162 ) ) ;
#156288 = CARTESIAN_POINT ( 'NONE',  ( 6.505214776458575265, 6.483838748823460563, 1.040834085586084257E-14 ) ) ;
#156289 = CARTESIAN_POINT ( 'NONE',  ( 5.800273438847154850, -2.081326394616866970, 0.9752826944557994038 ) ) ;
#156290 = CARTESIAN_POINT ( 'NONE',  ( 4.222669843016475966, 3.519858668466393947, 2.499999999999998668 ) ) ;
#156291 = CARTESIAN_POINT ( 'NONE',  ( -5.399890319992785237, 9.521898816625391504, 0.7998128361456291469 ) ) ;
#156292 = CARTESIAN_POINT ( 'NONE',  ( 5.260568668178753349, -1.354309965608934352, 1.290672426560689035 ) ) ;
#156293 = B_SPLINE_CURVE_WITH_KNOTS ( 'NONE', 3,
 ( #95303, #161352, #146183, #63835 ),
 .UNSPECIFIED., .F., .F.,
 ( 4, 4 ),
 ( 0.7146167707638562128, 1.000000000000000000 ),
 .UNSPECIFIED. ) ;
#156295 = CARTESIAN_POINT ( 'NONE',  ( -4.767627293860968507, 5.591261926706423857, -1.199719254218453823 ) ) ;
#156294 = CARTESIAN_POINT ( 'NONE',  ( 3.515784362865181478, -0.5505564139345071606, 1.831456330389509501 ) ) ;
#156296 = CARTESIAN_POINT ( 'NONE',  ( 4.846401659255799466, 2.200796399388889935, 0.1645688927329121420 ) ) ;
#156297 = CARTESIAN_POINT ( 'NONE',  ( 4.329393036353162749, -1.639139883998712799, -1.340335314225228780 ) ) ;
#156298 = CARTESIAN_POINT ( 'NONE',  ( -1.552391752028397856E-14, 0.5000000006828063670, -1.414508159514587415 ) ) ;
#156299 = EDGE_CURVE ( 'NONE', #168810, #135502, #64035, .T. ) ;
#156300 = CARTESIAN_POINT ( 'NONE',  ( 6.983263157960404754, 0.5693283498368858497, 2.097578288773850552 ) ) ;
#156301 = CARTESIAN_POINT ( 'NONE',  ( 4.706088717274885092, 8.504537580213796133, 0.7216878364870317197 ) ) ;
#156302 = CARTESIAN_POINT ( 'NONE',  ( -5.926322542504884439, 6.086666852443364029, -0.7216878364870338292 ) ) ;
#156303 = CARTESIAN_POINT ( 'NONE',  ( 5.391314312714450274, -0.05227466736787074464, -2.120015263102632552 ) ) ;
#156304 = CARTESIAN_POINT ( 'NONE',  ( 2.063905019644726835, 0.3937302209732340685, -2.273608288252434662 ) ) ;
#156305 = CARTESIAN_POINT ( 'NONE',  ( 3.631260574587381829, 0.05062604155347744800, -1.961386756325018021 ) ) ;
#156306 = CARTESIAN_POINT ( 'NONE',  ( 6.977413162628444354, -0.1478290182607009950, 2.029965231729473185 ) ) ;
#156307 = CARTESIAN_POINT ( 'NONE',  ( 3.958617665510264949, 5.641473247893851628, -1.443375672974051449 ) ) ;
#156308 = CARTESIAN_POINT ( 'NONE',  ( 2.905190055078214595, 6.611415174225076186, 0.7998128361456271485 ) ) ;
#156309 = ORIENTED_EDGE ( 'NONE', *, *, #172591, .F. ) ;
#156310 = CARTESIAN_POINT ( 'NONE',  ( 5.331267653506235327, -1.592659417495114083, -1.236803018183525449 ) ) ;
#156311 = CARTESIAN_POINT ( 'NONE',  ( -8.622095623286845978, 12.14652976288826913, 1.199719254218462483 ) ) ;
#156312 = CARTESIAN_POINT ( 'NONE',  ( -15.75000000000000000, 10.90000000000000036, -1.100000000000002087 ) ) ;
#156313 = CARTESIAN_POINT ( 'NONE',  ( -0.2408018239684095729, -0.007136184528808943960, -2.100252307185761058 ) ) ;
#156314 = CARTESIAN_POINT ( 'NONE',  ( 1.604584692665763423, 2.168457688117795712, 0.1093331725631509210 ) ) ;
#156315 = CARTESIAN_POINT ( 'NONE',  ( 3.811250579217332568, 5.539821323877241355, 1.214306433183764966E-14 ) ) ;
#156316 = EDGE_CURVE ( 'NONE', #171070, #56380, #188314, .T. ) ;
#156317 = CARTESIAN_POINT ( 'NONE',  ( -1.500000000000013101, 0.7020833340161545255, 0.8660254037844403729 ) ) ;
#156318 = CARTESIAN_POINT ( 'NONE',  ( -0.8956962585354001360, 14.55305237108631466, -11.95586207031294101 ) ) ;
#156319 = CARTESIAN_POINT ( 'NONE',  ( 2.535011536075336913, 5.133042487381361596, -7.499999999999997335 ) ) ;
#156320 = CARTESIAN_POINT ( 'NONE',  ( 5.950060389077887812, 7.221515259811701171, 1.225279837341096689 ) ) ;
#156321 = CARTESIAN_POINT ( 'NONE',  ( 1.071639231386111391, 1.986785141929363618, -0.5470796107636519690 ) ) ;
#156322 = CIRCLE ( 'NONE', #62915, 11.09999999999999964 ) ;
#156324 = CARTESIAN_POINT ( 'NONE',  ( 6.727182134110196721, 2.084960209934753284, 2.120171393779949565 ) ) ;
#156323 = CARTESIAN_POINT ( 'NONE',  ( -8.859363311525973117, 12.42334206583395328, -1.199719254218446718 ) ) ;
#156325 = CARTESIAN_POINT ( 'NONE',  ( 0.6823417656249882723, 0.4260416670080896528, -1.181850606188749264 ) ) ;
#156326 = DIRECTION ( 'NONE',  ( 0.000000000000000000, 0.000000000000000000, -1.000000000000000000 ) ) ;
#156327 = ORIENTED_EDGE ( 'NONE', *, *, #190484, .T. ) ;
#156328 = CARTESIAN_POINT ( 'NONE',  ( 3.299369280271017946, 1.727720890571235124, -0.8199460011262191816 ) ) ;
#156329 = CARTESIAN_POINT ( 'NONE',  ( 5.436323762753620947, 1.744125921451036065, 0.2996227856876289564 ) ) ;
#156330 = CARTESIAN_POINT ( 'NONE',  ( 6.886615681098613884, 6.999082814228660077, 0.000000000000000000 ) ) ;
#156331 = CARTESIAN_POINT ( 'NONE',  ( -5.427341564172148303, 5.226320001155936090, 0.000000000000000000 ) ) ;
#156332 = CARTESIAN_POINT ( 'NONE',  ( 0.03503794071320948805, -0.08894543905034424380, 1.809493548878613023 ) ) ;
#156333 = CARTESIAN_POINT ( 'NONE',  ( 6.274997412412571585, 1.664062557780759066, -0.9488046768871650771 ) ) ;
#156334 = CARTESIAN_POINT ( 'NONE',  ( 1.499999999999987121, 0.004166666666691258049, 0.8660254037844524744 ) ) ;
#156335 = CARTESIAN_POINT ( 'NONE',  ( 0.5552397518338060278, 1.722184604005328357, -1.148819969904082861 ) ) ;
#156336 = CARTESIAN_POINT ( 'NONE',  ( 0.6823417656249864960, -0.7614583329919113464, -1.181850606188749264 ) ) ;
#156337 = COLOUR_RGB ( '', 0.66274510, 0.83137255, 0.94901961) ;
#156338 = CARTESIAN_POINT ( 'NONE',  ( 5.735183426005796115, -1.690533149647139410, 0.8011652756413772947 ) ) ;
#156339 = CARTESIAN_POINT ( 'NONE',  ( 3.017977635683791071, -0.9002817137206723386, -1.588204215665294461 ) ) ;
#156341 = CARTESIAN_POINT ( 'NONE',  ( 6.491225937077876651, 6.748298437306541331, 0.07656069123261090292 ) ) ;
#156340 = CARTESIAN_POINT ( 'NONE',  ( 6.111994396789379280, -2.190734547077430872, 0.2660306753756238041 ) ) ;
#156342 = CARTESIAN_POINT ( 'NONE',  ( -1.402160292154681736E-14, -0.1781249996585796136, 1.575800808251672791 ) ) ;
#156343 = CARTESIAN_POINT ( 'NONE',  ( 2.945816691342293847, 1.456820166381930015, 1.460492231956188824 ) ) ;
#156344 = CARTESIAN_POINT ( 'NONE',  ( -7.202405917357668663, 9.425892875049191488, 1.599625672291295375 ) ) ;
#156345 = CARTESIAN_POINT ( 'NONE',  ( 7.716561984472250835, 12.15440608185967086, 1.040834085586084257E-14 ) ) ;
#156346 = CARTESIAN_POINT ( 'NONE',  ( 4.761938266897790761, 6.578680616179307883, 1.599625672291267175 ) ) ;
#156347 = EDGE_CURVE ( 'NONE', #33705, #82863, #191867, .T. ) ;
#156348 = CARTESIAN_POINT ( 'NONE',  ( -0.07804503809600779607, -9.997560133496188328, -10.91958144425261423 ) ) ;
#156349 = CARTESIAN_POINT ( 'NONE',  ( 6.619590326553026038, 0.3579758704960536719, -2.039031579972025554 ) ) ;
#156350 = CARTESIAN_POINT ( 'NONE',  ( -1.402160292154681736E-14, -0.4906249996585810846, -1.575800808251665908 ) ) ;
#156351 = CARTESIAN_POINT ( 'NONE',  ( 3.901784996602038813, -0.6316019492740264640, 2.067237329103743804 ) ) ;
#156353 = CARTESIAN_POINT ( 'NONE',  ( 2.348037267531626338, -0.8415878996531295231, 1.772339229757218471 ) ) ;
#156352 = CARTESIAN_POINT ( 'NONE',  ( 4.195966715351859833, 1.320990344651201021, 1.527833845825769643 ) ) ;
#156354 = CARTESIAN_POINT ( 'NONE',  ( 6.620655732516668834, 6.034240673559561507, 2.768629221164942145 ) ) ;
#156357 = CARTESIAN_POINT ( 'NONE',  ( 5.165293337126522388, 8.969999960048859577, 1.040834085586084257E-14 ) ) ;
#156356 = CARTESIAN_POINT ( 'NONE',  ( 1.001543065824772753E-15, -0.2624999999999988454, 4.012584370867899430 ) ) ;
#156355 = CARTESIAN_POINT ( 'NONE',  ( -1.162044386198238837E-16, 1.437500000000019540, -1.225000000000020739 ) ) ;
#156358 = CARTESIAN_POINT ( 'NONE',  ( -6.257970421159510188, 9.458660037064859694, 1.199719254218452047 ) ) ;
#156359 = CARTESIAN_POINT ( 'NONE',  ( 2.518767860054324625, 0.2516336668320385828, 2.000731427934741902 ) ) ;
#156360 = CARTESIAN_POINT ( 'NONE',  ( -5.525111292768871252, 6.404716915440499037, -1.199719254218446718 ) ) ;
#156361 =( BOUNDED_SURFACE ( )  B_SPLINE_SURFACE ( 1, 2, ( 
 ( #158908, #125416, #74456, #108087, #159972, #191382, #208699, #60326, #126487, #192450, #176233, #27835, #93931, #79779, #48376, #97130, #114488, #127567, #211902, #113427, #61404, #131779, #180485, #112357, #164237, #193536, #32104, #214008, #96064, #161041, #162116, #145891, #49420, #14767, #165293, #45178, #77647, #130742, #163182, #65631, #33163, #31054, #15825, #98189, #115540, #196735, #80858, #81910, #146948, #63539, #13706, #129694, #181535, #111291, #195677, #197782, #144833, #47313, #177296, #179433, #212963, #143769, #147998, #64601, #99244, #194596, #209763, #29978, #28910, #94995, #12636, #78707, #210841, #62467, #128629, #46240, #178370, #17949, #199909, #116602, #104574, #120892, #100292, #50482, #202017, #69892, #117681, #16887, #149042, #184720, #183673, #36344, #166359, #198836, #151189, #182596, #617, #20090, #168490, #102422, #169558, #38496, #4884, #137072, #84036, #136004, #82969, #34219, #66685, #21140, #53676, #186866, #86177, #87243, #152247, #1698, #132832, #67752, #119808, #101354, #54742, #3820, #85104, #150125, #19024, #185787, #37421, #103497, #133902, #2761, #52607, #51555, #70962, #153309, #35277, #203097, #167432, #68830, #134952, #200960, #118736, #14765, #50479, #147996, #113425, #163180, #112355, #132830, #78705, #198834, #194594, #15823, #179431, #130740, #80855, #97128, #63537, #98187, #149040, #146946, #62465, #165291, #34217, #16885, #615, #31052, #196733, #81908, #128627, #96061, #131777, #48374, #114486, #180483, #32102, #46238, #164235, #129692, #47311, #115538, #66683, #100290, #64599, #99242, #212961, #195675, #116600, #65628, #82967, #214006, #211900, #197780, #182594, #49418, #13704, #181533, #12634, #178368, #29976, #144831, #162114, #33161, #210839, #79777, #145889, #151188, #4882, #134951, #119807, #154382, #133900, #137071, #51553, #17947, #199907, #52606, #2760, #118735, #68829, #67750, #37420, #84034, #103496, #70961, #168489, #39558, #150123, #54741, #120891, #138142, #184719, #69890, #117678, #36343, #152246, #86176, #102421, #203096, #38495, #200958, #186865, #167431, #136003, #20088, #166357, #3819, #202016, #19023, #53675, #72030, #85103, #185786, #1696, #169557, #104573, #21139, #87242, #5959, #170618, #22205, #153307, #88318, #204151, #55807, #121961, #187928, #183671, #35274, #101352, #205236, #109971, #56877, #107833, #173858, #42792, #25434, #90461, #158654, #74206, #59011, #93673, #73105, #76328, #123053, #171687, #139206, #206319, #156527, #57943, #8118, #7029, #191126, #23284, #108901, #10252, #91540, #193278, #89396, #208442, #60076, #77392, #124108, #9194, #189004, #190071, #157599, #75265, #41723, #142434, #192193, #140300, #126232, #106750, #141379, #207390, #105659, #125167, #174924, #172777, #26504, #11314, #24351, #92611, #43857, #175982, #40647, #27575, #159716, #143508, #209505, #61145, #127307, #155444, #79531, #197532, #160786, #62221, #78459, #96878, #12379, #47055, #82719, #180238, #145649, #195425, #144577, #165042, #111031, #16635, #210591, #48128, #211645, #162928, #113171, #129442, #95809, #130499, #181285, #179175, #94740, #49177, #66439, #115294, #32912, #63280, #14509, #114240, #128378, #194346, #163995, #80600, #146696, #212712, #64353, #45987, #196486, #161865, #30799, #147744, #98989, #31862, #97937, #148796, #132581, #366, #44923, #112108, #15570, #177036, #178111, #28653, #29727, #81657, #13455, #213760, #65383, #131529, #183420, #33968, #35023, #169307, #68580, #21950, #3573, #52362, #83781, #201778, #53418, #202846, #102175, #153059, #85927, #117423, #168242, #5702, #101095, #71779, #100045, #200711, #19841, #198584, #50230, #119555, #118491, #20892, #69646, #86988, #166108, #184474, #152001, #182340, #38243, #4634, #18770, #70706, #17694, #136819, #120639, #2507, #67505, #84854, #185541, #116350, #149873, #1441, #133652, #199652, #37169, #135755, #186617, #154132, #103247, #54495, #104317, #88060, #170367, #51298, #167181, #150944, #36091, #134706, #156274, #27314, #171441, #123854, #59824, #204985, #7858, #23031, #189818, #25184, #203914, #208191, #140038, #26244, #40392, #175722, #90210, #92363, #73943, #91285 ),
 ( #190874, #24107, #137895, #55561, #157344, #206062, #8933, #72856, #105403, #57697, #89146, #121716, #141123, #41468, #187680, #39308, #75013, #107577, #207134, #138963, #155200, #173611, #6781, #56630, #58759, #124911, #42540, #76075, #159456, #125977, #43598, #122795, #108643, #188753, #106496, #11055, #142175, #174671, #93419, #158400, #191934, #9998, #172522, #109717, #61963, #47873, #161609, #115037, #96620, #145393, #176776, #80339, #146439, #81405, #195166, #31602, #178925, #210326, #46801, #98730, #128120, #164788, #193009, #79275, #112914, #77135, #143256, #212452, #211391, #113984, #162674, #179981, #127049, #63020, #30540, #60889, #131289, #97678, #111851, #163736, #44662, #15317, #213510, #95558, #160525, #177855, #64096, #209245, #110776, #28392, #94487, #12130, #130238, #14244, #65131, #32652, #196231, #147488, #197276, #181036, #48916, #78202, #144327, #194080, #129188, #13199, #45733, #29467, #49972, #2251, #152803, #83525, #100844, #116091, #68327, #118235, #82459, #86733, #18523, #119298, #133389, #54242, #183167, #185284, #34771, #184220, #101921, #166930, #102989, #69391, #200461, #199395, #17441, #51041, #182082, #104062, #120380, #99790, #33713, #201522, #135499, #84601, #1190, #53170, #117164, #35842, #4382, #198332, #36907, #165856, #148548, #149608, #150689, #67254, #134458, #52107, #132327, #167987, #114, #19592, #169047, #85665, #16380, #66181, #20644, #70454, #202590, #151751, #3322, #136569, #186355, #37990, #89959, #40129, #206874, #42275, #154944, #124660, #171183, #73683, #23852, #170109, #156010, #106239, #22773, #122536, #75819, #88890, #6528, #188497, #172265, #203658, #72605, #140860, #204722, #7598, #139781, #207939, #187428, #56373, #108389, #71528, #39057, #55308, #205808, #137639, #57439, #59561, #91026, #123600, #189565, #121457, #141927, #21696, #125721, #105143, #173341, #41210, #107317, #24921, #157087, #138705, #8676, #92098, #74758, #5449, #174413, #191681, #25990, #158152, #58505, #190617, #9745, #43342, #87807, #153880, #79010, #145126, #62756, #128916, #142995, #194897, #160269, #144069, #212195, #163477, #197027, #161348, #195979, #45470, #77948, #15059, #162417, #47612, #12929, #94231, #96363, #213264, #112656, #110524, #178665, #109462, #60629, #208993, #113726, #126792, #111587, #177597, #46535, #127872, #64891, #192747, #95299, #31349, #176524, #193822, #44404, #211132, #30277, #175469, #179730, #29209, #63833, #11871, #147236, #61704, #129991, #13994, #80078, #146180, #97423, #81151, #131038, #27055, #210064, #28135, #93162, #159199, #10800, #76874, #134987, #82204, #22243, #104609, #152283, #48664, #180778, #4918, #3856, #70995, #200997, #16121, #185824, #148298, #32404, #54779, #203137, #137108, #204187, #73137, #39593, #171723, #52642, #170656, #114780, #214295, #139242, #55843, #88353, #7064, #120926, #121999, #186899, #36383, #98470, #102461, #154418, #136041, #89430, #38531, #119846, #68867, #5996, #72067, #187965, #169594, #138177, #153348, #184756, #21176, #164535, #168527, #118772, #20125, #53713, #87279, #86211, #69929, #105696, #37455, #23322, #155481, #202053, #103534, #125197, #26536, #189043, #44955, #176015, #25468, #77426, #40680, #159747, #127339, #9226, #74238, #91576, #126268, #12411, #205273, #78491, #106783, #56913, #43888, #10284, #193309, #160819, #158686, #143543, #93707, #28685, #110002, #142465, #27607, #76358, #191160, #75298, #11345, #208473, #209537, #60109, #42827, #141413, #207420, #94771, #24383, #108933, #111063, #57977, #59039, #90496, #174954, #92644, #123086, #61179, #192225, #177069, #107867, #172811, #157628, #156559, #8154, #140331, #206350, #124140, #190102, #41755, #173893, #47085, #145679, #113203, #29757, #17724, #34001, #13485, #178143, #115328, #197564, #30833, #144608, #62249, #97970, #96909, #164029, #79560, #112139, #64381, #95842, #128410, #147775, #81691, #15604, #82753, #166137, #132611, #50265, #211677, #49208, #210623, #161898, #194377, #148826, #181319, #100075, #213791, #399, #65414, #129474, #46020, #195456, #32947, #14540, #182372, #131563, #212747, #63313, #99021, #165078, #66470, #48160, #16669 ) ),
 .UNSPECIFIED., .F., .F., .F. ) 
 B_SPLINE_SURFACE_WITH_KNOTS ( ( 2, 2 ),
 ( 3, 2, 2, 2, 2, 2, 2, 2, 2, 2, 2, 2, 2, 2, 2, 2, 2, 2, 2, 2, 2, 2, 2, 2, 2, 2, 2, 2, 2, 2, 2, 2, 2, 2, 2, 2, 2, 2, 2, 2, 2, 2, 2, 2, 2, 2, 2, 2, 2, 2, 2, 2, 2, 2, 2, 2, 2, 2, 2, 2, 2, 2, 2, 2, 2, 2, 2, 2, 2, 2, 2, 2, 2, 2, 2, 2, 2, 2, 2, 2, 2, 2, 2, 2, 2, 2, 2, 2, 2, 2, 2, 2, 2, 2, 2, 2, 2, 2, 2, 2, 2, 2, 2, 2, 2, 2, 2, 2, 2, 2, 2, 2, 2, 2, 2, 2, 2, 2, 2, 2, 2, 2, 2, 2, 2, 2, 2, 2, 2, 2, 2, 2, 2, 2, 2, 2, 2, 2, 2, 2, 2, 2, 2, 2, 2, 2, 2, 2, 2, 2, 2, 2, 2, 2, 2, 2, 2, 2, 2, 2, 2, 2, 2, 2, 2, 2, 2, 2, 2, 2, 2, 2, 2, 2, 2, 2, 2, 2, 2, 2, 2, 2, 2, 2, 2, 2, 2, 2, 2, 2, 2, 2, 2, 2, 2, 2, 2, 2, 2, 2, 2, 2, 2, 2, 2, 2, 2, 2, 2, 2, 2, 2, 2, 2, 2, 2, 2, 2, 2, 2, 2, 2, 2, 2, 2, 2, 2, 2, 2, 2, 2, 2, 2, 2, 2, 2, 2, 2, 2, 2, 3 ),
 ( 0.000000000000000000, 1.000000000000000000 ),
 ( 0.000000000000000000, 0.004166666666666666609, 0.008333333333333333218, 0.01250000000000000069, 0.01666666666666666644, 0.02083333333333333218, 0.02500000000000000139, 0.02916666666666666713, 0.03333333333333333287, 0.03749999999999999861, 0.04166666666666666435, 0.04583333333333333010, 0.05000000000000000278, 0.05416666666666666852, 0.05833333333333333426, 0.06250000000000000000, 0.06666666666666666574, 0.07083333333333333148, 0.07499999999999999722, 0.07916666666666666297, 0.08333333333333332871, 0.08749999999999999445, 0.09166666666666666019, 0.09583333333333333981, 0.1000000000000000056, 0.1041666666666666713, 0.1083333333333333370, 0.1125000000000000028, 0.1166666666666666685, 0.1208333333333333343, 0.1250000000000000000, 0.1291666666666666796, 0.1333333333333333315, 0.1375000000000000111, 0.1416666666666666630, 0.1458333333333333426, 0.1499999999999999944, 0.1541666666666666741, 0.1583333333333333259, 0.1625000000000000056, 0.1666666666666666574, 0.1708333333333333370, 0.1749999999999999889, 0.1791666666666666685, 0.1833333333333333204, 0.1875000000000000000, 0.1916666666666666796, 0.1958333333333333315, 0.2000000000000000111, 0.2041666666666666630, 0.2083333333333333426, 0.2124999999999999944, 0.2166666666666666741, 0.2208333333333333259, 0.2250000000000000056, 0.2291666666666666574, 0.2333333333333333370, 0.2374999999999999889, 0.2416666666666666685, 0.2458333333333333204, 0.2500000000000000000, 0.2541666666666666519, 0.2583333333333333592, 0.2625000000000000111, 0.2666666666666666630, 0.2708333333333333148, 0.2750000000000000222, 0.2791666666666666741, 0.2833333333333333259, 0.2874999999999999778, 0.2916666666666666852, 0.2958333333333333370, 0.2999999999999999889, 0.3041666666666666408, 0.3083333333333333481, 0.3125000000000000000, 0.3166666666666666519, 0.3208333333333333592, 0.3250000000000000111, 0.3291666666666666630, 0.3333333333333333148, 0.3375000000000000222, 0.3416666666666666741, 0.3458333333333333259, 0.3499999999999999778, 0.3541666666666666852, 0.3583333333333333370, 0.3624999999999999889, 0.3666666666666666408, 0.3708333333333333481, 0.3750000000000000000, 0.3791666666666666519, 0.3833333333333333592, 0.3875000000000000111, 0.3916666666666666630, 0.3958333333333333148, 0.4000000000000000222, 0.4041666666666666741, 0.4083333333333333259, 0.4124999999999999778, 0.4166666666666666852, 0.4208333333333333370, 0.4249999999999999889, 0.4291666666666666408, 0.4333333333333333481, 0.4375000000000000000, 0.4416666666666666519, 0.4458333333333333592, 0.4500000000000000111, 0.4541666666666666630, 0.4583333333333333148, 0.4625000000000000222, 0.4666666666666666741, 0.4708333333333333259, 0.4749999999999999778, 0.4791666666666666852, 0.4833333333333333370, 0.4874999999999999889, 0.4916666666666666408, 0.4958333333333333481, 0.5000000000000000000, 0.5041666666666666519, 0.5083333333333333037, 0.5124999999999999556, 0.5166666666666667185, 0.5208333333333333703, 0.5250000000000000222, 0.5291666666666666741, 0.5333333333333333259, 0.5374999999999999778, 0.5416666666666666297, 0.5458333333333332815, 0.5500000000000000444, 0.5541666666666666963, 0.5583333333333333481, 0.5625000000000000000, 0.5666666666666666519, 0.5708333333333333037, 0.5749999999999999556, 0.5791666666666667185, 0.5833333333333333703, 0.5875000000000000222, 0.5916666666666666741, 0.5958333333333333259, 0.5999999999999999778, 0.6041666666666666297, 0.6083333333333332815, 0.6125000000000000444, 0.6166666666666666963, 0.6208333333333333481, 0.6250000000000000000, 0.6291666666666666519, 0.6333333333333333037, 0.6374999999999999556, 0.6416666666666667185, 0.6458333333333333703, 0.6500000000000000222, 0.6541666666666666741, 0.6583333333333333259, 0.6624999999999999778, 0.6666666666666666297, 0.6708333333333332815, 0.6750000000000000444, 0.6791666666666666963, 0.6833333333333333481, 0.6875000000000000000, 0.6916666666666666519, 0.6958333333333333037, 0.6999999999999999556, 0.7041666666666667185, 0.7083333333333333703, 0.7125000000000000222, 0.7166666666666666741, 0.7208333333333333259, 0.7249999999999999778, 0.7291666666666666297, 0.7333333333333332815, 0.7375000000000000444, 0.7416666666666666963, 0.7458333333333333481, 0.7500000000000000000, 0.7541666666666666519, 0.7583333333333333037, 0.7624999999999999556, 0.7666666666666667185, 0.7708333333333333703, 0.7750000000000000222, 0.7791666666666666741, 0.7833333333333333259, 0.7874999999999999778, 0.7916666666666666297, 0.7958333333333332815, 0.8000000000000000444, 0.8041666666666666963, 0.8083333333333333481, 0.8125000000000000000, 0.8166666666666666519, 0.8208333333333333037, 0.8249999999999999556, 0.8291666666666667185, 0.8333333333333333703, 0.8375000000000000222, 0.8416666666666666741, 0.8458333333333333259, 0.8499999999999999778, 0.8541666666666666297, 0.8583333333333332815, 0.8625000000000000444, 0.8666666666666666963, 0.8708333333333333481, 0.8750000000000000000, 0.8791666666666666519, 0.8833333333333333037, 0.8874999999999999556, 0.8916666666666667185, 0.8958333333333333703, 0.9000000000000000222, 0.9041666666666666741, 0.9083333333333333259, 0.9124999999999999778, 0.9166666666666666297, 0.9208333333333332815, 0.9250000000000000444, 0.9291666666666666963, 0.9333333333333333481, 0.9375000000000000000, 0.9416666666666666519, 0.9458333333333333037, 0.9499999999999999556, 0.9541666666666667185, 0.9583333333333333703, 0.9625000000000000222, 0.9666666666666666741, 0.9708333333333333259, 0.9749999999999999778, 0.9791666666666666297, 0.9833333333333332815, 0.9875000000000000444, 0.9916666666666666963, 0.9958333333333333481, 1.000000000000000000 ),
 .UNSPECIFIED. ) 
 GEOMETRIC_REPRESENTATION_ITEM ( )  RATIONAL_B_SPLINE_SURFACE ( (
 ( 1.000000000000000000, 0.8660254037844387076, 1.000000000000000000, 0.8660254037844387076, 1.000000000000000000, 0.8660254037844387076, 1.000000000000000000, 0.8660254037844387076, 1.000000000000000000, 0.8660254037844387076, 1.000000000000000000, 0.8660254037844387076, 1.000000000000000000, 0.8660254037844387076, 1.000000000000000000, 0.8660254037844387076, 1.000000000000000000, 0.8660254037844387076, 1.000000000000000000, 0.8660254037844387076, 1.000000000000000000, 0.8660254037844387076, 1.000000000000000000, 0.8660254037844387076, 1.000000000000000000, 0.8660254037844387076, 1.000000000000000000, 0.8660254037844387076, 1.000000000000000000, 0.8660254037844387076, 1.000000000000000000, 0.8660254037844387076, 1.000000000000000000, 0.8660254037844387076, 1.000000000000000000, 0.8660254037844387076, 1.000000000000000000, 0.8660254037844387076, 1.000000000000000000, 0.8660254037844387076, 1.000000000000000000, 0.8660254037844387076, 1.000000000000000000, 0.8660254037844387076, 1.000000000000000000, 0.8660254037844387076, 1.000000000000000000, 0.8660254037844387076, 1.000000000000000000, 0.8660254037844387076, 1.000000000000000000, 0.8660254037844387076, 1.000000000000000000, 0.8660254037844387076, 1.000000000000000000, 0.8660254037844387076, 1.000000000000000000, 0.8660254037844387076, 1.000000000000000000, 0.8660254037844387076, 1.000000000000000000, 0.8660254037844387076, 1.000000000000000000, 0.8660254037844387076, 1.000000000000000000, 0.8660254037844387076, 1.000000000000000000, 0.8660254037844387076, 1.000000000000000000, 0.8660254037844387076, 1.000000000000000000, 0.8660254037844387076, 1.000000000000000000, 0.8660254037844387076, 1.000000000000000000, 0.8660254037844387076, 1.000000000000000000, 0.8660254037844387076, 1.000000000000000000, 0.8660254037844387076, 1.000000000000000000, 0.8660254037844387076, 1.000000000000000000, 0.8660254037844387076, 1.000000000000000000, 0.8660254037844387076, 1.000000000000000000, 0.8660254037844387076, 1.000000000000000000, 0.8660254037844387076, 1.000000000000000000, 0.8660254037844387076, 1.000000000000000000, 0.8660254037844387076, 1.000000000000000000, 0.8660254037844387076, 1.000000000000000000, 0.8660254037844387076, 1.000000000000000000, 0.8660254037844387076, 1.000000000000000000, 0.8660254037844387076, 1.000000000000000000, 0.8660254037844387076, 1.000000000000000000, 0.8660254037844387076, 1.000000000000000000, 0.8660254037844387076, 1.000000000000000000, 0.8660254037844387076, 1.000000000000000000, 0.8660254037844387076, 1.000000000000000000, 0.8660254037844387076, 1.000000000000000000, 0.8660254037844387076, 1.000000000000000000, 0.8660254037844387076, 1.000000000000000000, 0.8660254037844387076, 1.000000000000000000, 0.8660254037844387076, 1.000000000000000000, 0.8660254037844387076, 1.000000000000000000, 0.8660254037844387076, 1.000000000000000000, 0.8660254037844387076, 1.000000000000000000, 0.8660254037844387076, 1.000000000000000000, 0.8660254037844387076, 1.000000000000000000, 0.8660254037844387076, 1.000000000000000000, 0.8660254037844387076, 1.000000000000000000, 0.8660254037844387076, 1.000000000000000000, 0.8660254037844387076, 1.000000000000000000, 0.8660254037844387076, 1.000000000000000000, 0.8660254037844387076, 1.000000000000000000, 0.8660254037844387076, 1.000000000000000000, 0.8660254037844387076, 1.000000000000000000, 0.8660254037844387076, 1.000000000000000000, 0.8660254037844387076, 1.000000000000000000, 0.8660254037844387076, 1.000000000000000000, 0.8660254037844387076, 1.000000000000000000, 0.8660254037844387076, 1.000000000000000000, 0.8660254037844387076, 1.000000000000000000, 0.8660254037844387076, 1.000000000000000000, 0.8660254037844387076, 1.000000000000000000, 0.8660254037844387076, 1.000000000000000000, 0.8660254037844387076, 1.000000000000000000, 0.8660254037844387076, 1.000000000000000000, 0.8660254037844387076, 1.000000000000000000, 0.8660254037844387076, 1.000000000000000000, 0.8660254037844387076, 1.000000000000000000, 0.8660254037844387076, 1.000000000000000000, 0.8660254037844387076, 1.000000000000000000, 0.8660254037844387076, 1.000000000000000000, 0.8660254037844387076, 1.000000000000000000, 0.8660254037844387076, 1.000000000000000000, 0.8660254037844387076, 1.000000000000000000, 0.8660254037844387076, 1.000000000000000000, 0.8660254037844387076, 1.000000000000000000, 0.8660254037844387076, 1.000000000000000000, 0.8660254037844387076, 1.000000000000000000, 0.8660254037844387076, 1.000000000000000000, 0.8660254037844387076, 1.000000000000000000, 0.8660254037844387076, 1.000000000000000000, 0.8660254037844387076, 1.000000000000000000, 0.8660254037844387076, 1.000000000000000000, 0.8660254037844387076, 1.000000000000000000, 0.8660254037844387076, 1.000000000000000000, 0.8660254037844387076, 1.000000000000000000, 0.8660254037844387076, 1.000000000000000000, 0.8660254037844387076, 1.000000000000000000, 0.8660254037844387076, 1.000000000000000000, 0.8660254037844387076, 1.000000000000000000, 0.8660254037844387076, 1.000000000000000000, 0.8660254037844387076, 1.000000000000000000, 0.8660254037844387076, 1.000000000000000000, 0.8660254037844387076, 1.000000000000000000, 0.8660254037844387076, 1.000000000000000000, 0.8660254037844387076, 1.000000000000000000, 0.8660254037844387076, 1.000000000000000000, 0.8660254037844387076, 1.000000000000000000, 0.8660254037844387076, 1.000000000000000000, 0.8660254037844387076, 1.000000000000000000, 0.8660254037844387076, 1.000000000000000000, 0.8660254037844387076, 1.000000000000000000, 0.8660254037844387076, 1.000000000000000000, 0.8660254037844387076, 1.000000000000000000, 0.8660254037844387076, 1.000000000000000000, 0.8660254037844387076, 1.000000000000000000, 0.8660254037844387076, 1.000000000000000000, 0.8660254037844387076, 1.000000000000000000, 0.8660254037844387076, 1.000000000000000000, 0.8660254037844387076, 1.000000000000000000, 0.8660254037844387076, 1.000000000000000000, 0.8660254037844387076, 1.000000000000000000, 0.8660254037844387076, 1.000000000000000000, 0.8660254037844387076, 1.000000000000000000, 0.8660254037844387076, 1.000000000000000000, 0.8660254037844387076, 1.000000000000000000, 0.8660254037844387076, 1.000000000000000000, 0.8660254037844387076, 1.000000000000000000, 0.8660254037844387076, 1.000000000000000000, 0.8660254037844387076, 1.000000000000000000, 0.8660254037844387076, 1.000000000000000000, 0.8660254037844387076, 1.000000000000000000, 0.8660254037844387076, 1.000000000000000000, 0.8660254037844387076, 1.000000000000000000, 0.8660254037844387076, 1.000000000000000000, 0.8660254037844387076, 1.000000000000000000, 0.8660254037844387076, 1.000000000000000000, 0.8660254037844387076, 1.000000000000000000, 0.8660254037844387076, 1.000000000000000000, 0.8660254037844387076, 1.000000000000000000, 0.8660254037844387076, 1.000000000000000000, 0.8660254037844387076, 1.000000000000000000, 0.8660254037844387076, 1.000000000000000000, 0.8660254037844387076, 1.000000000000000000, 0.8660254037844387076, 1.000000000000000000, 0.8660254037844387076, 1.000000000000000000, 0.8660254037844387076, 1.000000000000000000, 0.8660254037844387076, 1.000000000000000000, 0.8660254037844387076, 1.000000000000000000, 0.8660254037844387076, 1.000000000000000000, 0.8660254037844387076, 1.000000000000000000, 0.8660254037844387076, 1.000000000000000000, 0.8660254037844387076, 1.000000000000000000, 0.8660254037844387076, 1.000000000000000000, 0.8660254037844387076, 1.000000000000000000, 0.8660254037844387076, 1.000000000000000000, 0.8660254037844387076, 1.000000000000000000, 0.8660254037844387076, 1.000000000000000000, 0.8660254037844387076, 1.000000000000000000, 0.8660254037844387076, 1.000000000000000000, 0.8660254037844387076, 1.000000000000000000, 0.8660254037844387076, 1.000000000000000000, 0.8660254037844387076, 1.000000000000000000, 0.8660254037844387076, 1.000000000000000000, 0.8660254037844387076, 1.000000000000000000, 0.8660254037844387076, 1.000000000000000000, 0.8660254037844387076, 1.000000000000000000, 0.8660254037844387076, 1.000000000000000000, 0.8660254037844387076, 1.000000000000000000, 0.8660254037844387076, 1.000000000000000000, 0.8660254037844387076, 1.000000000000000000, 0.8660254037844387076, 1.000000000000000000, 0.8660254037844387076, 1.000000000000000000, 0.8660254037844387076, 1.000000000000000000, 0.8660254037844387076, 1.000000000000000000, 0.8660254037844387076, 1.000000000000000000, 0.8660254037844387076, 1.000000000000000000, 0.8660254037844387076, 1.000000000000000000, 0.8660254037844387076, 1.000000000000000000, 0.8660254037844387076, 1.000000000000000000, 0.8660254037844387076, 1.000000000000000000, 0.8660254037844387076, 1.000000000000000000, 0.8660254037844387076, 1.000000000000000000, 0.8660254037844387076, 1.000000000000000000, 0.8660254037844387076, 1.000000000000000000, 0.8660254037844387076, 1.000000000000000000, 0.8660254037844387076, 1.000000000000000000, 0.8660254037844387076, 1.000000000000000000, 0.8660254037844387076, 1.000000000000000000, 0.8660254037844387076, 1.000000000000000000, 0.8660254037844387076, 1.000000000000000000, 0.8660254037844387076, 1.000000000000000000, 0.8660254037844387076, 1.000000000000000000, 0.8660254037844387076, 1.000000000000000000, 0.8660254037844387076, 1.000000000000000000, 0.8660254037844387076, 1.000000000000000000, 0.8660254037844387076, 1.000000000000000000, 0.8660254037844387076, 1.000000000000000000, 0.8660254037844387076, 1.000000000000000000, 0.8660254037844387076, 1.000000000000000000, 0.8660254037844387076, 1.000000000000000000, 0.8660254037844387076, 1.000000000000000000, 0.8660254037844387076, 1.000000000000000000, 0.8660254037844387076, 1.000000000000000000, 0.8660254037844387076, 1.000000000000000000, 0.8660254037844387076, 1.000000000000000000, 0.8660254037844387076, 1.000000000000000000, 0.8660254037844387076, 1.000000000000000000, 0.8660254037844387076, 1.000000000000000000, 0.8660254037844387076, 1.000000000000000000, 0.8660254037844387076, 1.000000000000000000, 0.8660254037844387076, 1.000000000000000000, 0.8660254037844387076, 1.000000000000000000, 0.8660254037844387076, 1.000000000000000000, 0.8660254037844387076, 1.000000000000000000, 0.8660254037844387076, 1.000000000000000000, 0.8660254037844387076, 1.000000000000000000, 0.8660254037844387076, 1.000000000000000000, 0.8660254037844387076, 1.000000000000000000, 0.8660254037844387076, 1.000000000000000000, 0.8660254037844387076, 1.000000000000000000, 0.8660254037844387076, 1.000000000000000000, 0.8660254037844387076, 1.000000000000000000, 0.8660254037844387076, 1.000000000000000000, 0.8660254037844387076, 1.000000000000000000, 0.8660254037844387076, 1.000000000000000000, 0.8660254037844387076, 1.000000000000000000, 0.8660254037844387076, 1.000000000000000000, 0.8660254037844387076, 1.000000000000000000, 0.8660254037844387076, 1.000000000000000000),
 ( 1.000000000000000000, 0.8660254037844387076, 1.000000000000000000, 0.8660254037844387076, 1.000000000000000000, 0.8660254037844387076, 1.000000000000000000, 0.8660254037844387076, 1.000000000000000000, 0.8660254037844387076, 1.000000000000000000, 0.8660254037844387076, 1.000000000000000000, 0.8660254037844387076, 1.000000000000000000, 0.8660254037844387076, 1.000000000000000000, 0.8660254037844387076, 1.000000000000000000, 0.8660254037844387076, 1.000000000000000000, 0.8660254037844387076, 1.000000000000000000, 0.8660254037844387076, 1.000000000000000000, 0.8660254037844387076, 1.000000000000000000, 0.8660254037844387076, 1.000000000000000000, 0.8660254037844387076, 1.000000000000000000, 0.8660254037844387076, 1.000000000000000000, 0.8660254037844387076, 1.000000000000000000, 0.8660254037844387076, 1.000000000000000000, 0.8660254037844387076, 1.000000000000000000, 0.8660254037844387076, 1.000000000000000000, 0.8660254037844387076, 1.000000000000000000, 0.8660254037844387076, 1.000000000000000000, 0.8660254037844387076, 1.000000000000000000, 0.8660254037844387076, 1.000000000000000000, 0.8660254037844387076, 1.000000000000000000, 0.8660254037844387076, 1.000000000000000000, 0.8660254037844387076, 1.000000000000000000, 0.8660254037844387076, 1.000000000000000000, 0.8660254037844387076, 1.000000000000000000, 0.8660254037844387076, 1.000000000000000000, 0.8660254037844387076, 1.000000000000000000, 0.8660254037844387076, 1.000000000000000000, 0.8660254037844387076, 1.000000000000000000, 0.8660254037844387076, 1.000000000000000000, 0.8660254037844387076, 1.000000000000000000, 0.8660254037844387076, 1.000000000000000000, 0.8660254037844387076, 1.000000000000000000, 0.8660254037844387076, 1.000000000000000000, 0.8660254037844387076, 1.000000000000000000, 0.8660254037844387076, 1.000000000000000000, 0.8660254037844387076, 1.000000000000000000, 0.8660254037844387076, 1.000000000000000000, 0.8660254037844387076, 1.000000000000000000, 0.8660254037844387076, 1.000000000000000000, 0.8660254037844387076, 1.000000000000000000, 0.8660254037844387076, 1.000000000000000000, 0.8660254037844387076, 1.000000000000000000, 0.8660254037844387076, 1.000000000000000000, 0.8660254037844387076, 1.000000000000000000, 0.8660254037844387076, 1.000000000000000000, 0.8660254037844387076, 1.000000000000000000, 0.8660254037844387076, 1.000000000000000000, 0.8660254037844387076, 1.000000000000000000, 0.8660254037844387076, 1.000000000000000000, 0.8660254037844387076, 1.000000000000000000, 0.8660254037844387076, 1.000000000000000000, 0.8660254037844387076, 1.000000000000000000, 0.8660254037844387076, 1.000000000000000000, 0.8660254037844387076, 1.000000000000000000, 0.8660254037844387076, 1.000000000000000000, 0.8660254037844387076, 1.000000000000000000, 0.8660254037844387076, 1.000000000000000000, 0.8660254037844387076, 1.000000000000000000, 0.8660254037844387076, 1.000000000000000000, 0.8660254037844387076, 1.000000000000000000, 0.8660254037844387076, 1.000000000000000000, 0.8660254037844387076, 1.000000000000000000, 0.8660254037844387076, 1.000000000000000000, 0.8660254037844387076, 1.000000000000000000, 0.8660254037844387076, 1.000000000000000000, 0.8660254037844387076, 1.000000000000000000, 0.8660254037844387076, 1.000000000000000000, 0.8660254037844387076, 1.000000000000000000, 0.8660254037844387076, 1.000000000000000000, 0.8660254037844387076, 1.000000000000000000, 0.8660254037844387076, 1.000000000000000000, 0.8660254037844387076, 1.000000000000000000, 0.8660254037844387076, 1.000000000000000000, 0.8660254037844387076, 1.000000000000000000, 0.8660254037844387076, 1.000000000000000000, 0.8660254037844387076, 1.000000000000000000, 0.8660254037844387076, 1.000000000000000000, 0.8660254037844387076, 1.000000000000000000, 0.8660254037844387076, 1.000000000000000000, 0.8660254037844387076, 1.000000000000000000, 0.8660254037844387076, 1.000000000000000000, 0.8660254037844387076, 1.000000000000000000, 0.8660254037844387076, 1.000000000000000000, 0.8660254037844387076, 1.000000000000000000, 0.8660254037844387076, 1.000000000000000000, 0.8660254037844387076, 1.000000000000000000, 0.8660254037844387076, 1.000000000000000000, 0.8660254037844387076, 1.000000000000000000, 0.8660254037844387076, 1.000000000000000000, 0.8660254037844387076, 1.000000000000000000, 0.8660254037844387076, 1.000000000000000000, 0.8660254037844387076, 1.000000000000000000, 0.8660254037844387076, 1.000000000000000000, 0.8660254037844387076, 1.000000000000000000, 0.8660254037844387076, 1.000000000000000000, 0.8660254037844387076, 1.000000000000000000, 0.8660254037844387076, 1.000000000000000000, 0.8660254037844387076, 1.000000000000000000, 0.8660254037844387076, 1.000000000000000000, 0.8660254037844387076, 1.000000000000000000, 0.8660254037844387076, 1.000000000000000000, 0.8660254037844387076, 1.000000000000000000, 0.8660254037844387076, 1.000000000000000000, 0.8660254037844387076, 1.000000000000000000, 0.8660254037844387076, 1.000000000000000000, 0.8660254037844387076, 1.000000000000000000, 0.8660254037844387076, 1.000000000000000000, 0.8660254037844387076, 1.000000000000000000, 0.8660254037844387076, 1.000000000000000000, 0.8660254037844387076, 1.000000000000000000, 0.8660254037844387076, 1.000000000000000000, 0.8660254037844387076, 1.000000000000000000, 0.8660254037844387076, 1.000000000000000000, 0.8660254037844387076, 1.000000000000000000, 0.8660254037844387076, 1.000000000000000000, 0.8660254037844387076, 1.000000000000000000, 0.8660254037844387076, 1.000000000000000000, 0.8660254037844387076, 1.000000000000000000, 0.8660254037844387076, 1.000000000000000000, 0.8660254037844387076, 1.000000000000000000, 0.8660254037844387076, 1.000000000000000000, 0.8660254037844387076, 1.000000000000000000, 0.8660254037844387076, 1.000000000000000000, 0.8660254037844387076, 1.000000000000000000, 0.8660254037844387076, 1.000000000000000000, 0.8660254037844387076, 1.000000000000000000, 0.8660254037844387076, 1.000000000000000000, 0.8660254037844387076, 1.000000000000000000, 0.8660254037844387076, 1.000000000000000000, 0.8660254037844387076, 1.000000000000000000, 0.8660254037844387076, 1.000000000000000000, 0.8660254037844387076, 1.000000000000000000, 0.8660254037844387076, 1.000000000000000000, 0.8660254037844387076, 1.000000000000000000, 0.8660254037844387076, 1.000000000000000000, 0.8660254037844387076, 1.000000000000000000, 0.8660254037844387076, 1.000000000000000000, 0.8660254037844387076, 1.000000000000000000, 0.8660254037844387076, 1.000000000000000000, 0.8660254037844387076, 1.000000000000000000, 0.8660254037844387076, 1.000000000000000000, 0.8660254037844387076, 1.000000000000000000, 0.8660254037844387076, 1.000000000000000000, 0.8660254037844387076, 1.000000000000000000, 0.8660254037844387076, 1.000000000000000000, 0.8660254037844387076, 1.000000000000000000, 0.8660254037844387076, 1.000000000000000000, 0.8660254037844387076, 1.000000000000000000, 0.8660254037844387076, 1.000000000000000000, 0.8660254037844387076, 1.000000000000000000, 0.8660254037844387076, 1.000000000000000000, 0.8660254037844387076, 1.000000000000000000, 0.8660254037844387076, 1.000000000000000000, 0.8660254037844387076, 1.000000000000000000, 0.8660254037844387076, 1.000000000000000000, 0.8660254037844387076, 1.000000000000000000, 0.8660254037844387076, 1.000000000000000000, 0.8660254037844387076, 1.000000000000000000, 0.8660254037844387076, 1.000000000000000000, 0.8660254037844387076, 1.000000000000000000, 0.8660254037844387076, 1.000000000000000000, 0.8660254037844387076, 1.000000000000000000, 0.8660254037844387076, 1.000000000000000000, 0.8660254037844387076, 1.000000000000000000, 0.8660254037844387076, 1.000000000000000000, 0.8660254037844387076, 1.000000000000000000, 0.8660254037844387076, 1.000000000000000000, 0.8660254037844387076, 1.000000000000000000, 0.8660254037844387076, 1.000000000000000000, 0.8660254037844387076, 1.000000000000000000, 0.8660254037844387076, 1.000000000000000000, 0.8660254037844387076, 1.000000000000000000, 0.8660254037844387076, 1.000000000000000000, 0.8660254037844387076, 1.000000000000000000, 0.8660254037844387076, 1.000000000000000000, 0.8660254037844387076, 1.000000000000000000, 0.8660254037844387076, 1.000000000000000000, 0.8660254037844387076, 1.000000000000000000, 0.8660254037844387076, 1.000000000000000000, 0.8660254037844387076, 1.000000000000000000, 0.8660254037844387076, 1.000000000000000000, 0.8660254037844387076, 1.000000000000000000, 0.8660254037844387076, 1.000000000000000000, 0.8660254037844387076, 1.000000000000000000, 0.8660254037844387076, 1.000000000000000000, 0.8660254037844387076, 1.000000000000000000, 0.8660254037844387076, 1.000000000000000000, 0.8660254037844387076, 1.000000000000000000, 0.8660254037844387076, 1.000000000000000000, 0.8660254037844387076, 1.000000000000000000, 0.8660254037844387076, 1.000000000000000000, 0.8660254037844387076, 1.000000000000000000, 0.8660254037844387076, 1.000000000000000000, 0.8660254037844387076, 1.000000000000000000, 0.8660254037844387076, 1.000000000000000000, 0.8660254037844387076, 1.000000000000000000, 0.8660254037844387076, 1.000000000000000000, 0.8660254037844387076, 1.000000000000000000, 0.8660254037844387076, 1.000000000000000000, 0.8660254037844387076, 1.000000000000000000, 0.8660254037844387076, 1.000000000000000000, 0.8660254037844387076, 1.000000000000000000, 0.8660254037844387076, 1.000000000000000000, 0.8660254037844387076, 1.000000000000000000, 0.8660254037844387076, 1.000000000000000000, 0.8660254037844387076, 1.000000000000000000, 0.8660254037844387076, 1.000000000000000000, 0.8660254037844387076, 1.000000000000000000, 0.8660254037844387076, 1.000000000000000000, 0.8660254037844387076, 1.000000000000000000, 0.8660254037844387076, 1.000000000000000000, 0.8660254037844387076, 1.000000000000000000, 0.8660254037844387076, 1.000000000000000000, 0.8660254037844387076, 1.000000000000000000, 0.8660254037844387076, 1.000000000000000000, 0.8660254037844387076, 1.000000000000000000, 0.8660254037844387076, 1.000000000000000000, 0.8660254037844387076, 1.000000000000000000, 0.8660254037844387076, 1.000000000000000000, 0.8660254037844387076, 1.000000000000000000, 0.8660254037844387076, 1.000000000000000000, 0.8660254037844387076, 1.000000000000000000, 0.8660254037844387076, 1.000000000000000000, 0.8660254037844387076, 1.000000000000000000, 0.8660254037844387076, 1.000000000000000000, 0.8660254037844387076, 1.000000000000000000, 0.8660254037844387076, 1.000000000000000000, 0.8660254037844387076, 1.000000000000000000, 0.8660254037844387076, 1.000000000000000000, 0.8660254037844387076, 1.000000000000000000, 0.8660254037844387076, 1.000000000000000000, 0.8660254037844387076, 1.000000000000000000, 0.8660254037844387076, 1.000000000000000000, 0.8660254037844387076, 1.000000000000000000, 0.8660254037844387076, 1.000000000000000000) ) ) 
 REPRESENTATION_ITEM ( '' )  SURFACE ( )  );
#156362 = DIRECTION ( 'NONE',  ( -1.000000000000000000, 0.000000000000000000, 0.000000000000000000 ) ) ;
#156363 = CARTESIAN_POINT ( 'NONE',  ( 5.572493885891085519, 0.7809320506734825917, 1.745880147543739325 ) ) ;
#156364 = CARTESIAN_POINT ( 'NONE',  ( -4.036671995544492297, 7.285761072467114019, 0.7944190476826870073 ) ) ;
#156365 = CARTESIAN_POINT ( 'NONE',  ( 4.975479186090847605, 7.788180902872553268, 1.082531754730558626 ) ) ;
#156367 = CARTESIAN_POINT ( 'NONE',  ( 3.444935562074178392, -1.779636981393231565, -0.9480232565319337557 ) ) ;
#156366 = CARTESIAN_POINT ( 'NONE',  ( -8.473482818416675499, 9.948446711983361723, -1.082531754730543083 ) ) ;
#156368 = CARTESIAN_POINT ( 'NONE',  ( -0.7500000000000215383, 3.691666666666690411, 1.299038105676671107 ) ) ;
#156369 = CARTESIAN_POINT ( 'NONE',  ( 0.6823417656249934904, 14.75520833367473195, 1.181850606188764807 ) ) ;
#156370 = CARTESIAN_POINT ( 'NONE',  ( 5.948237010872538200, 1.723075781188963207, 0.07969437682242562493 ) ) ;
#156371 = CARTESIAN_POINT ( 'NONE',  ( 7.201315867513990554, 8.430565262634994284, -1.199719254218452047 ) ) ;
#156372 = CARTESIAN_POINT ( 'NONE',  ( 8.270110514656021650, 11.63191745286530576, 1.082531754730557072 ) ) ;
#156373 = CARTESIAN_POINT ( 'NONE',  ( -11.44779963594988814, 10.90000000000000036, -3.600000000000000977 ) ) ;
#156374 = CARTESIAN_POINT ( 'NONE',  ( 4.622238261848357510, 1.152259890254858421, -1.473394524551620011 ) ) ;
#156375 = CARTESIAN_POINT ( 'NONE',  ( 4.575498903167257936, 8.352182797088220312, 0.2657046714051370384 ) ) ;
#156377 = STYLED_ITEM ( 'NONE', ( #60584 ), #62018 ) ;
#156376 = CARTESIAN_POINT ( 'NONE',  ( 2.254815949590884827, -0.5480598642870064818, -1.996355599893632649 ) ) ;
#156378 = CARTESIAN_POINT ( 'NONE',  ( -7.878696662872776812, 8.364436659539265406, -0.7216878364870338292 ) ) ;
#156379 = ORIENTED_EDGE ( 'NONE', *, *, #77841, .F. ) ;
#156381 = CARTESIAN_POINT ( 'NONE',  ( 5.063044020060520900, 4.871582543017558109, 0.7998128361456352531 ) ) ;
#156380 = AXIS2_PLACEMENT_3D ( 'NONE', #27182, #76996, #71119 ) ;
#156382 = CARTESIAN_POINT ( 'NONE',  ( -0.3423093779010479842, 3.099999999999998757, 0.3999999999999559464 ) ) ;
#156383 = CARTESIAN_POINT ( 'NONE',  ( 0.1932431142802397694, 1.690279412936572134, -0.6521791651670250101 ) ) ;
#156384 = CARTESIAN_POINT ( 'NONE',  ( 3.729901657090938460, 7.365652676665848553, 0.7216878364870257245 ) ) ;
#156385 = CARTESIAN_POINT ( 'NONE',  ( -0.3852658704378487120, -6.836271227032193032, -10.85717823004578264 ) ) ;
#156386 = CARTESIAN_POINT ( 'NONE',  ( 8.066738210006679566, 10.43428054980638997, 1.443375672974076540 ) ) ;
#156387 = CARTESIAN_POINT ( 'NONE',  ( 6.564118927310645724, 10.80988918183778225, -0.7998128361456291469 ) ) ;
#156388 = CARTESIAN_POINT ( 'NONE',  ( 5.607027416250175200, -0.04201266709560196738, 1.915314589656505362 ) ) ;
#156389 = CARTESIAN_POINT ( 'NONE',  ( 3.226477370372323072, 6.708047998835549031, 0.7216878364870540352 ) ) ;
#156390 = FACE_OUTER_BOUND ( 'NONE', #62703, .T. ) ;
#156391 = CARTESIAN_POINT ( 'NONE',  ( 4.000000000000012434, 0.000000000000000000, -0.7500000000000006661 ) ) ;
#156393 = ORIENTED_EDGE ( 'NONE', *, *, #141157, .T. ) ;
#156392 = CARTESIAN_POINT ( 'NONE',  ( 4.039966587192259873, 5.736380323189513852, 1.443375672974062551 ) ) ;
#156394 = CARTESIAN_POINT ( 'NONE',  ( -6.832946231607472498, 9.955225789308602913, 1.082531754730549967 ) ) ;
#156395 = CARTESIAN_POINT ( 'NONE',  ( 3.450221060135277629, 2.161883445724331665, 0.001893877739161941697 ) ) ;
#156396 = CARTESIAN_POINT ( 'NONE',  ( -7.946487431385463651, 8.443525889470736345, 0.7216878364870317197 ) ) ;
#156397 = CARTESIAN_POINT ( 'NONE',  ( 3.040771591214902259, 6.769593633051179005, -0.7998128361456362523 ) ) ;
#156398 = CARTESIAN_POINT ( 'NONE',  ( -4.288456660624211381, 3.897620947016656956, 1.214306433183764966E-14 ) ) ;
#156399 = CARTESIAN_POINT ( 'NONE',  ( 5.719710266082651096, -1.780569991979109590, 0.4021758204828808081 ) ) ;
#156400 = CARTESIAN_POINT ( 'NONE',  ( 8.826461557825265203, 13.26498588611182505, 7.661703860454772474 ) ) ;
#156401 = CARTESIAN_POINT ( 'NONE',  ( 1.106637804720354668, 1.495658270405418877, -1.284366697391533529 ) ) ;
#156402 = CARTESIAN_POINT ( 'NONE',  ( 3.568532368641282648, 0.6928216322696268969, 1.782650395559831180 ) ) ;
#156403 = ORIENTED_EDGE ( 'NONE', *, *, #17378, .F. ) ;
#156404 = LINE ( 'NONE', #170499, #56217 ) ;
#156405 = CARTESIAN_POINT ( 'NONE',  ( 5.055114266443681004, 1.638575763527612583, -1.092465951337840524 ) ) ;
#156406 = CARTESIAN_POINT ( 'NONE',  ( 0.9373250018651816395, 0.7876268737729983371, -1.775224631529322306 ) ) ;
#156407 = ORIENTED_EDGE ( 'NONE', *, *, #124535, .T. ) ;
#156408 = CARTESIAN_POINT ( 'NONE',  ( -5.906512197408906317, 6.919960980845699439, -1.199719254218453823 ) ) ;
#156410 = CARTESIAN_POINT ( 'NONE',  ( 6.363548717301088509, -1.704009271243651868, -1.262090224194649446 ) ) ;
#156409 = CARTESIAN_POINT ( 'NONE',  ( -3.610214042988883598, 7.433943160120816351, 0.7998128361456352531 ) ) ;
#156411 = CARTESIAN_POINT ( 'NONE',  ( 6.333067150914816423, 7.521571443223021625, 1.082531754730549967 ) ) ;
#156413 = ORIENTED_EDGE ( 'NONE', *, *, #121519, .F. ) ;
#156412 = CARTESIAN_POINT ( 'NONE',  ( 3.914637684252043393, -0.6027250981219151038, -1.814865640613130271 ) ) ;
#156414 = CARTESIAN_POINT ( 'NONE',  ( 1.272829778695073299, -1.399090282553701270, 1.706552004499435560 ) ) ;
#156415 = CIRCLE ( 'NONE', #38751, 9.499999999999992895 ) ;
#156416 = CARTESIAN_POINT ( 'NONE',  ( 9.475937985776971217, 4.398642190548649467, -7.290290962746341918 ) ) ;
#156417 = CARTESIAN_POINT ( 'NONE',  ( 6.287749749268194854, 1.925770139592613450, -0.5864224512089585284 ) ) ;
#156418 = CARTESIAN_POINT ( 'NONE',  ( 0.2331563151865486683, 0.005903526429595904942, -1.945944850731482934 ) ) ;
#156420 = CARTESIAN_POINT ( 'NONE',  ( 5.700407750362016301, 1.350738941191354625, -1.497498989668680114 ) ) ;
#156419 = CARTESIAN_POINT ( 'NONE',  ( -1.387358672527334136, 7.251968950354660493, -4.302625267139479348 ) ) ;
#156421 = LINE ( 'NONE', #205133, #206951 ) ;
#156422 = CARTESIAN_POINT ( 'NONE',  ( 1.908725956546155178, 0.6474277305483535638, 1.966616875269424192 ) ) ;
#156423 = CARTESIAN_POINT ( 'NONE',  ( -5.900823170445743671, 7.907379670318584353, 1.599625672291269396 ) ) ;
#156424 = CARTESIAN_POINT ( 'NONE',  ( -4.733264021794758136, 8.224961065399975624, 0.6825151564062783560 ) ) ;
#156425 = CARTESIAN_POINT ( 'NONE',  ( 0.3282377607281158904, 1.823664549684622882, 1.224999999999982991 ) ) ;
#156426 = CARTESIAN_POINT ( 'NONE',  ( 5.015626762051672571, 7.938982758113895422, 1.199719254218462483 ) ) ;
#156427 = DIRECTION ( 'NONE',  ( 1.000000000000000000, 0.000000000000000000, 0.000000000000000000 ) ) ;
#156428 = CARTESIAN_POINT ( 'NONE',  ( 5.912764389335563919, 6.070849007079172743, -0.7216878364870458196 ) ) ;
#156429 = CARTESIAN_POINT ( 'NONE',  ( -0.06269018847469841338, -7.008739397177404129, 9.499801640457409491 ) ) ;
#156430 = EDGE_CURVE ( 'NONE', #145411, #72859, #213882, .T. ) ;
#156431 = DIRECTION ( 'NONE',  ( 1.000000000000000000, -0.000000000000000000, -0.000000000000000000 ) ) ;
#156432 = CARTESIAN_POINT ( 'NONE',  ( -0.6823417656250039265, 12.13020833367473017, -1.181850606188755259 ) ) ;
#156434 = CARTESIAN_POINT ( 'NONE',  ( -6.740338644649361832, 7.892758502626242567, -1.199719254218452047 ) ) ;
#156433 = CARTESIAN_POINT ( 'NONE',  ( 6.925078400183553917, 6.038071034253152725, 2.450556290382682523 ) ) ;
#156435 = CARTESIAN_POINT ( 'NONE',  ( 4.904772540272760217, -0.9336124152922348207, -1.461164293347013921 ) ) ;
#156436 = AXIS2_PLACEMENT_3D ( 'NONE', #152826, #187449, #202613 ) ;
#156437 = CARTESIAN_POINT ( 'NONE',  ( -4.009460741339347045, 5.700790169694431420, -1.599625672291256295 ) ) ;
#156438 = CONICAL_SURFACE ( 'NONE', #12060, 1.000000000000000000, 0.7853981633974508325 ) ;
#156439 = CARTESIAN_POINT ( 'NONE',  ( 2.465759480183654428, -0.4578044685884518072, 2.018832516862689275 ) ) ;
#156440 = CARTESIAN_POINT ( 'NONE',  ( 4.007494584968971374, -2.025512140874039524, 0.6163414799803969002 ) ) ;
#156441 = CARTESIAN_POINT ( 'NONE',  ( 8.288111976655649471, 8.563885482386732306, -0.7998128361456291469 ) ) ;
#156442 = CARTESIAN_POINT ( 'NONE',  ( 1.364683531249988535, 3.405208333674749621, -0.7879004041258239610 ) ) ;
#156443 = CARTESIAN_POINT ( 'NONE',  ( 1.639439270303972851, 1.821716124042528584, -0.7488776562727271768 ) ) ;
#156444 = CARTESIAN_POINT ( 'NONE',  ( 5.480859523967800406, 6.436073219340427976, 1.263442102793509880 ) ) ;
#156446 = CARTESIAN_POINT ( 'NONE',  ( -0.08783152977152529350, -1.912005390248720627, -0.04503566501021933483 ) ) ;
#156445 = CARTESIAN_POINT ( 'NONE',  ( 3.475000000000000533, -2.624999999999998668, 0.000000000000000000 ) ) ;
#156447 = CARTESIAN_POINT ( 'NONE',  ( 3.433774379101984575, 1.031038968642459475, -2.047360584804863493 ) ) ;
#156448 = CARTESIAN_POINT ( 'NONE',  ( 1.963248404482214049, 0.3131683437365209710, -1.798463397695612809 ) ) ;
#156449 = CARTESIAN_POINT ( 'NONE',  ( 4.203910148689107729, 7.062256385849379647, -1.199719254218448494 ) ) ;
#156450 = CARTESIAN_POINT ( 'NONE',  ( 5.436456408955479880, 9.286356877182658565, -0.7216878364870267237 ) ) ;
#156451 = CARTESIAN_POINT ( 'NONE',  ( -8.345207244411405156, 9.694828859023472134, 1.199719254218462483 ) ) ;
#156452 = CARTESIAN_POINT ( 'NONE',  ( 3.146742683403806140, 1.965092980649842502, 0.4368759242464967940 ) ) ;
#156453 = CARTESIAN_POINT ( 'NONE',  ( 2.940231979924610162, -1.012623612260230566, 1.680088604585870060 ) ) ;
#156454 = CARTESIAN_POINT ( 'NONE',  ( -9.020252271793614440, 9.418049160047695878, 0.7998128361456462443 ) ) ;
#156455 = CARTESIAN_POINT ( 'NONE',  ( -7.250913225210214641, 7.353820272367037170, 0.7998128361456341429 ) ) ;
#156456 = CARTESIAN_POINT ( 'NONE',  ( -1.400751299551485696, 7.315968950354793776, -4.333496285525604286 ) ) ;
#156458 = CARTESIAN_POINT ( 'NONE',  ( 4.873781607783202574, 1.020544065373253817, 1.445763320596996193 ) ) ;
#156457 = CARTESIAN_POINT ( 'NONE',  ( 6.298786922650962516, 1.737427944715240091, 1.162477542130130548 ) ) ;
#156459 = CARTESIAN_POINT ( 'NONE',  ( -11.84668730067608600, 19.00000000000000000, 1.319999999999998286 ) ) ;
#156460 = CARTESIAN_POINT ( 'NONE',  ( 1.131117939106265569, -1.979831898266545487, 0.9398196729281658168 ) ) ;
#156461 = CARTESIAN_POINT ( 'NONE',  ( 6.105355155539634815, -1.726289741429184899, 0.2200517785161565654 ) ) ;
#156462 = AXIS2_PLACEMENT_3D ( 'NONE', #129764, #195747, #47384 ) ;
#156463 = CARTESIAN_POINT ( 'NONE',  ( 8.046927864910717432, 9.346836249606042202, 1.199719254218462483 ) ) ;
#156464 = DIRECTION ( 'NONE',  ( -0.7771862570881792331, -0.6292706268317843632, -6.822565806923340619E-15 ) ) ;
#156465 = CARTESIAN_POINT ( 'NONE',  ( 0.2460673368967214447, -2.230335335914147343, -0.5547215216719133535 ) ) ;
#156466 = LINE ( 'NONE', #190011, #39220 ) ;
#156467 = CARTESIAN_POINT ( 'NONE',  ( 5.729790939124476346, -1.568816369837353619, -0.7386035493782086014 ) ) ;
#156468 = CARTESIAN_POINT ( 'NONE',  ( 1.594636444620714633, -2.196503929104542951, -0.2137616909994101977 ) ) ;
#156469 = CARTESIAN_POINT ( 'NONE',  ( 5.354042097475935513, -0.7863316197885154013, 2.023950393233854061 ) ) ;
#156470 = CARTESIAN_POINT ( 'NONE',  ( 5.456087663318581527, 6.086207979321623718, 0.9243867668097293100 ) ) ;
#156471 = CARTESIAN_POINT ( 'NONE',  ( 0.5325983862809284819, 0.6208049431430485710, 2.024263306480874380 ) ) ;
#156472 = CARTESIAN_POINT ( 'NONE',  ( 3.750000000000002665, 2.137871159508210026E-13, 2.052068128417945836 ) ) ;
#156473 = DIRECTION ( 'NONE',  ( 0.000000000000000000, 1.000000000000000000, 0.000000000000000000 ) ) ;
#156474 = CARTESIAN_POINT ( 'NONE',  ( 4.084924167595121780, -0.1881231333150361895, -1.917172266129524294 ) ) ;
#156475 = CARTESIAN_POINT ( 'NONE',  ( -1.500000000000001110, 11.05208333401613707, 0.8660254037844419273 ) ) ;
#156476 = CARTESIAN_POINT ( 'NONE',  ( 1.208037074693757651, 1.685330760668615646, 1.447128815913247379 ) ) ;
#156477 = EDGE_LOOP ( 'NONE', ( #167880, #134426, #58761, #209248 ) ) ;
#156478 = CARTESIAN_POINT ( 'NONE',  ( -1.500000000000013101, 4.129166666666687746, -0.8660254037844313801 ) ) ;
#156479 = CARTESIAN_POINT ( 'NONE',  ( 5.335297142177534369, 6.183267073083954735, -1.199719254218452047 ) ) ;
#156480 = CARTESIAN_POINT ( 'NONE',  ( 7.630541526392844887, 7.796719957080126662, 0.7998128361456341429 ) ) ;
#156481 = CARTESIAN_POINT ( 'NONE',  ( 4.160924129468469346, 0.5925846814045959698, 2.140718581676650079 ) ) ;
#156482 = CARTESIAN_POINT ( 'NONE',  ( -9.503902493499651882, 10.19023378527882784, 1.040834085586084257E-14 ) ) ;
#156483 = SURFACE_STYLE_USAGE ( .BOTH. , #92569 ) ;
#156484 = CARTESIAN_POINT ( 'NONE',  ( 6.860062538834778678, 8.066123052471139587, -1.082531754730543083 ) ) ;
#156485 = CARTESIAN_POINT ( 'NONE',  ( -9.639484029191951464, 10.34841224358651601, 0.7216878364870438212 ) ) ;
#156486 = CARTESIAN_POINT ( 'NONE',  ( 6.373741612200162443, 8.529394195690610303, 1.443375672974065660 ) ) ;
#156487 = CARTESIAN_POINT ( 'NONE',  ( 0.8092204703840089053, 1.198858234535697065, -1.621184076614573533 ) ) ;
#156489 = CARTESIAN_POINT ( 'NONE',  ( 6.725054104113727504, -1.884248279909329638, -0.8396177084525523471 ) ) ;
#156488 = CARTESIAN_POINT ( 'NONE',  ( 8.320953590485093088, 10.73086516036454618, 1.599625672291281386 ) ) ;
#156490 = CARTESIAN_POINT ( 'NONE',  ( -10.87166355890668790, -6.717152734873728548, 0.1969747848976953764 ) ) ;
#156491 = CARTESIAN_POINT ( 'NONE',  ( 6.116136693096175136, 9.189224337703940648, -1.082531754730548412 ) ) ;
#156492 = CARTESIAN_POINT ( 'NONE',  ( -0.07694640568740516995, -1.131669979810394633, -1.452919414246391261 ) ) ;
#156493 = DIRECTION ( 'NONE',  ( 0.000000000000000000, 0.000000000000000000, -1.000000000000000000 ) ) ;
#156494 = CARTESIAN_POINT ( 'NONE',  ( 1.364683531249988535, 2.613541667008089764, 0.7879004041258500513 ) ) ;
#156495 = CARTESIAN_POINT ( 'NONE',  ( 1.862210123611393708, -1.255811410660602867, 1.247235970127296811 ) ) ;
#156496 = CARTESIAN_POINT ( 'NONE',  ( 0.5631252389872200004, -1.117830369828230808, 1.678006741548984770 ) ) ;
#156497 = CARTESIAN_POINT ( 'NONE',  ( 6.567905868640212752, -1.062476624526029312, 1.378933096211315101 ) ) ;
#156498 = CARTESIAN_POINT ( 'NONE',  ( 4.546573649138107243, -1.841725595444974939, 1.364713657601625885 ) ) ;
#156499 = CARTESIAN_POINT ( 'NONE',  ( -1.364683531250014514, -0.4697916663252449943, 0.7879004041258379498 ) ) ;
#156500 = CARTESIAN_POINT ( 'NONE',  ( 2.413779523973126118, 1.202770565240804279, -1.394052804434331216 ) ) ;
#156501 = CARTESIAN_POINT ( 'NONE',  ( 8.401248741962376698, 12.95320729893149370, 0.7998128361456462443 ) ) ;
#156502 = CARTESIAN_POINT ( 'NONE',  ( 10.21213376015692909, 9.983165060110801292, -6.481890735896122635 ) ) ;
#156503 = CARTESIAN_POINT ( 'NONE',  ( 3.205874166558682514, -1.823564452915670042, 0.08818595847179949709 ) ) ;
#156504 = CARTESIAN_POINT ( 'NONE',  ( 3.551407868487792552, -1.352154898762620849, 1.496051317864899088 ) ) ;
#156505 = CARTESIAN_POINT ( 'NONE',  ( -10.31505594189871111, 10.92865344183699428, -0.7998128361456291469 ) ) ;
#156507 = CARTESIAN_POINT ( 'NONE',  ( -0.3769810270648435990, 3.049942316455334090, 0.4288785890452350702 ) ) ;
#156506 = CARTESIAN_POINT ( 'NONE',  ( 3.362467959171450360, 1.015586399080644187, 2.021831916694483144 ) ) ;
#156508 = CARTESIAN_POINT ( 'NONE',  ( 5.772525194315006658, -1.338739070262290110, 1.625669279078660878 ) ) ;
#156509 = CARTESIAN_POINT ( 'NONE',  ( 6.870046935992006887, 15.99925261518604636, 9.444314260337707267 ) ) ;
#156510 = CARTESIAN_POINT ( 'NONE',  ( 2.102089431743926706, 0.7944251937819692966, -1.912079865474418439 ) ) ;
#156511 = CARTESIAN_POINT ( 'NONE',  ( 2.842405760359353106, 6.467890487061221272, -0.7998128361456291469 ) ) ;
#156512 = CARTESIAN_POINT ( 'NONE',  ( -0.6801582343750559589, -0.03645833299194961574, 1.178068619123796568 ) ) ;
#156513 = CARTESIAN_POINT ( 'NONE',  ( 6.358074577831472673, 0.8120454629646983724, -1.959034198684066697 ) ) ;
#156515 = CARTESIAN_POINT ( 'NONE',  ( 0.6801461905075457670, -1.071176224578209935, 1.601055298966150842 ) ) ;
#156514 = CARTESIAN_POINT ( 'NONE',  ( -9.829825065107822724, 11.42688298316931572, 1.199719254218462483 ) ) ;
#156516 = CARTESIAN_POINT ( 'NONE',  ( -5.490125858891038213, 5.369844688319787451, -0.7998128361456362523 ) ) ;
#156517 = CARTESIAN_POINT ( 'NONE',  ( 8.585337585951586803, 11.03931315507545108, -1.599625672291255185 ) ) ;
#156518 = CARTESIAN_POINT ( 'NONE',  ( 5.519577934094861860, 6.572500690266394940, 1.082531754730549078 ) ) ;
#156519 = CARTESIAN_POINT ( 'NONE',  ( 4.163006777067105091, 7.380761635867615134, 0.7803290320304544503 ) ) ;
#156520 = CARTESIAN_POINT ( 'NONE',  ( -3.475000000000000533, -1.035416665710751527, -2.006292185433948827 ) ) ;
#156521 = CARTESIAN_POINT ( 'NONE',  ( -5.440899717785814715, 5.242137847038546461, 0.7998128361456341429 ) ) ;
#156522 = CARTESIAN_POINT ( 'NONE',  ( 0.2994921435493704820, -0.2801620449621230469, -2.203647339609093869 ) ) ;
#156523 = CARTESIAN_POINT ( 'NONE',  ( 2.626118769021787536, -1.211593817910999293, -1.722331309457482362 ) ) ;
#156524 = CARTESIAN_POINT ( 'NONE',  ( -5.002032328799064231, 4.800402236545811441, -0.7998128361456362523 ) ) ;
#156525 = CARTESIAN_POINT ( 'NONE',  ( 8.209625708274705502, 9.536650400197368427, 1.199719254218462483 ) ) ;
#156526 = CARTESIAN_POINT ( 'NONE',  ( 6.420743829754993470, -1.316656903452334992, 1.315380689086578236 ) ) ;
#156527 = CARTESIAN_POINT ( 'NONE',  ( 8.098297826064319693, 8.342435640030188893, 0.7998128361456481317 ) ) ;
#156528 = CARTESIAN_POINT ( 'NONE',  ( 0.07680821025393690105, 0.005952109439256307241, -1.810863387344714193 ) ) ;
#156529 = CARTESIAN_POINT ( 'NONE',  ( -7.621091744657483069, 8.063897588288083895, 0.7216878364870317197 ) ) ;
#156530 = CARTESIAN_POINT ( 'NONE',  ( -7.212574532790087645, 11.35849468832304154, -0.7216878364870267237 ) ) ;
#156531 = AXIS2_PLACEMENT_3D ( 'NONE', #134260, #151555, #69192 ) ;
#156532 = CARTESIAN_POINT ( 'NONE',  ( 0.03560581989598374242, -0.09759080014098624190, 2.118463022953632091 ) ) ;
#156533 = DIRECTION ( 'NONE',  ( -1.000000000000000000, 0.000000000000000000, -8.638326563840826660E-31 ) ) ;
#156535 = CARTESIAN_POINT ( 'NONE',  ( 2.805073129645048624, -1.632656238785214597, 1.087510969322850629 ) ) ;
#156534 = CARTESIAN_POINT ( 'NONE',  ( -1.225000000000040057, -0.02083333333332007889, -0.7072540797572998139 ) ) ;
#156536 = CARTESIAN_POINT ( 'NONE',  ( 2.237400686453533183, -1.931180590798301955, 0.9714560045831142077 ) ) ;
#156537 = AXIS2_PLACEMENT_3D ( 'NONE', #55855, #39604, #86223 ) ;
#156539 = CARTESIAN_POINT ( 'NONE',  ( -5.320367241134011493, 6.379272830146158313, -1.120692317505559643 ) ) ;
#156538 = CARTESIAN_POINT ( 'NONE',  ( -3.772911886352873445, 7.623757310712140800, 0.7998128361456352531 ) ) ;
#156540 = CARTESIAN_POINT ( 'NONE',  ( 0.6823417656249899377, 2.092708333674753174, 1.181850606188767472 ) ) ;
#156541 = CARTESIAN_POINT ( 'NONE',  ( 3.486021976759791308, -0.3410757193606011040, -1.706382030880509104 ) ) ;
#156542 = CARTESIAN_POINT ( 'NONE',  ( 5.910991785878156435, 7.919243054989755670, -1.443375672974057666 ) ) ;
#156543 = CARTESIAN_POINT ( 'NONE',  ( -11.65676533170044138, 6.358709890710655621, 4.978123860300238235 ) ) ;
#156544 = CARTESIAN_POINT ( 'NONE',  ( 2.530624857006387618, 1.977747929495787371, -0.3905373530270899174 ) ) ;
#156545 = CARTESIAN_POINT ( 'NONE',  ( -0.09775709102117645377, -9.919835437265268396, -10.99956570265432454 ) ) ;
#156546 = CARTESIAN_POINT ( 'NONE',  ( 0.2511322555047851290, -1.735185354305257110, 1.289038484408123963 ) ) ;
#156547 = CARTESIAN_POINT ( 'NONE',  ( 2.184392200726268829, -1.933073530578834465, -0.3863716293817393566 ) ) ;
#156550 = ORIENTED_EDGE ( 'NONE', *, *, #148852, .F. ) ;
#156549 = CARTESIAN_POINT ( 'NONE',  ( -5.641601317062259646, 5.754492089426966217, -0.7216878364870338292 ) ) ;
#156548 = CARTESIAN_POINT ( 'NONE',  ( -11.07790593930098311, 9.799999999999998934, 0.6999999999999992895 ) ) ;
#156551 = CARTESIAN_POINT ( 'NONE',  ( -6.278834536460198734, 6.497930845391236332, 0.7216878364870257245 ) ) ;
#156552 = CARTESIAN_POINT ( 'NONE',  ( 6.574778147984297938, 6.635272358928617997, -0.7998128361456481317 ) ) ;
#156553 = CARTESIAN_POINT ( 'NONE',  ( -6.330731382938325602, 6.350551133041632212, 0.7998128361456281477 ) ) ;
#156554 = CARTESIAN_POINT ( 'NONE',  ( 2.860025901456241471, 0.7249204854099660089, -1.885284610270787642 ) ) ;
#156555 = LINE ( 'NONE', #190097, #142549 ) ;
#156556 = CARTESIAN_POINT ( 'NONE',  ( 5.631924041214952936, -1.458266564992457104, -1.788428398515107043 ) ) ;
#156557 = DIRECTION ( 'NONE',  ( -0.6095094443598249034, 0.000000000000000000, -0.7927788072572181655 ) ) ;
#156558 = CARTESIAN_POINT ( 'NONE',  ( 2.641395077882053410, 1.795597516233004232, -0.7905247784146393064 ) ) ;
#156559 = CARTESIAN_POINT ( 'NONE',  ( 9.921869487102386032, 10.46993591124128997, 0.000000000000000000 ) ) ;
#156560 = CARTESIAN_POINT ( 'NONE',  ( 0.5631252389872200004, -1.117830369828230808, 1.678006741548984770 ) ) ;
#156561 = ORIENTED_EDGE ( 'NONE', *, *, #79408, .T. ) ;
#156562 = CARTESIAN_POINT ( 'NONE',  ( 2.184896953550282461, 1.697450634274371595, -1.265404921814163641 ) ) ;
#156564 = CARTESIAN_POINT ( 'NONE',  ( -5.856232286098998152, 8.919689202835742847, 1.199719254218452047 ) ) ;
#156563 = DIRECTION ( 'NONE',  ( 1.000000000000000000, -0.000000000000000000, -0.000000000000000000 ) ) ;
#156565 = CARTESIAN_POINT ( 'NONE',  ( 2.554438963407625884, -1.601868926591401232, -0.9074879233003440016 ) ) ;
#156566 = VERTEX_POINT ( 'NONE', #177157 ) ;
#156567 = CARTESIAN_POINT ( 'NONE',  ( -8.136864746495904299, 12.64475930422059768, -0.7998128361456281477 ) ) ;
#156568 = CARTESIAN_POINT ( 'NONE',  ( -1.419999999067559138, 7.203691543881443948, 4.238255391841873276 ) ) ;
#156570 = EDGE_CURVE ( 'NONE', #76889, #49812, #15698, .T. ) ;
#156569 = CARTESIAN_POINT ( 'NONE',  ( 4.517907016363444939, -0.5628432189327194912, 2.044499502628312371 ) ) ;
#156571 = CARTESIAN_POINT ( 'NONE',  ( 0.5152501731416662123, -0.9825955030486509534, -1.556829690179861281 ) ) ;
#156572 = CARTESIAN_POINT ( 'NONE',  ( 1.499999999999990896, 5.056250000682820378, 1.214306433183764966E-14 ) ) ;
#156573 = CARTESIAN_POINT ( 'NONE',  ( 7.588813295347141441, 9.876701482703580837, -1.599625672291262513 ) ) ;
#156574 = CARTESIAN_POINT ( 'NONE',  ( 7.364013710877980401, 8.620379413226322285, -1.199719254218452047 ) ) ;
#156575 = CARTESIAN_POINT ( 'NONE',  ( 4.200502791967850591, -0.6429285697095908914, -1.958015678616845445 ) ) ;
#156576 = CIRCLE ( 'NONE', #115190, 12.00000000000000178 ) ;
#156578 = CARTESIAN_POINT ( 'NONE',  ( 1.540310226958538475, -1.555040833713853710, 0.9856339240054690087 ) ) ;
#156577 = CARTESIAN_POINT ( 'NONE',  ( -6.191269702934848240, 10.37489842006599616, 0.000000000000000000 ) ) ;
#156579 = CARTESIAN_POINT ( 'NONE',  ( -1.001543065824772872E-14, 5.321875000341422357, 1.575800808251672791 ) ) ;
#156580 = FACE_OUTER_BOUND ( 'NONE', #117459, .T. ) ;
#156581 = CARTESIAN_POINT ( 'NONE',  ( 6.509000000000037645, 7.629137130509070275, 2.600000000000001421 ) ) ;
#156582 = CARTESIAN_POINT ( 'NONE',  ( 1.647397727484143592, -1.863059487452220386, 1.182652941231487453 ) ) ;
#156583 = CARTESIAN_POINT ( 'NONE',  ( 3.620660229735796154, 1.438486863682734818, -1.746180642158390084 ) ) ;
#156584 = CARTESIAN_POINT ( 'NONE',  ( -7.483737605063437215, 10.71448239167390604, 1.082531754730549967 ) ) ;
#156585 = CARTESIAN_POINT ( 'NONE',  ( 3.972783152890049241, -1.338232477621086547, 1.221218810135711541 ) ) ;
#156586 = CARTESIAN_POINT ( 'NONE',  ( 2.624132809847005365, 1.901796678110598382, 0.2296932149444090299 ) ) ;
#156587 = CARTESIAN_POINT ( 'NONE',  ( 3.824723168590526523, -1.392635068473629500, 1.532133406949770960 ) ) ;
#156588 = CARTESIAN_POINT ( 'NONE',  ( -1.364683531250012516, 3.551041667008086211, -0.7879004041258300672 ) ) ;
#156589 = CARTESIAN_POINT ( 'NONE',  ( 2.465646028844501902, 1.933766160897397057, -0.3828895411656701997 ) ) ;
#156590 = CARTESIAN_POINT ( 'NONE',  ( 0.5692023642799119987, 0.1922812221162081003, -1.916781067358761748 ) ) ;
#156591 = CARTESIAN_POINT ( 'NONE',  ( 4.223419137798128276, -1.790188510885984297, 0.5427707113358354318 ) ) ;
#156592 = CARTESIAN_POINT ( 'NONE',  ( 2.631810907782325071, -2.152760894471450914, 0.8317484501371147365 ) ) ;
#156593 = CARTESIAN_POINT ( 'NONE',  ( 4.123391753781197266, 0.2291962677869363585, -1.846827494033479455 ) ) ;
#156594 = CARTESIAN_POINT ( 'NONE',  ( -1.364683531249997417, 4.259375000341424133, 1.214306433183764966E-14 ) ) ;
#156595 =( GEOMETRIC_REPRESENTATION_CONTEXT ( 3 ) GLOBAL_UNCERTAINTY_ASSIGNED_CONTEXT ( ( #95231 ) ) GLOBAL_UNIT_ASSIGNED_CONTEXT ( ( #120207, #165559, #198048 ) ) REPRESENTATION_CONTEXT ( 'NONE', 'WORKASPACE' ) );
#156597 = CARTESIAN_POINT ( 'NONE',  ( -5.436983294280064882, 6.301900917203534291, 1.199719254218450271 ) ) ;
#156596 = COLOUR_RGB ( '', 0.40784314, 0.44705882, 0.49803922) ;
#156598 = CARTESIAN_POINT ( 'NONE',  ( 6.959412922516382771, 7.013736585890911535, 0.7998128361456341429 ) ) ;
#156599 = CARTESIAN_POINT ( 'NONE',  ( 6.643335646896344038, -7.986884274785886362, 6.845108005540233798 ) ) ;
#156600 = ADVANCED_FACE ( 'NONE', ( #79651 ), #94967, .T. ) ;
#156601 = CARTESIAN_POINT ( 'NONE',  ( 0.3992258182855871196, 1.749727718737997373, -1.171850562161039777 ) ) ;
#156602 = CARTESIAN_POINT ( 'NONE',  ( 4.216222583725566686, 4.981643104843690217, -1.082531754730548412 ) ) ;
#156604 = CARTESIAN_POINT ( 'NONE',  ( -0.6311622855796928944, 3.199999999999994404, 0.3999999999999611644 ) ) ;
#156603 = CARTESIAN_POINT ( 'NONE',  ( -1.364683531250012516, 4.051041667008088432, -0.7879004041258300672 ) ) ;
#156605 = CARTESIAN_POINT ( 'NONE',  ( 6.837200347746460238, -1.934230338078479550, 0.9651617863762136373 ) ) ;
#156606 = CARTESIAN_POINT ( 'NONE',  ( 1.670341986359990205, 2.114562342887704283, -0.1611296783964668855 ) ) ;
#156607 = CARTESIAN_POINT ( 'NONE',  ( 0.3166733070498818359, -0.6846287639105748113, -1.900330225253379801 ) ) ;
#156608 = CARTESIAN_POINT ( 'NONE',  ( -1.364683531250000748, 1.259375000341421469, 0.000000000000000000 ) ) ;
#156609 = CARTESIAN_POINT ( 'NONE',  ( -3.741687207691642314, 6.348756928073427730, 1.082531754730560403 ) ) ;
#156610 = CARTESIAN_POINT ( 'NONE',  ( 5.311043488251262268, 7.219303374425030562, -1.599625672291256295 ) ) ;
#156611 = CARTESIAN_POINT ( 'NONE',  ( 1.001511639980020130, 1.766541945284912263, 1.245431700958275600 ) ) ;
#156614 = CARTESIAN_POINT ( 'NONE',  ( 4.690757960648234359, 4.574898496952131133, 0.7216878364870317197 ) ) ;
#156613 = CARTESIAN_POINT ( 'NONE',  ( 6.825078400183516081, 0.5802287360496224400, 2.007770452540482697 ) ) ;
#156612 = CARTESIAN_POINT ( 'NONE',  ( 5.091969210384201361, 8.098325291160362482, 1.199719254218452047 ) ) ;
#156615 = DIRECTION ( 'NONE',  ( 0.000000000000000000, 0.000000000000000000, 1.000000000000000000 ) ) ;
#156616 = CARTESIAN_POINT ( 'NONE',  ( 5.682827415814322158, 1.645762192317705486, -1.164983060713747909 ) ) ;
#156618 = CARTESIAN_POINT ( 'NONE',  ( -6.007671464186866928, 8.102312356341712984, 1.443375672974058777 ) ) ;
#156617 = CARTESIAN_POINT ( 'NONE',  ( -9.327646496521992958, 9.984601788804893019, -0.7216878364870267237 ) ) ;
#156619 = CARTESIAN_POINT ( 'NONE',  ( 0.000000000000000000, -1.600000000000000755, 0.000000000000000000 ) ) ;
#156621 = CARTESIAN_POINT ( 'NONE',  ( -1.364683531250014514, 10.58854166700806765, -0.7879004041258335089 ) ) ;
#156620 = CARTESIAN_POINT ( 'NONE',  ( 0.5853300251711880398, -0.2802842603415867107, -2.245014038439311577 ) ) ;
#156622 = CARTESIAN_POINT ( 'NONE',  ( -9.917953063596627317, 11.52969898140628047, -1.199719254218441611 ) ) ;
#156624 = CARTESIAN_POINT ( 'NONE',  ( 1.423292265346193464, -1.388624197914482883, -1.319832876491247697 ) ) ;
#156623 = CARTESIAN_POINT ( 'NONE',  ( -5.382223794500843539, 7.302347065049529462, -1.443375672974051449 ) ) ;
#156625 = CARTESIAN_POINT ( 'NONE',  ( -1.364683531250014514, 0.8010416670080889867, -0.7879004041258289570 ) ) ;
#156626 = CARTESIAN_POINT ( 'NONE',  ( 3.147653791585693028, 8.920000000000001705, 2.499999999999999556 ) ) ;
#156627 = CIRCLE ( 'NONE', #104828, 10.99999999999999112 ) ;
#156628 = CARTESIAN_POINT ( 'NONE',  ( 0.7500000000000006661, 8.583333333333332149, 1.299038105676657340 ) ) ;
#156629 = CARTESIAN_POINT ( 'NONE',  ( 2.525662786804376836, -0.9926222177696201188, -1.410421675411769993 ) ) ;
#156630 = CARTESIAN_POINT ( 'NONE',  ( 7.075376061485196821, 9.347967719856493218, 1.599625672291268286 ) ) ;
#156631 = CARTESIAN_POINT ( 'NONE',  ( 3.528865121306874464, 7.339036084825155015, -0.7998128361456362523 ) ) ;
#156632 = CARTESIAN_POINT ( 'NONE',  ( 0.7371257246046484246, -1.245724469572104587, -1.257322912719664787 ) ) ;
#156633 = CARTESIAN_POINT ( 'NONE',  ( 1.471341131262299706, -1.727646810417843959, -1.033094421854539036 ) ) ;
#156634 = CARTESIAN_POINT ( 'NONE',  ( 3.716033540554028125, -2.174548934981130444, 0.3748234698989146851 ) ) ;
#156635 = ORIENTED_EDGE ( 'NONE', *, *, #13181, .F. ) ;
#156636 = CARTESIAN_POINT ( 'NONE',  ( 9.395437264145964917, 10.06369101769952934, -0.7216878364870257245 ) ) ;
#156637 = CARTESIAN_POINT ( 'NONE',  ( -7.533490631048818109, 8.818102486758951031, -1.199719254218452047 ) ) ;
#156639 = CARTESIAN_POINT ( 'NONE',  ( 4.534779904478015489, -1.617806963314952773, 1.203370736114671269 ) ) ;
#156638 = CARTESIAN_POINT ( 'NONE',  ( 4.055424778641623540, -1.844328037693225397, 1.046277804987456372 ) ) ;
#156641 = ORIENTED_EDGE ( 'NONE', *, *, #191456, .T. ) ;
#156640 = CARTESIAN_POINT ( 'NONE',  ( 3.673895663291579350, 1.797233291820631962, -0.2271657407440821064 ) ) ;
#156642 = CARTESIAN_POINT ( 'NONE',  ( 4.549643065837591038, 7.465611455855944101, -1.199719254218452047 ) ) ;
#156643 = ORIENTED_EDGE ( 'NONE', *, *, #84877, .F. ) ;
#156644 = CARTESIAN_POINT ( 'NONE',  ( 1.094370286708164386, -0.4508366001288487968, -1.815394955969009461 ) ) ;
#156645 = CARTESIAN_POINT ( 'NONE',  ( 5.760330229460346452, 0.7440287100829169331, 1.667389206893993725 ) ) ;
#156646 = LINE ( 'NONE', #88443, #209301 ) ;
#156647 = CARTESIAN_POINT ( 'NONE',  ( -1.286956418854606543, 4.047654341997520611, 0.4592741676706140197 ) ) ;
#156648 = CARTESIAN_POINT ( 'NONE',  ( -3.946537740505278613, 2.817530495244580102, 0.7750000000000135669 ) ) ;
#156649 = CARTESIAN_POINT ( 'NONE',  ( -1.364683531250012516, 1.342708333674755616, 0.7879004041258379498 ) ) ;
#156650 = DIRECTION ( 'NONE',  ( 0.000000000000000000, -1.000000000000000000, -0.000000000000000000 ) ) ;
#156651 = CARTESIAN_POINT ( 'NONE',  ( 6.536439455564155843, 8.719208346281938304, 1.443375672974065660 ) ) ;
#156652 = CARTESIAN_POINT ( 'NONE',  ( -4.502716413514313842, 5.386162249589033557, -1.082531754730549967 ) ) ;
#156653 = CARTESIAN_POINT ( 'NONE',  ( -6.180537922983287302, 8.303989891604203422, -1.599625672291271394 ) ) ;
#156654 = CARTESIAN_POINT ( 'NONE',  ( 4.096021571020786567, 1.387573888390711385, 1.603661410755026440 ) ) ;
#156656 = CARTESIAN_POINT ( 'NONE',  ( -10.85762644215163775, 5.701980886241464042, -6.452002860825420960 ) ) ;
#156655 = CARTESIAN_POINT ( 'NONE',  ( -0.02968770228140016343, 1.391517546076680434, -2.083419219542380407 ) ) ;
#156657 = B_SPLINE_CURVE_WITH_KNOTS ( 'NONE', 3,
 ( #175621, #126943, #27208, #93314, #159350, #12025, #207024, #173499, #56525, #157236 ),
 .UNSPECIFIED., .F., .F.,
 ( 4, 2, 2, 2, 4 ),
 ( 2.453269466693236920E-18, 0.0002503535593264603985, 0.0005007071186529184117, 0.0007510606779793763165, 0.001001414237305834221 ),
 .UNSPECIFIED. ) ;
#156658 = CARTESIAN_POINT ( 'NONE',  ( 3.954335293022055886, 0.7064427249091516092, 1.840614667007954841 ) ) ;
#156659 = CARTESIAN_POINT ( 'NONE',  ( -1.364683531250014514, 1.238541667008091096, -0.7879004041258289570 ) ) ;
#156660 = CARTESIAN_POINT ( 'NONE',  ( 6.486579876843341808, -1.171037552013409089, 1.512559164390047783 ) ) ;
#156661 = ORIENTED_EDGE ( 'NONE', *, *, #212430, .F. ) ;
#156662 = CARTESIAN_POINT ( 'NONE',  ( 0.2634788376212302552, 1.973769265480609381, -0.7665230665306818070 ) ) ;
#156663 = CARTESIAN_POINT ( 'NONE',  ( 7.872268696974136226, 14.32328115913407096, 9.059783805236799381 ) ) ;
#156664 = CARTESIAN_POINT ( 'NONE',  ( 0.9946828900261883710, 2.039433816042154124, 0.3556643922909968891 ) ) ;
#156665 = CARTESIAN_POINT ( 'NONE',  ( 7.354371980770088690, 7.544798497178720531, 0.000000000000000000 ) ) ;
#156666 = CARTESIAN_POINT ( 'NONE',  ( 5.529746549527311039, 7.544733289238903851, -1.599625672291281386 ) ) ;
#156667 = CARTESIAN_POINT ( 'NONE',  ( 7.713663051532233972, 7.963971413067895355, -0.7998128361456341429 ) ) ;
#156669 = CARTESIAN_POINT ( 'NONE',  ( 5.840865249388943248, 5.708764300575555062, 0.7998128361456341429 ) ) ;
#156668 = CARTESIAN_POINT ( 'NONE',  ( 3.960945476642624641, 0.2557261242597759776, -2.074860007841982767 ) ) ;
#156670 = CARTESIAN_POINT ( 'NONE',  ( 6.200875153403774043, 8.327716660428123419, -1.599625672291283607 ) ) ;
#156672 = CARTESIAN_POINT ( 'NONE',  ( 1.189788175852508845, 1.078664940389061577, 1.455116354534333079 ) ) ;
#156671 = CARTESIAN_POINT ( 'NONE',  ( 1.781981981289095796, -0.9795585948506604357, 1.540336029244721461 ) ) ;
#156673 = CARTESIAN_POINT ( 'NONE',  ( 6.076841795016812320, -2.094286673724785164, -0.6961510500591641115 ) ) ;
#156674 = DIRECTION ( 'NONE',  ( -0.000000000000000000, -1.000000000000000000, 0.000000000000000000 ) ) ;
#156675 = CARTESIAN_POINT ( 'NONE',  ( 4.032405518703926717, 1.182977813604596973, -1.862726815517960821 ) ) ;
#156676 = CARTESIAN_POINT ( 'NONE',  ( 6.500244582748090139, 9.671036882259738121, 1.199719254218460707 ) ) ;
#156677 = CARTESIAN_POINT ( 'NONE',  ( -1.364683531250000748, 8.421875000341403350, 0.000000000000000000 ) ) ;
#156678 = CARTESIAN_POINT ( 'NONE',  ( 2.420441844550869526, -0.7335502799032425081, -1.766186906296034698 ) ) ;
#156679 = VECTOR ( 'NONE', #69847, 1000.000000000000000 ) ;
#156680 = CARTESIAN_POINT ( 'NONE',  ( 8.422639742587595180, 10.84949900448412130, -1.599625672291268286 ) ) ;
#156681 = CARTESIAN_POINT ( 'NONE',  ( 4.844224204019831781, -0.9789346907586125024, 1.824324395707350943 ) ) ;
#156682 = CIRCLE ( 'NONE', #52918, 0.7499999999999997780 ) ;
#156684 = CARTESIAN_POINT ( 'NONE',  ( -2.428612866367529932E-14, -1.099999999999976108, 2.499999999999998668 ) ) ;
#156683 = CARTESIAN_POINT ( 'NONE',  ( 1.499999999999990896, 8.627523663848661428, -2.579999999999989413 ) ) ;
#156685 = CARTESIAN_POINT ( 'NONE',  ( 6.269083535738129598, 2.097726667780253074, -0.6343229546324488100 ) ) ;
#156686 = ORIENTED_EDGE ( 'NONE', *, *, #140696, .F. ) ;
#156687 = VERTEX_POINT ( 'NONE', #161988 ) ;
#156688 = CARTESIAN_POINT ( 'NONE',  ( -11.41267819554183127, 3.447199233515635619, 3.708203932499423150 ) ) ;
#156689 = DIRECTION ( 'NONE',  ( -3.330669073875478989E-16, 3.330669073875478989E-16, 1.000000000000000000 ) ) ;
#156690 = EDGE_CURVE ( 'NONE', #156842, #156205, #8499, .T. ) ;
#156691 = CARTESIAN_POINT ( 'NONE',  ( 5.248941747146098180, 6.152795455539095570, -1.199719254218452047 ) ) ;
#156692 = CARTESIAN_POINT ( 'NONE',  ( 3.285556943750000514, -1.801041666188707202, 1.896917185911906722 ) ) ;
#156693 = SPHERICAL_SURFACE ( 'NONE', #153825, 0.08000000000000000167 ) ;
#156694 = CARTESIAN_POINT ( 'NONE',  ( -7.049876689426097798, 11.16868053773170821, -0.7216878364870267237 ) ) ;
#156695 = CARTESIAN_POINT ( 'NONE',  ( 3.400062661977048428, 7.188766548940353829, -1.734723475976807094E-15 ) ) ;
#156696 = CARTESIAN_POINT ( 'NONE',  ( 5.577033793921920335, 1.910671465402475677, 0.7975372692515869666 ) ) ;
#156697 = CARTESIAN_POINT ( 'NONE',  ( 4.600175520841607302, -1.926116679539988885, -0.04579137001822254638 ) ) ;
#156698 = CARTESIAN_POINT ( 'NONE',  ( 0.1050925082292548940, -0.09611335402343046397, 2.014234898253919326 ) ) ;
#156699 = DIRECTION ( 'NONE',  ( -1.000000000000000000, -3.451266460341927087E-31, -8.638326563840810896E-31 ) ) ;
#156700 = CARTESIAN_POINT ( 'NONE',  ( 4.543917759235442944, 5.330267469643351852, 1.199719254218452935 ) ) ;
#156701 = CARTESIAN_POINT ( 'NONE',  ( 0.000000000000000000, 15.00000000000000000, -12.18000000000000149 ) ) ;
#156702 = CARTESIAN_POINT ( 'NONE',  ( 6.597627758599571735, -2.291905675289906519, 0.04924309260747637695 ) ) ;
#156703 = CARTESIAN_POINT ( 'NONE',  ( 5.057177669875371429, -1.544152220135000420, -0.9737345633797565014 ) ) ;
#156704 = EDGE_CURVE ( 'NONE', #160443, #185175, #211768, .T. ) ;
#156705 = CARTESIAN_POINT ( 'NONE',  ( 5.072158865288233898, 7.971250205261355859, 1.082531754730549078 ) ) ;
#156706 = CARTESIAN_POINT ( 'NONE',  ( 3.755245360860917536, 5.404205559136275205, -1.443375672974051449 ) ) ;
#156707 = CARTESIAN_POINT ( 'NONE',  ( -6.967964602780620353, 7.093989889524320525, 0.000000000000000000 ) ) ;
#156708 = CARTESIAN_POINT ( 'NONE',  ( 5.366329872910639232, 5.155139694684188534, 1.040834085586084257E-14 ) ) ;
#156709 = CARTESIAN_POINT ( 'NONE',  ( 5.713835393516482952, 5.630839145382857680, 0.7998128361456352531 ) ) ;
#156710 = EDGE_LOOP ( 'NONE', ( #148290, #129198, #70828, #57165 ) ) ;
#156712 = CARTESIAN_POINT ( 'NONE',  ( -0.05795285570054254515, -1.240470478354677164, -1.586248892985191006 ) ) ;
#156711 = CARTESIAN_POINT ( 'NONE',  ( 2.981803241483144351, -1.814435276338403735, -0.3121031562058202424 ) ) ;
#156713 = CARTESIAN_POINT ( 'NONE',  ( 0.8085102987360716087, -1.969961327451934086, 1.183767188307288221 ) ) ;
#156714 = CARTESIAN_POINT ( 'NONE',  ( 6.543807102324334934, 1.350441955444921849, 1.423202910149905298 ) ) ;
#156715 = CARTESIAN_POINT ( 'NONE',  ( -4.771579997005698459, 7.654261532226910525, -1.199719254218452047 ) ) ;
#156716 = CARTESIAN_POINT ( 'NONE',  ( -3.945059511896602089, 7.546393830613923548, 1.040834085586084257E-14 ) ) ;
#156717 = CARTESIAN_POINT ( 'NONE',  ( -4.647747731386360215, 4.316793862905830892, 0.7998128361456341429 ) ) ;
#156718 = CARTESIAN_POINT ( 'NONE',  ( 0.3442982867475213871, -0.9772804826688463731, 1.825211318103404867 ) ) ;
#156719 = CARTESIAN_POINT ( 'NONE',  ( -2.986538976760251263, 6.706322249520737522, -0.7998128361456481317 ) ) ;
#156721 = CARTESIAN_POINT ( 'NONE',  ( 1.252583056964752029, -1.476889893665521925, 1.148006582770304096 ) ) ;
#156720 = CARTESIAN_POINT ( 'NONE',  ( 2.577772492168933116, -1.072305133946813260, 1.794659622045821079 ) ) ;
#156722 = CARTESIAN_POINT ( 'NONE',  ( 1.493517298738750609, 1.942243344100362590, 0.5404107738020345053 ) ) ;
#156723 = CARTESIAN_POINT ( 'NONE',  ( 8.595506201384008449, 11.05117653974661529, 1.443375672974076540 ) ) ;
#156724 = VERTEX_POINT ( 'NONE', #127432 ) ;
#156725 = CARTESIAN_POINT ( 'NONE',  ( 0.6823417656249917140, 4.655208333674755394, 1.181850606188765695 ) ) ;
#156726 = CARTESIAN_POINT ( 'NONE',  ( 1.997219015684068344, -1.740079325084613604, 0.04332556902747128347 ) ) ;
#156727 = CIRCLE ( 'NONE', #191322, 2.000000000000006217 ) ;
#156728 = CARTESIAN_POINT ( 'NONE',  ( 4.904298879841284098, 6.744767997946721216, 1.599625672291267398 ) ) ;
#156730 = DIRECTION ( 'NONE',  ( 0.000000000000000000, -1.000000000000000000, 0.000000000000000000 ) ) ;
#156729 = DIRECTION ( 'NONE',  ( -0.7592566023653017915, -0.6507913734559624963, 9.298211678181604981E-17 ) ) ;
#156731 = CARTESIAN_POINT ( 'NONE',  ( 3.316762602600237475, 1.559927958434914608, 0.7363868292221543710 ) ) ;
#156732 = CARTESIAN_POINT ( 'NONE',  ( 3.175498511859841333, 1.392037702009111033, 1.692654053968026151 ) ) ;
#156733 = CARTESIAN_POINT ( 'NONE',  ( 4.864015066594513215, 2.183220759563545776, -0.3215228633955333759 ) ) ;
#156734 = CARTESIAN_POINT ( 'NONE',  ( -10.65086514279933994, 4.118349190211191058, -6.883315229069521202 ) ) ;
#156735 = CARTESIAN_POINT ( 'NONE',  ( 2.747136105846450516, -0.3671824478193272956, -2.139636267262314373 ) ) ;
#156736 = CARTESIAN_POINT ( 'NONE',  ( 0.9085097582094739943, 1.384192474337717194, -1.190531929384466281 ) ) ;
#156737 = CARTESIAN_POINT ( 'NONE',  ( 4.944582029040364368, -1.531444570474638667, 1.462332997386527556 ) ) ;
#156738 = CARTESIAN_POINT ( 'NONE',  ( -3.294268138440636928, 6.787137228248626641, 1.040834085586084257E-14 ) ) ;
#156739 = EDGE_CURVE ( 'NONE', #93560, #3330, #14632, .T. ) ;
#156740 = ORIENTED_EDGE ( 'NONE', *, *, #32247, .T. ) ;
#156742 = CARTESIAN_POINT ( 'NONE',  ( 0.6823417656249899377, 1.405208333674752508, 1.181850606188755259 ) ) ;
#156741 = CARTESIAN_POINT ( 'NONE',  ( 4.915721525821019178, -1.224934246408443839, -1.937497040551818150 ) ) ;
#156743 = CARTESIAN_POINT ( 'NONE',  ( 1.224999999999989875, 2.624999999999995559, -2.255140518769849223E-14 ) ) ;
#156744 = CARTESIAN_POINT ( 'NONE',  ( 3.408985558832261731, 6.064568021024562938, 1.199719254218462483 ) ) ;
#156745 = CARTESIAN_POINT ( 'NONE',  ( 0.8387270772249322270, 1.259995426201226953, -1.705408266269872630 ) ) ;
#156746 = CARTESIAN_POINT ( 'NONE',  ( -5.422898255786193111, 8.310169817517122581, -1.082531754730544860 ) ) ;
#156747 = CARTESIAN_POINT ( 'NONE',  ( 4.378920427533921078, 4.211088041652093494, 1.214306433183764966E-14 ) ) ;
#156748 = PRESENTATION_LAYER_ASSIGNMENT (  '', '', ( #35651 ) ) ;
#156749 = CARTESIAN_POINT ( 'NONE',  ( -7.348156068482412095, 7.675196289425353591, 1.040834085586084257E-14 ) ) ;
#156750 = AXIS2_PLACEMENT_3D ( 'NONE', #166579, #18166, #5105 ) ;
#156751 = CARTESIAN_POINT ( 'NONE',  ( 3.851925040058331806, 5.587274861525073355, -1.443375672974066548 ) ) ;
#156752 = EDGE_LOOP ( 'NONE', ( #134599, #68276, #178297, #211255 ) ) ;
#156753 = CARTESIAN_POINT ( 'NONE',  ( 5.520157785563180930, -1.821743191724470634, 0.8647220171385738841 ) ) ;
#156755 = CARTESIAN_POINT ( 'NONE',  ( 3.432538798476657327, -1.232314722524804562, 1.653799735942045990 ) ) ;
#156754 = CARTESIAN_POINT ( 'NONE',  ( 5.931855901178834323, 6.879252291918818152, 1.199719254218462483 ) ) ;
#156757 = CARTESIAN_POINT ( 'NONE',  ( -0.1409997244346088141, 2.874455162768466909, -2.488748179275114492 ) ) ;
#156756 = CARTESIAN_POINT ( 'NONE',  ( 6.994027139803230320, 9.253060644560830994, -1.599625672291267398 ) ) ;
#156758 = EDGE_CURVE ( 'NONE', #56213, #182554, #139968, .T. ) ;
#156759 = CARTESIAN_POINT ( 'NONE',  ( 6.502017186205484300, 9.743381262951846367, -1.199719254218452047 ) ) ;
#156760 = CARTESIAN_POINT ( 'NONE',  ( -3.285556943750000070, -3.959374999522043304, 0.000000000000000000 ) ) ;
#156761 = CARTESIAN_POINT ( 'NONE',  ( 6.369083545433415594, 2.098215621258665564, -0.6323776016037768732 ) ) ;
#156762 = CARTESIAN_POINT ( 'NONE',  ( 3.674454069786535548, 1.462445212485608437, 1.388486266691544957 ) ) ;
#156763 = CARTESIAN_POINT ( 'NONE',  ( 3.104851637799400876, -0.3563606998662186554, 1.806257425991746546 ) ) ;
#156764 = EDGE_CURVE ( 'NONE', #173456, #113953, #74231, .T. ) ;
#156765 = CARTESIAN_POINT ( 'NONE',  ( 7.091078035147269532, 8.231678114882006625, 1.199719254218462483 ) ) ;
#156766 = SHAPE_REPRESENTATION_RELATIONSHIP ( 'NONE' , 'NONE' ,  #142805, #194826 ) ;
#156767 = CARTESIAN_POINT ( 'NONE',  ( 0.1293586867831516274, -1.054425554818343880, -1.365251215659948558 ) ) ;
#156768 = AXIS2_PLACEMENT_3D ( 'NONE', #207880, #125660, #191622 ) ;
#156769 = CARTESIAN_POINT ( 'NONE',  ( -7.874588291438845644, 8.081441182967111558, -0.7998128361456291469 ) ) ;
#156770 = CARTESIAN_POINT ( 'NONE',  ( 6.473497647428577473, 2.167417048064937291, -0.6491153028224846411 ) ) ;
#156771 = CARTESIAN_POINT ( 'NONE',  ( 1.735132801782751200, 0.2076089413485527335, 2.095809512812545350 ) ) ;
#156772 = CARTESIAN_POINT ( 'NONE',  ( -6.784929528996132220, 6.880448970109080520, 0.000000000000000000 ) ) ;
#156773 = CARTESIAN_POINT ( 'NONE',  ( 7.052212457402625922, 11.37933163361175382, -0.7998128361456291469 ) ) ;
#156774 = CARTESIAN_POINT ( 'NONE',  ( 6.658462837642789012, 9.821938173008357253, 1.082531754730549078 ) ) ;
#156775 = CARTESIAN_POINT ( 'NONE',  ( 8.378074386687000441, 10.50815134976859078, 15.76159487570644480 ) ) ;
#156776 = CARTESIAN_POINT ( 'NONE',  ( -6.847031270101295419, 7.946956888995021728, -1.199719254218446718 ) ) ;
#156777 = CARTESIAN_POINT ( 'NONE',  ( 8.419250203962011625, 8.924806114151579095, -0.7216878364870267237 ) ) ;
#156778 = CARTESIAN_POINT ( 'NONE',  ( 4.002182886544830787, 7.824783036946191039, -0.1358892651178236766 ) ) ;
#156779 = CIRCLE ( 'NONE', #4578, 0.8299999999999999600 ) ;
#156780 = CARTESIAN_POINT ( 'NONE',  ( -3.425406365747000859, 7.148057860013469877, 1.040834085586084257E-14 ) ) ;
#156781 = CARTESIAN_POINT ( 'NONE',  ( 4.008219027074312990, -0.8479933951243652235, 2.053374474559205520 ) ) ;
#156782 = CARTESIAN_POINT ( 'NONE',  ( 2.326364362698669641, 2.126017103801054464, 0.5310240739047759062 ) ) ;
#156783 = CARTESIAN_POINT ( 'NONE',  ( 0.4873205249028254027, -0.2742316277877173691, -2.189713876267186166 ) ) ;
#156784 = CARTESIAN_POINT ( 'NONE',  ( -5.971440312176176768, 5.931378217152456500, 0.000000000000000000 ) ) ;
#156785 = CARTESIAN_POINT ( 'NONE',  ( 4.562918044398325712, 1.517878595006398212, -1.242988302126393441 ) ) ;
#156786 = CARTESIAN_POINT ( 'NONE',  ( 9.915090410295563927, 10.46202698829998567, -0.7998128361456281477 ) ) ;
#156787 =( BOUNDED_CURVE ( )  B_SPLINE_CURVE ( 2, ( #15360, #79319, #129234, #148589, #193054, #81453, #82502, #145435, #65174 ),
 .UNSPECIFIED., .F., .T. ) 
 B_SPLINE_CURVE_WITH_KNOTS ( ( 3, 2, 2, 2, 3 ),
 ( 0.3125000000000000000, 0.3194444444444444198, 0.3333333333333333148, 0.3472222222222222099, 0.3541666666666666852 ),
 .UNSPECIFIED. ) 
 CURVE ( )  GEOMETRIC_REPRESENTATION_ITEM ( )  RATIONAL_B_SPLINE_CURVE ( ( 0.9330127018922194093, 0.9330127018922194093, 1.000000000000000000, 0.8660254037844387076, 1.000000000000000000, 0.8660254037844387076, 1.000000000000000000, 0.9330127018922190762, 0.9330127018922194093 ) ) 
 REPRESENTATION_ITEM ( '' )  );
#156788 = CARTESIAN_POINT ( 'NONE',  ( -1.364683531250012516, 0.5302083336747518416, 0.7879004041258379498 ) ) ;
#156789 = CARTESIAN_POINT ( 'NONE',  ( 6.610000000000006537, 2.052567036419289614, 2.306714106643445561 ) ) ;
#156791 = VERTEX_POINT ( 'NONE', #179303 ) ;
#156790 = CARTESIAN_POINT ( 'NONE',  ( -5.205967797967562483, 8.057084283395347768, 1.082531754730548412 ) ) ;
#156792 = CARTESIAN_POINT ( 'NONE',  ( 3.023802379225454473, -0.4096935937694180518, 2.080477853870852378 ) ) ;
#156793 = CARTESIAN_POINT ( 'NONE',  ( -3.135678666510573365, 6.880318554229450712, 0.000000000000000000 ) ) ;
#156794 = CARTESIAN_POINT ( 'NONE',  ( 4.979442225389012933, 2.018306902694905425, -0.7746836383674888804 ) ) ;
#156795 = CARTESIAN_POINT ( 'NONE',  ( 4.124425300631988200, 0.09459923933386081563, 1.838956108544815171 ) ) ;
#156796 = CARTESIAN_POINT ( 'NONE',  ( 11.97929049433705373, 11.37999999999999901, -0.7046979865771834106 ) ) ;
#156797 = CARTESIAN_POINT ( 'NONE',  ( -1.364683531250014514, 1.551041667008084435, -0.7879004041258289570 ) ) ;
#156798 = CARTESIAN_POINT ( 'NONE',  ( 6.703062861115646420, -0.3699031437116198084, 1.706546720392573491 ) ) ;
#156799 = CARTESIAN_POINT ( 'NONE',  ( 6.827182134110164391, 0.6048993162116442779, 1.764860727632423076 ) ) ;
#156800 = CARTESIAN_POINT ( 'NONE',  ( 2.575685996916329046, 5.948791396470269888, 0.7216878364870438212 ) ) ;
#156801 = CARTESIAN_POINT ( 'NONE',  ( -0.1000000000000028644, -9.999999999999994671, -9.579478065113972818 ) ) ;
#156802 = CARTESIAN_POINT ( 'NONE',  ( 3.801785103514757846, -0.6297183656660889639, 2.067937956787009757 ) ) ;
#156803 = CARTESIAN_POINT ( 'NONE',  ( -4.273844736805832767, 6.009238164405336313, 1.599625672291267398 ) ) ;
#156804 = CARTESIAN_POINT ( 'NONE',  ( 5.114611164699836010, 0.6351010243071940620, -1.913510948406547563 ) ) ;
#156805 = CARTESIAN_POINT ( 'NONE',  ( -8.039621902779392926, 9.442275643739831636, 1.082531754730558626 ) ) ;
#156806 = CARTESIAN_POINT ( 'NONE',  ( 3.749029689823797806, -1.768526636652943296, 1.242828150824742961 ) ) ;
#156807 = CARTESIAN_POINT ( 'NONE',  ( 4.147701676541888816, 0.6670536769024897339, -1.855179015784082619 ) ) ;
#156808 = CARTESIAN_POINT ( 'NONE',  ( -0.2435857797690326454, -7.709701271428947678, 10.99755231369147523 ) ) ;
#156809 = CARTESIAN_POINT ( 'NONE',  ( 0.6402171227658737251, -1.634652429315278654, -1.629011242183490804 ) ) ;
#156810 = CARTESIAN_POINT ( 'NONE',  ( 4.147771190963340793, 0.6980094919085011451, -1.939086781881957933 ) ) ;
#156811 = CARTESIAN_POINT ( 'NONE',  ( 6.163619218806376310, 1.002299704222510357, 1.663313343435903091 ) ) ;
#156812 = CARTESIAN_POINT ( 'NONE',  ( -8.961576348508655698, 9.557519949455999253, -0.7216878364870267237 ) ) ;
#156813 = CARTESIAN_POINT ( 'NONE',  ( -5.794130544993808307, 7.853181283949808744, 1.599625672291263179 ) ) ;
#156814 = CYLINDRICAL_SURFACE ( 'NONE', #64616, 1.500000000000000222 ) ;
#156816 = ORIENTED_EDGE ( 'NONE', *, *, #18383, .T. ) ;
#156815 = CARTESIAN_POINT ( 'NONE',  ( -5.015590482412729756, 4.816220082428420923, 0.000000000000000000 ) ) ;
#156817 = CARTESIAN_POINT ( 'NONE',  ( -7.822691444960709006, 10.14955932391940330, -1.443375672974058777 ) ) ;
#156818 = CARTESIAN_POINT ( 'NONE',  ( 2.608667852368121043, -0.8438080161984360394, -2.039271889284439254 ) ) ;
#156819 = CARTESIAN_POINT ( 'NONE',  ( 3.285556943749998737, -0.2552083328553768071, -1.896917185911906500 ) ) ;
#156820 = ORIENTED_EDGE ( 'NONE', *, *, #186606, .T. ) ;
#156821 = CARTESIAN_POINT ( 'NONE',  ( 6.350445966956749899, -1.952004966925089624, -0.1956573963535559180 ) ) ;
#156822 = CARTESIAN_POINT ( 'NONE',  ( -0.02900071798682749002, 0.2267074960015900975, -2.207170277039482986 ) ) ;
#156823 = DIRECTION ( 'NONE',  ( 0.000000000000000000, 0.000000000000000000, -1.000000000000000000 ) ) ;
#156824 = DIRECTION ( 'NONE',  ( 1.000000000000000000, -0.000000000000000000, -0.000000000000000000 ) ) ;
#156826 = DIRECTION ( 'NONE',  ( 0.000000000000000000, 0.000000000000000000, -1.000000000000000000 ) ) ;
#156825 = CARTESIAN_POINT ( 'NONE',  ( 0.7499999999999902300, 5.097916667349482012, -1.299038105676658228 ) ) ;
#156827 = CARTESIAN_POINT ( 'NONE',  ( 5.665905727187005247, -1.164751086281138770, 1.425882759469448979 ) ) ;
#156828 = ORIENTED_EDGE ( 'NONE', *, *, #164628, .F. ) ;
#156829 = CARTESIAN_POINT ( 'NONE',  ( 2.289980725320222010, -0.8822103741390595610, 1.862666789336121509 ) ) ;
#156830 = CARTESIAN_POINT ( 'NONE',  ( 0.6801582343749970061, 0.8072916670080754198, -1.178068619123858962 ) ) ;
#156831 = CARTESIAN_POINT ( 'NONE',  ( -6.344325816190970357, 9.489131654609717970, 1.199719254218452047 ) ) ;
#156832 = CARTESIAN_POINT ( 'NONE',  ( 11.07131242353766254, 13.80000000000000071, -0.8043462106219256835 ) ) ;
#156833 = ADVANCED_FACE ( 'NONE', ( #97000 ), #11905, .T. ) ;
#156834 = CARTESIAN_POINT ( 'NONE',  ( 4.150767584078112193, 7.994312614733129152, 0.7998128361456321445 ) ) ;
#156835 = CARTESIAN_POINT ( 'NONE',  ( 0.5849274615713345726, -0.2514902370338990001, -2.045404637917444646 ) ) ;
#156837 = CARTESIAN_POINT ( 'NONE',  ( 4.915489835137424102, -0.9894786724786635013, -1.552603174752004600 ) ) ;
#156836 = CARTESIAN_POINT ( 'NONE',  ( 4.875577028304626914, 4.957510466404852600, 0.6186772747242745840 ) ) ;
#156838 = CARTESIAN_POINT ( 'NONE',  ( 6.632963465583686435, 8.761543347979550589, -1.599625672291262513 ) ) ;
#156839 = CONICAL_SURFACE ( 'NONE', #143108, 11.53746066217574473, 0.1181278931043537039 ) ;
#156840 = CARTESIAN_POINT ( 'NONE',  ( -6.967964602780620353, 7.093989889524320525, 0.000000000000000000 ) ) ;
#156842 = VERTEX_POINT ( 'NONE', #28776 ) ;
#156841 = CARTESIAN_POINT ( 'NONE',  ( 2.734094378161750605, 2.930569811600769459, 2.453211638583554954 ) ) ;
#156843 = STYLED_ITEM ( 'NONE', ( #205294 ), #55827 ) ;
#156844 = CARTESIAN_POINT ( 'NONE',  ( 4.090592613104036879, -2.182713160620152859, -0.3248913242878055385 ) ) ;
#156845 = CARTESIAN_POINT ( 'NONE',  ( 0.4038910500440278106, -0.5768866637368921246, 2.083095904058133385 ) ) ;
#156846 = CARTESIAN_POINT ( 'NONE',  ( -4.284013352238250860, 7.941839977679187257, -0.7216878364870267237 ) ) ;
#156847 = CARTESIAN_POINT ( 'NONE',  ( 0.4922593472763935329, -1.060406550076501642, 1.591262010887870115 ) ) ;
#156848 = CARTESIAN_POINT ( 'NONE',  ( 0.5675926644314840397, 1.357872185771633156, 1.490966652548594285 ) ) ;
#156849 = CARTESIAN_POINT ( 'NONE',  ( -6.701130199342137495, -6.864242587301023768, 6.729185404178084084 ) ) ;
#156850 = LINE ( 'NONE', #7357, #11224 ) ;
#156851 = CARTESIAN_POINT ( 'NONE',  ( -0.2397550221597893050, 6.511191356812029873, 3.135202776928581514 ) ) ;
#156852 = DIRECTION ( 'NONE',  ( -0.000000000000000000, 1.000000000000000000, -0.000000000000000000 ) ) ;
#156853 = CARTESIAN_POINT ( 'NONE',  ( 0.2329894512427649333, -1.712236961970284632, 0.7538099095961707796 ) ) ;
#156854 = CARTESIAN_POINT ( 'NONE',  ( 2.466030083290056130, -1.032479112849067793, 1.731996155473938259 ) ) ;
#156856 = CARTESIAN_POINT ( 'NONE',  ( -4.339333680283728789, 7.686373885219706992, 0.7730735768287697596 ) ) ;
#156855 = CARTESIAN_POINT ( 'NONE',  ( 0.6823417656249882723, 0.4260416670080896528, -1.181850606188749264 ) ) ;
#156858 = CARTESIAN_POINT ( 'NONE',  ( 3.510471945985794928, -0.8535800194418289299, -1.925527614133336840 ) ) ;
#156857 = CARTESIAN_POINT ( 'NONE',  ( -8.341290820905609138, 10.75459192918846618, 1.599625672291269396 ) ) ;
#156859 = CARTESIAN_POINT ( 'NONE',  ( 7.904567251967224095, 9.180748867838630645, 1.199719254218462483 ) ) ;
#156861 = CARTESIAN_POINT ( 'NONE',  ( -6.855619230004478482, 11.14997286831390788, -0.7998128361456291469 ) ) ;
#156860 = CARTESIAN_POINT ( 'NONE',  ( 3.790386463472274148, 6.579812086429759788, 1.199719254218452047 ) ) ;
#156862 = CARTESIAN_POINT ( 'NONE',  ( -11.81905481421901705, 11.25735655617265074, 1.592167362352176818 ) ) ;
#156863 = CARTESIAN_POINT ( 'NONE',  ( 4.254169105220822367, 0.8597269205913078416, -1.827796444439087287 ) ) ;
#156864 = CARTESIAN_POINT ( 'NONE',  ( -1.364683531250010295, 5.238541667008086655, -0.7879004041258300672 ) ) ;
#156865 = CARTESIAN_POINT ( 'NONE',  ( 9.164948653157988900, 11.71552606681625619, -1.443375672974057666 ) ) ;
#156866 = CARTESIAN_POINT ( 'NONE',  ( 4.464260128311710041, 1.014592192358022338, 1.908665273222116543 ) ) ;
#156867 = CARTESIAN_POINT ( 'NONE',  ( 7.713663051532233972, 7.963971413067895355, -0.7998128361456341429 ) ) ;
#156868 = CARTESIAN_POINT ( 'NONE',  ( -0.6823417656250003738, -0.4697916663252491021, -1.181850606188749264 ) ) ;
#156870 = PRESENTATION_STYLE_ASSIGNMENT (( #173123 ) ) ;
#156869 = CARTESIAN_POINT ( 'NONE',  ( 4.993145711582793744, 9.047363440147082159, -0.7998128361456481317 ) ) ;
#156871 = CARTESIAN_POINT ( 'NONE',  ( 8.446366511189332016, 9.916811020218137429, -1.082531754730543083 ) ) ;
#156873 = CARTESIAN_POINT ( 'NONE',  ( -0.2721095781817652881, -7.697284395437295146, 10.99684423689256008 ) ) ;
#156872 = CARTESIAN_POINT ( 'NONE',  ( 1.627621631281210179, 0.1606834768266463820, -2.165304058017766486 ) ) ;
#156875 = CARTESIAN_POINT ( 'NONE',  ( 0.7844012160764175512, 1.623964078452419857, -0.8677550623670119423 ) ) ;
#156874 = CARTESIAN_POINT ( 'NONE',  ( -4.717874267875590277, 7.487641831621378863, 1.082531754730560403 ) ) ;
#156876 = CARTESIAN_POINT ( 'NONE',  ( -1.402160292154681736E-14, 1.696875000341421469, -1.575800808251659024 ) ) ;
#156877 = CARTESIAN_POINT ( 'NONE',  ( 3.228257827484398490, 2.138632370135685523, 0.4780590757816546854 ) ) ;
#156878 = CARTESIAN_POINT ( 'NONE',  ( -0.2897211420239401147, -7.754973434576984737, 10.97056425546335845 ) ) ;
#156879 = CARTESIAN_POINT ( 'NONE',  ( 4.118261297349164352, -1.160217402330826042, -1.942256231939092137 ) ) ;
#156880 = CARTESIAN_POINT ( 'NONE',  ( -5.994676475536691029, 10.14553965476814845, 0.7998128361456481317 ) ) ;
#156881 = CARTESIAN_POINT ( 'NONE',  ( 1.364683531249990311, 5.176041667008085767, 0.7879004041258500513 ) ) ;
#156882 = CARTESIAN_POINT ( 'NONE',  ( 6.157602363183391603, 6.969851231138187941, -0.9158007892692658913 ) ) ;
#156883 = CARTESIAN_POINT ( 'NONE',  ( 1.499999999999997113, 12.39583333333333215, -0.8660254037844378194 ) ) ;
#156884 = CARTESIAN_POINT ( 'NONE',  ( 4.082413651490639062, 7.776916670132135501, 0.000000000000000000 ) ) ;
#156885 = CARTESIAN_POINT ( 'NONE',  ( 4.516719421352251906, 1.617689212748760985, 0.7181139158070405371 ) ) ;
#156886 = CARTESIAN_POINT ( 'NONE',  ( 8.121497709785879593, 9.433834401960398353, -1.199719254218445830 ) ) ;
#156887 = CARTESIAN_POINT ( 'NONE',  ( 1.167171324275569466, -1.903845421566036311, -0.9005605707013781824 ) ) ;
#156889 = CARTESIAN_POINT ( 'NONE',  ( -0.7500000000000006661, 0.8583333333333567072, -1.299038105676652011 ) ) ;
#156888 = CARTESIAN_POINT ( 'NONE',  ( 1.364683531250000303, 11.00520833367473550, -0.7879004041258355073 ) ) ;
#156890 = CARTESIAN_POINT ( 'NONE',  ( 0.5550503504515170716, 1.639475800691666985, -1.091118944626153331 ) ) ;
#156891 = CARTESIAN_POINT ( 'NONE',  ( -3.298376509874564988, 7.070132704820777825, 0.000000000000000000 ) ) ;
#156892 = CARTESIAN_POINT ( 'NONE',  ( -9.356550365033054817, 15.43420774010369811, -7.432331899221634508 ) ) ;
#156894 = ORIENTED_EDGE ( 'NONE', *, *, #20202, .F. ) ;
#156893 = CARTESIAN_POINT ( 'NONE',  ( 5.185751641416406876, 1.743707907788614619, -0.4909320375018846883 ) ) ;
#156895 = CARTESIAN_POINT ( 'NONE',  ( 7.185458225562760148, 8.445751353653788485, -1.082531754730543083 ) ) ;
#156896 = EDGE_CURVE ( 'NONE', #162364, #205873, #115705, .T. ) ;
#156897 = CARTESIAN_POINT ( 'NONE',  ( 8.398386088661320414, 11.88553530582519357, -1.199719254218446718 ) ) ;
#156898 = CARTESIAN_POINT ( 'NONE',  ( 4.838664814796108438, 0.3202261158844340039, 1.842872994462002145 ) ) ;
#156899 = CIRCLE ( 'NONE', #153481, 0.07999999999999984901 ) ;
#156900 = CARTESIAN_POINT ( 'NONE',  ( 4.873920291170623642, -2.031351322358550870, 0.3986081187722507746 ) ) ;
#156901 = CARTESIAN_POINT ( 'NONE',  ( -0.6125000000000037081, 2.458333333333319271, -1.060881119635955327 ) ) ;
#156902 = CARTESIAN_POINT ( 'NONE',  ( -7.227905289416814760, 7.605180057173966723, -0.7216878364870338292 ) ) ;
#156903 = CARTESIAN_POINT ( 'NONE',  ( 2.923734802589327941, -0.9258770086069849636, -1.625642389100794949 ) ) ;
#156904 = CARTESIAN_POINT ( 'NONE',  ( 9.738834413317897898, 10.25639499182604730, 0.000000000000000000 ) ) ;
#156905 = CARTESIAN_POINT ( 'NONE',  ( -10.50487009249003378, 11.15010328419353947, 0.7998128361456462443 ) ) ;
#156906 = CARTESIAN_POINT ( 'NONE',  ( 6.318982112420993502, 9.529840343536603697, -1.199719254218452047 ) ) ;
#156907 = AXIS2_PLACEMENT_3D ( 'NONE', #85907, #137874, #200692 ) ;
#156908 = CARTESIAN_POINT ( 'NONE',  ( -4.911641409265215863, 4.703012472579248815, -0.3725085341543794559 ) ) ;
#156909 = CARTESIAN_POINT ( 'NONE',  ( -1.402160292154681736E-14, 0.3218750003414227456, 1.575800808251672791 ) ) ;
#156910 = CARTESIAN_POINT ( 'NONE',  ( 1.499999999999985123, 0.2958333333333566517, -0.8660254037844323793 ) ) ;
#156911 = CARTESIAN_POINT ( 'NONE',  ( 4.228923158279327410, -1.829750178516520442, -0.7082015076659909925 ) ) ;
#156912 = CARTESIAN_POINT ( 'NONE',  ( 2.302111043707856020, -1.802142186715177674, 0.9039695891032775155 ) ) ;
#156913 = DIRECTION ( 'NONE',  ( 0.000000000000000000, -1.000000000000000000, 0.000000000000000000 ) ) ;
#156914 = AXIS2_PLACEMENT_3D ( 'NONE', #201637, #133509, #53285 ) ;
#156915 = CARTESIAN_POINT ( 'NONE',  ( -11.44791656467458374, 9.799999999999982947, 3.303228920649577294 ) ) ;
#156916 = CYLINDRICAL_SURFACE ( 'NONE', #128993, 0.07999999999999998779 ) ;
#156917 = CARTESIAN_POINT ( 'NONE',  ( 1.616246341788161622, 1.260175398906153266, -1.382505567627971388 ) ) ;
#156918 = CARTESIAN_POINT ( 'NONE',  ( -1.364683531249997417, 4.759375000341424133, 1.214306433183764966E-14 ) ) ;
#156919 = CARTESIAN_POINT ( 'NONE',  ( 3.972906070543721579, -1.488974544083881746, 1.355118003239277336 ) ) ;
#156921 = CARTESIAN_POINT ( 'NONE',  ( 3.620818518838536004, 0.3129716219542731936, 2.093870907184330221 ) ) ;
#156920 = CARTESIAN_POINT ( 'NONE',  ( -7.212574532790110737, 7.517017831117667193, -0.7216878364870278340 ) ) ;
#156922 = CYLINDRICAL_SURFACE ( 'NONE', #139101, 3.475000000000000089 ) ;
#156923 = CARTESIAN_POINT ( 'NONE',  ( 5.143061708805018561, -0.2499388813127951525, -2.055141626981969338 ) ) ;
#156924 = CARTESIAN_POINT ( 'NONE',  ( 5.234329823327693809, 8.264412672927770487, 1.199719254218451159 ) ) ;
#156926 = CARTESIAN_POINT ( 'NONE',  ( 0.000000000000000000, 0.4330127018922214077, 0.000000000000000000 ) ) ;
#156925 = CARTESIAN_POINT ( 'NONE',  ( 6.650343161644081569, -1.616936162011050948, 1.324992778059615128 ) ) ;
#156928 = VERTEX_POINT ( 'NONE', #180355 ) ;
#156927 = CARTESIAN_POINT ( 'NONE',  ( 5.684540951402929920, -1.781552174421060064, -0.3977488440568625605 ) ) ;
#156929 = CARTESIAN_POINT ( 'NONE',  ( 8.402302512167096893, 10.82577223566020841, -1.599625672291268286 ) ) ;
#156930 = CARTESIAN_POINT ( 'NONE',  ( -4.934804725694231564, 5.819988937140460727, -1.082531754730544860 ) ) ;
#156931 = CARTESIAN_POINT ( 'NONE',  ( 0.000000000000000000, 19.00000000000000000, 0.000000000000000000 ) ) ;
#156932 = CARTESIAN_POINT ( 'NONE',  ( -11.25552992593869206, 3.531787801817266370, 5.933966561491729408 ) ) ;
#156933 = CARTESIAN_POINT ( 'NONE',  ( -1.364683531250000748, 12.42187500034139980, 0.000000000000000000 ) ) ;
#156934 = CARTESIAN_POINT ( 'NONE',  ( 6.621744163077868173, -0.4141588628726756149, 1.873750786029332316 ) ) ;
#156935 = CARTESIAN_POINT ( 'NONE',  ( -9.484092147959342967, 11.02352791316275216, 1.199719254218462483 ) ) ;
#156936 = CARTESIAN_POINT ( 'NONE',  ( 5.849453209292126310, 8.911780279894442103, 1.199719254218462483 ) ) ;
#156937 = CARTESIAN_POINT ( 'NONE',  ( -11.86239285000045918, 11.30000000000000249, -1.812080536912752837 ) ) ;
#156938 = CARTESIAN_POINT ( 'NONE',  ( 3.023105065722954787, 5.510411095776657220, 1.082531754730546636 ) ) ;
#156939 = CARTESIAN_POINT ( 'NONE',  ( 4.630273154266905777, 5.360739087188218122, 1.199719254218464037 ) ) ;
#156940 = ORIENTED_EDGE ( 'NONE', *, *, #142360, .F. ) ;
#156941 = CARTESIAN_POINT ( 'NONE',  ( -6.099189001301292379, 8.209082816308541197, 1.599625672291263179 ) ) ;
#156942 = CARTESIAN_POINT ( 'NONE',  ( 5.273064617572334356, 1.777004185780726386, -0.9530273427700783895 ) ) ;
#156943 = CARTESIAN_POINT ( 'NONE',  ( -3.997905685561188083, 7.705784594723285252, -0.04799061902135907248 ) ) ;
#156944 = DIRECTION ( 'NONE',  ( -0.000000000000000000, -1.000000000000000000, -0.000000000000000000 ) ) ;
#156945 = CARTESIAN_POINT ( 'NONE',  ( -5.341549334104202629, 7.254893527920112994, 1.443375672974064550 ) ) ;
#156946 = CARTESIAN_POINT ( 'NONE',  ( 9.897088948295943212, 11.60932053017587506, 1.082531754730548412 ) ) ;
#156947 = CARTESIAN_POINT ( 'NONE',  ( 2.782036810173736718, -1.130008284276774022, -1.612816519099938173 ) ) ;
#156948 = CARTESIAN_POINT ( 'NONE',  ( 3.427361390312729572, -1.528753972193249933, -1.314983687342549556 ) ) ;
#156949 = CARTESIAN_POINT ( 'NONE',  ( -5.856232286098998152, 8.919689202835742847, 1.199719254218452047 ) ) ;
#156950 = CARTESIAN_POINT ( 'NONE',  ( 6.727182134110219813, 2.036943547479725058, 2.394510323907019345 ) ) ;
#156951 = CARTESIAN_POINT ( 'NONE',  ( 3.961010909407122860, 0.2689195440248594027, -2.174814543647784593 ) ) ;
#156952 =( NAMED_UNIT ( * ) SI_UNIT ( $, .STERADIAN. ) SOLID_ANGLE_UNIT ( ) );
#156953 = CARTESIAN_POINT ( 'NONE',  ( 3.047785661706010174, 0.6947733606382737737, -1.796906316042534923 ) ) ;
#156954 = CARTESIAN_POINT ( 'NONE',  ( -9.820183334999905256, 10.35130206712171130, 1.040834085586084257E-14 ) ) ;
#156955 = SURFACE_STYLE_FILL_AREA ( #141802 ) ;
#156956 = CARTESIAN_POINT ( 'NONE',  ( 4.593150236022219428E-15, -8.011313137147251240, -11.00000000000000178 ) ) ;
#156957 = ADVANCED_FACE ( 'NONE', ( #98059 ), #197654, .F. ) ;
#156958 = CARTESIAN_POINT ( 'NONE',  ( 10.95308175811721085, 11.29999999999999893, -1.800000000000001155 ) ) ;
#156959 = CARTESIAN_POINT ( 'NONE',  ( 1.364683531249997417, 12.73437500034139980, 2.602085213965210642E-15 ) ) ;
#156960 = CARTESIAN_POINT ( 'NONE',  ( 4.449046963578762615, 8.342305224150557308, -0.7998128361456231517 ) ) ;
#156961 =( BOUNDED_CURVE ( )  B_SPLINE_CURVE ( 2, ( #177969, #29583, #95671, #13317, #129305, #195282, #46914 ),
 .UNSPECIFIED., .F., .T. ) 
 B_SPLINE_CURVE_WITH_KNOTS ( ( 3, 2, 2, 3 ),
 ( 0.3605655240965703334, 0.3630952380952380820, 0.3690476190476190688, 0.3715773330462868174 ),
 .UNSPECIFIED. ) 
 CURVE ( )  GEOMETRIC_REPRESENTATION_ITEM ( )  RATIONAL_B_SPLINE_CURVE ( ( 0.9345202395942613371, 0.9430618748659225226, 1.000000000000000000, 0.8660254037844387076, 1.000000000000000000, 0.9430618748659225226, 0.9345202395942613371 ) ) 
 REPRESENTATION_ITEM ( '' )  );
#156962 = CARTESIAN_POINT ( 'NONE',  ( -6.661184053808019812, -7.645781813054106202, 6.773376336901249850 ) ) ;
#156963 = CARTESIAN_POINT ( 'NONE',  ( 6.387299765813869712, 6.624473612970537495, 0.000000000000000000 ) ) ;
#156964 = ORIENTED_EDGE ( 'NONE', *, *, #176622, .T. ) ;
#156966 = CARTESIAN_POINT ( 'NONE',  ( 2.385404357411140541, 0.09669159202466531822, -2.010876702762071311 ) ) ;
#156965 = CARTESIAN_POINT ( 'NONE',  ( 5.759284750224211713, 1.812880138157666465, -0.3211251414683007899 ) ) ;
#156967 = CARTESIAN_POINT ( 'NONE',  ( 5.396019846235262207, 0.1618137187183350256, 2.292739235009821908 ) ) ;
#156969 = CARTESIAN_POINT ( 'NONE',  ( 2.781907013001069906, -1.067198605185412763, -1.524341717138616215 ) ) ;
#156968 = CARTESIAN_POINT ( 'NONE',  ( 0.000000000000000000, 5.999999999999998224, 0.000000000000000000 ) ) ;
#156971 = CARTESIAN_POINT ( 'NONE',  ( -3.285556943750000514, -0.4885416661887091450, -1.896917185911906500 ) ) ;
#156970 = APPLICATION_CONTEXT ( 'automotive_design' ) ;
#156972 = CARTESIAN_POINT ( 'NONE',  ( -9.569423160901790126, -7.256398209936431698, 1.138412281109779656E-15 ) ) ;
#156973 = DIRECTION ( 'NONE',  ( 0.000000000000000000, -1.000000000000000000, 0.000000000000000000 ) ) ;
#156974 = CARTESIAN_POINT ( 'NONE',  ( -8.342344591110322227, 8.627156865917170236, -0.7998128361456291469 ) ) ;
#156975 = CARTESIAN_POINT ( 'NONE',  ( -4.448483799059637533, 7.243629294661272588, 1.082531754730549967 ) ) ;
#156976 = CARTESIAN_POINT ( 'NONE',  ( 6.497611715980437630, -2.090283427287362272, 0.05178676472679385329 ) ) ;
#156977 = CARTESIAN_POINT ( 'NONE',  ( 5.829642864196162400, 7.824335979694092558, 1.443375672974062551 ) ) ;
#156978 = ORIENTED_EDGE ( 'NONE', *, *, #132737, .F. ) ;
#156979 = CARTESIAN_POINT ( 'NONE',  ( -1.485661138092309042, 7.335467742082953713, 4.255596723431145811 ) ) ;
#156981 = CARTESIAN_POINT ( 'NONE',  ( 3.018661757337009810, 6.673522483535157868, 0.000000000000000000 ) ) ;
#156980 = FACE_OUTER_BOUND ( 'NONE', #55917, .T. ) ;
#156982 = CARTESIAN_POINT ( 'NONE',  ( 5.830603237517035353, 1.664100180626144398, 0.4535787370015566533 ) ) ;
#156983 = CARTESIAN_POINT ( 'NONE',  ( -4.574986769607567894, 7.424902766929059261, 1.199719254218464037 ) ) ;
#156984 = AXIS2_PLACEMENT_3D ( 'NONE', #150694, #152808, #52114 ) ;
#156985 = CARTESIAN_POINT ( 'NONE',  ( 1.705275228087951955, 1.618143048327233435, 0.6241232001420042863 ) ) ;
#156986 = CARTESIAN_POINT ( 'NONE',  ( -2.226451178929228281, 14.55178036729105884, 11.75480792874617819 ) ) ;
#156987 = DIRECTION ( 'NONE',  ( -1.000000000000000000, -3.451266460341925773E-31, -8.638326563840809144E-31 ) ) ;
#156988 = CARTESIAN_POINT ( 'NONE',  ( -5.832844346354424836, 6.047612191973543716, -0.4696115756501819671 ) ) ;
#156990 = AXIS2_PLACEMENT_3D ( 'NONE', #146746, #212765, #64400 ) ;
#156989 = CARTESIAN_POINT ( 'NONE',  ( 6.192256317468841864, 1.077302059837774273, -1.884901478735945046 ) ) ;
#156991 = CARTESIAN_POINT ( 'NONE',  ( 4.758326833623739205, 0.7015320795021735556, 1.685726030614169924 ) ) ;
#156992 = CARTESIAN_POINT ( 'NONE',  ( 1.990992145637654698, 0.1870960246039363450, 1.952785824368876932 ) ) ;
#156993 = CARTESIAN_POINT ( 'NONE',  ( -2.113655003624821838, 5.617681270870908072, 1.040834085586084257E-14 ) ) ;
#156994 = CARTESIAN_POINT ( 'NONE',  ( -10.10098813738111545, 11.74323990082152491, -1.199719254218441611 ) ) ;
#156995 = CARTESIAN_POINT ( 'NONE',  ( 6.414979237560321401, 10.63589287712906462, 1.040834085586084257E-14 ) ) ;
#156996 = CARTESIAN_POINT ( 'NONE',  ( 3.194099758881031814, 1.346771490053525033, 1.637864368873870990 ) ) ;
#156997 = CARTESIAN_POINT ( 'NONE',  ( -2.155383234892699562, 5.458438174109348395, 1.040834085586084257E-14 ) ) ;
#156998 = DIRECTION ( 'NONE',  ( -0.000000000000000000, -0.000000000000000000, 1.000000000000000000 ) ) ;
#156999 = CARTESIAN_POINT ( 'NONE',  ( -4.791002085003811750, 6.784460936665063890, -1.245152473204954591 ) ) ;
#157000 = CARTESIAN_POINT ( 'NONE',  ( 1.463825199929311260, -0.5068179562870354093, 2.007114080642191656 ) ) ;
#157002 = CARTESIAN_POINT ( 'NONE',  ( -1.402160292154681736E-14, 14.84375000068279427, 1.732050807568881190 ) ) ;
#157001 = CARTESIAN_POINT ( 'NONE',  ( -9.604686356149274573, 3.530917816115240804, 7.193747284969077782 ) ) ;
#157004 = VERTEX_POINT ( 'NONE', #144700 ) ;
#157003 = CARTESIAN_POINT ( 'NONE',  ( 3.633611385093922674, -0.1624337102359394436, 2.215399726503309630 ) ) ;
#157005 = CARTESIAN_POINT ( 'NONE',  ( 1.337049673779285852, 0.6609975811289883207, -2.201632501652720286 ) ) ;
#157007 = CARTESIAN_POINT ( 'NONE',  ( 6.262562444065095768, -0.7369429887811511648, -1.926613908347002413 ) ) ;
#157006 = CARTESIAN_POINT ( 'NONE',  ( 7.782016984564043227, 12.02284421539267356, 0.7216878364870438212 ) ) ;
#157009 = CARTESIAN_POINT ( 'NONE',  ( 0.000000000000000000, -3.346874999522042149, -3.793834371823813001 ) ) ;
#157008 = CARTESIAN_POINT ( 'NONE',  ( 3.932747076415766596, 6.745899468197171345, 1.199719254218451159 ) ) ;
#157010 = EDGE_CURVE ( 'NONE', #43590, #182367, #118605, .T. ) ;
#157011 = DIRECTION ( 'NONE',  ( 0.000000000000000000, 0.000000000000000000, -1.000000000000000000 ) ) ;
#157012 = CARTESIAN_POINT ( 'NONE',  ( -11.06296324151031918, 11.25662273973621730, 0.9090245397293565954 ) ) ;
#157013 = DIRECTION ( 'NONE',  ( 0.000000000000000000, 0.000000000000000000, -1.000000000000000000 ) ) ;
#157014 = ADVANCED_FACE ( 'NONE', ( #87108 ), #180362, .T. ) ;
#157015 = CARTESIAN_POINT ( 'NONE',  ( -0.1102773484824119132, 0.6802821481026833927, -2.283667859588431881 ) ) ;
#157016 = CARTESIAN_POINT ( 'NONE',  ( 2.678358392608829686, -1.649718294651691730, -0.5031959223205755283 ) ) ;
#157017 = CARTESIAN_POINT ( 'NONE',  ( 2.325407997918966796, -1.497503195670712328, -1.350734289967000512 ) ) ;
#157018 = CARTESIAN_POINT ( 'NONE',  ( 3.954570948191834745, 0.8096313216635497856, 2.112761250790657908 ) ) ;
#157019 = CARTESIAN_POINT ( 'NONE',  ( 5.830723289215218763, 2.029276893092274658, 0.5632808350878695247 ) ) ;
#157020 = CARTESIAN_POINT ( 'NONE',  ( -6.699137298928187434, 8.909022496873262753, 1.443375672974064550 ) ) ;
#157021 = CARTESIAN_POINT ( 'NONE',  ( 4.042088942692352305, 1.761052656288846663, 0.1752445044498444349 ) ) ;
#157023 = CARTESIAN_POINT ( 'NONE',  ( 6.181209693220585777, 1.577568176048673720, 1.663411239723869173 ) ) ;
#157022 = CARTESIAN_POINT ( 'NONE',  ( 6.502017186205484300, 9.743381262951846367, -1.199719254218452047 ) ) ;
#157024 = B_SPLINE_CURVE_WITH_KNOTS ( 'NONE', 3,
 ( #119142, #49816, #34624, #166771, #18367, #84444 ),
 .UNSPECIFIED., .F., .F.,
 ( 4, 2, 4 ),
 ( 0.001889712630306643673, 0.002203932548491402497, 0.002518152466676161320 ),
 .UNSPECIFIED. ) ;
#157025 = CARTESIAN_POINT ( 'NONE',  ( 5.244037021109955177, 0.5378974813256987009, 1.760811445753920346 ) ) ;
#157026 = CARTESIAN_POINT ( 'NONE',  ( -4.460796234096120472, 5.163016013655583158, 1.199719254218462483 ) ) ;
#157027 = CARTESIAN_POINT ( 'NONE',  ( 1.499999999999989120, 3.254166666666690855, 0.8660254037844524744 ) ) ;
#157028 = CARTESIAN_POINT ( 'NONE',  ( 5.929655999079198381, 1.083026401007038952, -1.905042663481799403 ) ) ;
#157029 = CARTESIAN_POINT ( 'NONE',  ( -6.739251124622717803, 15.51951738225662325, 9.939126542081607951 ) ) ;
#157030 = CARTESIAN_POINT ( 'NONE',  ( 5.512195382060368409, 2.068158883198469855, -0.09793725168850964113 ) ) ;
#157031 = CARTESIAN_POINT ( 'NONE',  ( -11.92619526913699524, 10.07219975838509818, -1.328859060402685976 ) ) ;
#157032 = CARTESIAN_POINT ( 'NONE',  ( -1.364683531249997417, 5.009375000341425022, 1.214306433183764966E-14 ) ) ;
#157033 = CARTESIAN_POINT ( 'NONE',  ( 3.914609504329464418, 1.361597497701543480, -1.363134563274936761 ) ) ;
#157034 = CARTESIAN_POINT ( 'NONE',  ( -1.364683531250010295, 10.88020833367473372, 0.7879004041258445001 ) ) ;
#157035 = CARTESIAN_POINT ( 'NONE',  ( -3.687454593236990430, 4.364747115940301292, 1.082531754730560403 ) ) ;
#157036 = CARTESIAN_POINT ( 'NONE',  ( -0.08724509969064601911, -2.221098688967707790, -0.04574986941241648841 ) ) ;
#157038 = ORIENTED_EDGE ( 'NONE', *, *, #202085, .T. ) ;
#157037 = PLANE ( 'NONE',  #140590 ) ;
#157040 = CARTESIAN_POINT ( 'NONE',  ( 4.850610703097786747, 8.175460293138137047, -1.048226046837946512 ) ) ;
#157039 = CARTESIAN_POINT ( 'NONE',  ( -4.841670253855968831, 4.821239182352949904, 0.000000000000000000 ) ) ;
#157041 = CARTESIAN_POINT ( 'NONE',  ( 3.083589872104280705, 5.684939719841914929, 1.199719254218450271 ) ) ;
#157042 = DIRECTION ( 'NONE',  ( 0.000000000000000000, 0.000000000000000000, 1.000000000000000000 ) ) ;
#157043 = CARTESIAN_POINT ( 'NONE',  ( 3.894326384698054255, 7.335661066667313435, -0.8064731704051804062 ) ) ;
#157044 = CARTESIAN_POINT ( 'NONE',  ( 11.92559808404167576, 7.608499137140611879, 0.8913980220144042121 ) ) ;
#157045 = CARTESIAN_POINT ( 'NONE',  ( 9.856414487010587422, 11.56186699200962487, 1.082531754730548412 ) ) ;
#157046 = CARTESIAN_POINT ( 'NONE',  ( 1.627322669196319849, 0.1476378700930695564, -1.956383933670035713 ) ) ;
#157047 = CARTESIAN_POINT ( 'NONE',  ( 0.6823417656249899377, 0.6552083336747518416, 1.181850606188755259 ) ) ;
#157048 = DIRECTION ( 'NONE',  ( 0.000000000000000000, 1.000000000000000000, 0.000000000000000000 ) ) ;
#157049 = CIRCLE ( 'NONE', #181304, 1.359291649810832503 ) ;
#157050 = CARTESIAN_POINT ( 'NONE',  ( 5.424254290899477304, 0.9654600744411747648, 1.707767180430696641 ) ) ;
#157051 = CARTESIAN_POINT ( 'NONE',  ( -7.483210719738908168, 10.81783070874899799, 1.199719254218453823 ) ) ;
#157052 = CARTESIAN_POINT ( 'NONE',  ( -5.924549939047510705, 6.974691686052601369, 1.082531754730549967 ) ) ;
#157053 = CARTESIAN_POINT ( 'NONE',  ( 0.4798239446817476606, 2.109833986122396254, -0.8175194613929820386 ) ) ;
#157055 = ORIENTED_EDGE ( 'NONE', *, *, #172864, .F. ) ;
#157054 = CARTESIAN_POINT ( 'NONE',  ( -0.2106725631049838343, 0.7236243445625335502, -2.087119268998542942 ) ) ;
#157056 = CARTESIAN_POINT ( 'NONE',  ( -1.500000000000015099, -0.8395833326505166561, -0.8660254037844383745 ) ) ;
#157057 = CARTESIAN_POINT ( 'NONE',  ( 0.5966796567213605851, 1.558732183387041781, -1.033768272189788950 ) ) ;
#157058 = CARTESIAN_POINT ( 'NONE',  ( 0.4395775532227184090, -1.463650450414313520, -0.9296597220836488873 ) ) ;
#157059 = AXIS2_PLACEMENT_3D ( 'NONE', #157686, #90557, #110054 ) ;
#157061 = CARTESIAN_POINT ( 'NONE',  ( 3.333693798916517625, 0.9835563995168915552, -1.958507884819527867 ) ) ;
#157060 = CARTESIAN_POINT ( 'NONE',  ( 1.360316468749983576, 1.515625000341386253, -4.163336342344337027E-14 ) ) ;
#157062 = CARTESIAN_POINT ( 'NONE',  ( 5.016800025512162975, 1.595470874386342608, -1.667385368739245255 ) ) ;
#157063 = CARTESIAN_POINT ( 'NONE',  ( 0.5321925127804688627, 1.059884587108523402, -1.767317575122410167 ) ) ;
#157064 = CARTESIAN_POINT ( 'NONE',  ( 2.220557385006210804, 0.0001418518128949025625, 1.942124712491780869 ) ) ;
#157065 = CARTESIAN_POINT ( 'NONE',  ( -6.033015167956810920, 7.101234453113482559, -1.082531754730543083 ) ) ;
#157066 = FACE_OUTER_BOUND ( 'NONE', #70527, .T. ) ;
#157067 = CARTESIAN_POINT ( 'NONE',  ( 5.097945154717048233, 1.425953928781589886, 1.569717048080176314 ) ) ;
#157068 = CARTESIAN_POINT ( 'NONE',  ( -1.975475456537005874E-15, 2.812500000000000888, 1.224999999999953904 ) ) ;
#157069 = CARTESIAN_POINT ( 'NONE',  ( 3.973279856364997809, -1.994869694282218386, -0.2930714778977619450 ) ) ;
#157070 = CARTESIAN_POINT ( 'NONE',  ( -4.948362878863562742, 5.835806782504650236, 1.082531754730558626 ) ) ;
#157071 = CARTESIAN_POINT ( 'NONE',  ( -7.014364370223741929, 9.276787413384745662, -1.599625672291271394 ) ) ;
#157072 = CARTESIAN_POINT ( 'NONE',  ( 10.72180055030867329, 11.40318881831530540, 0.7998128361456341429 ) ) ;
#157073 = CARTESIAN_POINT ( 'NONE',  ( 1.101864800459760207, -1.825872481749410525, -0.002338443969775172437 ) ) ;
#157074 = CARTESIAN_POINT ( 'NONE',  ( -5.152980901645737077, 8.169505597632108262, -1.199719254218453823 ) ) ;
#157075 = CARTESIAN_POINT ( 'NONE',  ( 1.907519672996875082, 3.236073672982398008, -0.4612874649729831744 ) ) ;
#157076 = CARTESIAN_POINT ( 'NONE',  ( -10.55163518180063242, 5.124035624933899413, 7.011265714045999076 ) ) ;
#157077 = ORIENTED_EDGE ( 'NONE', *, *, #46969, .F. ) ;
#157078 = CARTESIAN_POINT ( 'NONE',  ( 5.383688703920392449, 1.382483038487541283, 1.528581890270568122 ) ) ;
#157079 = CARTESIAN_POINT ( 'NONE',  ( -5.248414861821563804, 9.137251415518218067, 0.7216878364870267237 ) ) ;
#157080 = CARTESIAN_POINT ( 'NONE',  ( -1.500000000000015099, 11.76041666734946922, -0.8660254037844309360 ) ) ;
#157081 = CARTESIAN_POINT ( 'NONE',  ( -5.101945877444165944, 4.846691699973280976, 0.000000000000000000 ) ) ;
#157082 = CARTESIAN_POINT ( 'NONE',  ( -6.138157471807708987, 5.995865026538652387, 1.148737437293850421E-12 ) ) ;
#157083 = CARTESIAN_POINT ( 'NONE',  ( 4.934242777533356161, -1.082215927170935954, -1.705062858592779174 ) ) ;
#157084 = CARTESIAN_POINT ( 'NONE',  ( 5.408899451717416262, -0.5379699361975317506, -2.155043070319954790 ) ) ;
#157086 = CARTESIAN_POINT ( 'NONE',  ( 9.002250809793993724, 11.52571191622492464, -1.443375672974057666 ) ) ;
#157085 = CARTESIAN_POINT ( 'NONE',  ( -6.563028877466991595, 9.814561569423593923, 1.199719254218452935 ) ) ;
#157087 = CARTESIAN_POINT ( 'NONE',  ( 5.632522751473472589, 8.658694745772667289, -1.199719254218440723 ) ) ;
#157088 = CARTESIAN_POINT ( 'NONE',  ( 3.696211625926352440, -2.058462806815289259, -0.1027275840673105151 ) ) ;
#157089 = CARTESIAN_POINT ( 'NONE',  ( 3.938125092175647879, -1.678004675797317713, -1.117833462672225497 ) ) ;
#157090 = ORIENTED_EDGE ( 'NONE', *, *, #24698, .F. ) ;
#157091 = DIRECTION ( 'NONE',  ( -0.6507913734559658270, -0.7592566023652989049, 0.000000000000000000 ) ) ;
#157092 = CARTESIAN_POINT ( 'NONE',  ( 4.355193658487811703, 6.104145239700998538, -1.599625672291255185 ) ) ;
#157094 = ORIENTED_EDGE ( 'NONE', *, *, #187841, .F. ) ;
#157093 = CARTESIAN_POINT ( 'NONE',  ( -7.442499979258930587, 7.647614495415686164, -0.7998128361456362523 ) ) ;
#157095 = CARTESIAN_POINT ( 'NONE',  ( 5.583942420111207561, 7.395222456726187943, -1.242479836444350783 ) ) ;
#157096 = CARTESIAN_POINT ( 'NONE',  ( 3.479842141819572632, 1.821463063354014533, 0.8645922719773959653 ) ) ;
#157097 = CARTESIAN_POINT ( 'NONE',  ( 2.396224210035051261, 1.478860665732561586, -1.096489538662905217 ) ) ;
#157098 = CARTESIAN_POINT ( 'NONE',  ( 1.208152727780729130, -0.5562822606778123902, 2.239534654701015981 ) ) ;
#157099 = CARTESIAN_POINT ( 'NONE',  ( 5.996449078994045223, 10.21788403546024782, 0.7998128361456331437 ) ) ;
#157100 = CARTESIAN_POINT ( 'NONE',  ( 3.585389192675687564, 1.955840111083558597, -0.9206723451176119788 ) ) ;
#157101 = CARTESIAN_POINT ( 'NONE',  ( -6.521635583373313061, 7.567328587812373719, -1.199719254218446718 ) ) ;
#157102 = CARTESIAN_POINT ( 'NONE',  ( 3.673487740190139572, -0.9280425899400122081, -2.102842487114229275 ) ) ;
#157103 = ORIENTED_EDGE ( 'NONE', *, *, #191456, .F. ) ;
#157104 = CARTESIAN_POINT ( 'NONE',  ( -0.02244404828157658613, -0.004869073801674199918, -2.189079685368473527 ) ) ;
#157105 = CARTESIAN_POINT ( 'NONE',  ( 1.885419139999934934, 1.287927767047767125, 1.356919574424742203 ) ) ;
#157106 = ORIENTED_EDGE ( 'NONE', *, *, #39019, .F. ) ;
#157107 = CARTESIAN_POINT ( 'NONE',  ( 5.717641559312711230, -1.923570962979544330, 0.4312651734501466994 ) ) ;
#157108 = VECTOR ( 'NONE', #677, 1000.000000000000000 ) ;
#157110 = CARTESIAN_POINT ( 'NONE',  ( 9.869972640624258275, 10.61731562359089587, 0.000000000000000000 ) ) ;
#157109 = CARTESIAN_POINT ( 'NONE',  ( -1.364683531250010295, 4.530208333674754506, 0.7879004041258379498 ) ) ;
#157112 = CARTESIAN_POINT ( 'NONE',  ( 0.8388348947251201837, 2.174866457552121268, 0.3736606161612308630 ) ) ;
#157111 = CARTESIAN_POINT ( 'NONE',  ( -6.250472511100020334, 7.250971670160158311, 1.199719254218450271 ) ) ;
#157113 = CARTESIAN_POINT ( 'NONE',  ( 1.110223024625156540E-16, 1.551257596039481879, -2.000000000000006217 ) ) ;
#157114 = CARTESIAN_POINT ( 'NONE',  ( 6.017121246366603060, 5.914396297049491658, 1.040834085586084257E-14 ) ) ;
#157115 = CARTESIAN_POINT ( 'NONE',  ( -5.708146366553361162, 6.618257834855742594, -1.199719254218446718 ) ) ;
#157116 = CARTESIAN_POINT ( 'NONE',  ( -7.893838479094924310, -5.325441678136489720, 7.661067326845521386 ) ) ;
#157117 = CARTESIAN_POINT ( 'NONE',  ( 6.596557512146871360, -0.5253642993188823995, -1.900122941938019450 ) ) ;
#157118 = CARTESIAN_POINT ( 'NONE',  ( 5.391387774523593635, 2.037479383949382772, -1.083606018200606869 ) ) ;
#157119 = CARTESIAN_POINT ( 'NONE',  ( 6.303157624210896870, -1.571610030290017557, 0.9964359807085266807 ) ) ;
#157120 = CARTESIAN_POINT ( 'NONE',  ( 3.168856051829985532, 1.497182195067780386, -1.418930203433153903 ) ) ;
#157121 = CARTESIAN_POINT ( 'NONE',  ( 5.938108093105483931, 8.911247961056314892, -1.082531754730537088 ) ) ;
#157122 = CARTESIAN_POINT ( 'NONE',  ( 5.806634928402749196, 9.996434193103704402, -0.7998128361456481317 ) ) ;
#157123 = CARTESIAN_POINT ( 'NONE',  ( 7.090551149822739596, 8.335026431957096804, 1.082531754730558626 ) ) ;
#157124 = CARTESIAN_POINT ( 'NONE',  ( -1.364683531249997417, 2.821875000341422801, 1.214306433183764966E-14 ) ) ;
#157125 = CARTESIAN_POINT ( 'NONE',  ( -9.719589822879429519, 3.553060291783284974, -6.966707445246908215 ) ) ;
#157126 = CARTESIAN_POINT ( 'NONE',  ( 4.311129659021211147, 7.973475668925984472, 1.040834085586084257E-14 ) ) ;
#157127 = CARTESIAN_POINT ( 'NONE',  ( 5.072805357664615045, 1.500764584350265718, -1.569201701505947844 ) ) ;
#157128 = CARTESIAN_POINT ( 'NONE',  ( -11.41381675112453387, 10.19999999999998153, 3.704697986577180746 ) ) ;
#157130 = CARTESIAN_POINT ( 'NONE',  ( 4.599059095968327071, -0.4863373063577690059, 1.775805238918099382 ) ) ;
#157129 = CARTESIAN_POINT ( 'NONE',  ( -4.134873662487946966, 3.926366815765101936, 1.214306433183764966E-14 ) ) ;
#157132 = CARTESIAN_POINT ( 'NONE',  ( 6.720655732516610747, 3.700489942686377098, 2.440724243369211788 ) ) ;
#157131 = CARTESIAN_POINT ( 'NONE',  ( -10.07455280567990563, 1.264806443676224301, -6.263461699855405129 ) ) ;
#157133 = CARTESIAN_POINT ( 'NONE',  ( -6.773846765317318663, 0.000000000000000000, 6.773846765317342644 ) ) ;
#157134 = CARTESIAN_POINT ( 'NONE',  ( 0.2847049989426675976, 3.404688149418213960, 1.981472963502264317 ) ) ;
#157135 = CARTESIAN_POINT ( 'NONE',  ( 0.8610526709191126393, -1.638059776709074322, 1.560773681941391100 ) ) ;
#157136 = CARTESIAN_POINT ( 'NONE',  ( -3.990270464981529486, 7.829052896380438220, 0.2716399205876223744 ) ) ;
#157137 = CARTESIAN_POINT ( 'NONE',  ( -2.974142338115852269, 6.685868392857900133, 0.1038623869373533903 ) ) ;
#157138 = CARTESIAN_POINT ( 'NONE',  ( 6.400241882075590638, 6.902609158730609096, 0.7749192096189911894 ) ) ;
#157139 = CARTESIAN_POINT ( 'NONE',  ( -4.109529958273628658, 7.808552361378938045, 0.7216878364870338292 ) ) ;
#157140 = CARTESIAN_POINT ( 'NONE',  ( 0.3461628310420067356, 0.9829124436787043395, -1.640176041098049264 ) ) ;
#157141 = CARTESIAN_POINT ( 'NONE',  ( 1.973191454406374890, 1.694654629526294087, -0.5103889506637182549 ) ) ;
#157142 = CARTESIAN_POINT ( 'NONE',  ( 5.057293878089731187, -1.725371964895198840, 1.036928162195766889 ) ) ;
#157143 = CARTESIAN_POINT ( 'NONE',  ( 4.659198344590585350, 8.587481835331020719, 0.7998128361456462443 ) ) ;
#157144 = CARTESIAN_POINT ( 'NONE',  ( 4.137795317726181032, -1.450671198928995098, -1.526879382678330010 ) ) ;
#157146 = CARTESIAN_POINT ( 'NONE',  ( 3.075699878008768096, -0.7735687425090407299, 1.752645402151173926 ) ) ;
#157145 = CARTESIAN_POINT ( 'NONE',  ( -4.256897044566581911, 4.068727428190179296, 1.214306433183764966E-14 ) ) ;
#157147 = CARTESIAN_POINT ( 'NONE',  ( 0.008366613517340512618, 2.629643693813621397, -12.00001160347414775 ) ) ;
#157148 = CARTESIAN_POINT ( 'NONE',  ( 3.771889708208826075, -1.940809680921409486, 0.3342159591338197400 ) ) ;
#157150 = EDGE_CURVE ( 'NONE', #202900, #41604, #50979, .T. ) ;
#157149 = CARTESIAN_POINT ( 'NONE',  ( 0.05319811239242258627, 0.3688592364489845510, 2.088132107045739705 ) ) ;
#157151 = CARTESIAN_POINT ( 'NONE',  ( 2.869827659178546764, 0.9992216309704025079, 1.581230272166146644 ) ) ;
#157153 = ORIENTED_EDGE ( 'NONE', *, *, #33674, .F. ) ;
#157152 = CARTESIAN_POINT ( 'NONE',  ( 4.863727610707407223, 1.705404662657764137, -0.2575704655415639310 ) ) ;
#157155 = CARTESIAN_POINT ( 'NONE',  ( 5.680503174445848735, 5.729601246382692636, 1.040834085586084257E-14 ) ) ;
#157154 = CARTESIAN_POINT ( 'NONE',  ( 2.877765823869771644, 2.095344539500657799, -0.6929138170133213315 ) ) ;
#157156 = CARTESIAN_POINT ( 'NONE',  ( -1.364683531249997417, 3.321875000341423245, 1.214306433183764966E-14 ) ) ;
#157157 = CARTESIAN_POINT ( 'NONE',  ( 6.848121815800094936, -0.8396676627679277027, 1.771385694100804375 ) ) ;
#157159 = EDGE_CURVE ( 'NONE', #116525, #138593, #169901, .T. ) ;
#157158 = CARTESIAN_POINT ( 'NONE',  ( 7.751511138711133064, 10.06651563329490529, -1.599625672291262513 ) ) ;
#157160 = CARTESIAN_POINT ( 'NONE',  ( -9.829825065107822724, 11.42688298316931572, 1.199719254218462483 ) ) ;
#157161 = CARTESIAN_POINT ( 'NONE',  ( -10.84253909858433218, 4.919570308430900596, -5.035411995924089723 ) ) ;
#157162 = CARTESIAN_POINT ( 'NONE',  ( 0.1747926744264660381, 0.006858446013176254172, -1.855468577918440776 ) ) ;
#157163 = CARTESIAN_POINT ( 'NONE',  ( 0.000000000000000000, 19.00000000000000000, 0.000000000000000000 ) ) ;
#157164 = ORIENTED_EDGE ( 'NONE', *, *, #34519, .F. ) ;
#157165 = CARTESIAN_POINT ( 'NONE',  ( 1.715371797147913435, -1.774658612622433296, -1.066089629202723765 ) ) ;
#157166 = CARTESIAN_POINT ( 'NONE',  ( -1.201851678989727383E-14, 2.837500000000024780, -1.732050807568863648 ) ) ;
#157167 = CARTESIAN_POINT ( 'NONE',  ( 5.986088515633498197, 6.942523675449257858, -1.199719254218446718 ) ) ;
#157168 = CARTESIAN_POINT ( 'NONE',  ( 3.444653546323793947, 6.176457016423196222, 1.199719254218451159 ) ) ;
#157169 = CARTESIAN_POINT ( 'NONE',  ( 6.621762855810419346, -0.4656160214656123175, 2.076383538966434017 ) ) ;
#157170 = CARTESIAN_POINT ( 'NONE',  ( -1.201851678989727383E-14, 4.446875000341417916, -1.575800808251660134 ) ) ;
#157171 = CARTESIAN_POINT ( 'NONE',  ( 8.432808358020004391, 12.78210081775797669, 0.7216878364870438212 ) ) ;
#157172 = CARTESIAN_POINT ( 'NONE',  ( 5.325545996062735377, -1.462220743079494012, 1.388274341532859335 ) ) ;
#157173 = CARTESIAN_POINT ( 'NONE',  ( 4.751152363292252545, 0.1813030634821456710, -1.907091066879146757 ) ) ;
#157174 = CARTESIAN_POINT ( 'NONE',  ( -1.500000000000039524, 7.193113254731344774, -10.88798745763943110 ) ) ;
#157175 = CARTESIAN_POINT ( 'NONE',  ( 2.648187065138879692, 0.7411268365287644322, 2.062558662443473523 ) ) ;
#157176 = CARTESIAN_POINT ( 'NONE',  ( -1.499999999999997780, 1.931250000682817269, 0.000000000000000000 ) ) ;
#157177 = CARTESIAN_POINT ( 'NONE',  ( 2.970861089138315592, -1.445268511421276214, 1.252435071843561731 ) ) ;
#157178 = CARTESIAN_POINT ( 'NONE',  ( -4.381256195510448315, 8.263215994737505454, 1.040834085586084257E-14 ) ) ;
#157179 = CARTESIAN_POINT ( 'NONE',  ( 0.2457205463545810431, 1.994068899247893434, -0.2986513045247774500 ) ) ;
#157180 = CARTESIAN_POINT ( 'NONE',  ( -1.364683531250014514, 9.901041667008064096, -0.7879004041258335089 ) ) ;
#157182 = CARTESIAN_POINT ( 'NONE',  ( -5.444481204339554736, 8.509589284108232121, 1.199719254218454489 ) ) ;
#157181 = CARTESIAN_POINT ( 'NONE',  ( 3.579701903670178709, -1.028438467219190411, 1.820211688285853446 ) ) ;
#157184 = ORIENTED_EDGE ( 'NONE', *, *, #194076, .F. ) ;
#157183 = CARTESIAN_POINT ( 'NONE',  ( 2.625662686473359653, -0.9909224867145174365, -1.411489731159983219 ) ) ;
#157185 = CARTESIAN_POINT ( 'NONE',  ( -1.324887192667531632, -1.296481010641094000, 1.500000000000001776 ) ) ;
#157186 = CARTESIAN_POINT ( 'NONE',  ( 5.636439174979242850, 7.598931675607687453, -1.599625672291262513 ) ) ;
#157187 = EDGE_CURVE ( 'NONE', #132416, #14896, #159555, .T. ) ;
#157188 = CARTESIAN_POINT ( 'NONE',  ( 10.50000000000000533, 13.50841679891518687, -3.600000000000000533 ) ) ;
#157189 = CARTESIAN_POINT ( 'NONE',  ( 5.602074566136501232, 5.729665287594564838, 0.6253354971682704155 ) ) ;
#157190 = CARTESIAN_POINT ( 'NONE',  ( 6.667912619822566000, 6.673652899414787676, 1.040834085586084257E-14 ) ) ;
#157191 = VERTEX_POINT ( 'NONE', #117068 ) ;
#157192 = CARTESIAN_POINT ( 'NONE',  ( 0.000000000000000000, 3.956598013261175772, 0.000000000000000000 ) ) ;
#157193 = ORIENTED_EDGE ( 'NONE', *, *, #64923, .F. ) ;
#157194 = CARTESIAN_POINT ( 'NONE',  ( 3.053145041208281452, -1.596494782498259157, 0.8559496646718143253 ) ) ;
#157195 = VERTEX_POINT ( 'NONE', #183066 ) ;
#157196 = CARTESIAN_POINT ( 'NONE',  ( 8.353795204314554468, 12.89784483834236184, -0.7998128361456352531 ) ) ;
#157197 = CARTESIAN_POINT ( 'NONE',  ( 5.357406976055401948, 6.279338222599979424, 1.199719254218452935 ) ) ;
#157198 = CARTESIAN_POINT ( 'NONE',  ( 3.879414023784663712, 0.2179053609261162039, -1.798230022952992613 ) ) ;
#157199 = CARTESIAN_POINT ( 'NONE',  ( 6.539320575229256249, 6.037491965140660000, 2.591644950450102680 ) ) ;
#157200 = DIRECTION ( 'NONE',  ( -0.7592566023653004592, -0.6507913734559641616, 0.000000000000000000 ) ) ;
#157201 = CARTESIAN_POINT ( 'NONE',  ( 5.892130686423356245, 5.977214202646935703, -0.03562020706840245132 ) ) ;
#157203 = CARTESIAN_POINT ( 'NONE',  ( 1.364683531249996529, 14.46354166700806410, 0.7879004041258405033 ) ) ;
#157202 = CARTESIAN_POINT ( 'NONE',  ( 4.263987252221818736, -1.856165113571141445, 0.1354236832897796894 ) ) ;
#157204 = CARTESIAN_POINT ( 'NONE',  ( 1.880356884260485195, -0.5129869988758984922, -1.845544782535366801 ) ) ;
#157205 = CARTESIAN_POINT ( 'NONE',  ( 1.201864610381056853, -1.825762228264395048, -0.004348209057210283834 ) ) ;
#157206 = CIRCLE ( 'NONE', #184833, 0.05000000000000109912 ) ;
#157207 = CARTESIAN_POINT ( 'NONE',  ( 4.816680029521997142, 8.110538062004499338, 0.8573938582591574820 ) ) ;
#157208 = CYLINDRICAL_SURFACE ( 'NONE', #150765, 11.00000000000000000 ) ;
#157209 = CARTESIAN_POINT ( 'NONE',  ( 6.017777097630443883, 7.067734144800174256, 1.048426327298467742 ) ) ;
#157210 = CARTESIAN_POINT ( 'NONE',  ( 9.482679952114482447, 14.00853213111861351, 8.402045824544956076 ) ) ;
#157211 = CARTESIAN_POINT ( 'NONE',  ( -10.99943592164172834, -9.900000000000005684, 0.1113975120798846308 ) ) ;
#157212 = CARTESIAN_POINT ( 'NONE',  ( -4.161449568064929494, 3.976298073660712529, 0.4629614534431922834 ) ) ;
#157213 = AXIS2_PLACEMENT_3D ( 'NONE', #180106, #97803, #14375 ) ;
#157214 = CARTESIAN_POINT ( 'NONE',  ( 6.317736394288131052, 9.354147645769410602, 1.082531754730558626 ) ) ;
#157215 = CARTESIAN_POINT ( 'NONE',  ( 6.244967536942622743, -0.2852903188887367936, -1.948516424197583197 ) ) ;
#157216 = CARTESIAN_POINT ( 'NONE',  ( -3.952365473583647315, 4.569846793057691592, 1.199719254218462483 ) ) ;
#157217 = CARTESIAN_POINT ( 'NONE',  ( 0.1105426557568081891, -0.9253945370547181914, -1.951590883024490353 ) ) ;
#157218 = CARTESIAN_POINT ( 'NONE',  ( 1.377023180242874068, 1.931088066391934976, -0.8015266744223081830 ) ) ;
#157219 = CARTESIAN_POINT ( 'NONE',  ( 6.633821588623410648, -1.258873362295178655, -1.458256629947017879 ) ) ;
#157220 = CARTESIAN_POINT ( 'NONE',  ( -6.742482464697739708, 6.760651051769146491, 0.7998128361456341429 ) ) ;
#157221 = CARTESIAN_POINT ( 'NONE',  ( 1.043660158496478196, 0.7440559408637310579, -1.667260813828251642 ) ) ;
#157222 = CARTESIAN_POINT ( 'NONE',  ( 3.510573375967055654, -0.8941257848905452832, -2.017821460644920073 ) ) ;
#157223 = EDGE_CURVE ( 'NONE', #168515, #125736, #120986, .T. ) ;
#157224 = CARTESIAN_POINT ( 'NONE',  ( 11.94105721237523277, 12.69999999999999929, 1.187919463087245386 ) ) ;
#157225 = CARTESIAN_POINT ( 'NONE',  ( 0.5625819312903357350, 0.5574351770905332515, 1.829310545699929458 ) ) ;
#157226 = VERTEX_POINT ( 'NONE', #36807 ) ;
#157227 = AXIS2_PLACEMENT_3D ( 'NONE', #1087, #133285, #199292 ) ;
#157228 = CARTESIAN_POINT ( 'NONE',  ( 1.521857752106166695, 1.940948540861246352, -0.3334180107718246466 ) ) ;
#157229 = CARTESIAN_POINT ( 'NONE',  ( 2.665492718168083641, 1.041058713608807418, 1.639284265488485381 ) ) ;
#157230 = ORIENTED_EDGE ( 'NONE', *, *, #187873, .F. ) ;
#157231 = CARTESIAN_POINT ( 'NONE',  ( -4.650083499807250220, 5.295740330745369207, -7.499999999999997335 ) ) ;
#157233 = CARTESIAN_POINT ( 'NONE',  ( 6.209776894639321476, 0.5414253987558427239, -1.780396208465367280 ) ) ;
#157232 = CARTESIAN_POINT ( 'NONE',  ( -6.154475385960665790, 6.144919136567696505, 0.000000000000000000 ) ) ;
#157234 = CARTESIAN_POINT ( 'NONE',  ( 5.761288931164342486, 5.686201605971993978, -0.7998128361456481317 ) ) ;
#157235 = CARTESIAN_POINT ( 'NONE',  ( 0.06258739273032451478, -9.383611379567494026, -9.609645335164882951 ) ) ;
#157236 = CARTESIAN_POINT ( 'NONE',  ( -7.834948825496938163, -5.907420853759296264, -7.720982897393569466 ) ) ;
#157237 = CARTESIAN_POINT ( 'NONE',  ( -6.123442655227560927, 7.173046514967467147, 1.199719254218452047 ) ) ;
#157238 = CARTESIAN_POINT ( 'NONE',  ( 2.085717061910817183, -0.9337068281064246911, 1.982830571388309204 ) ) ;
#157239 =( NAMED_UNIT ( * ) SI_UNIT ( $, .STERADIAN. ) SOLID_ANGLE_UNIT ( ) );
#157240 = CARTESIAN_POINT ( 'NONE',  ( 10.91970695577495754, -6.134628647623513231, 1.924458856161770370E-15 ) ) ;
#157241 = CARTESIAN_POINT ( 'NONE',  ( 4.207107738942202246, 3.802713871720993399, 1.214306433183764966E-14 ) ) ;
#157243 = EDGE_CURVE ( 'NONE', #23953, #35460, #149176, .T. ) ;
#157242 = CARTESIAN_POINT ( 'NONE',  ( 2.736711336054332921, 0.2235625380298221498, 1.811883384933578256 ) ) ;
#157244 = CARTESIAN_POINT ( 'NONE',  ( -2.279742385392243165, 5.811449882932888222, -0.7998128361456281477 ) ) ;
#157245 = CARTESIAN_POINT ( 'NONE',  ( -4.992018142146231519, 8.041046192835899831, -1.132135330316372590 ) ) ;
#157246 = DIRECTION ( 'NONE',  ( 0.000000000000000000, 1.000000000000000000, -0.000000000000000000 ) ) ;
#157247 = CARTESIAN_POINT ( 'NONE',  ( 8.483651433849084711, 10.92067931095586886, 1.599625672291281386 ) ) ;
#157248 = CARTESIAN_POINT ( 'NONE',  ( 1.910648867733771850, 1.427813452364127045, -1.293523827780170166 ) ) ;
#157249 = CARTESIAN_POINT ( 'NONE',  ( 5.524254240939322713, 0.9636562883742012531, 1.708648623189083393 ) ) ;
#157250 = CARTESIAN_POINT ( 'NONE',  ( 1.499999999999993117, 14.85416666666666252, 0.8660254037844409281 ) ) ;
#157251 = CARTESIAN_POINT ( 'NONE',  ( -6.877010230629689858, 9.046264573866535486, 1.599625672291283607 ) ) ;
#157252 = CARTESIAN_POINT ( 'NONE',  ( 5.345992642490140057, 5.131412925860272090, 1.040834085586084257E-14 ) ) ;
#157253 = CARTESIAN_POINT ( 'NONE',  ( -5.926322542504884439, 6.086666852443364029, -0.7216878364870338292 ) ) ;
#157254 = CIRCLE ( 'NONE', #5053, 6.249999999999995559 ) ;
#157255 = CARTESIAN_POINT ( 'NONE',  ( 4.000000000000012434, 0.000000000000000000, -0.7500000000000006661 ) ) ;
#157256 = CARTESIAN_POINT ( 'NONE',  ( -2.155383234892699562, 5.458438174109348395, 1.040834085586084257E-14 ) ) ;
#157257 = CARTESIAN_POINT ( 'NONE',  ( 5.172746982222708567, 1.431596967658786745, -1.495705434250683918 ) ) ;
#157259 = CARTESIAN_POINT ( 'NONE',  ( -1.201851678989727383E-14, 2.384375000341416584, 1.575800808251672791 ) ) ;
#157258 = CARTESIAN_POINT ( 'NONE',  ( -1.556029036868112447, 0.4000000000000010214, 1.827231139298829632 ) ) ;
#157260 = VERTEX_POINT ( 'NONE', #164694 ) ;
#157261 = ORIENTED_EDGE ( 'NONE', *, *, #184187, .T. ) ;
#157262 = CARTESIAN_POINT ( 'NONE',  ( 5.080843078579284189, -0.8290085517158821693, 2.144167039965215071 ) ) ;
#157263 = CARTESIAN_POINT ( 'NONE',  ( 6.073689629242148058, 8.109057205581079231, -1.443375672974057666 ) ) ;
#157265 = CARTESIAN_POINT ( 'NONE',  ( 1.718115394875207702, -1.500000000000000888, -2.017567716309123682 ) ) ;
#157264 = CARTESIAN_POINT ( 'NONE',  ( 5.017926250833595780, 7.907978821730911712, -1.082531754730548412 ) ) ;
#157266 = CARTESIAN_POINT ( 'NONE',  ( 0.2172540613933468812, -0.1060665143617581102, 2.289936275665432674 ) ) ;
#157268 = EDGE_CURVE ( 'NONE', #111968, #117552, #202465, .T. ) ;
#157267 = CARTESIAN_POINT ( 'NONE',  ( 1.154700538379228147, -2.500000000000002220, -1.734723475976807094E-15 ) ) ;
#157269 = CARTESIAN_POINT ( 'NONE',  ( -6.180537922983287302, 8.303989891604203422, -1.599625672291271394 ) ) ;
#157270 = CARTESIAN_POINT ( 'NONE',  ( 4.417874594837376101, 1.193482090904834925, -1.531842204047480616 ) ) ;
#157271 = VERTEX_POINT ( 'NONE', #20551 ) ;
#157272 = CARTESIAN_POINT ( 'NONE',  ( 9.856414487010592751, 10.60149777770828194, 0.7216878364870438212 ) ) ;
#157273 = ADVANCED_FACE ( 'NONE', ( #85564 ), #151653, .F. ) ;
#157274 = ORIENTED_EDGE ( 'NONE', *, *, #157159, .F. ) ;
#157275 = CARTESIAN_POINT ( 'NONE',  ( 6.275647926998929371, 0.3200337115364471074, -1.885262484646982095 ) ) ;
#157276 = CARTESIAN_POINT ( 'NONE',  ( -0.005825499538506145533, -0.3671160670182890273, -1.691004160741523155 ) ) ;
#157277 = CARTESIAN_POINT ( 'NONE',  ( 5.384000029850495750, -2.016708404008683786, 0.004832792792668073358 ) ) ;
#157279 = CARTESIAN_POINT ( 'NONE',  ( -3.689227196694346400, 6.357829925235092716, -1.082531754730546636 ) ) ;
#157278 = CARTESIAN_POINT ( 'NONE',  ( -9.612894607289142357, 11.17379744904754801, -1.199719254218441611 ) ) ;
#157280 = CARTESIAN_POINT ( 'NONE',  ( -1.642778471875000035, -1.305208332855377407, -2.845375778867859751 ) ) ;
#157282 = CARTESIAN_POINT ( 'NONE',  ( 0.1096998152198442600, -0.7512755041745984297, -1.601369504124000587 ) ) ;
#157281 = CARTESIAN_POINT ( 'NONE',  ( 2.168024591681999791, -1.285456077792548335, 1.648657952768191715 ) ) ;
#157283 = CARTESIAN_POINT ( 'NONE',  ( 6.188124994278807023, 1.678003296889327034, 1.117835524071027598 ) ) ;
#157285 = CARTESIAN_POINT ( 'NONE',  ( 2.783473570837506017, 1.621738419858234304, 1.620254553110695772 ) ) ;
#157284 = CARTESIAN_POINT ( 'NONE',  ( 3.223806664999388172, 6.983134552466421674, -0.7998128361456362523 ) ) ;
#157286 = CARTESIAN_POINT ( 'NONE',  ( 2.044474178175458068, -1.396829902048246197, -1.037857226380611619 ) ) ;
#157287 = CARTESIAN_POINT ( 'NONE',  ( 5.984665970559388093, 7.172686677051047788, -1.260417782354812832 ) ) ;
#157288 = CARTESIAN_POINT ( 'NONE',  ( 2.336848640490073237, -1.070562806433389857, 1.363724479458855443 ) ) ;
#157289 = CARTESIAN_POINT ( 'NONE',  ( -1.360316468750028651, 1.692708333674761922, 0.7853790794158620470 ) ) ;
#157290 = CARTESIAN_POINT ( 'NONE',  ( 1.240418688720058560, -1.814558931778247119, -0.4126190233522536444 ) ) ;
#157291 = CARTESIAN_POINT ( 'NONE',  ( 2.348295082997472250, -0.9299805079447539535, 1.962071136543291683 ) ) ;
#157292 = CARTESIAN_POINT ( 'NONE',  ( 3.573454097414618946, 1.463926983822515293, 1.387100322000796027 ) ) ;
#157293 = CARTESIAN_POINT ( 'NONE',  ( 5.062500000000005329, -1.451031289061317064, -1.451031289060909168 ) ) ;
#157294 = CARTESIAN_POINT ( 'NONE',  ( -1.500000000000011324, 3.452083334016151639, 0.8660254037844403729 ) ) ;
#157295 = CARTESIAN_POINT ( 'NONE',  ( 0.6395170938602061650, -1.359983930408629194, -1.364592209491755082 ) ) ;
#157296 = CARTESIAN_POINT ( 'NONE',  ( 1.364683531249997417, 14.48437500034140157, 2.602085213965210642E-15 ) ) ;
#157297 = CARTESIAN_POINT ( 'NONE',  ( 3.797323596237450971, -0.2205154750010793197, -2.210469098741683514 ) ) ;
#157298 = ORIENTED_EDGE ( 'NONE', *, *, #126517, .T. ) ;
#157299 = CARTESIAN_POINT ( 'NONE',  ( -0.2108831679771167866, 1.375689764684871808, -2.152500126786048185 ) ) ;
#157300 = CARTESIAN_POINT ( 'NONE',  ( 1.499999999999987121, 0.7958333333333510451, -0.8660254037844253849 ) ) ;
#157301 = CARTESIAN_POINT ( 'NONE',  ( 8.209625708274705502, 9.536650400197368427, 1.199719254218462483 ) ) ;
#157302 = CARTESIAN_POINT ( 'NONE',  ( -1.402160292154681736E-14, -0.6781249996585819728, 1.575800808251672791 ) ) ;
#157303 = CARTESIAN_POINT ( 'NONE',  ( 5.801095770108652516, -0.3255204119565913157, -2.197341616521626406 ) ) ;
#157304 = CARTESIAN_POINT ( 'NONE',  ( 4.914483161888778540, 0.7490505147796694407, 1.813437088826752142 ) ) ;
#157306 = CARTESIAN_POINT ( 'NONE',  ( -5.097502569058207200, 8.890910730635814829, -0.7216878364870207285 ) ) ;
#157305 = CARTESIAN_POINT ( 'NONE',  ( 9.164948653157988900, 11.71552606681625619, -1.443375672974057666 ) ) ;
#157307 = SURFACE_STYLE_FILL_AREA ( #40358 ) ;
#157308 = CARTESIAN_POINT ( 'NONE',  ( 6.011039796215681186, 1.991063742206979459, 1.074381780396720165 ) ) ;
#157309 = CARTESIAN_POINT ( 'NONE',  ( -4.828112100242279325, 8.646898193675708555, -0.7216878364870338292 ) ) ;
#157310 = CARTESIAN_POINT ( 'NONE',  ( 2.295447401932719345, -1.843475527790199964, 0.9254330757148797604 ) ) ;
#157311 = CARTESIAN_POINT ( 'NONE',  ( -4.855791571988752331, 8.816840600628864877, 0.7998128361456481317 ) ) ;
#157312 = ORIENTED_EDGE ( 'NONE', *, *, #6621, .T. ) ;
#157313 = CARTESIAN_POINT ( 'NONE',  ( 0.7499999999999902300, 2.014583334016148530, 1.299038105676669330 ) ) ;
#157314 = CARTESIAN_POINT ( 'NONE',  ( 0.6823417656249917140, 4.405208333674755394, 1.181850606188765695 ) ) ;
#157315 = CARTESIAN_POINT ( 'NONE',  ( 4.376139848268215893, -1.078761963904120602, 1.527931137620001989 ) ) ;
#157316 = CARTESIAN_POINT ( 'NONE',  ( 3.269848819717678712, 1.566352396371019973, -0.7445194440909275180 ) ) ;
#157317 = CARTESIAN_POINT ( 'NONE',  ( 2.577381053492054264, -0.8929794387350452611, 1.493718712549793715 ) ) ;
#157318 = CARTESIAN_POINT ( 'NONE',  ( 0.7675861853312654359, 2.207383698986573162, -0.6181827981695892094 ) ) ;
#157319 = CARTESIAN_POINT ( 'NONE',  ( 1.571597221169357628, 0.1616201177277211132, -2.200922231076734459 ) ) ;
#157320 = CARTESIAN_POINT ( 'NONE',  ( 4.546477914129923192, -1.678139501482888152, 1.246787890680167710 ) ) ;
#157321 = CARTESIAN_POINT ( 'NONE',  ( 5.964781414698055784, 0.1407378593174268555, -1.936906258807554071 ) ) ;
#157322 = DIRECTION ( 'NONE',  ( 0.000000000000000000, 1.000000000000000000, 0.000000000000000000 ) ) ;
#157323 = CARTESIAN_POINT ( 'NONE',  ( 0.2994542103806375200, 1.388483683912977495, -1.462447666687356485 ) ) ;
#157324 = SURFACE_SIDE_STYLE ('',( #44644 ) ) ;
#157325 = CARTESIAN_POINT ( 'NONE',  ( 0.000000000000000000, 1.000000000000000888, 0.000000000000000000 ) ) ;
#157326 = CARTESIAN_POINT ( 'NONE',  ( -3.054546515950523400, 6.451825606165701110, 0.6676900015689657408 ) ) ;
#157327 = CARTESIAN_POINT ( 'NONE',  ( -7.831806290188425557, 12.28885777186185990, -0.7998128361456281477 ) ) ;
#157328 = CARTESIAN_POINT ( 'NONE',  ( 5.621827251160867789, 9.710548892996357040, 1.040834085586084257E-14 ) ) ;
#157329 = LINE ( 'NONE', #8921, #42684 ) ;
#157330 = CARTESIAN_POINT ( 'NONE',  ( 4.740742070742828496, 0.3150700179065483719, 1.798135100120237251 ) ) ;
#157331 = EDGE_CURVE ( 'NONE', #160543, #84121, #179102, .T. ) ;
#157332 = CARTESIAN_POINT ( 'NONE',  ( 1.852830919558448697, 0.6925466627333074499, 2.095365425716289032 ) ) ;
#157333 = VERTEX_POINT ( 'NONE', #87702 ) ;
#157334 = CARTESIAN_POINT ( 'NONE',  ( -7.930593509350902792, 8.217056947189661287, -0.7998128361456362523 ) ) ;
#157335 = AXIS2_PLACEMENT_3D ( 'NONE', #192695, #173287, #205754 ) ;
#157336 = UNCERTAINTY_MEASURE_WITH_UNIT (LENGTH_MEASURE( 1.000000000000000082E-05 ), #54350, 'distance_accuracy_value', 'NONE');
#157337 = CARTESIAN_POINT ( 'NONE',  ( -4.004454267989906668, 5.765225627445230927, 1.599625672291270506 ) ) ;
#157338 = CARTESIAN_POINT ( 'NONE',  ( 3.285556943749998737, -2.442708332855375364, -1.896917185911906500 ) ) ;
#157339 = CARTESIAN_POINT ( 'NONE',  ( -6.989391883044787868, 8.113044270762433285, -1.199719254218446718 ) ) ;
#157340 = CARTESIAN_POINT ( 'NONE',  ( 1.019792603244329410, -0.4866989216864863188, 1.960159232486478498 ) ) ;
#157341 = CARTESIAN_POINT ( 'NONE',  ( 0.3554123170483105554, 14.00000000000028955, -12.67999999502907649 ) ) ;
#157342 = CARTESIAN_POINT ( 'NONE',  ( -4.797606254389363833, 6.690569611577942943, 1.599625672291263179 ) ) ;
#157343 = CARTESIAN_POINT ( 'NONE',  ( 3.203785720953303606, 0.6742969627455961401, -1.734658892920079243 ) ) ;
#157344 = CARTESIAN_POINT ( 'NONE',  ( 2.703961570921634028, 5.242040035128820108, -1.199719254218446718 ) ) ;
#157345 = CARTESIAN_POINT ( 'NONE',  ( -4.911258385257075254, 4.778213610993594429, 0.3496101188117561875 ) ) ;
#157346 = VERTEX_POINT ( 'NONE', #25886 ) ;
#157347 = ORIENTED_EDGE ( 'NONE', *, *, #73875, .T. ) ;
#157348 = CARTESIAN_POINT ( 'NONE',  ( -4.446184310277715213, 7.274633231044262516, -1.199719254218452047 ) ) ;
#157349 = CARTESIAN_POINT ( 'NONE',  ( -7.635213062790267458, 12.05949900656400686, 0.000000000000000000 ) ) ;
#157350 = CARTESIAN_POINT ( 'NONE',  ( 4.002439121739418404, -0.5745171773131328985, -1.733004836422600725 ) ) ;
#157352 = CARTESIAN_POINT ( 'NONE',  ( 3.475000000000000533, -3.004166666666665542, 2.006292185433948827 ) ) ;
#157351 = CARTESIAN_POINT ( 'NONE',  ( -4.679499295372141709, 5.488445928469455559, 1.199719254218452935 ) ) ;
#157353 = CARTESIAN_POINT ( 'NONE',  ( 6.184762415132515123, 7.051423785172313607, -1.050594063207562545 ) ) ;
#157354 = CARTESIAN_POINT ( 'NONE',  ( 6.890000000000050306, -0.002781820520068867264, 1.999840353888074240 ) ) ;
#157355 = CARTESIAN_POINT ( 'NONE',  ( 5.665905727187005247, -1.164751086281138770, 1.425882759469448979 ) ) ;
#157356 = CARTESIAN_POINT ( 'NONE',  ( 4.530063604893081575, -1.417328398590127714, -1.821081770091488083 ) ) ;
#157357 = CARTESIAN_POINT ( 'NONE',  ( 3.705121118284530279, 7.544668081299086282, -1.734723475976807094E-15 ) ) ;
#157358 = CARTESIAN_POINT ( 'NONE',  ( 0.6321923500852930644, 1.061553894661429576, -1.766199267744901658 ) ) ;
#157359 = CARTESIAN_POINT ( 'NONE',  ( 5.360842878201462547, -0.8341330746063200241, 2.141841041818067559 ) ) ;
#157360 = CARTESIAN_POINT ( 'NONE',  ( 2.687227643083427534E-13, -3.232243495192088201, 3.285556943749999625 ) ) ;
#157362 = VECTOR ( 'NONE', #121648, 1000.000000000000000 ) ;
#157361 = CARTESIAN_POINT ( 'NONE',  ( -5.015590482412729756, 4.816220082428420923, 0.000000000000000000 ) ) ;
#157363 = CARTESIAN_POINT ( 'NONE',  ( 5.787941465827733722, -0.8397648285632768328, 1.671655200917811168 ) ) ;
#157365 = CARTESIAN_POINT ( 'NONE',  ( -5.320648938720212051, 5.172121614787156929, 0.000000000000000000 ) ) ;
#157364 = CARTESIAN_POINT ( 'NONE',  ( 2.056764645581514728, 0.4224895836346024280, 1.864965418913032913 ) ) ;
#157366 = CARTESIAN_POINT ( 'NONE',  ( 3.668774463136436736, -1.482526648764719734, 1.634931011441637771 ) ) ;
#157367 = CARTESIAN_POINT ( 'NONE',  ( 4.610634390349757084, 2.027228601534016406, 0.6112464051817678712 ) ) ;
#157368 = CARTESIAN_POINT ( 'NONE',  ( 1.224999999999947020, 0.1666666673495328654, 0.7072540797572737237 ) ) ;
#157369 = CARTESIAN_POINT ( 'NONE',  ( 6.883263157960370471, 7.052343128562386987, 2.644342559190917541 ) ) ;
#157370 = CARTESIAN_POINT ( 'NONE',  ( -0.2110808730066961458, 1.402160971018800995, -2.056005932258188285 ) ) ;
#157371 = CARTESIAN_POINT ( 'NONE',  ( 6.170369307550831017, 6.371388078330353366, 0.7216878364870328300 ) ) ;
#157372 = CARTESIAN_POINT ( 'NONE',  ( -4.245111494410291897, 7.006361605903701495, 1.082531754730549967 ) ) ;
#157373 = CARTESIAN_POINT ( 'NONE',  ( 1.782679935646735769, -1.233298141988391272, 1.950204222970158385 ) ) ;
#157374 = CARTESIAN_POINT ( 'NONE',  ( 3.244534624505683418, -1.932379277470747558, -0.3379807920969243873 ) ) ;
#157375 = CARTESIAN_POINT ( 'NONE',  ( -4.960304097753355457, 6.880383762169266504, 1.599625672291263401 ) ) ;
#157376 = EDGE_CURVE ( 'NONE', #166389, #51765, #22235, .T. ) ;
#157377 = CARTESIAN_POINT ( 'NONE',  ( 6.789892339975323488, -1.342670783288713698, -1.565829586757736758 ) ) ;
#157378 = CARTESIAN_POINT ( 'NONE',  ( 4.704316114261903436, 4.590716342834741504, 1.214306433183764966E-14 ) ) ;
#157379 = CARTESIAN_POINT ( 'NONE',  ( 4.686278372178935392, 5.496354851410763409, 1.199719254218452047 ) ) ;
#157380 = VERTEX_POINT ( 'NONE', #171079 ) ;
#157381 = CARTESIAN_POINT ( 'NONE',  ( 4.276577519141481432, -0.4465006364167342645, -1.966305148836451577 ) ) ;
#157382 = CARTESIAN_POINT ( 'NONE',  ( -9.969323024750229578, 10.52529837183042716, -0.7998128361456291469 ) ) ;
#157383 =( BOUNDED_SURFACE ( )  B_SPLINE_SURFACE ( 3, 2, ( 
 ( #194863, #109428, #25957 ),
 ( #178630, #9711, #190585 ),
 ( #30242, #93127, #58472 ),
 ( #110490, #124627, #75787 ),
 ( #207905, #60594, #126752 ),
 ( #59526, #44367, #176489 ),
 ( #28100, #87254, #4893 ),
 ( #3829, #214264, #185797 ) ),
 .UNSPECIFIED., .F., .F., .T. ) 
 B_SPLINE_SURFACE_WITH_KNOTS ( ( 4, 2, 2, 4 ),
 ( 3, 3 ),
 ( -2.710505431213761085E-20, 0.0002475938981900015407, 0.0004951877963800030815, 0.0009903755927600061629 ),
 ( 0.000000000000000000, 1.000000000000000000 ),
 .UNSPECIFIED. ) 
 GEOMETRIC_REPRESENTATION_ITEM ( )  RATIONAL_B_SPLINE_SURFACE ( (
 ( 1.000000000000000000, 0.9238795325112871826, 1.000000000000000000),
 ( 1.000000000000000000, 0.9248499699754035852, 1.000000000000000000),
 ( 1.000000000000000000, 0.9171047238582761274, 1.000000000000000000),
 ( 1.000000000000000000, 0.8907236462370136110, 1.000000000000000000),
 ( 1.000000000000000000, 0.8725411758594030509, 1.000000000000000000),
 ( 1.000000000000000000, 0.8105159241144254123, 1.000000000000000000),
 ( 1.000000000000000000, 0.7599483315139430317, 1.000000000000000000),
 ( 1.000000000000000000, 0.7045118851637766078, 1.000000000000000000) ) ) 
 REPRESENTATION_ITEM ( '' )  SURFACE ( )  );
#157385 = CARTESIAN_POINT ( 'NONE',  ( -1.499999999999997780, 4.150000000000021672, 1.214306433183764966E-14 ) ) ;
#157384 = VECTOR ( 'NONE', #16358, 1000.000000000000000 ) ;
#157386 = CARTESIAN_POINT ( 'NONE',  ( -10.52284260640670688, 5.420240069097000735, -5.071998063130033430 ) ) ;
#157387 = CARTESIAN_POINT ( 'NONE',  ( 8.748035429315576650, 11.22912730566677553, -1.599625672291255185 ) ) ;
#157388 = CARTESIAN_POINT ( 'NONE',  ( 2.167058194802372828, 1.611091607626200961, -1.455523108145313937 ) ) ;
#157389 = CARTESIAN_POINT ( 'NONE',  ( 5.337069745634900997, 6.255611453776062980, 1.199719254218452047 ) ) ;
#157390 = CARTESIAN_POINT ( 'NONE',  ( 4.774898309648160755, 8.276035162536045320, 0.8191430224755236189 ) ) ;
#157391 = CARTESIAN_POINT ( 'NONE',  ( 0.7728169288007546989, -1.939476032597256872, -0.6969182633713083552 ) ) ;
#157393 = CARTESIAN_POINT ( 'NONE',  ( -4.907894938888482272, 6.474487383728027012, -2.499999999999995559 ) ) ;
#157392 = CARTESIAN_POINT ( 'NONE',  ( 0.07755575628183572490, 2.860544851022389867, -2.677061994759164065 ) ) ;
#157394 = CARTESIAN_POINT ( 'NONE',  ( 0.6823417656249882723, 0.09270833367475139752, 1.181850606188755259 ) ) ;
#157395 = PLANE ( 'NONE',  #128483 ) ;
#157396 =( BOUNDED_CURVE ( )  B_SPLINE_CURVE ( 2, ( #157189, #206980, #90062, #22880, #156124 ),
 .UNSPECIFIED., .F., .T. ) 
 B_SPLINE_CURVE_WITH_KNOTS ( ( 3, 2, 3 ),
 ( 0.2462631119352014508, 0.2500000000000000000, 0.2543051829449332057 ),
 .UNSPECIFIED. ) 
 CURVE ( )  GEOMETRIC_REPRESENTATION_ITEM ( )  RATIONAL_B_SPLINE_CURVE ( ( 0.9337253982215369952, 0.9399222316499036278, 1.000000000000000000, 0.9307857823982145229, 0.9330867333962934440 ) ) 
 REPRESENTATION_ITEM ( '' )  );
#157397 = ORIENTED_EDGE ( 'NONE', *, *, #2500, .T. ) ;
#157398 = CARTESIAN_POINT ( 'NONE',  ( 3.527896108305649037, -1.883508717751972705, 0.3295761852530054159 ) ) ;
#157399 = CARTESIAN_POINT ( 'NONE',  ( 5.260532772634206822, -1.280100971201453497, 1.222426461919926322 ) ) ;
#157400 = AXIS2_PLACEMENT_3D ( 'NONE', #41285, #6599, #39129 ) ;
#157401 = CARTESIAN_POINT ( 'NONE',  ( 5.794130544993763898, 7.853181283949808744, 1.599625672291269396 ) ) ;
#157402 = CARTESIAN_POINT ( 'NONE',  ( -4.711622075948912247, 5.455646162483875017, -1.199719254218446718 ) ) ;
#157404 = CARTESIAN_POINT ( 'NONE',  ( 6.081633583971849610, -0.6405020660514448849, 1.805506905929341821 ) ) ;
#157403 = FACE_OUTER_BOUND ( 'NONE', #86219, .T. ) ;
#157405 = CARTESIAN_POINT ( 'NONE',  ( -1.402160292154681736E-14, 0.4625000000000214495, 1.732050807568877637 ) ) ;
#157406 = CARTESIAN_POINT ( 'NONE',  ( 1.117730493923989599, 0.4056601665377962407, -2.030061024271647252 ) ) ;
#157407 = CARTESIAN_POINT ( 'NONE',  ( -1.402160292154681736E-14, -0.9906249996585834161, -1.575800808251665908 ) ) ;
#157408 = EDGE_CURVE ( 'NONE', #177833, #45474, #77622, .T. ) ;
#157409 = CARTESIAN_POINT ( 'NONE',  ( 6.438356904408193415, 1.850619875698428674, 0.2722718653145329015 ) ) ;
#157410 = CARTESIAN_POINT ( 'NONE',  ( 1.998415063578623085, -0.4859047700337820741, -1.759764234465097221 ) ) ;
#157412 = CARTESIAN_POINT ( 'NONE',  ( 4.990887655837901171, 7.926359819171765686, 1.063311220390166234 ) ) ;
#157411 = CARTESIAN_POINT ( 'NONE',  ( 5.584669497696876483, -2.152379054646291756, -0.4867646435422824935 ) ) ;
#157413 = CARTESIAN_POINT ( 'NONE',  ( 1.364683531249986537, -0.09479166632524321789, -0.7879004041258309554 ) ) ;
#157414 = CARTESIAN_POINT ( 'NONE',  ( 3.420431513525914902, 0.9250737872015384333, 1.843656989716379035 ) ) ;
#157415 = CARTESIAN_POINT ( 'NONE',  ( -5.703176172842872482, 9.805455968292021041, 0.000000000000000000 ) ) ;
#157416 = CARTESIAN_POINT ( 'NONE',  ( 8.890396042259068210, 11.39521468743417998, -1.599625672291257406 ) ) ;
#157417 = CYLINDRICAL_SURFACE ( 'NONE', #48087, 1.224999999999996980 ) ;
#157418 = CARTESIAN_POINT ( 'NONE',  ( 0.5620833348847533717, 2.138143771118843350, -0.3165822943479515983 ) ) ;
#157419 = CARTESIAN_POINT ( 'NONE',  ( 7.354371980770088690, 7.544798497178720531, 0.000000000000000000 ) ) ;
#157420 = CARTESIAN_POINT ( 'NONE',  ( 4.932118098221458524, 1.189261692661430114, 1.694535115018414917 ) ) ;
#157421 = CARTESIAN_POINT ( 'NONE',  ( -0.6823417656250246877, -0.3864583329919110688, 1.181850606188755259 ) ) ;
#157422 = CARTESIAN_POINT ( 'NONE',  ( 3.304151629394710632, -2.159270932758147854, 0.1024373671053082913 ) ) ;
#157423 = CARTESIAN_POINT ( 'NONE',  ( -4.733264021794758136, 8.224961065399975624, 0.6825151564062783560 ) ) ;
#157425 = CARTESIAN_POINT ( 'NONE',  ( 2.558977423257744022, 1.577441344615847951, -1.166261179026031325 ) ) ;
#157424 = CARTESIAN_POINT ( 'NONE',  ( 3.088540408894335787, -1.201353318763114020, 1.623377594596470352 ) ) ;
#157426 = CARTESIAN_POINT ( 'NONE',  ( 6.720655732516665815, 6.034026441762381232, 2.768628153821062199 ) ) ;
#157427 = EDGE_CURVE ( 'NONE', #62417, #200114, #112808, .T. ) ;
#157430 = CARTESIAN_POINT ( 'NONE',  ( 6.100805936469477331, 9.101062111647635788, -1.082531754730537088 ) ) ;
#157429 = CARTESIAN_POINT ( 'NONE',  ( -3.475000000000000533, -1.779166666666666785, -2.006292185433948827 ) ) ;
#157428 = CARTESIAN_POINT ( 'NONE',  ( -0.7500000000000215383, 3.722916667349487785, 1.299038105676671107 ) ) ;
#157431 = CARTESIAN_POINT ( 'NONE',  ( -7.442499979258930587, 7.647614495415686164, -0.7998128361456362523 ) ) ;
#157432 = CARTESIAN_POINT ( 'NONE',  ( 1.692592581891849912, 1.490968054865527304, -1.357870634957742961 ) ) ;
#157434 = CARTESIAN_POINT ( 'NONE',  ( 6.356982542327763497, 0.3766756592470664744, -2.158781491689326426 ) ) ;
#157433 = CARTESIAN_POINT ( 'NONE',  ( -5.739179097286464248, 5.590130456455974617, -0.7998128361456221525 ) ) ;
#157435 = CARTESIAN_POINT ( 'NONE',  ( 4.270455198180219902, 6.965652916976816655, -1.082531754730548412 ) ) ;
#157436 = CARTESIAN_POINT ( 'NONE',  ( 5.431871263539022721, -1.864374737420209760, 0.4251265778823994368 ) ) ;
#157438 = CARTESIAN_POINT ( 'NONE',  ( 4.297571505407542958, 7.957657823043374989, -0.7216878364870197293 ) ) ;
#157437 = B_SPLINE_CURVE_WITH_KNOTS ( 'NONE', 3,
 ( #205531, #190348, #55037, #154669 ),
 .UNSPECIFIED., .F., .F.,
 ( 4, 4 ),
 ( 0.000000000000000000, 0.0007699926951938503451 ),
 .UNSPECIFIED. ) ;
#157440 = CARTESIAN_POINT ( 'NONE',  ( 3.304314702139679039, 1.277028363417181289, -1.560513873864778578 ) ) ;
#157439 = CARTESIAN_POINT ( 'NONE',  ( -7.822691444960700125, 11.10992853822074444, -1.082531754730543083 ) ) ;
#157441 = CARTESIAN_POINT ( 'NONE',  ( 0.7499999999999885647, 3.566666666666690411, -1.299038105676658228 ) ) ;
#157442 = CARTESIAN_POINT ( 'NONE',  ( -8.012344526598182026E-15, 13.10937500034140157, -1.575800808251669460 ) ) ;
#157443 = CARTESIAN_POINT ( 'NONE',  ( 6.247054435025749086, -1.454095476552646593, 0.9272665607438534963 ) ) ;
#157444 = CARTESIAN_POINT ( 'NONE',  ( 7.364013710877980401, 8.620379413226322285, -1.199719254218452047 ) ) ;
#157445 = CARTESIAN_POINT ( 'NONE',  ( 9.246297574839983824, 9.889694713509232571, 0.7216878364870438212 ) ) ;
#157446 = CARTESIAN_POINT ( 'NONE',  ( -11.43195036480942051, 11.15524496285257783, -3.649565797774410036 ) ) ;
#157447 = CARTESIAN_POINT ( 'NONE',  ( 4.323419078940895943, -1.790677508454678657, 0.5408235849187342792 ) ) ;
#157448 = SURFACE_STYLE_USAGE ( .BOTH. , #25287 ) ;
#157450 =( BOUNDED_CURVE ( )  B_SPLINE_CURVE ( 2, ( #10548, #189313, #124406, #206621, #125466 ),
 .UNSPECIFIED., .F., .T. ) 
 B_SPLINE_CURVE_WITH_KNOTS ( ( 3, 2, 3 ),
 ( 0.1232094925783373957, 0.1250000000000000000, 0.1270731450466760504 ),
 .UNSPECIFIED. ) 
 CURVE ( )  GEOMETRIC_REPRESENTATION_ITEM ( )  RATIONAL_B_SPLINE_CURVE ( ( 0.9343361104663525651, 0.9424281978788288106, 1.000000000000000000, 0.9333402950740685711, 0.9330143039465762511 ) ) 
 REPRESENTATION_ITEM ( '' )  );
#157449 = CARTESIAN_POINT ( 'NONE',  ( 2.395452669547156077, -1.851176756146424074, 0.9269567275110508486 ) ) ;
#157451 = CARTESIAN_POINT ( 'NONE',  ( -1.296982317953438165E-13, -8.296536394940860148, -10.41260094161052230 ) ) ;
#157452 = VERTEX_POINT ( 'NONE', #120280 ) ;
#157453 = CARTESIAN_POINT ( 'NONE',  ( 5.740951700743842423, 5.662474837148078421, -0.7998128361456481317 ) ) ;
#157454 = DIRECTION ( 'NONE',  ( -0.9486832980505139901, -0.3162277660168373861, 3.312310031615527941E-15 ) ) ;
#157455 = CARTESIAN_POINT ( 'NONE',  ( 0.2459857770662046417, 0.9310377468562742731, -1.553837941864342875 ) ) ;
#157456 = CARTESIAN_POINT ( 'NONE',  ( 4.760321331729593375, 5.686701320840210627, -1.082531754730548412 ) ) ;
#157457 = CARTESIAN_POINT ( 'NONE',  ( 10.87378820908022625, 9.632687173196126551, -5.088116269538504710 ) ) ;
#157458 = EDGE_LOOP ( 'NONE', ( #20743, #53762, #19185 ) ) ;
#157459 = CARTESIAN_POINT ( 'NONE',  ( 7.890482213029013536, 12.14938698193514277, 1.040834085586084257E-14 ) ) ;
#157461 = CARTESIAN_POINT ( 'NONE',  ( 7.938462636001388795, 9.220293482545153907, -1.199719254218441611 ) ) ;
#157460 = CARTESIAN_POINT ( 'NONE',  ( 1.996468121258226924, 1.940055844723225009, 0.2909814450420752929 ) ) ;
#157462 = CARTESIAN_POINT ( 'NONE',  ( 6.310162246266422414, 1.098484216484491904, -1.569160930707512502 ) ) ;
#157463 = CARTESIAN_POINT ( 'NONE',  ( -11.44779964734699540, 13.49810470129609286, 3.599999963171390593 ) ) ;
#157464 = CARTESIAN_POINT ( 'NONE',  ( -2.128168088883454642E-12, -3.089410100848593466, 3.428390338093493028 ) ) ;
#157465 = CARTESIAN_POINT ( 'NONE',  ( 0.3282377607281144472, 0.6763354503153764519, -1.225000000000007194 ) ) ;
#157467 = ORIENTED_EDGE ( 'NONE', *, *, #32785, .T. ) ;
#157466 = CARTESIAN_POINT ( 'NONE',  ( 3.551873057100283226, 6.127307085716883428, 1.082531754730558626 ) ) ;
#157468 = CARTESIAN_POINT ( 'NONE',  ( -6.548225005720456515, 10.58342024007512983, 0.000000000000000000 ) ) ;
#157469 = CARTESIAN_POINT ( 'NONE',  ( 2.659225025413253007, -1.880336703546074073, -1.066323988048664795 ) ) ;
#157470 = CARTESIAN_POINT ( 'NONE',  ( -4.604929450496978660, 5.401447776115099408, -1.199719254218453823 ) ) ;
#157471 = CARTESIAN_POINT ( 'NONE',  ( 5.994113311017540191, 9.046863725278862844, -1.082531754730548412 ) ) ;
#157472 = CARTESIAN_POINT ( 'NONE',  ( -2.981903720001798597, 5.566305875722335372, -1.199719254218446718 ) ) ;
#157473 = CARTESIAN_POINT ( 'NONE',  ( 5.561492448144861989, 0.3540975402388062410, -1.790731494587729067 ) ) ;
#157474 = EDGE_CURVE ( 'NONE', #10457, #107037, #189468, .T. ) ;
#157475 = CARTESIAN_POINT ( 'NONE',  ( 10.48926859151676005, 8.662495522311813190, -6.550045777748900733 ) ) ;
#157476 = CARTESIAN_POINT ( 'NONE',  ( 0.9660189047021714437, 0.9680410686894457273, 1.717217487461615955 ) ) ;
#157477 = CARTESIAN_POINT ( 'NONE',  ( 3.814637755342592307, -0.6046605605216844870, -1.814329123173196834 ) ) ;
#157478 = VERTEX_POINT ( 'NONE', #42176 ) ;
#157479 = CARTESIAN_POINT ( 'NONE',  ( -3.111427826557872756, 14.48006665645140956, -11.59831528793133337 ) ) ;
#157480 = CARTESIAN_POINT ( 'NONE',  ( 5.476995390384709061, 1.819097369218507732, 0.7554879866787550524 ) ) ;
#157481 = ORIENTED_EDGE ( 'NONE', *, *, #37467, .T. ) ;
#157482 = CARTESIAN_POINT ( 'NONE',  ( 5.917518263527802524, -1.082453682572570797, -1.612232301441741233 ) ) ;
#157483 = ORIENTED_EDGE ( 'NONE', *, *, #140722, .T. ) ;
#157484 = CARTESIAN_POINT ( 'NONE',  ( -4.610654757099099221, 7.536791762327691657, 1.199719254218452935 ) ) ;
#157486 = CARTESIAN_POINT ( 'NONE',  ( 6.949550370340926264, -6.532648880269158909, -6.447678837262559526 ) ) ;
#157485 = CARTESIAN_POINT ( 'NONE',  ( -4.176793841461789114, 7.030620694084159794, -1.199719254218455378 ) ) ;
#157488 = AXIS2_PLACEMENT_3D ( 'NONE', #200521, #171237, #119360 ) ;
#157487 = CARTESIAN_POINT ( 'NONE',  ( 6.441532379824158383, 9.568852638886589546, -1.082531754730548412 ) ) ;
#157490 = ORIENTED_EDGE ( 'NONE', *, *, #183389, .F. ) ;
#157489 = CARTESIAN_POINT ( 'NONE',  ( 4.477155480220369910, -1.709698060584059043, -0.8567103784868701499 ) ) ;
#157491 = CARTESIAN_POINT ( 'NONE',  ( 0.4291286860223575972, 2.112415399404877547, 0.6383354507134838540 ) ) ;
#157492 = FACE_OUTER_BOUND ( 'NONE', #149465, .T. ) ;
#157493 = CARTESIAN_POINT ( 'NONE',  ( 6.569000952640477564, -1.554625895936670554, 1.278542242695315689 ) ) ;
#157494 = CARTESIAN_POINT ( 'NONE',  ( -6.966220764712169000, 6.002124920821316323, -2.420000000000000373 ) ) ;
#157495 = CARTESIAN_POINT ( 'NONE',  ( 6.692070433991195166, -0.7751425012093198230, 1.651373049820707317 ) ) ;
#157496 = CARTESIAN_POINT ( 'NONE',  ( 2.119664376568120012, 0.3561266789769075292, -2.039353370234835872 ) ) ;
#157497 = CARTESIAN_POINT ( 'NONE',  ( -7.061099074618889304, 7.132370430010492868, -0.7998128361456291469 ) ) ;
#157498 = CARTESIAN_POINT ( 'NONE',  ( -5.575295409310188965, 7.417394932307940003, -1.244639187630245170 ) ) ;
#157499 = CARTESIAN_POINT ( 'NONE',  ( 0.000000000000000000, -9.006862915010128035, 0.000000000000000000 ) ) ;
#157500 = CARTESIAN_POINT ( 'NONE',  ( 6.491075539335432687, 1.626419376453295706, -0.9240138038444989377 ) ) ;
#157501 = CARTESIAN_POINT ( 'NONE',  ( 6.810273232766058449, 6.839740281182199233, 1.040834085586084257E-14 ) ) ;
#157502 = CYLINDRICAL_SURFACE ( 'NONE', #55521, 1.250000000000000000 ) ;
#157503 = CARTESIAN_POINT ( 'NONE',  ( 3.594320121398666856, 7.207474218358159490, -1.734723475976807094E-15 ) ) ;
#157504 = CARTESIAN_POINT ( 'NONE',  ( -1.402160292154681736E-14, 11.98437500034140335, 1.575800808251682339 ) ) ;
#157506 = CARTESIAN_POINT ( 'NONE',  ( -7.442499979258930587, 7.647614495415686164, -0.7998128361456362523 ) ) ;
#157505 = CARTESIAN_POINT ( 'NONE',  ( 6.925078400183578786, 2.094238355957972253, 2.065574651578235610 ) ) ;
#157508 = CARTESIAN_POINT ( 'NONE',  ( 5.027816288645148290, -1.483603310789272323, 0.8976219912088311270 ) ) ;
#157507 = VECTOR ( 'NONE', #62885, 1000.000000000000000 ) ;
#157509 = CARTESIAN_POINT ( 'NONE',  ( -5.199715606040888005, 6.025088614257851027, -1.199719254218446718 ) ) ;
#157510 = CARTESIAN_POINT ( 'NONE',  ( 2.289971195246335078, -1.349064171463711936, -1.570471239911851669 ) ) ;
#157511 = CARTESIAN_POINT ( 'NONE',  ( 3.251669871774115705, 2.065089526129770814, -0.4662906127247400945 ) ) ;
#157512 = CARTESIAN_POINT ( 'NONE',  ( 7.962716289927667113, 8.184257181204083409, -0.7998128361456291469 ) ) ;
#157513 = DIRECTION ( 'NONE',  ( 0.6507913734559658270, -0.7592566023652989049, 0.000000000000000000 ) ) ;
#157514 = CARTESIAN_POINT ( 'NONE',  ( 2.008593398387849671, 0.6130636034600014383, 1.871695086544410636 ) ) ;
#157515 = CARTESIAN_POINT ( 'NONE',  ( 5.993251976321238850, 6.092249680885792884, 0.6249505139499841322 ) ) ;
#157517 = CARTESIAN_POINT ( 'NONE',  ( 0.2285749388857594433, 1.317234250586714284, -1.386657971642536014 ) ) ;
#157516 = CARTESIAN_POINT ( 'NONE',  ( 1.737500000000001155, -1.633333333333333748, 3.009438278150922130 ) ) ;
#157518 = CARTESIAN_POINT ( 'NONE',  ( 3.890815911290066875, 1.937189890886330756, -1.225201777657213498 ) ) ;
#157520 = EDGE_CURVE ( 'NONE', #83982, #185214, #91569, .T. ) ;
#157519 = CARTESIAN_POINT ( 'NONE',  ( 1.717148762710469789, -0.2249250470785572054, 1.811706739299999924 ) ) ;
#157521 = CARTESIAN_POINT ( 'NONE',  ( 5.337069745634900997, 6.255611453776062980, 1.199719254218452047 ) ) ;
#157522 = CARTESIAN_POINT ( 'NONE',  ( 7.090551149822744925, 7.374657217655760100, 0.7216878364870317197 ) ) ;
#157523 = CARTESIAN_POINT ( 'NONE',  ( -8.182509401047415309, 9.505014708432145909, 1.199719254218462483 ) ) ;
#157524 = CARTESIAN_POINT ( 'NONE',  ( 2.830340462983381489, -0.9960867002655849900, -1.749474899777081704 ) ) ;
#157525 = CARTESIAN_POINT ( 'NONE',  ( 1.850371385673426294, -1.951817131159512719, -0.1975377159662907445 ) ) ;
#157526 = CARTESIAN_POINT ( 'NONE',  ( -7.645908563102897126, 11.00764485934031889, 1.199719254218453823 ) ) ;
#157527 = CARTESIAN_POINT ( 'NONE',  ( -4.713430959045263435, 8.650753218861462202, 0.7998128361456481317 ) ) ;
#157529 = ADVANCED_FACE ( 'NONE', ( #9642 ), #38959, .T. ) ;
#157528 = DIRECTION ( 'NONE',  ( 1.000000000000000000, -0.000000000000000000, -0.000000000000000000 ) ) ;
#157531 = CARTESIAN_POINT ( 'NONE',  ( 4.856192259477753126, 0.6790438925599675546, 1.634599669825251178 ) ) ;
#157530 = CARTESIAN_POINT ( 'NONE',  ( 5.349593081218750434, 2.088290806564324420, -0.1017214290881287009 ) ) ;
#157532 = CARTESIAN_POINT ( 'NONE',  ( -5.346851039111035320, 6.199209027673978412, 2.420000000000001261 ) ) ;
#157533 = CARTESIAN_POINT ( 'NONE',  ( 1.166276502169643070, -1.387892208999995436, 1.695937554688830451 ) ) ;
#157534 = CARTESIAN_POINT ( 'NONE',  ( 5.560439297528310121, -1.575983010118024774, -0.7385839837668640717 ) ) ;
#157535 = CARTESIAN_POINT ( 'NONE',  ( 8.925345196497941558, 9.307324238869423283, 1.040834085586084257E-14 ) ) ;
#157536 = CARTESIAN_POINT ( 'NONE',  ( 0.1331715793776782342, 4.090830978607494117, -2.508370148267160538 ) ) ;
#157537 = CARTESIAN_POINT ( 'NONE',  ( 6.100222456320119058, -0.2858642287353658218, 2.280774976835740819 ) ) ;
#157538 = CARTESIAN_POINT ( 'NONE',  ( 6.081315976822482483, 1.162057296412899676, -1.286934115659829736 ) ) ;
#157539 = CARTESIAN_POINT ( 'NONE',  ( 5.512245374570181156, 2.168932156859445737, -0.1011643165890318136 ) ) ;
#157540 = CARTESIAN_POINT ( 'NONE',  ( 5.484430959185961463, 6.043327615839654499, 0.8208683321978844649 ) ) ;
#157541 = CARTESIAN_POINT ( 'NONE',  ( 0.2513570338038995100, 0.2008850299538050832, -2.107768975555255331 ) ) ;
#157543 = TOROIDAL_SURFACE ( 'NONE', #15728, 10.75000000000000000, 0.5000000000000007772 ) ;
#157542 = CARTESIAN_POINT ( 'NONE',  ( 3.937500000000001776, 1.451031289060957574, -1.451031289061275320 ) ) ;
#157544 = CARTESIAN_POINT ( 'NONE',  ( 0.006800380015298257419, 7.009756401597622144, -1.999988438674496383 ) ) ;
#157545 = CARTESIAN_POINT ( 'NONE',  ( 4.928697230495170167, 1.843396615675118699, 0.5593075106890015302 ) ) ;
#157546 = CARTESIAN_POINT ( 'NONE',  ( -0.7500000000000006661, 11.48958333401613174, -1.299038105676657340 ) ) ;
#157547 = CARTESIAN_POINT ( 'NONE',  ( 0.6630925397578091296, 0.6502370396846578471, 2.123993688044391259 ) ) ;
#157548 = ORIENTED_EDGE ( 'NONE', *, *, #106610, .F. ) ;
#157549 = CARTESIAN_POINT ( 'NONE',  ( 1.499999999999989120, 4.004166666666685970, 0.8660254037844524744 ) ) ;
#157550 = CARTESIAN_POINT ( 'NONE',  ( 4.202137545231717120, 6.989912005157271402, 1.199719254218462483 ) ) ;
#157551 = CARTESIAN_POINT ( 'NONE',  ( 7.332262146892202459, 7.448727347662698506, -0.7998128361456281477 ) ) ;
#157552 = CARTESIAN_POINT ( 'NONE',  ( 2.438390712420679396, -1.281362850324974989, -1.814285216940268342 ) ) ;
#157553 = FACE_OUTER_BOUND ( 'NONE', #48476, .T. ) ;
#157554 = CARTESIAN_POINT ( 'NONE',  ( 6.982085921357777281, 7.248114451113292667, 1.040834085586084257E-14 ) ) ;
#157555 = CARTESIAN_POINT ( 'NONE',  ( -9.612367721964613310, 11.27714576612263997, -1.082531754730537976 ) ) ;
#157556 = EDGE_CURVE ( 'NONE', #158833, #179029, #198662, .T. ) ;
#157557 = CARTESIAN_POINT ( 'NONE',  ( 5.546694241766559230, 9.485244025454063532, 0.000000000000000000 ) ) ;
#157558 = AXIS2_PLACEMENT_3D ( 'NONE', #195824, #165448, #98326 ) ;
#157559 = CARTESIAN_POINT ( 'NONE',  ( 0.7213275451133926985, 1.987047012402185731, 0.3419330716275259530 ) ) ;
#157561 = CARTESIAN_POINT ( 'NONE',  ( 0.3739784900498700493, -2.023488180542520887, 0.3987778971655773219 ) ) ;
#157560 = CARTESIAN_POINT ( 'NONE',  ( 9.887974103068218668, 10.43039129653476493, 0.7998128361456462443 ) ) ;
#157562 = SURFACE_STYLE_FILL_AREA ( #120854 ) ;
#157563 = CARTESIAN_POINT ( 'NONE',  ( 6.577113915960825175, 8.766661883411348555, -1.443375672974078761 ) ) ;
#157564 = CARTESIAN_POINT ( 'NONE',  ( -2.554955805669734570, 1.016282880930316823, 12.02012201174058426 ) ) ;
#157565 = CARTESIAN_POINT ( 'NONE',  ( 0.6823417656249882723, 0.9260416670080831025, -1.181850606188749264 ) ) ;
#157566 = CARTESIAN_POINT ( 'NONE',  ( 1.844620604044054035, -1.498293487275937697, 0.9415191625909284934 ) ) ;
#157567 = CARTESIAN_POINT ( 'NONE',  ( 0.7389079861009685279, 2.013985778099684154, -0.1017531103126300962 ) ) ;
#157568 = CARTESIAN_POINT ( 'NONE',  ( 5.530708837500646347, -1.570004293196942013, 0.7514903552788397834 ) ) ;
#157569 = CARTESIAN_POINT ( 'NONE',  ( 3.720531229262864947, 2.177046216224611364, 0.7181995365407625176 ) ) ;
#157570 = CARTESIAN_POINT ( 'NONE',  ( -0.6823417656250003738, -0.5322916663252491576, -1.181850606188749264 ) ) ;
#157571 = CARTESIAN_POINT ( 'NONE',  ( 2.765369989423609454, 0.9851603262180377296, 1.555203531693909680 ) ) ;
#157572 = CIRCLE ( 'NONE', #143691, 0.07999999999999977962 ) ;
#157573 = CARTESIAN_POINT ( 'NONE',  ( 9.908311333488716954, 10.45411806535867782, 0.7998128361456462443 ) ) ;
#157574 = CARTESIAN_POINT ( 'NONE',  ( 2.819161699164650869, -0.1809198688003388622, 1.816599095187728219 ) ) ;
#157575 = CARTESIAN_POINT ( 'NONE',  ( 3.533827422916273164, -1.646839391163470223, 1.163268690995450383 ) ) ;
#157576 = CARTESIAN_POINT ( 'NONE',  ( -10.00321840878439339, 10.56484298653695397, 1.040834085586084257E-14 ) ) ;
#157578 = CARTESIAN_POINT ( 'NONE',  ( 3.069588487047324915E-15, 0.2401923788623739342, -10.89999999999920277 ) ) ;
#157577 = CARTESIAN_POINT ( 'NONE',  ( 2.466018556964240549, 2.218949015226141963, -0.4410763869808070337 ) ) ;
#157579 = CARTESIAN_POINT ( 'NONE',  ( 5.719784389160836646, -2.055351168476500234, 0.4581721925015455610 ) ) ;
#157580 = CARTESIAN_POINT ( 'NONE',  ( 10.09133975709188213, 13.93637380468759623, 7.385690965161497701 ) ) ;
#157581 = CARTESIAN_POINT ( 'NONE',  ( 2.453653613718423276, 1.598880132357576755, 1.315258840600006085 ) ) ;
#157582 = CARTESIAN_POINT ( 'NONE',  ( 5.040934186182656873, 4.775511393501539636, 1.040834085586084257E-14 ) ) ;
#157583 = CARTESIAN_POINT ( 'NONE',  ( 0.6801582343749847936, 0.5052083336747614783, 1.178068619123803451 ) ) ;
#157584 = CARTESIAN_POINT ( 'NONE',  ( 4.406960118137589255, -0.4655763551070742912, -2.068578822641816473 ) ) ;
#157585 = APPLICATION_PROTOCOL_DEFINITION ( 'draft international standard', 'automotive_design', 1998, #212288 ) ;
#157587 = CARTESIAN_POINT ( 'NONE',  ( 1.400868510093127073, 1.575373640256217733, -1.108617158386180357 ) ) ;
#157586 = CARTESIAN_POINT ( 'NONE',  ( -4.080641047588918546, 4.823464646017586510, -1.082531754730548412 ) ) ;
#157588 = CARTESIAN_POINT ( 'NONE',  ( -3.793249116773374396, 7.647484079536056356, 0.7998128361456352531 ) ) ;
#157589 = CARTESIAN_POINT ( 'NONE',  ( 7.910292558569346433, 11.31609285405122556, -1.199719254218446718 ) ) ;
#157590 = CARTESIAN_POINT ( 'NONE',  ( 4.706088717274885092, 8.504537580213796133, 0.7216878364870317197 ) ) ;
#157591 = CARTESIAN_POINT ( 'NONE',  ( 5.181774431428755712, 6.445567486282277159, 1.182616053296376979 ) ) ;
#157592 = CARTESIAN_POINT ( 'NONE',  ( -3.475000000000000533, -0.3354166657107504612, -2.006292185433948827 ) ) ;
#157593 = CARTESIAN_POINT ( 'NONE',  ( -5.115504031057831469, 4.862509545855891346, 0.7998128361456341429 ) ) ;
#157594 = CARTESIAN_POINT ( 'NONE',  ( -0.08724509969064601911, -2.221098688967707790, -0.04574986941241648841 ) ) ;
#157595 = CARTESIAN_POINT ( 'NONE',  ( 2.678859613419749763, -2.014854250346362008, -0.6126693332187698182 ) ) ;
#157596 = CARTESIAN_POINT ( 'NONE',  ( -5.652823702255029836, 5.559658838911111900, -0.7998128361456362523 ) ) ;
#157597 = CARTESIAN_POINT ( 'NONE',  ( 8.076906825439115423, 10.44614393447756129, -1.599625672291262513 ) ) ;
#157598 = CARTESIAN_POINT ( 'NONE',  ( 6.684420909863875160, 1.071953792136259187, -1.520962823361602601 ) ) ;
#157599 = CARTESIAN_POINT ( 'NONE',  ( 6.238723240582662477, 10.43026088065513513, -0.7998128361456291469 ) ) ;
#157600 = CARTESIAN_POINT ( 'NONE',  ( 11.95360554405587017, 9.995550034974165499, 1.059413164304713773 ) ) ;
#157601 = CARTESIAN_POINT ( 'NONE',  ( -4.065465959251405081, 5.836405933916976707, -1.599625672291271394 ) ) ;
#157602 = CARTESIAN_POINT ( 'NONE',  ( -8.676855123066019360, 11.14608361504227574, -1.443375672974059665 ) ) ;
#157603 = CARTESIAN_POINT ( 'NONE',  ( 0.4047333657465709278, -2.105317319661216047, -0.2534319464195868843 ) ) ;
#157605 = CARTESIAN_POINT ( 'NONE',  ( 3.842202535371820993, -0.9690557767615382012, 1.705768119890891610 ) ) ;
#157604 = CARTESIAN_POINT ( 'NONE',  ( -0.6125000000000037081, -0.2083333333333242665, 1.060881119635920689 ) ) ;
#157606 = CARTESIAN_POINT ( 'NONE',  ( 2.202237438260604030, -2.161223104231101644, 0.05255616829508147347 ) ) ;
#157608 = CARTESIAN_POINT ( 'NONE',  ( -5.639314450680645407, 6.167449467472198243, -0.8320033040390877321 ) ) ;
#157607 = CARTESIAN_POINT ( 'NONE',  ( -3.284818356260900796, 7.054314858938165678, 0.7998128361456352531 ) ) ;
#157609 = CARTESIAN_POINT ( 'NONE',  ( 1.364683531249988535, 1.613541667008084879, 0.7879004041258500513 ) ) ;
#157610 = CARTESIAN_POINT ( 'NONE',  ( 3.028976774107559944, -1.169381637243168903, -1.289075744332576878 ) ) ;
#157611 = CARTESIAN_POINT ( 'NONE',  ( 5.490689023854504747, 9.349628261231513804, 1.040834085586084257E-14 ) ) ;
#157612 = CARTESIAN_POINT ( 'NONE',  ( -11.38502332509229831, 5.468749262791421373, -5.576278951475440948 ) ) ;
#157613 = ORIENTED_EDGE ( 'NONE', *, *, #47233, .F. ) ;
#157614 = CARTESIAN_POINT ( 'NONE',  ( 1.897814322125553010, 0.1948091626960517242, 2.006652841580962132 ) ) ;
#157615 = CARTESIAN_POINT ( 'NONE',  ( 6.825078400183579141, 1.241995729952071637, 2.258014901253778461 ) ) ;
#157616 = CARTESIAN_POINT ( 'NONE',  ( -2.972980823146582186, 6.690504403638126263, 0.000000000000000000 ) ) ;
#157617 = CARTESIAN_POINT ( 'NONE',  ( 2.711746521272298871, -1.950232680175187250, 0.2877518621813393018 ) ) ;
#157619 = CARTESIAN_POINT ( 'NONE',  ( -5.966997003790240228, 6.134120390609613338, -0.7216878364870338292 ) ) ;
#157618 = CARTESIAN_POINT ( 'NONE',  ( 5.572493885891085519, 0.7809320506734825917, 1.745880147543739325 ) ) ;
#157620 = CARTESIAN_POINT ( 'NONE',  ( -4.448483798615272100, 8.203998508444197313, 0.000000000000000000 ) ) ;
#157621 = CARTESIAN_POINT ( 'NONE',  ( 6.038177310039780643, 8.137902509836795417, -1.599625672291283607 ) ) ;
#157622 = CARTESIAN_POINT ( 'NONE',  ( -5.119085517611572378, 8.129960982925583224, 1.199719254218452935 ) ) ;
#157623 = CARTESIAN_POINT ( 'NONE',  ( 2.279949990775688384, 1.980252038983502993, -0.3961774098769352825 ) ) ;
#157624 = CARTESIAN_POINT ( 'NONE',  ( -10.60211293576223213, 11.47147930125185589, 1.040834085586084257E-14 ) ) ;
#157625 = CARTESIAN_POINT ( 'NONE',  ( 5.948310197725324322, 2.304532173486303570, 0.1212388396696506970 ) ) ;
#157626 = CARTESIAN_POINT ( 'NONE',  ( 6.689906388054261299, -1.280585065398877731, -1.486383542710856043 ) ) ;
#157627 = CARTESIAN_POINT ( 'NONE',  ( 2.448037131198562921, -0.8433605282326918084, 1.771390271482737200 ) ) ;
#157628 = CARTESIAN_POINT ( 'NONE',  ( 9.908311333488716954, 10.45411806535867782, 0.7998128361456462443 ) ) ;
#157629 = CARTESIAN_POINT ( 'NONE',  ( 0.8092204703840089053, 1.198858234535697065, -1.621184076614573533 ) ) ;
#157630 = VERTEX_POINT ( 'NONE', #123503 ) ;
#157631 = CARTESIAN_POINT ( 'NONE',  ( 2.852857698155007782, -1.958159313504294730, -0.8059144277542380497 ) ) ;
#157633 = CARTESIAN_POINT ( 'NONE',  ( -7.152089726408780379, 8.302858421353754181, -1.199719254218446718 ) ) ;
#157632 = CARTESIAN_POINT ( 'NONE',  ( -3.273404022695637572, 5.906389562198459231, 1.199719254218462483 ) ) ;
#157634 = CARTESIAN_POINT ( 'NONE',  ( 2.238008233095424515, 0.4029187984595939409, 1.796341404040911804 ) ) ;
#157635 = ORIENTED_EDGE ( 'NONE', *, *, #76553, .T. ) ;
#157636 = CARTESIAN_POINT ( 'NONE',  ( -9.592557376868645846, 11.15007068022363157, -1.199719254218441611 ) ) ;
#157637 = CARTESIAN_POINT ( 'NONE',  ( 10.41968677110260089, 10.52501210740200754, 5.960825342340682731 ) ) ;
#157638 = CARTESIAN_POINT ( 'NONE',  ( 2.795306286867365486, -0.1602278063087131110, -2.114629986603839829 ) ) ;
#157639 = CARTESIAN_POINT ( 'NONE',  ( 0.7437973067255730930, 0.5320827018340993364, 1.762565881533173950 ) ) ;
#157640 = CARTESIAN_POINT ( 'NONE',  ( -1.201851678989727383E-14, 4.618750000682821266, -1.732050807568863648 ) ) ;
#157641 = CARTESIAN_POINT ( 'NONE',  ( 6.238723240582662477, 10.43026088065513513, -0.7998128361456291469 ) ) ;
#157642 = CARTESIAN_POINT ( 'NONE',  ( 6.013923656113508542, 9.173938811177871244, -1.199719254218452047 ) ) ;
#157643 = CARTESIAN_POINT ( 'NONE',  ( 4.182927011504236070, -0.1980092267137799622, -2.051220347156012647 ) ) ;
#157645 = CARTESIAN_POINT ( 'NONE',  ( 1.804012939494209267, 1.363607186100148638, -1.237405090928713092 ) ) ;
#157644 = CARTESIAN_POINT ( 'NONE',  ( -8.877891658850122880, 9.251961778280284321, 0.7998128361456462443 ) ) ;
#157646 = CARTESIAN_POINT ( 'NONE',  ( -1.364683531250012516, 4.488541667008090208, -0.7879004041258300672 ) ) ;
#157647 = CARTESIAN_POINT ( 'NONE',  ( -0.02244404828157658613, 5.719765766439059540, -2.783169749654360814 ) ) ;
#157648 = CARTESIAN_POINT ( 'NONE',  ( -1.506201402929161048, 8.679372656207108960, 2.542017642366253050 ) ) ;
#157649 = CARTESIAN_POINT ( 'NONE',  ( 11.04536101718726293, 13.40000000000000036, 1.099999999999996758 ) ) ;
#157650 = CARTESIAN_POINT ( 'NONE',  ( 1.295869073816724226, 1.673045085319382119, 1.439284050222865652 ) ) ;
#157651 = CARTESIAN_POINT ( 'NONE',  ( 2.776973401877864234, -2.164208356635976216, -0.6592219059844570683 ) ) ;
#157652 = CARTESIAN_POINT ( 'NONE',  ( -7.375272376154077492, 11.54830883891436422, -0.7216878364870267237 ) ) ;
#157653 = CARTESIAN_POINT ( 'NONE',  ( 3.603588835282888869, 1.315886683649561295, 1.245372468285299128 ) ) ;
#157654 = CARTESIAN_POINT ( 'NONE',  ( 3.204202018521628226, 1.211454676919420326, -1.484069150048252350 ) ) ;
#157655 = CARTESIAN_POINT ( 'NONE',  ( 4.650872726564402981, -0.4503784926754761386, -2.020631409805350387 ) ) ;
#157656 = CARTESIAN_POINT ( 'NONE',  ( -1.364683531250012516, 3.301041667008084879, -0.7879004041258289570 ) ) ;
#157657 = EDGE_CURVE ( 'NONE', #147411, #191004, #23757, .T. ) ;
#157658 = CARTESIAN_POINT ( 'NONE',  ( 2.307442625383813617, -0.4335913300187159702, 1.923040929009907973 ) ) ;
#157659 = CARTESIAN_POINT ( 'NONE',  ( 0.6570953225405625764, -1.625623130003026606, -1.033337472089399078 ) ) ;
#157660 = CARTESIAN_POINT ( 'NONE',  ( 3.924554409752772699, 1.776107677202539925, 0.5873546117282567591 ) ) ;
#157661 = CARTESIAN_POINT ( 'NONE',  ( 2.210004991130873453, -0.5033687547432836862, 2.251983625769232500 ) ) ;
#157662 = CARTESIAN_POINT ( 'NONE',  ( 3.560865204049929122, 1.468383728701172064, -1.143307097947023010 ) ) ;
#157663 = CARTESIAN_POINT ( 'NONE',  ( -1.201851678989727383E-14, 4.446875000341417916, -1.575800808251660134 ) ) ;
#157664 = CARTESIAN_POINT ( 'NONE',  ( -5.135841261478327979, 4.886236314679810455, 0.7998128361456341429 ) ) ;
#157665 = CARTESIAN_POINT ( 'NONE',  ( 5.113396490648394632, 9.117379672398465473, 1.040834085586084257E-14 ) ) ;
#157666 = CARTESIAN_POINT ( 'NONE',  ( 3.834746474454188013E-15, 8.843750000682797818, 1.500000000000001554 ) ) ;
#157667 = CARTESIAN_POINT ( 'NONE',  ( 0.9617104568129207776, 0.4090027284681818642, -2.065791855309044411 ) ) ;
#157668 = AXIS2_PLACEMENT_3D ( 'NONE', #84878, #202870, #150966 ) ;
#157670 = DIRECTION ( 'NONE',  ( -0.000000000000000000, -1.000000000000000000, -0.000000000000000000 ) ) ;
#157669 = CARTESIAN_POINT ( 'NONE',  ( -1.201851678989727383E-14, 3.509375000341421469, -1.575800808251660134 ) ) ;
#157671 = CARTESIAN_POINT ( 'NONE',  ( -1.865749732055444365, 8.973930515401084662, -0.7749999999999996891 ) ) ;
#157672 = CARTESIAN_POINT ( 'NONE',  ( 2.408575119285644384, -2.115224228095522907, -0.1514441693673748146 ) ) ;
#157673 = CARTESIAN_POINT ( 'NONE',  ( 6.393224328948585722, -0.1011241736039915490, -2.017280362314947340 ) ) ;
#157674 = CARTESIAN_POINT ( 'NONE',  ( -0.6823417656250003738, 1.467708333674752730, -1.181850606188749264 ) ) ;
#157675 = CARTESIAN_POINT ( 'NONE',  ( -3.118012141462980669, 6.581505231774690046, 0.7216878364870317197 ) ) ;
#157676 = CARTESIAN_POINT ( 'NONE',  ( 4.741601036477289810, 6.554953847355395880, 1.599625672291267398 ) ) ;
#157677 = CARTESIAN_POINT ( 'NONE',  ( 1.019082891775088484, 1.996809913787592095, 0.8282600050937348746 ) ) ;
#157678 = EDGE_CURVE ( 'NONE', #148901, #62943, #136146, .T. ) ;
#157681 = CARTESIAN_POINT ( 'NONE',  ( 3.389175213736297820, 4.977123720824209840, 1.443375672974062551 ) ) ;
#157680 = CARTESIAN_POINT ( 'NONE',  ( -4.083708824282378913, 7.596498746673441715, 0.5977277219625460880 ) ) ;
#157679 = CARTESIAN_POINT ( 'NONE',  ( 5.254667053748194760, 8.288139441751686931, 1.199719254218452047 ) ) ;
#157682 = CARTESIAN_POINT ( 'NONE',  ( -0.08058608058609216529, -8.407420853759283830, -10.99970480893080271 ) ) ;
#157683 = CARTESIAN_POINT ( 'NONE',  ( 5.823453932400854960, -1.463924103857511039, -1.387103351090559711 ) ) ;
#157685 = CARTESIAN_POINT ( 'NONE',  ( -6.577113915960849155, 6.845923454808663600, -0.7216878364870338292 ) ) ;
#157684 = CARTESIAN_POINT ( 'NONE',  ( -8.785320351975364872, 12.23299559640450518, 1.082531754730560403 ) ) ;
#157686 = CARTESIAN_POINT ( 'NONE',  ( 0.000000000000000000, 0.5000000000000004441, 0.000000000000000000 ) ) ;
#157688 = CARTESIAN_POINT ( 'NONE',  ( -1.402160292154681736E-14, 10.17187500034139447, 1.575800808251682339 ) ) ;
#157687 = CARTESIAN_POINT ( 'NONE',  ( 0.09312846265441956928, -0.5046389715205062965, -2.214118724221309620 ) ) ;
#157689 = CARTESIAN_POINT ( 'NONE',  ( -10.13488352141530768, 11.78278451552804817, 1.199719254218462483 ) ) ;
#157691 = CARTESIAN_POINT ( 'NONE',  ( 6.556263154800559434, -1.238474754573845038, 1.591913907798309991 ) ) ;
#157690 = CARTESIAN_POINT ( 'NONE',  ( -6.521108698048791119, 6.710307690586118312, -0.7216878364870267237 ) ) ;
#157692 = CARTESIAN_POINT ( 'NONE',  ( 1.364683531249986537, 0.4260416670080872659, 0.7879004041258500513 ) ) ;
#157693 = B_SPLINE_CURVE_WITH_KNOTS ( 'NONE', 3,
 ( #132068, #129980, #214287, #146170, #51853, #150425 ),
 .UNSPECIFIED., .F., .F.,
 ( 4, 2, 4 ),
 ( 0.001259240562161249421, 0.001573673787268791650, 0.001888107012376333878 ),
 .UNSPECIFIED. ) ;
#157694 = CARTESIAN_POINT ( 'NONE',  ( 0.1376292675369541196, -5.401429653175749301, 10.96107445065239183 ) ) ;
#157695 = DIRECTION ( 'NONE',  ( -1.000000000000000000, 1.016547956922408957E-15, 1.479114432388267300E-31 ) ) ;
#157696 = CARTESIAN_POINT ( 'NONE',  ( 3.211258912624019857, -0.3355696072399985685, 1.691725950409156631 ) ) ;
#157697 = CARTESIAN_POINT ( 'NONE',  ( 5.110497557708379546, 4.926945003606695295, -0.7998128361456481317 ) ) ;
#157698 = CARTESIAN_POINT ( 'NONE',  ( 5.879395890181562834, 6.888325289080478697, -1.199719254218452047 ) ) ;
#157699 = CARTESIAN_POINT ( 'NONE',  ( 0.7195362622018970367, -0.9397137143956849625, -1.499438161327722341 ) ) ;
#157700 = CARTESIAN_POINT ( 'NONE',  ( 1.401040355039730345, -0.2976371227399738917, -1.990864243493442709 ) ) ;
#157701 =( NAMED_UNIT ( * ) PLANE_ANGLE_UNIT ( ) SI_UNIT ( $, .RADIAN. ) );
#157703 = AXIS2_PLACEMENT_3D ( 'NONE', #109818, #113019, #81513 ) ;
#157702 = CARTESIAN_POINT ( 'NONE',  ( 3.997267248050282884, 1.865803599355109421, -1.178106810156675843 ) ) ;
#157704 = ORIENTED_EDGE ( 'NONE', *, *, #91562, .F. ) ;
#157705 = CARTESIAN_POINT ( 'NONE',  ( 9.368320956918616105, 10.03205532593431037, 0.7216878364870458196 ) ) ;
#157707 = CARTESIAN_POINT ( 'NONE',  ( 2.864861414439429321, -0.1511590275467006583, -2.010826137130202529 ) ) ;
#157706 = CARTESIAN_POINT ( 'NONE',  ( 4.283913115580790354, 2.056533504189705930, -0.5163123687341104606 ) ) ;
#157709 = VERTEX_POINT ( 'NONE', #122435 ) ;
#157708 = CARTESIAN_POINT ( 'NONE',  ( 3.796947700133224135, -0.1831754980210500150, -1.802320314001674806 ) ) ;
#157710 = CARTESIAN_POINT ( 'NONE',  ( 6.222266154028957885, 6.224008365980749247, 0.7998128361456352531 ) ) ;
#157711 = VERTEX_POINT ( 'NONE', #188393 ) ;
#157712 = CARTESIAN_POINT ( 'NONE',  ( 0.7603692911175019553, -1.357789551990191246, 1.287012767582619510 ) ) ;
#157713 = CARTESIAN_POINT ( 'NONE',  ( 4.029797971759831121, 5.724516938518342535, -1.599625672291255185 ) ) ;
#157714 = CARTESIAN_POINT ( 'NONE',  ( 6.164658409365947556, -1.287482145768016339, 1.294691480910937775 ) ) ;
#157717 = CARTESIAN_POINT ( 'NONE',  ( 2.413182783470344983, -1.785834301256707723, 0.6938157933340273198 ) ) ;
#157716 = PRESENTATION_LAYER_ASSIGNMENT (  '', '', ( #130111 ) ) ;
#157715 = CARTESIAN_POINT ( 'NONE',  ( -4.627410500965859264, 4.293067094081919777, 0.7998128361456341429 ) ) ;
#157718 = CARTESIAN_POINT ( 'NONE',  ( 4.161989969715248705, 4.726297878971393196, -2.420000000000000373 ) ) ;
#157719 = CARTESIAN_POINT ( 'NONE',  ( -3.922984035321194884, 2.804646012044678560, 0.7750000000000135669 ) ) ;
#157720 = CARTESIAN_POINT ( 'NONE',  ( -0.6823417656250003738, 2.280208333674753174, -1.181850606188749264 ) ) ;
#157721 = SURFACE_STYLE_USAGE ( .BOTH. , #204280 ) ;
#157722 = ORIENTED_EDGE ( 'NONE', *, *, #177164, .F. ) ;
#157723 = CIRCLE ( 'NONE', #188783, 0.08000000000000020983 ) ;
#157724 = CARTESIAN_POINT ( 'NONE',  ( 5.885648082108177803, 9.880690172519326353, 0.7216878364870317197 ) ) ;
#157725 = CARTESIAN_POINT ( 'NONE',  ( -3.512971199716682591, 7.112567143062499930, 0.000000000000000000 ) ) ;
#157726 = CARTESIAN_POINT ( 'NONE',  ( -6.129167961829681488, 9.308390501180058507, -1.199719254218452047 ) ) ;
#157727 = CARTESIAN_POINT ( 'NONE',  ( 3.428091063814618700, -2.088597262255381448, 0.3661859999234198249 ) ) ;
#157729 = CARTESIAN_POINT ( 'NONE',  ( -10.91449010664383223, 5.922815305582411760, 6.336942051301835299 ) ) ;
#157728 = CARTESIAN_POINT ( 'NONE',  ( -0.1296875068448125057, 1.390030859318210688, -2.083197486262199138 ) ) ;
#157730 = CARTESIAN_POINT ( 'NONE',  ( 4.903572647403447782, -0.5284346980384787562, 1.899126047080600621 ) ) ;
#157731 = CARTESIAN_POINT ( 'NONE',  ( 0.2287712656204986261, 1.385237311202421662, -1.461098210751586857 ) ) ;
#157732 = ORIENTED_EDGE ( 'NONE', *, *, #191014, .T. ) ;
#157733 = CARTESIAN_POINT ( 'NONE',  ( 6.350787976822619640, -1.936633936377421206, -0.8562603515115329023 ) ) ;
#157734 = DIRECTION ( 'NONE',  ( 0.000000000000000000, 0.000000000000000000, 1.000000000000000000 ) ) ;
#157735 = CARTESIAN_POINT ( 'NONE',  ( 1.961466609329724164, 1.720096886549182136, 1.151944459977225055 ) ) ;
#157736 = CARTESIAN_POINT ( 'NONE',  ( 3.046748965309022505, -1.587984067068026528, -1.117546226756223726 ) ) ;
#157737 = CARTESIAN_POINT ( 'NONE',  ( 5.692444392891300886, 7.734547439830227411, -1.599625672291281386 ) ) ;
#157738 = CARTESIAN_POINT ( 'NONE',  ( 4.864343252252968597, 8.897093904262280972, 0.000000000000000000 ) ) ;
#157740 = CARTESIAN_POINT ( 'NONE',  ( 5.738125327081736060, 7.717565519727259904, 1.599625672291267398 ) ) ;
#157739 = CARTESIAN_POINT ( 'NONE',  ( 3.433613042289254569, 0.9395709039844526433, -1.867677030932006765 ) ) ;
#157741 = CARTESIAN_POINT ( 'NONE',  ( 4.868786560638896255, 5.813244087901094481, 1.082531754730549078 ) ) ;
#157743 = EDGE_LOOP ( 'NONE', ( #234, #98419, #176118, #107692 ) ) ;
#157742 = CARTESIAN_POINT ( 'NONE',  ( 1.013979471798792886, -1.811656969585205612, -0.0007847632289004204901 ) ) ;
#157744 = CARTESIAN_POINT ( 'NONE',  ( 5.549527019956425278, -1.737703232767298545, -1.360318885177333570 ) ) ;
#157745 = CARTESIAN_POINT ( 'NONE',  ( 3.048090068225879801, 6.453403318663617050, -0.2959858980189428168 ) ) ;
#157746 = CARTESIAN_POINT ( 'NONE',  ( 3.786314268594536347, -1.089870966172037825, 1.918795532666245363 ) ) ;
#157747 = CARTESIAN_POINT ( 'NONE',  ( 6.259060471003163428, 10.45398764947904624, -0.7998128361456291469 ) ) ;
#157748 = CYLINDRICAL_SURFACE ( 'NONE', #27011, 11.00000000000000000 ) ;
#157749 = CARTESIAN_POINT ( 'NONE',  ( 3.053266463924544372, -1.685387242695039811, 0.9035085923766730254 ) ) ;
#157750 = CARTESIAN_POINT ( 'NONE',  ( 9.921869487102386032, 10.46993591124128997, 0.000000000000000000 ) ) ;
#157751 = CARTESIAN_POINT ( 'NONE',  ( 5.336411075974297979, -1.153114810915600641, 1.719314882265559286 ) ) ;
#157753 = CARTESIAN_POINT ( 'NONE',  ( 2.975616057669258741, 2.053088362031017855, -0.6768339029224537118 ) ) ;
#157752 = CARTESIAN_POINT ( 'NONE',  ( 1.566570994388963856, 8.685985410138266971, -2.500753655585654656 ) ) ;
#157754 = CARTESIAN_POINT ( 'NONE',  ( 4.300438532332786501, 1.693616701070689956, -1.390861761948622766 ) ) ;
#157755 = ORIENTED_EDGE ( 'NONE', *, *, #124443, .F. ) ;
#157756 = CARTESIAN_POINT ( 'NONE',  ( -11.86145016429273014, 10.90000000000000036, -1.100000000000002087 ) ) ;
#157757 = DIRECTION ( 'NONE',  ( -5.578564026256490882E-16, -1.000000000000000000, -9.066213480720158442E-32 ) ) ;
#157758 = CARTESIAN_POINT ( 'NONE',  ( 5.032011289327418702, 5.899709921417326974, 1.199719254218452935 ) ) ;
#157759 = CARTESIAN_POINT ( 'NONE',  ( 0.6823417656249934904, 15.25520833367473372, 1.181850606188764807 ) ) ;
#157760 = CARTESIAN_POINT ( 'NONE',  ( -9.178506806771670412, 9.810605484096178941, 1.040834085586084257E-14 ) ) ;
#157761 = CARTESIAN_POINT ( 'NONE',  ( 4.441177836928239309, 7.339068688795062911, 1.199719254218452047 ) ) ;
#157762 = CARTESIAN_POINT ( 'NONE',  ( 6.262565978045822490, -0.7396069823457154246, -1.933831554736538338 ) ) ;
#157763 = CARTESIAN_POINT ( 'NONE',  ( 4.793539397740587127, 1.428753304119126266, 1.292492988728560999 ) ) ;
#157764 = CARTESIAN_POINT ( 'NONE',  ( 0.5621253344089729431, -1.117812357707391069, 1.678020072846800659 ) ) ;
#157765 = CARTESIAN_POINT ( 'NONE',  ( 4.580100504995564314, 8.463430921191662293, -0.5085073561186970181 ) ) ;
#157766 = CARTESIAN_POINT ( 'NONE',  ( 6.505933609711257226, 8.683618192786854095, -1.599625672291281386 ) ) ;
#157767 = CARTESIAN_POINT ( 'NONE',  ( 9.367496997597600128, 3.481540744127370690, 7.500000000000001776 ) ) ;
#157768 = CARTESIAN_POINT ( 'NONE',  ( 4.856285946018928712, -1.968934436971051305, -0.05237921274019693985 ) ) ;
#157769 = B_SPLINE_CURVE_WITH_KNOTS ( 'NONE', 3,
 ( #6681, #107477, #74911, #120533 ),
 .UNSPECIFIED., .F., .F.,
 ( 4, 4 ),
 ( 1.788112030672750545E-18, 0.0006551727224232820924 ),
 .UNSPECIFIED. ) ;
#157770 = CARTESIAN_POINT ( 'NONE',  ( 0.4807640440005828131, -0.2721776580492247799, -2.174417363000572756 ) ) ;
#157771 = CARTESIAN_POINT ( 'NONE',  ( 5.373610676068619973, 1.758448663713826132, -0.4906839848310071139 ) ) ;
#157772 = PRODUCT ( 'rubber for drip tip', 'rubber for drip tip', '', ( #134937 ) ) ;
#157773 = CARTESIAN_POINT ( 'NONE',  ( 4.746763178560241769, 8.551991118380046331, 0.7216878364870328300 ) ) ;
#157774 = CARTESIAN_POINT ( 'NONE',  ( 4.351804119862229037, 4.179452349368450115, -0.7216878364870188411 ) ) ;
#157775 = CARTESIAN_POINT ( 'NONE',  ( -5.550083779947821760, 7.568460058062819407, -1.599625672291271394 ) ) ;
#157776 = CARTESIAN_POINT ( 'NONE',  ( 4.529305835417093640, 7.441884687032027657, -1.199719254218450271 ) ) ;
#157777 = ORIENTED_EDGE ( 'NONE', *, *, #135974, .F. ) ;
#157779 = CARTESIAN_POINT ( 'NONE',  ( -0.1106856583841060310, -0.002128758811529348188, -1.996853503091333470 ) ) ;
#157778 = CARTESIAN_POINT ( 'NONE',  ( 3.016969003575611818, -1.773741936391802332, 0.4936923545346691977 ) ) ;
#157780 = CARTESIAN_POINT ( 'NONE',  ( 1.072081722297711259, 1.739511735661619429, -1.502347287396257114 ) ) ;
#157781 = CARTESIAN_POINT ( 'NONE',  ( 6.244970037249994554, -0.2844439363869250004, -1.940879991452467479 ) ) ;
#157782 = CARTESIAN_POINT ( 'NONE',  ( -4.882907879216086933, 8.848476292394087395, -0.7998128361456281477 ) ) ;
#157783 = CARTESIAN_POINT ( 'NONE',  ( -4.244597871138700462, 7.508646359881505639, -0.8219154050654879917 ) ) ;
#157784 = COLOUR_RGB ( '', 0.72549020, 0.75294118, 0.79215686) ;
#157785 = CARTESIAN_POINT ( 'NONE',  ( -4.783329267523015460, 4.474972321731942593, -0.7998128361456221525 ) ) ;
#157787 = ADVANCED_FACE ( 'NONE', ( #205705 ), #117439, .F. ) ;
#157786 = CARTESIAN_POINT ( 'NONE',  ( 1.777638883463123598, -0.9165151389911446733, 1.199999999999999734 ) ) ;
#157788 = CARTESIAN_POINT ( 'NONE',  ( -4.122561227007127016, 6.967349310553715647, 1.199719254218452935 ) ) ;
#157790 = CARTESIAN_POINT ( 'NONE',  ( 0.7076149179639171782, -1.862046558926268913, 0.1791945732521060819 ) ) ;
#157789 = CARTESIAN_POINT ( 'NONE',  ( 2.226223261843117918, 2.028672367434441792, 0.5052007718874002018 ) ) ;
#157791 = CARTESIAN_POINT ( 'NONE',  ( 1.528672481244568448, 1.986742605292156405, -0.3418812301651391605 ) ) ;
#157792 = ORIENTED_EDGE ( 'NONE', *, *, #54959, .F. ) ;
#157793 = CARTESIAN_POINT ( 'NONE',  ( 1.364683531249988535, 3.717708333674750953, -0.7879004041258239610 ) ) ;
#157794 = CARTESIAN_POINT ( 'NONE',  ( 2.102700294964424454, -0.3804589880251930123, 1.698169956227519872 ) ) ;
#157795 = CARTESIAN_POINT ( 'NONE',  ( 4.462605117192430804, 8.358123070033169455, 1.040834085586084257E-14 ) ) ;
#157797 = CARTESIAN_POINT ( 'NONE',  ( 0.000000000000000000, 3.447199233515649386, 12.00000000000000178 ) ) ;
#157796 = CARTESIAN_POINT ( 'NONE',  ( -15.75000000000000000, 13.40000000000000036, -1.800000000000001155 ) ) ;
#157798 = CARTESIAN_POINT ( 'NONE',  ( 2.596001052779199014, -1.720239769356088688, -0.1272231981628013098 ) ) ;
#157799 = CARTESIAN_POINT ( 'NONE',  ( 2.736070936638954176, 2.175344985778558726, 0.2654339622269741295 ) ) ;
#157800 = CARTESIAN_POINT ( 'NONE',  ( 5.461621781982892720, 0.4335984126433762853, -2.163701019753036192 ) ) ;
#157801 = CARTESIAN_POINT ( 'NONE',  ( -9.409940793360268785, 3.999985931113709814, -6.919963696468023784 ) ) ;
#157802 = CARTESIAN_POINT ( 'NONE',  ( 3.010768451359053355, 0.7272417100659108735, 2.045797318486474836 ) ) ;
#157803 = CARTESIAN_POINT ( 'NONE',  ( 1.383131112650197281, 1.687622997524572677, -0.6969523973551354779 ) ) ;
#157804 = CARTESIAN_POINT ( 'NONE',  ( 3.415340404243884187, -1.954662906411578804, 0.8143554997327147049 ) ) ;
#157805 = CARTESIAN_POINT ( 'NONE',  ( 6.539320575229270460, 2.052047842581938841, 2.303245992296603983 ) ) ;
#157806 = ORIENTED_EDGE ( 'NONE', *, *, #195600, .F. ) ;
#157808 = CARTESIAN_POINT ( 'NONE',  ( -0.6823417656250003738, 1.280208333674752508, -1.181850606188749264 ) ) ;
#157807 = CARTESIAN_POINT ( 'NONE',  ( 3.896227223837216869, -0.7194467914123764407, -2.176594258899899437 ) ) ;
#157809 = CARTESIAN_POINT ( 'NONE',  ( 1.224999999999951017, 0.1458333333333527160, -0.7072540797573078075 ) ) ;
#157810 = CARTESIAN_POINT ( 'NONE',  ( 3.541704441667858472, 5.155074486744371853, -1.599625672291262513 ) ) ;
#157811 = CARTESIAN_POINT ( 'NONE',  ( 5.514381189547274076, -2.221473413594120760, -0.001881066846495804690 ) ) ;
#157812 = CARTESIAN_POINT ( 'NONE',  ( -5.205967797967562483, 8.057084283395347768, 1.082531754730548412 ) ) ;
#157813 = PRESENTATION_LAYER_ASSIGNMENT (  '', '', ( #50633 ) ) ;
#157814 = CARTESIAN_POINT ( 'NONE',  ( 3.009546912553647147, 5.494593250412460606, -1.082531754730543083 ) ) ;
#157815 = CARTESIAN_POINT ( 'NONE',  ( -6.683806541412776525, 7.860491055478785682, -1.082531754730543083 ) ) ;
#157816 = EDGE_CURVE ( 'NONE', #102987, #45840, #207348, .T. ) ;
#157817 = CARTESIAN_POINT ( 'NONE',  ( 3.282482588284323821, 6.843663763058119187, 0.7216878364870257245 ) ) ;
#157819 = ORIENTED_EDGE ( 'NONE', *, *, #199481, .F. ) ;
#157818 = AXIS2_PLACEMENT_3D ( 'NONE', #101317, #167399, #20054 ) ;
#157820 = CARTESIAN_POINT ( 'NONE',  ( 4.377577386359387646, -0.4445010797573499817, -1.966645064109616481 ) ) ;
#157822 = CARTESIAN_POINT ( 'NONE',  ( 2.817292378285217502, -1.792290562959488742, -1.020665671854523060 ) ) ;
#157821 = CARTESIAN_POINT ( 'NONE',  ( 5.289652487626049115, 9.323011668872403845, 0.7998128361456462443 ) ) ;
#157823 = CARTESIAN_POINT ( 'NONE',  ( 6.210516883511641772, 9.403297576475722508, 1.199719254218452047 ) ) ;
#157824 = CARTESIAN_POINT ( 'NONE',  ( 6.393551957296131683, 9.616838495890963401, 1.199719254218452047 ) ) ;
#157825 = CARTESIAN_POINT ( 'NONE',  ( -3.285556943750000514, -2.938541666188710266, -1.896917185911906500 ) ) ;
#157826 = SURFACE_STYLE_FILL_AREA ( #57110 ) ;
#157827 = CARTESIAN_POINT ( 'NONE',  ( 6.070311387754347088, -2.079788119406985825, -0.6908379657195938828 ) ) ;
#157828 = CARTESIAN_POINT ( 'NONE',  ( 3.428361437285933455, -1.528740797599713153, -1.314997250469025936 ) ) ;
#157829 = CARTESIAN_POINT ( 'NONE',  ( 2.841158510722852970, 0.6603703904487292498, -1.718939526767604420 ) ) ;
#157830 = CARTESIAN_POINT ( 'NONE',  ( 7.145310649601935182, 8.294949498412453437, -1.199719254218446718 ) ) ;
#157831 =( NAMED_UNIT ( * ) SI_UNIT ( $, .STERADIAN. ) SOLID_ANGLE_UNIT ( ) );
#157832 = CARTESIAN_POINT ( 'NONE',  ( 6.141596500199405284, -1.324292569296809052, -1.256812384211228428 ) ) ;
#157833 = CARTESIAN_POINT ( 'NONE',  ( -7.413611068574208041, 7.543634422958360730, 0.7998128361456341429 ) ) ;
#157834 = CARTESIAN_POINT ( 'NONE',  ( 0.1931282604852417040, -0.5026490872193057902, -2.214429643963564232 ) ) ;
#157835 = CARTESIAN_POINT ( 'NONE',  ( 2.315183273126443009, 1.881732686034083724, 0.9459776246590365645 ) ) ;
#157836 = CARTESIAN_POINT ( 'NONE',  ( -6.961185525973791144, 7.086080966583015339, 0.7998128361456341429 ) ) ;
#157837 = CARTESIAN_POINT ( 'NONE',  ( 7.914208982075123799, 10.25632978388623684, -1.599625672291262513 ) ) ;
#157838 = CARTESIAN_POINT ( 'NONE',  ( 7.499068361690118145, 7.921536974826172361, -0.7216878364870317197 ) ) ;
#157839 = SURFACE_STYLE_USAGE ( .BOTH. , #189254 ) ;
#157840 = CARTESIAN_POINT ( 'NONE',  ( -6.204827856548512877, 10.39071626594860476, -0.7998128361456291469 ) ) ;
#157841 = CARTESIAN_POINT ( 'NONE',  ( 7.047292192040121250, -5.787795860784306079, 7.664865541495959889 ) ) ;
#157842 = CARTESIAN_POINT ( 'NONE',  ( 7.497295758232718654, 9.769931022736756177, -1.443375672974058777 ) ) ;
#157843 = CARTESIAN_POINT ( 'NONE',  ( 4.093767505759832837, 7.703081727663242617, 0.6588811006658854552 ) ) ;
#157844 = CARTESIAN_POINT ( 'NONE',  ( -5.610376637956639101, 5.439860920571172542, 0.000000000000000000 ) ) ;
#157846 = CARTESIAN_POINT ( 'NONE',  ( 4.060924178622978609, 0.5945426864985210447, 2.140278595106285042 ) ) ;
#157845 = CARTESIAN_POINT ( 'NONE',  ( 2.074623746436579985, 0.9110886696130392481, 1.915067268644244702 ) ) ;
#157847 = CARTESIAN_POINT ( 'NONE',  ( 1.148660753082946240, -1.725648174752218100, 1.350667304935410318 ) ) ;
#157848 = CARTESIAN_POINT ( 'NONE',  ( 0.1709339574563934483, -1.438030690398562239, 1.674123062825278563 ) ) ;
#157849 = CARTESIAN_POINT ( 'NONE',  ( -5.147255595043616516, 6.034161611419515125, 1.199719254218452935 ) ) ;
#157850 = CARTESIAN_POINT ( 'NONE',  ( 5.335297142177534369, 6.183267073083954735, -1.199719254218452047 ) ) ;
#157851 = CARTESIAN_POINT ( 'NONE',  ( 4.387127823891323608, 0.09410986116351567621, 1.959716250186482434 ) ) ;
#157852 = CARTESIAN_POINT ( 'NONE',  ( 10.40318394038753702, 11.03146944007395724, -0.7998128361456281477 ) ) ;
#157853 = CARTESIAN_POINT ( 'NONE',  ( -5.693503466768185639, 6.133329901302775333, 0.7540896269448340572 ) ) ;
#157854 = CARTESIAN_POINT ( 'NONE',  ( -3.930962900855138553, 2.807348321460037432, -0.7749999999999944711 ) ) ;
#157855 = CARTESIAN_POINT ( 'NONE',  ( 1.364683531249986537, 0.1552083336747499542, -0.7879004041258309554 ) ) ;
#157856 = CARTESIAN_POINT ( 'NONE',  ( 6.610000000000011866, 2.967812824040619191, 2.453181572820534395 ) ) ;
#157859 = ORIENTED_EDGE ( 'NONE', *, *, #73531, .T. ) ;
#157858 = CARTESIAN_POINT ( 'NONE',  ( -6.887178846062128379, 7.137389529935019183, -0.7216878364870278340 ) ) ;
#157857 = AXIS2_PLACEMENT_3D ( 'NONE', #32759, #53275, #20747 ) ;
#157860 = CARTESIAN_POINT ( 'NONE',  ( 3.797228045176269440, -0.2112621354826669517, -2.110076569278092062 ) ) ;
#157861 = CARTESIAN_POINT ( 'NONE',  ( -4.821859908315634158, 5.654533310236863564, 1.199719254218452935 ) ) ;
#157862 = CARTESIAN_POINT ( 'NONE',  ( 5.612251347527116963, -0.9680786960581324596, -1.932885698521320528 ) ) ;
#157863 = CARTESIAN_POINT ( 'NONE',  ( 4.001369526190221571, -1.836035423186295201, 0.1395379388276704880 ) ) ;
#157864 = CARTESIAN_POINT ( 'NONE',  ( 5.348842313791752900, -1.825074749614737701, -0.8578464102408298597 ) ) ;
#157865 = CARTESIAN_POINT ( 'NONE',  ( -5.552553451737586521, 6.223206628393089801, 0.9334509375357492589 ) ) ;
#157866 = CARTESIAN_POINT ( 'NONE',  ( -0.6823417656250003738, 2.030208333674753174, -1.181850606188749264 ) ) ;
#157867 = CARTESIAN_POINT ( 'NONE',  ( 0.3798832434597871344, -0.2101876225509922147, -1.727645577085941353 ) ) ;
#157868 = CARTESIAN_POINT ( 'NONE',  ( 11.44779963594995564, 12.69999999999997797, 3.600000000000075140 ) ) ;
#157869 = CARTESIAN_POINT ( 'NONE',  ( 4.555176424511575561, 4.416720038126027426, -0.7216878364870188411 ) ) ;
#157870 = CARTESIAN_POINT ( 'NONE',  ( 11.75830593302511851, 6.921630077720365648, 2.442185041723917927 ) ) ;
#157871 = CIRCLE ( 'NONE', #30304, 2.021340551328831392 ) ;
#157872 = CARTESIAN_POINT ( 'NONE',  ( 3.678741886385179072, -2.082744454470350615, -0.5786317199799119182 ) ) ;
#157873 = CARTESIAN_POINT ( 'NONE',  ( 5.694685421800770087, -1.276849089899323886, -1.560260200769040706 ) ) ;
#157874 = CARTESIAN_POINT ( 'NONE',  ( -9.137832345486311070, 9.763151945929928743, 1.040834085586084257E-14 ) ) ;
#157875 = CARTESIAN_POINT ( 'NONE',  ( 3.485389320157119997, 1.955090977548096687, -0.9225387301767663528 ) ) ;
#157876 = CARTESIAN_POINT ( 'NONE',  ( 3.725814648419359720, -1.171505211990100159, -1.585385422309880887 ) ) ;
#157877 = CARTESIAN_POINT ( 'NONE',  ( -0.1232117409455633916, -0.1621322592461546530, -2.156395338765437764 ) ) ;
#157878 = CARTESIAN_POINT ( 'NONE',  ( 1.624504772527136875, -1.283422126333678692, -1.917570747650028551 ) ) ;
#157879 = CARTESIAN_POINT ( 'NONE',  ( 2.513025655421320170, 1.839406356194466463, 0.9293899518807801075 ) ) ;
#157880 = CARTESIAN_POINT ( 'NONE',  ( 5.319850173407331795, 1.153525655430783337, -1.562239502177962480 ) ) ;
#157883 = ORIENTED_EDGE ( 'NONE', *, *, #69142, .F. ) ;
#157882 = CARTESIAN_POINT ( 'NONE',  ( 7.873959529867758711, -5.295524846228442328, -7.681496476274664253 ) ) ;
#157881 = CARTESIAN_POINT ( 'NONE',  ( -8.636180661780672452, 9.177891648273343250, -0.7216878364870267237 ) ) ;
#157884 = AXIS2_PLACEMENT_3D ( 'NONE', #114453, #195644, #177261 ) ;
#157885 = CARTESIAN_POINT ( 'NONE',  ( -5.824109505522200081, 8.952488968821326054, -1.199719254218452047 ) ) ;
#157886 = CARTESIAN_POINT ( 'NONE',  ( 11.91826848330682154, 10.09270354043018436, 1.400000080589831608 ) ) ;
#157888 = VERTEX_POINT ( 'NONE', #60524 ) ;
#157887 = CARTESIAN_POINT ( 'NONE',  ( -3.332271893908731464, 7.109677319527304640, -0.7998128361456481317 ) ) ;
#157889 = CARTESIAN_POINT ( 'NONE',  ( -6.846504384776750385, 10.93141284897413890, -0.7216878364870267237 ) ) ;
#157890 = CARTESIAN_POINT ( 'NONE',  ( 2.098912041516465266, -0.5885267676426220174, -2.126790307141281033 ) ) ;
#157891 = CARTESIAN_POINT ( 'NONE',  ( 2.520460663003311730, -4.179124451297094645, -2.338645729556988240 ) ) ;
#157892 = CARTESIAN_POINT ( 'NONE',  ( 6.069191303861535935, 1.728486752094375190, 0.9278679456784575397 ) ) ;
#157893 = CARTESIAN_POINT ( 'NONE',  ( -0.1290005225502641184, 1.996213967822700663, -2.587563282167547385 ) ) ;
#157894 = CARTESIAN_POINT ( 'NONE',  ( -1.201851678989727383E-14, 4.868750000682822154, -1.732050807568863648 ) ) ;
#157896 = CARTESIAN_POINT ( 'NONE',  ( 1.500000000000001332, 12.65625000068279427, 0.000000000000000000 ) ) ;
#157895 = CARTESIAN_POINT ( 'NONE',  ( -6.297925439369929101, 6.970297724909739756, -0.9421744322617598977 ) ) ;
#157897 = CARTESIAN_POINT ( 'NONE',  ( 5.490138966579363178, -0.4511402564183407127, -1.784887083484905768 ) ) ;
#157898 = EDGE_LOOP ( 'NONE', ( #84338, #183248, #137379 ) ) ;
#157899 = CARTESIAN_POINT ( 'NONE',  ( 2.395450018592326646, 1.592181132671898869, 1.308497088967359723 ) ) ;
#157900 = CARTESIAN_POINT ( 'NONE',  ( -1.360316468750006669, 0.1614583336747227316, 0.7853790794158981292 ) ) ;
#157901 = CARTESIAN_POINT ( 'NONE',  ( -7.314787569772770226, 8.492672571945082183, -1.199719254218452935 ) ) ;
#157902 = FACE_OUTER_BOUND ( 'NONE', #15337, .T. ) ;
#157903 = CARTESIAN_POINT ( 'NONE',  ( 11.97929049433705551, 11.29999999999999893, 0.7046979865771804130 ) ) ;
#157904 = CARTESIAN_POINT ( 'NONE',  ( 9.451968220918345764, 11.05088267330476448, -7.322606453075928279 ) ) ;
#157905 = CARTESIAN_POINT ( 'NONE',  ( 3.960953433486789521, 7.772862772376584850, -0.7998128361456221525 ) ) ;
#157906 = CARTESIAN_POINT ( 'NONE',  ( 0.4443025167278572551, 2.055347410954794451, 0.1520637142833832778 ) ) ;
#157908 = CARTESIAN_POINT ( 'NONE',  ( 4.405690278861111864, -0.7914791229979671883, -1.662609734262666894 ) ) ;
#157907 = CARTESIAN_POINT ( 'NONE',  ( -10.91970695577495931, -6.134628647623513231, 0.000000000000000000 ) ) ;
#157909 = CARTESIAN_POINT ( 'NONE',  ( 8.294891053462476904, 8.571794405328034827, 1.040834085586084257E-14 ) ) ;
#157910 = CARTESIAN_POINT ( 'NONE',  ( -5.030313335769911021, 7.996221790701172338, -1.198669363888727357 ) ) ;
#157911 = CARTESIAN_POINT ( 'NONE',  ( -5.550083779947821760, 7.568460058062819407, -1.599625672291271394 ) ) ;
#157913 = VERTEX_POINT ( 'NONE', #195867 ) ;
#157912 = CARTESIAN_POINT ( 'NONE',  ( -9.183873789516530550, -7.868711957285995595, 1.138412281109779656E-15 ) ) ;
#157914 = CARTESIAN_POINT ( 'NONE',  ( 4.196070124731249074, -0.8457972711899945928, 2.038567251995755836 ) ) ;
#157915 = CARTESIAN_POINT ( 'NONE',  ( 6.679017863784723730, -0.1010099541198590523, -2.260277599329813647 ) ) ;
#157916 = CARTESIAN_POINT ( 'NONE',  ( -6.263503779833496488, 6.409768619334935913, 0.7216878364870317197 ) ) ;
#157917 = CARTESIAN_POINT ( 'NONE',  ( 0.1758378621803426134, 1.891278220088285833, -0.2826890867150752551 ) ) ;
#157918 = CARTESIAN_POINT ( 'NONE',  ( -0.1706859984542466180, -1.561801110730935971, -1.275320528755889526 ) ) ;
#157919 = CARTESIAN_POINT ( 'NONE',  ( -6.949925879317538246, -6.532648833121172061, 6.447267651612382799 ) ) ;
#157920 = EDGE_CURVE ( 'NONE', #49683, #42393, #145021, .T. ) ;
#157921 = CARTESIAN_POINT ( 'NONE',  ( 7.654042494670951690E-16, -13.99999999999999822, -6.249999999999995559 ) ) ;
#157922 = CARTESIAN_POINT ( 'NONE',  ( 5.883449979803575758, 0.1360998956825946737, -1.907488392096804874 ) ) ;
#157923 = CARTESIAN_POINT ( 'NONE',  ( 0.000000000000000000, 1.750000000000001554, 0.000000000000000000 ) ) ;
#157924 = CARTESIAN_POINT ( 'NONE',  ( 0.3911966820569385828, 1.383097094795827209, 1.259704262696823118 ) ) ;
#157925 = CARTESIAN_POINT ( 'NONE',  ( 2.360564879530482330, -1.931125380751706810, -0.5807522007576990664 ) ) ;
#157926 = EDGE_CURVE ( 'NONE', #401, #149119, #127831, .T. ) ;
#157928 = CARTESIAN_POINT ( 'NONE',  ( 3.897179185067170870, 1.779300596213341690, -1.126466309965125756 ) ) ;
#157927 = CARTESIAN_POINT ( 'NONE',  ( -7.316596452869116973, 11.68777962832266049, 0.7998128361456481317 ) ) ;
#157929 = CARTESIAN_POINT ( 'NONE',  ( 7.096803341749390981, 10.36702210109460154, -1.199719254218441611 ) ) ;
#157931 = CARTESIAN_POINT ( 'NONE',  ( -7.934546212495630968, 10.28005655271014795, -1.599625672291263179 ) ) ;
#157930 = CARTESIAN_POINT ( 'NONE',  ( -0.7500000000000006661, 0.1083333333333560966, -1.299038105676652011 ) ) ;
#157932 = CARTESIAN_POINT ( 'NONE',  ( 11.49978884755362252, 9.857291788371890462, 3.429452816445146546 ) ) ;
#157933 = CARTESIAN_POINT ( 'NONE',  ( 4.271743411778946786, 0.4384756098019436665, -1.971458303354764352 ) ) ;
#157934 = CARTESIAN_POINT ( 'NONE',  ( 0.6823417656249899377, 4.926041667008086655, -1.181850606188754593 ) ) ;
#157935 = CARTESIAN_POINT ( 'NONE',  ( 9.327646496521982300, 11.90534021740758064, -1.443375672974057666 ) ) ;
#157936 = CARTESIAN_POINT ( 'NONE',  ( 4.429101881081805914, 0.1011787780425543737, 2.159334005894457231 ) ) ;
#157937 = CARTESIAN_POINT ( 'NONE',  ( 7.309781096423290769, 8.557108029695882578, 1.199719254218452935 ) ) ;
#157938 = CARTESIAN_POINT ( 'NONE',  ( -0.7500000000000215383, 4.941666666666684193, 1.299038105676671107 ) ) ;
#157940 = SURFACE_SIDE_STYLE ('',( #158991 ) ) ;
#157939 = CARTESIAN_POINT ( 'NONE',  ( 5.006703865196457492, 9.063181286029688977, 0.000000000000000000 ) ) ;
#157941 = CARTESIAN_POINT ( 'NONE',  ( 7.253248993186713456, 11.40594822545244824, 0.7216878364870438212 ) ) ;
#157943 = CARTESIAN_POINT ( 'NONE',  ( -0.3610206255356728233, -7.699789852011537761, 10.99434576732824631 ) ) ;
#157942 = CARTESIAN_POINT ( 'NONE',  ( 2.014367633873125563, 2.165423841567072127, -0.1585431616079237827 ) ) ;
#157945 = CARTESIAN_POINT ( 'NONE',  ( 0.6789530235665336422, 1.236279375446739603, 1.364625092910062953 ) ) ;
#157944 = CARTESIAN_POINT ( 'NONE',  ( -6.724481002698130538, 7.907944593645035880, -1.082531754730544860 ) ) ;
#157946 = CIRCLE ( 'NONE', #182178, 11.89429233241351902 ) ;
#157947 = CARTESIAN_POINT ( 'NONE',  ( 0.6823417656249882723, 1.426041667008083547, -1.181850606188749264 ) ) ;
#157948 = CARTESIAN_POINT ( 'NONE',  ( 2.841561854484982774, 0.7863008361240211297, -2.045831095052422555 ) ) ;
#157949 = CARTESIAN_POINT ( 'NONE',  ( 6.483881968795301098, 6.767627347268279969, 0.2992266196225811803 ) ) ;
#157950 = CARTESIAN_POINT ( 'NONE',  ( 3.801889278938491934, -0.6593813483589389124, 2.164292034026161549 ) ) ;
#157951 = CARTESIAN_POINT ( 'NONE',  ( -7.019370843573183194, 9.212351955633947043, 1.599625672291283607 ) ) ;
#157952 = CARTESIAN_POINT ( 'NONE',  ( 1.364683531249990311, 5.426041667008086655, 0.7879004041258500513 ) ) ;
#157953 = CARTESIAN_POINT ( 'NONE',  ( 6.266472554743693912, 6.895788939045927712, 0.7740814723603481884 ) ) ;
#157954 = CARTESIAN_POINT ( 'NONE',  ( 0.7500000000000006661, 12.08333333333333570, 1.299038105676657340 ) ) ;
#157955 = CARTESIAN_POINT ( 'NONE',  ( 6.916067756746836714, 8.201738816693689316, -1.082531754730548412 ) ) ;
#157956 = CARTESIAN_POINT ( 'NONE',  ( 4.235448325177215700, -1.219352424245947253, -1.282881785660697771 ) ) ;
#157957 = CARTESIAN_POINT ( 'NONE',  ( 9.368847842243145152, 10.88907622316056312, 1.199719254218453823 ) ) ;
#157958 = CARTESIAN_POINT ( 'NONE',  ( 0.8859290024384089968, 1.414438444053778055, 1.560449103131421156 ) ) ;
#157961 = EDGE_CURVE ( 'NONE', #11879, #142064, #59463, .T. ) ;
#157960 = CARTESIAN_POINT ( 'NONE',  ( -0.7500000000000006661, 1.858333333333357595, -1.299038105676652011 ) ) ;
#157959 = CARTESIAN_POINT ( 'NONE',  ( 1.364683531250000303, 10.50520833367473195, -0.7879004041258355073 ) ) ;
#157962 = CARTESIAN_POINT ( 'NONE',  ( 0.8363043462186695587, -1.097040784323728424, 1.635518954194992824 ) ) ;
#157963 = CARTESIAN_POINT ( 'NONE',  ( -4.502189528189771472, 7.410248995266807803, -1.199719254218453823 ) ) ;
#157964 = CARTESIAN_POINT ( 'NONE',  ( 6.292592244351721043, 1.492246071875057645, -1.356311808412967723 ) ) ;
#157965 = ORIENTED_EDGE ( 'NONE', *, *, #10566, .F. ) ;
#157966 = CARTESIAN_POINT ( 'NONE',  ( 7.131225611108096274, 8.382479970123348778, 1.082531754730558626 ) ) ;
#157967 = CARTESIAN_POINT ( 'NONE',  ( 8.910733272679570049, 11.41894145625809820, -1.599625672291255185 ) ) ;
#157969 = CARTESIAN_POINT ( 'NONE',  ( 4.258574955689950592, -1.386304660245713860, 1.256184814050688603 ) ) ;
#157968 = CIRCLE ( 'NONE', #78474, 6.277139874739035008 ) ;
#157970 = CARTESIAN_POINT ( 'NONE',  ( 4.575093719746353038, 1.890691655113156289, 0.8438020912069632562 ) ) ;
#157971 = CARTESIAN_POINT ( 'NONE',  ( 0.6124999999999862776, 2.333333333333325932, 1.060881119635898040 ) ) ;
#157972 =( BOUNDED_SURFACE ( )  B_SPLINE_SURFACE ( 3, 2, ( 
 ( #2666, #131687, #197689 ),
 ( #17854, #200868, #52512 ),
 ( #36247, #115453, #205140 ),
 ( #203006, #138046, #74106 ),
 ( #57847, #120794, #186771 ),
 ( #107741, #140199, #124008 ),
 ( #23186, #38398, #156429 ),
 ( #206220, #54646, #189975 ) ),
 .UNSPECIFIED., .F., .F., .T. ) 
 B_SPLINE_SURFACE_WITH_KNOTS ( ( 4, 2, 2, 4 ),
 ( 3, 3 ),
 ( 0.000000000000000000, 0.0002204160392919288941, 0.0004408320785838577881, 0.0008816641571677155762 ),
 ( 0.000000000000000000, 1.000000000000000000 ),
 .UNSPECIFIED. ) 
 GEOMETRIC_REPRESENTATION_ITEM ( )  RATIONAL_B_SPLINE_SURFACE ( (
 ( 1.000000000000000000, 0.4127341956165084258, 1.000000000000000000),
 ( 1.000000000000000000, 0.4103180386332804241, 1.000000000000000000),
 ( 1.000000000000000000, 0.4223234233956687511, 1.000000000000000000),
 ( 1.000000000000000000, 0.4613847219400475375, 1.000000000000000000),
 ( 1.000000000000000000, 0.4878744032656874285, 1.000000000000000000),
 ( 1.000000000000000000, 0.5702658980232629959, 1.000000000000000000),
 ( 1.000000000000000000, 0.6280001242511515924, 1.000000000000000000),
 ( 1.000000000000000000, 0.6787756258918324903, 1.000000000000000000) ) ) 
 REPRESENTATION_ITEM ( '' )  SURFACE ( )  );
#157973 = CARTESIAN_POINT ( 'NONE',  ( -6.753369912938502750, 7.051555451282599307, 0.000000000000000000 ) ) ;
#157974 = CARTESIAN_POINT ( 'NONE',  ( 2.539911556248050761, -0.9198678134644189264, -2.162407946988131435 ) ) ;
#157975 = MECHANICAL_DESIGN_GEOMETRIC_PRESENTATION_REPRESENTATION (  '', ( #23105 ), #213280 ) ;
#157976 = CARTESIAN_POINT ( 'NONE',  ( 7.242026607993941489, 11.60078147596829901, 0.7998128361456462443 ) ) ;
#157977 = CARTESIAN_POINT ( 'NONE',  ( -8.618179199781044630, 13.20629283305325963, 0.7998128361456341429 ) ) ;
#157978 = CARTESIAN_POINT ( 'NONE',  ( 0.000000000000000000, 4.000007913748540922, 0.000000000000000000 ) ) ;
#157979 = ADVANCED_FACE ( 'NONE', ( #208893 ), #127767, .F. ) ;
#157980 = CARTESIAN_POINT ( 'NONE',  ( -0.02968770228140016343, 0.003472272166151618711, -1.826291111852257343 ) ) ;
#157981 = CARTESIAN_POINT ( 'NONE',  ( -0.6823417656249969321, 5.280208333674756283, -1.181850606188749264 ) ) ;
#157982 = CARTESIAN_POINT ( 'NONE',  ( 3.947668504265917644, 1.419370528949075005, 1.354593381527373186 ) ) ;
#157983 = CARTESIAN_POINT ( 'NONE',  ( 2.337267334706777611, -1.242538083881424615, 1.587593183769491656 ) ) ;
#157984 = CARTESIAN_POINT ( 'NONE',  ( -3.902768115887413014, 5.646591783325653147, -1.599625672291283607 ) ) ;
#157985 = CARTESIAN_POINT ( 'NONE',  ( 7.462104991928526054, -5.166862915010159263, 8.081892667527535323 ) ) ;
#157986 = CARTESIAN_POINT ( 'NONE',  ( 1.018573325691285003, 1.726041315240328444, 0.7214104187760682629 ) ) ;
#157987 = CARTESIAN_POINT ( 'NONE',  ( 1.364683531249988535, 4.155208333674753618, -0.7879004041258239610 ) ) ;
#157988 = CARTESIAN_POINT ( 'NONE',  ( 3.199479786217104493, 1.818179288054132536, -0.8647478076822049387 ) ) ;
#157990 = CARTESIAN_POINT ( 'NONE',  ( 3.814152603263697650, 1.130891212129871093, -1.789721717560237790 ) ) ;
#157989 = CARTESIAN_POINT ( 'NONE',  ( -6.073689629242160493, 8.109057205581079231, -1.443375672974059665 ) ) ;
#157991 = CARTESIAN_POINT ( 'NONE',  ( 6.825078400183551608, 4.689370880799383912, 2.706890346843467299 ) ) ;
#157992 = CARTESIAN_POINT ( 'NONE',  ( 5.389151899530504330, 0.1487064154041470299, 2.065066873896327593 ) ) ;
#157993 = CARTESIAN_POINT ( 'NONE',  ( 5.110497557708379546, 4.926945003606695295, -0.7998128361456481317 ) ) ;
#157995 = CARTESIAN_POINT ( 'NONE',  ( 6.720655732516672920, 1.239197277384354035, 2.287559680360019332 ) ) ;
#157994 = CARTESIAN_POINT ( 'NONE',  ( -0.1291982275798781443, -0.004298614154785855221, -2.073875112923003083 ) ) ;
#157997 = EDGE_LOOP ( 'NONE', ( #115676, #29904, #164897, #97688, #103019 ) ) ;
#157996 = CARTESIAN_POINT ( 'NONE',  ( 5.438443955714742373, 1.798867289239113987, 0.3102399082220568816 ) ) ;
#157998 = CARTESIAN_POINT ( 'NONE',  ( 8.158255747121103241, 10.54105100977322174, 1.599625672291281386 ) ) ;
#157999 = CARTESIAN_POINT ( 'NONE',  ( 6.539320575229296217, -0.001643797937642094186, 2.203502507913539077 ) ) ;
#158000 = CARTESIAN_POINT ( 'NONE',  ( -11.86145017031048177, 13.50581953513855105, 1.099999999999996980 ) ) ;
#158001 = CARTESIAN_POINT ( 'NONE',  ( -10.12531724201500616, 3.239403609407997653, 5.873437370650227862 ) ) ;
#158002 = CARTESIAN_POINT ( 'NONE',  ( 0.6823417656249934904, 11.75520833367473017, 1.181850606188764807 ) ) ;
#158003 = CARTESIAN_POINT ( 'NONE',  ( 6.533860241792342372, -1.853627334332415888, 0.4695604596292660138 ) ) ;
#158005 = CARTESIAN_POINT ( 'NONE',  ( -9.643927338022246332, 10.14567007064778004, -0.7998128361456291469 ) ) ;
#158004 = CIRCLE ( 'NONE', #50833, 0.8300000000000008482 ) ;
#158006 = CARTESIAN_POINT ( 'NONE',  ( 5.469824908109481854, 8.468880595181346393, -1.199719254218446718 ) ) ;
#158007 = CARTESIAN_POINT ( 'NONE',  ( -11.87815913191725947, 11.30307820631414550, -1.708869976696590465 ) ) ;
#158008 = DIRECTION ( 'NONE',  ( -1.000000000000000000, 1.014813233446432150E-15, 1.972152263052529514E-31 ) ) ;
#158009 = CARTESIAN_POINT ( 'NONE',  ( 3.310162060030825248, 7.013606170011280838, -0.7998128361456291469 ) ) ;
#158010 = VERTEX_POINT ( 'NONE', #177491 ) ;
#158011 = AXIS2_PLACEMENT_3D ( 'NONE', #56102, #203383, #186083 ) ;
#158012 = CARTESIAN_POINT ( 'NONE',  ( -5.413448473606448985, 9.537716662508005427, 0.000000000000000000 ) ) ;
#158013 = CARTESIAN_POINT ( 'NONE',  ( 5.308220328704632784, 1.198845711980157214, -1.621194722098241003 ) ) ;
#158014 = DIRECTION ( 'NONE',  ( 0.000000000000000000, 0.000000000000000000, -1.000000000000000000 ) ) ;
#158015 =( NAMED_UNIT ( * ) SI_UNIT ( $, .STERADIAN. ) SOLID_ANGLE_UNIT ( ) );
#158016 = CARTESIAN_POINT ( 'NONE',  ( -6.488192154978348114, 6.766396236290696642, 0.1981293719705672085 ) ) ;
#158017 = CARTESIAN_POINT ( 'NONE',  ( -5.097502569058215194, 6.970172302033127210, -1.443375672974053447 ) ) ;
#158018 = CARTESIAN_POINT ( 'NONE',  ( 4.090809663021327758, 5.795697244990093644, 1.599625672291267398 ) ) ;
#158019 = CARTESIAN_POINT ( 'NONE',  ( 2.940244962816233265, -1.016462931258435010, 1.686739332702111405 ) ) ;
#158020 = CARTESIAN_POINT ( 'NONE',  ( 3.708611378246814638, 1.915606880664010747, 0.6298579873919087913 ) ) ;
#158021 = CARTESIAN_POINT ( 'NONE',  ( -7.049349804101573191, 10.31165964050546258, -1.199719254218440723 ) ) ;
#158022 = CARTESIAN_POINT ( 'NONE',  ( 6.727182134110234024, 0.5746707207614526469, 2.142055518182262475 ) ) ;
#158023 = CARTESIAN_POINT ( 'NONE',  ( 4.189532503254236318, -0.8396404696654431454, 2.024412170900617092 ) ) ;
#158024 = CARTESIAN_POINT ( 'NONE',  ( 2.116120358982703120, -0.9062717621706478655, -1.699889088518308222 ) ) ;
#158025 = CARTESIAN_POINT ( 'NONE',  ( -8.833300774503376473, 10.26427131079744193, 1.199719254218462483 ) ) ;
#158026 = DIRECTION ( 'NONE',  ( 1.561251128379126077E-17, 1.301042606982605475E-17, 1.000000000000000000 ) ) ;
#158027 = CARTESIAN_POINT ( 'NONE',  ( 0.2331563151865486128, 1.372759770070256291, -2.202161770551560149 ) ) ;
#158028 = DIRECTION ( 'NONE',  ( -3.497202527569253358E-15, 0.000000000000000000, -1.000000000000000000 ) ) ;
#158029 = CARTESIAN_POINT ( 'NONE',  ( 6.435316467980822353, 10.65961964595298817, 1.040834085586084257E-14 ) ) ;
#158030 = CARTESIAN_POINT ( 'NONE',  ( 4.527533231959700366, 7.369540306339926516, 1.199719254218462483 ) ) ;
#158031 = DIRECTION ( 'NONE',  ( -1.000000000000000000, 0.000000000000000000, 0.000000000000000000 ) ) ;
#158032 = CARTESIAN_POINT ( 'NONE',  ( 5.804299160426222848, 7.865044668620976509, -1.443375672974078761 ) ) ;
#158033 = ORIENTED_EDGE ( 'NONE', *, *, #115854, .T. ) ;
#158035 = CARTESIAN_POINT ( 'NONE',  ( 2.824860481609407614, 1.456601328488495106, -1.389772560336500318 ) ) ;
#158034 = CARTESIAN_POINT ( 'NONE',  ( 6.146043377905669125, 0.5841948715668408010, 1.746183665442810007 ) ) ;
#158036 = CARTESIAN_POINT ( 'NONE',  ( 4.569826555773855326, 1.780639694173843823, -1.453273832002010213 ) ) ;
#158038 = CARTESIAN_POINT ( 'NONE',  ( 2.658860470891976302, 1.497794124733292431, -1.104231377384189861 ) ) ;
#158037 = CARTESIAN_POINT ( 'NONE',  ( -0.02919842301646497981, 5.720960850909259321, -2.667883601355185430 ) ) ;
#158039 = CARTESIAN_POINT ( 'NONE',  ( -3.285556943750000514, -0.8385416661887076240, -1.896917185911906500 ) ) ;
#158040 = CARTESIAN_POINT ( 'NONE',  ( 0.000000000000000000, 2.000000000000001776, 0.000000000000000000 ) ) ;
#158041 = CARTESIAN_POINT ( 'NONE',  ( 1.359357947053562156E-15, 18.91999999999999815, -11.09999999999999964 ) ) ;
#158042 = CARTESIAN_POINT ( 'NONE',  ( -8.128276786592724790, 9.441743324901704426, -1.199719254218446718 ) ) ;
#158043 = ADVANCED_FACE ( 'NONE', ( #45367 ), #97318, .T. ) ;
#158044 = CARTESIAN_POINT ( 'NONE',  ( -4.828112100242291760, 6.726159765073026264, -1.443375672974066548 ) ) ;
#158045 = CARTESIAN_POINT ( 'NONE',  ( 6.409723817861421757, -0.9859548438324974295, -1.843685114342674458 ) ) ;
#158046 = CARTESIAN_POINT ( 'NONE',  ( 7.131225611108100715, 7.422110755822004968, 0.7216878364870317197 ) ) ;
#158047 = VERTEX_POINT ( 'NONE', #94129 ) ;
#158048 = CARTESIAN_POINT ( 'NONE',  ( 1.772826578343093873, 3.949999999999995293, 0.3999999999999819811 ) ) ;
#158049 = CARTESIAN_POINT ( 'NONE',  ( -1.420000000000001039, 6.280000000000042881, -2.579999999999995630 ) ) ;
#158050 = CARTESIAN_POINT ( 'NONE',  ( 6.357991264096761519, 1.719682601729131566, -0.1347253291539267650 ) ) ;
#158051 = CARTESIAN_POINT ( 'NONE',  ( -5.220052836461385404, 6.048815383081766583, -1.199719254218446718 ) ) ;
#158052 =( BOUNDED_SURFACE ( )  B_SPLINE_SURFACE ( 1, 2, ( 
 ( #38544, #57989, #203149, #104621, #170669, #22256, #88366, #152294, #6010, #136053, #73150, #72080, #171736, #138191, #204201, #23333, #89442, #155494, #139255, #205287, #56925, #123098, #189055, #40692, #106795, #184769, #74250, #140344, #172823, #90507, #156572, #160829, #145690, #158696, #59050, #178154, #93717, #177079, #111073, #92654, #190113, #108944, #127350, #159758, #28695, #61191, #10294, #11355, #79571, #41767, #76368, #157640, #107880, #29768, #144619, #193319, #210633, #173906, #60119, #62259, #142475, #125208, #208483, #27617, #126278, #211688, #124152, #75309, #192236, #12421, #9237, #209547, #44965, #25482, #91588, #141425, #43898, #77436, #207431, #191170, #95853, #42837, #143553, #174964, #26546, #128420, #94781, #110012, #78501, #176025, #194387, #161909, #46030, #112151, #13497, #212758, #164040, #409, #17733, #67548, #16679, #181330, #63324, #131574, #147786, #64393, #130537, #100086, #179219, #199696, #18810, #196528, #30844, #117466, #115339, #14552, #129485, #82764, #83822, #84897, #167224, #48171, #101136, #133692, #35065, #198627, #80648, #148837, #114284, #180281, #150984, #50274, #195467, #97981, #149915, #15615, #116393, #31904, #51341, #34011, #47098, #49220, #182381, #81705, #213802, #146740, #65425, #113214, #197575, #32958, #99033, #165088, #96922, #162972, #66481, #132621, #166147, #1483, #183459, #24147, #39352, #40438, #122840, #53464, #106539, #103288, #105448, #37215, #188801, #134746, #3613, #89191, #172564, #119601, #168287, #85968, #185585, #72904, #104362, #54535, #70752, #200755, #90250, #169350, #187724, #19884, #171484, #6824, #69691, #20935, #135795, #4678, #87031, #152043, #154177, #203954, #136864, #68623, #102218, #5745, #153103, #202890, #2548, #52404, #118531, #201819, #56676, #23075, #120682, #155242, #186659, #184514, #139008, #36135, #38285, #170407, #21996, #88106, #71822, #137932, #55601, #121756, #205030, #44436, #96393, #45503, #210095, #32432, #114807, #180806, #77977, #213291, #113754, #161380, #47643, #29239, #64917, #130017, #140083, #156317, #61734, #111619, #62786, #126821, #177631, #79041, #46564, #31375, #94261, #95331, #162444, #179758, #163506, #112684, #128949, #7900, #12964, #145156, #160300, #11903, #196008, #57740, #81180, #73988, #144100, #192778, #131066, #211162, #110553, #206107, #178694, #97451, #176555, #48692, #127902, #197054, #15090, #28165, #80106, #193853, #30308, #194927, #14019, #146210, #212228, #63861, #147259, #52937, #199163, #19358, #83292, #168822, #69162, #186128, #84374, #85438, #149377, #960, #115869, #67026, #82232, #165628, #17216, #68092, #133162, #148323, #54012, #50808, #120151, #116935, #136342, #182935, #98498, #135282, #202362, #4160, #34551, #164562, #100622, #201296, #166697, #70230, #16147, #99564, #185054, #214322, #18288, #49742, #181854, #150462, #20426, #200236, #2023, #134226, #65954, #132103, #51886 ),
 ( #151523, #3091, #33491, #198112, #35612, #118009, #183998, #119073, #101690, #167759, #36679, #102767, #86508, #152573, #207721, #206651, #174194, #24697, #74537, #59345, #72376, #187202, #91878, #7372, #90800, #156864, #6302, #103835, #22554, #40983, #73450, #8450, #189343, #138476, #139553, #125498, #169883, #204498, #71297, #21473, #157934, #58283, #107094, #124439, #87582, #188267, #190397, #56148, #38830, #122309, #155787, #39907, #37762, #153654, #203428, #106017, #140638, #137409, #123378, #173116, #5222, #55083, #121232, #172038, #205580, #104914, #170955, #9527, #88660, #57217, #154720, #23631, #42054, #108167, #89738, #25766, #75600, #141711, #31129, #27913, #13779, #179508, #210912, #147019, #62539, #192527, #191461, #175251, #45249, #64671, #97203, #163256, #26837, #92940, #12706, #28985, #14838, #128701, #178443, #63613, #127643, #79854, #113500, #158985, #177371, #145963, #94009, #44181, #142770, #194670, #161119, #211973, #195751, #80928, #112430, #111367, #43127, #160048, #110301, #11652, #77724, #143846, #10581, #209839, #208775, #129768, #76655, #46314, #78783, #61477, #213041, #109241, #47388, #60405, #30050, #126566, #176309, #193607, #95071, #144904, #96140, #162192, #117759, #99319, #196807, #115613, #133979, #166439, #183749, #67832, #165369, #100369, #86254, #48450, #83043, #164311, #114564, #184799, #151267, #199987, #2839, #180556, #66763, #68908, #149117, #65704, #16962, #34296, #132904, #152324, #130817, #81984, #198909, #167507, #15901, #1776, #51635, #32178, #3902, #98254, #50554, #18030, #148072, #214078, #36428, #131852, #84117, #197860, #49492, #135028, #35359, #181608, #19105, #33236, #182675, #102504, #698, #85183, #118814, #150204, #116676, #101434, #201041, #52684, #168567, #20167, #157674, #124186, #190149, #119891, #185868, #105746, #122046, #58022, #7113, #56960, #156608, #6044, #106831, #206396, #37503, #55889, #24432, #186945, #137155, #21220, #73186, #39638, #90544, #74283, #41803, #205322, #138224, #69972, #38578, #203180, #120977, #104653, #170701, #53759, #22286, #87325, #172861, #103579, #139292, #171772, #88399, #4963, #169637, #123134, #23369, #154466, #189091, #71041, #72115, #54827, #153392, #136083, #204237, #188010, #89478, #155533, #40725, #91623, #202100, #8198, #140377, #107916, #173942, #25515, #12458, #59085, #96956, #125245, #11390, #44997, #191205, #108978, #129517, #10326, #111107, #174997, #42870, #95887, #128452, #26582, #112183, #179254, #61225, #63359, #60152, #46061, #211722, #28728, #30877, #94814, #76400, #9271, #207466, #77468, #75343, #195497, #47133, #92684, #158730, #177112, #127381, #113248, #160864, #210666, #161942, #159788, #178187, #145723, #142509, #209580, #29802, #126309, #208517, #192269, #78533, #193353, #13534, #79604, #141459, #144651, #143587, #43930, #110045, #176057, #27653, #93750, #62293, #194420, #115373, #114314, #51381 ) ),
 .UNSPECIFIED., .F., .F., .T. ) 
 B_SPLINE_SURFACE_WITH_KNOTS ( ( 2, 2 ),
 ( 3, 2, 2, 2, 2, 2, 2, 2, 2, 2, 2, 2, 2, 2, 2, 2, 2, 2, 2, 2, 2, 2, 2, 2, 2, 2, 2, 2, 2, 2, 2, 2, 2, 2, 2, 2, 2, 2, 2, 2, 2, 2, 2, 2, 2, 2, 2, 2, 2, 2, 2, 2, 2, 2, 2, 2, 2, 2, 2, 2, 2, 2, 2, 2, 2, 2, 2, 2, 2, 2, 2, 2, 2, 2, 2, 2, 2, 2, 2, 2, 2, 2, 2, 2, 2, 2, 2, 2, 2, 2, 2, 2, 2, 2, 2, 2, 2, 2, 2, 2, 2, 2, 2, 2, 2, 2, 2, 2, 2, 2, 2, 2, 2, 2, 2, 2, 2, 2, 2, 2, 2, 2, 2, 2, 2, 2, 2, 2, 2, 2, 2, 2, 2, 2, 2, 2, 2, 2, 2, 2, 2, 2, 2, 2, 2, 2, 2, 2, 2, 2, 2, 2, 2, 2, 2, 2, 2, 2, 2, 2, 2, 2, 2, 2, 2, 2, 2, 2, 3 ),
 ( 0.000000000000000000, 1.000000000000000000 ),
 ( 0.000000000000000000, 0.005952380952380952051, 0.01190476190476190410, 0.01785714285714285615, 0.02380952380952380820, 0.02976190476190476025, 0.03571428571428571230, 0.04166666666666666435, 0.04761904761904761640, 0.05357142857142856845, 0.05952380952380952051, 0.06547619047619047949, 0.07142857142857142461, 0.07738095238095238360, 0.08333333333333332871, 0.08928571428571428770, 0.09523809523809523281, 0.1011904761904761918, 0.1071428571428571369, 0.1130952380952380959, 0.1190476190476190410, 0.1250000000000000000, 0.1309523809523809590, 0.1369047619047619180, 0.1428571428571428492, 0.1488095238095238082, 0.1547619047619047672, 0.1607142857142857262, 0.1666666666666666574, 0.1726190476190476164, 0.1785714285714285754, 0.1845238095238095344, 0.1904761904761904656, 0.1964285714285714246, 0.2023809523809523836, 0.2083333333333333426, 0.2142857142857142738, 0.2202380952380952328, 0.2261904761904761918, 0.2321428571428571508, 0.2380952380952380820, 0.2440476190476190410, 0.2500000000000000000, 0.2559523809523809312, 0.2619047619047619180, 0.2678571428571428492, 0.2738095238095238360, 0.2797619047619047672, 0.2857142857142856984, 0.2916666666666666852, 0.2976190476190476164, 0.3035714285714285476, 0.3095238095238095344, 0.3154761904761904656, 0.3214285714285714524, 0.3273809523809523836, 0.3333333333333333148, 0.3392857142857143016, 0.3452380952380952328, 0.3511904761904761640, 0.3571428571428571508, 0.3630952380952380820, 0.3690476190476190688, 0.3750000000000000000, 0.3809523809523809312, 0.3869047619047619180, 0.3928571428571428492, 0.3988095238095238360, 0.4047619047619047672, 0.4107142857142856984, 0.4166666666666666852, 0.4226190476190476164, 0.4285714285714285476, 0.4345238095238095344, 0.4404761904761904656, 0.4464285714285714524, 0.4523809523809523836, 0.4583333333333333148, 0.4642857142857143016, 0.4702380952380952328, 0.4761904761904761640, 0.4821428571428571508, 0.4880952380952380820, 0.4940476190476190688, 0.5000000000000000000, 0.5059523809523809312, 0.5119047619047618625, 0.5178571428571429047, 0.5238095238095238360, 0.5297619047619047672, 0.5357142857142856984, 0.5416666666666666297, 0.5476190476190476719, 0.5535714285714286031, 0.5595238095238095344, 0.5654761904761904656, 0.5714285714285713969, 0.5773809523809523281, 0.5833333333333333703, 0.5892857142857143016, 0.5952380952380952328, 0.6011904761904761640, 0.6071428571428570953, 0.6130952380952381375, 0.6190476190476190688, 0.6250000000000000000, 0.6309523809523809312, 0.6369047619047618625, 0.6428571428571429047, 0.6488095238095238360, 0.6547619047619047672, 0.6607142857142856984, 0.6666666666666666297, 0.6726190476190476719, 0.6785714285714286031, 0.6845238095238095344, 0.6904761904761904656, 0.6964285714285713969, 0.7023809523809523281, 0.7083333333333333703, 0.7142857142857143016, 0.7202380952380952328, 0.7261904761904761640, 0.7321428571428570953, 0.7380952380952381375, 0.7440476190476190688, 0.7500000000000000000, 0.7559523809523809312, 0.7619047619047618625, 0.7678571428571429047, 0.7738095238095238360, 0.7797619047619047672, 0.7857142857142856984, 0.7916666666666666297, 0.7976190476190476719, 0.8035714285714286031, 0.8095238095238095344, 0.8154761904761904656, 0.8214285714285713969, 0.8273809523809523281, 0.8333333333333333703, 0.8392857142857143016, 0.8452380952380952328, 0.8511904761904761640, 0.8571428571428570953, 0.8630952380952381375, 0.8690476190476190688, 0.8750000000000000000, 0.8809523809523809312, 0.8869047619047618625, 0.8928571428571429047, 0.8988095238095238360, 0.9047619047619047672, 0.9107142857142856984, 0.9166666666666666297, 0.9226190476190476719, 0.9285714285714286031, 0.9345238095238095344, 0.9404761904761904656, 0.9464285714285713969, 0.9523809523809523281, 0.9583333333333333703, 0.9642857142857143016, 0.9702380952380952328, 0.9761904761904761640, 0.9821428571428570953, 0.9880952380952381375, 0.9940476190476190688, 1.000000000000000000 ),
 .UNSPECIFIED. ) 
 GEOMETRIC_REPRESENTATION_ITEM ( )  RATIONAL_B_SPLINE_SURFACE ( (
 ( 1.000000000000000000, 0.8660254037844387076, 1.000000000000000000, 0.8660254037844387076, 1.000000000000000000, 0.8660254037844387076, 1.000000000000000000, 0.8660254037844387076, 1.000000000000000000, 0.8660254037844387076, 1.000000000000000000, 0.8660254037844387076, 1.000000000000000000, 0.8660254037844387076, 1.000000000000000000, 0.8660254037844387076, 1.000000000000000000, 0.8660254037844387076, 1.000000000000000000, 0.8660254037844387076, 1.000000000000000000, 0.8660254037844387076, 1.000000000000000000, 0.8660254037844387076, 1.000000000000000000, 0.8660254037844387076, 1.000000000000000000, 0.8660254037844387076, 1.000000000000000000, 0.8660254037844387076, 1.000000000000000000, 0.8660254037844387076, 1.000000000000000000, 0.8660254037844387076, 1.000000000000000000, 0.8660254037844387076, 1.000000000000000000, 0.8660254037844387076, 1.000000000000000000, 0.8660254037844387076, 1.000000000000000000, 0.8660254037844387076, 1.000000000000000000, 0.8660254037844387076, 1.000000000000000000, 0.8660254037844387076, 1.000000000000000000, 0.8660254037844387076, 1.000000000000000000, 0.8660254037844387076, 1.000000000000000000, 0.8660254037844387076, 1.000000000000000000, 0.8660254037844387076, 1.000000000000000000, 0.8660254037844387076, 1.000000000000000000, 0.8660254037844387076, 1.000000000000000000, 0.8660254037844387076, 1.000000000000000000, 0.8660254037844387076, 1.000000000000000000, 0.8660254037844387076, 1.000000000000000000, 0.8660254037844387076, 1.000000000000000000, 0.8660254037844387076, 1.000000000000000000, 0.8660254037844387076, 1.000000000000000000, 0.8660254037844387076, 1.000000000000000000, 0.8660254037844387076, 1.000000000000000000, 0.8660254037844387076, 1.000000000000000000, 0.8660254037844387076, 1.000000000000000000, 0.8660254037844387076, 1.000000000000000000, 0.8660254037844387076, 1.000000000000000000, 0.8660254037844387076, 1.000000000000000000, 0.8660254037844387076, 1.000000000000000000, 0.8660254037844387076, 1.000000000000000000, 0.8660254037844387076, 1.000000000000000000, 0.8660254037844387076, 1.000000000000000000, 0.8660254037844387076, 1.000000000000000000, 0.8660254037844387076, 1.000000000000000000, 0.8660254037844387076, 1.000000000000000000, 0.8660254037844387076, 1.000000000000000000, 0.8660254037844387076, 1.000000000000000000, 0.8660254037844387076, 1.000000000000000000, 0.8660254037844387076, 1.000000000000000000, 0.8660254037844387076, 1.000000000000000000, 0.8660254037844387076, 1.000000000000000000, 0.8660254037844387076, 1.000000000000000000, 0.8660254037844387076, 1.000000000000000000, 0.8660254037844387076, 1.000000000000000000, 0.8660254037844387076, 1.000000000000000000, 0.8660254037844387076, 1.000000000000000000, 0.8660254037844387076, 1.000000000000000000, 0.8660254037844387076, 1.000000000000000000, 0.8660254037844387076, 1.000000000000000000, 0.8660254037844387076, 1.000000000000000000, 0.8660254037844387076, 1.000000000000000000, 0.8660254037844387076, 1.000000000000000000, 0.8660254037844387076, 1.000000000000000000, 0.8660254037844387076, 1.000000000000000000, 0.8660254037844387076, 1.000000000000000000, 0.8660254037844387076, 1.000000000000000000, 0.8660254037844387076, 1.000000000000000000, 0.8660254037844387076, 1.000000000000000000, 0.8660254037844387076, 1.000000000000000000, 0.8660254037844387076, 1.000000000000000000, 0.8660254037844387076, 1.000000000000000000, 0.8660254037844387076, 1.000000000000000000, 0.8660254037844387076, 1.000000000000000000, 0.8660254037844387076, 1.000000000000000000, 0.8660254037844387076, 1.000000000000000000, 0.8660254037844387076, 1.000000000000000000, 0.8660254037844387076, 1.000000000000000000, 0.8660254037844387076, 1.000000000000000000, 0.8660254037844387076, 1.000000000000000000, 0.8660254037844387076, 1.000000000000000000, 0.8660254037844387076, 1.000000000000000000, 0.8660254037844387076, 1.000000000000000000, 0.8660254037844387076, 1.000000000000000000, 0.8660254037844387076, 1.000000000000000000, 0.8660254037844387076, 1.000000000000000000, 0.8660254037844387076, 1.000000000000000000, 0.8660254037844387076, 1.000000000000000000, 0.8660254037844387076, 1.000000000000000000, 0.8660254037844387076, 1.000000000000000000, 0.8660254037844387076, 1.000000000000000000, 0.8660254037844387076, 1.000000000000000000, 0.8660254037844387076, 1.000000000000000000, 0.8660254037844387076, 1.000000000000000000, 0.8660254037844387076, 1.000000000000000000, 0.8660254037844387076, 1.000000000000000000, 0.8660254037844387076, 1.000000000000000000, 0.8660254037844387076, 1.000000000000000000, 0.8660254037844387076, 1.000000000000000000, 0.8660254037844387076, 1.000000000000000000, 0.8660254037844387076, 1.000000000000000000, 0.8660254037844387076, 1.000000000000000000, 0.8660254037844387076, 1.000000000000000000, 0.8660254037844387076, 1.000000000000000000, 0.8660254037844387076, 1.000000000000000000, 0.8660254037844387076, 1.000000000000000000, 0.8660254037844387076, 1.000000000000000000, 0.8660254037844387076, 1.000000000000000000, 0.8660254037844387076, 1.000000000000000000, 0.8660254037844387076, 1.000000000000000000, 0.8660254037844387076, 1.000000000000000000, 0.8660254037844387076, 1.000000000000000000, 0.8660254037844387076, 1.000000000000000000, 0.8660254037844387076, 1.000000000000000000, 0.8660254037844387076, 1.000000000000000000, 0.8660254037844387076, 1.000000000000000000, 0.8660254037844387076, 1.000000000000000000, 0.8660254037844387076, 1.000000000000000000, 0.8660254037844387076, 1.000000000000000000, 0.8660254037844387076, 1.000000000000000000, 0.8660254037844387076, 1.000000000000000000, 0.8660254037844387076, 1.000000000000000000, 0.8660254037844387076, 1.000000000000000000, 0.8660254037844387076, 1.000000000000000000, 0.8660254037844387076, 1.000000000000000000, 0.8660254037844387076, 1.000000000000000000, 0.8660254037844387076, 1.000000000000000000, 0.8660254037844387076, 1.000000000000000000, 0.8660254037844387076, 1.000000000000000000, 0.8660254037844387076, 1.000000000000000000, 0.8660254037844387076, 1.000000000000000000, 0.8660254037844387076, 1.000000000000000000, 0.8660254037844387076, 1.000000000000000000, 0.8660254037844387076, 1.000000000000000000, 0.8660254037844387076, 1.000000000000000000, 0.8660254037844387076, 1.000000000000000000, 0.8660254037844387076, 1.000000000000000000, 0.8660254037844387076, 1.000000000000000000, 0.8660254037844387076, 1.000000000000000000, 0.8660254037844387076, 1.000000000000000000, 0.8660254037844387076, 1.000000000000000000, 0.8660254037844387076, 1.000000000000000000, 0.8660254037844387076, 1.000000000000000000, 0.8660254037844387076, 1.000000000000000000, 0.8660254037844387076, 1.000000000000000000, 0.8660254037844387076, 1.000000000000000000, 0.8660254037844387076, 1.000000000000000000, 0.8660254037844387076, 1.000000000000000000, 0.8660254037844387076, 1.000000000000000000, 0.8660254037844387076, 1.000000000000000000, 0.8660254037844387076, 1.000000000000000000, 0.8660254037844387076, 1.000000000000000000, 0.8660254037844387076, 1.000000000000000000, 0.8660254037844387076, 1.000000000000000000, 0.8660254037844387076, 1.000000000000000000, 0.8660254037844387076, 1.000000000000000000, 0.8660254037844387076, 1.000000000000000000, 0.8660254037844387076, 1.000000000000000000, 0.8660254037844387076, 1.000000000000000000, 0.8660254037844387076, 1.000000000000000000, 0.8660254037844387076, 1.000000000000000000, 0.8660254037844387076, 1.000000000000000000, 0.8660254037844387076, 1.000000000000000000, 0.8660254037844387076, 1.000000000000000000, 0.8660254037844387076, 1.000000000000000000),
 ( 1.000000000000000000, 0.8660254037844387076, 1.000000000000000000, 0.8660254037844387076, 1.000000000000000000, 0.8660254037844387076, 1.000000000000000000, 0.8660254037844387076, 1.000000000000000000, 0.8660254037844387076, 1.000000000000000000, 0.8660254037844387076, 1.000000000000000000, 0.8660254037844387076, 1.000000000000000000, 0.8660254037844387076, 1.000000000000000000, 0.8660254037844387076, 1.000000000000000000, 0.8660254037844387076, 1.000000000000000000, 0.8660254037844387076, 1.000000000000000000, 0.8660254037844387076, 1.000000000000000000, 0.8660254037844387076, 1.000000000000000000, 0.8660254037844387076, 1.000000000000000000, 0.8660254037844387076, 1.000000000000000000, 0.8660254037844387076, 1.000000000000000000, 0.8660254037844387076, 1.000000000000000000, 0.8660254037844387076, 1.000000000000000000, 0.8660254037844387076, 1.000000000000000000, 0.8660254037844387076, 1.000000000000000000, 0.8660254037844387076, 1.000000000000000000, 0.8660254037844387076, 1.000000000000000000, 0.8660254037844387076, 1.000000000000000000, 0.8660254037844387076, 1.000000000000000000, 0.8660254037844387076, 1.000000000000000000, 0.8660254037844387076, 1.000000000000000000, 0.8660254037844387076, 1.000000000000000000, 0.8660254037844387076, 1.000000000000000000, 0.8660254037844387076, 1.000000000000000000, 0.8660254037844387076, 1.000000000000000000, 0.8660254037844387076, 1.000000000000000000, 0.8660254037844387076, 1.000000000000000000, 0.8660254037844387076, 1.000000000000000000, 0.8660254037844387076, 1.000000000000000000, 0.8660254037844387076, 1.000000000000000000, 0.8660254037844387076, 1.000000000000000000, 0.8660254037844387076, 1.000000000000000000, 0.8660254037844387076, 1.000000000000000000, 0.8660254037844387076, 1.000000000000000000, 0.8660254037844387076, 1.000000000000000000, 0.8660254037844387076, 1.000000000000000000, 0.8660254037844387076, 1.000000000000000000, 0.8660254037844387076, 1.000000000000000000, 0.8660254037844387076, 1.000000000000000000, 0.8660254037844387076, 1.000000000000000000, 0.8660254037844387076, 1.000000000000000000, 0.8660254037844387076, 1.000000000000000000, 0.8660254037844387076, 1.000000000000000000, 0.8660254037844387076, 1.000000000000000000, 0.8660254037844387076, 1.000000000000000000, 0.8660254037844387076, 1.000000000000000000, 0.8660254037844387076, 1.000000000000000000, 0.8660254037844387076, 1.000000000000000000, 0.8660254037844387076, 1.000000000000000000, 0.8660254037844387076, 1.000000000000000000, 0.8660254037844387076, 1.000000000000000000, 0.8660254037844387076, 1.000000000000000000, 0.8660254037844387076, 1.000000000000000000, 0.8660254037844387076, 1.000000000000000000, 0.8660254037844387076, 1.000000000000000000, 0.8660254037844387076, 1.000000000000000000, 0.8660254037844387076, 1.000000000000000000, 0.8660254037844387076, 1.000000000000000000, 0.8660254037844387076, 1.000000000000000000, 0.8660254037844387076, 1.000000000000000000, 0.8660254037844387076, 1.000000000000000000, 0.8660254037844387076, 1.000000000000000000, 0.8660254037844387076, 1.000000000000000000, 0.8660254037844387076, 1.000000000000000000, 0.8660254037844387076, 1.000000000000000000, 0.8660254037844387076, 1.000000000000000000, 0.8660254037844387076, 1.000000000000000000, 0.8660254037844387076, 1.000000000000000000, 0.8660254037844387076, 1.000000000000000000, 0.8660254037844387076, 1.000000000000000000, 0.8660254037844387076, 1.000000000000000000, 0.8660254037844387076, 1.000000000000000000, 0.8660254037844387076, 1.000000000000000000, 0.8660254037844387076, 1.000000000000000000, 0.8660254037844387076, 1.000000000000000000, 0.8660254037844387076, 1.000000000000000000, 0.8660254037844387076, 1.000000000000000000, 0.8660254037844387076, 1.000000000000000000, 0.8660254037844387076, 1.000000000000000000, 0.8660254037844387076, 1.000000000000000000, 0.8660254037844387076, 1.000000000000000000, 0.8660254037844387076, 1.000000000000000000, 0.8660254037844387076, 1.000000000000000000, 0.8660254037844387076, 1.000000000000000000, 0.8660254037844387076, 1.000000000000000000, 0.8660254037844387076, 1.000000000000000000, 0.8660254037844387076, 1.000000000000000000, 0.8660254037844387076, 1.000000000000000000, 0.8660254037844387076, 1.000000000000000000, 0.8660254037844387076, 1.000000000000000000, 0.8660254037844387076, 1.000000000000000000, 0.8660254037844387076, 1.000000000000000000, 0.8660254037844387076, 1.000000000000000000, 0.8660254037844387076, 1.000000000000000000, 0.8660254037844387076, 1.000000000000000000, 0.8660254037844387076, 1.000000000000000000, 0.8660254037844387076, 1.000000000000000000, 0.8660254037844387076, 1.000000000000000000, 0.8660254037844387076, 1.000000000000000000, 0.8660254037844387076, 1.000000000000000000, 0.8660254037844387076, 1.000000000000000000, 0.8660254037844387076, 1.000000000000000000, 0.8660254037844387076, 1.000000000000000000, 0.8660254037844387076, 1.000000000000000000, 0.8660254037844387076, 1.000000000000000000, 0.8660254037844387076, 1.000000000000000000, 0.8660254037844387076, 1.000000000000000000, 0.8660254037844387076, 1.000000000000000000, 0.8660254037844387076, 1.000000000000000000, 0.8660254037844387076, 1.000000000000000000, 0.8660254037844387076, 1.000000000000000000, 0.8660254037844387076, 1.000000000000000000, 0.8660254037844387076, 1.000000000000000000, 0.8660254037844387076, 1.000000000000000000, 0.8660254037844387076, 1.000000000000000000, 0.8660254037844387076, 1.000000000000000000, 0.8660254037844387076, 1.000000000000000000, 0.8660254037844387076, 1.000000000000000000, 0.8660254037844387076, 1.000000000000000000, 0.8660254037844387076, 1.000000000000000000, 0.8660254037844387076, 1.000000000000000000, 0.8660254037844387076, 1.000000000000000000, 0.8660254037844387076, 1.000000000000000000, 0.8660254037844387076, 1.000000000000000000, 0.8660254037844387076, 1.000000000000000000, 0.8660254037844387076, 1.000000000000000000, 0.8660254037844387076, 1.000000000000000000, 0.8660254037844387076, 1.000000000000000000, 0.8660254037844387076, 1.000000000000000000, 0.8660254037844387076, 1.000000000000000000, 0.8660254037844387076, 1.000000000000000000, 0.8660254037844387076, 1.000000000000000000, 0.8660254037844387076, 1.000000000000000000, 0.8660254037844387076, 1.000000000000000000, 0.8660254037844387076, 1.000000000000000000, 0.8660254037844387076, 1.000000000000000000, 0.8660254037844387076, 1.000000000000000000, 0.8660254037844387076, 1.000000000000000000, 0.8660254037844387076, 1.000000000000000000, 0.8660254037844387076, 1.000000000000000000, 0.8660254037844387076, 1.000000000000000000, 0.8660254037844387076, 1.000000000000000000, 0.8660254037844387076, 1.000000000000000000, 0.8660254037844387076, 1.000000000000000000, 0.8660254037844387076, 1.000000000000000000, 0.8660254037844387076, 1.000000000000000000, 0.8660254037844387076, 1.000000000000000000, 0.8660254037844387076, 1.000000000000000000, 0.8660254037844387076, 1.000000000000000000, 0.8660254037844387076, 1.000000000000000000, 0.8660254037844387076, 1.000000000000000000, 0.8660254037844387076, 1.000000000000000000, 0.8660254037844387076, 1.000000000000000000, 0.8660254037844387076, 1.000000000000000000, 0.8660254037844387076, 1.000000000000000000, 0.8660254037844387076, 1.000000000000000000, 0.8660254037844387076, 1.000000000000000000, 0.8660254037844387076, 1.000000000000000000, 0.8660254037844387076, 1.000000000000000000, 0.8660254037844387076, 1.000000000000000000, 0.8660254037844387076, 1.000000000000000000, 0.8660254037844387076, 1.000000000000000000, 0.8660254037844387076, 1.000000000000000000) ) ) 
 REPRESENTATION_ITEM ( '' )  SURFACE ( )  );
#158053 = CARTESIAN_POINT ( 'NONE',  ( 1.406441466896314996, -0.9629721463089849776, -1.441941353469172293 ) ) ;
#158054 =( NAMED_UNIT ( * ) SI_UNIT ( $, .STERADIAN. ) SOLID_ANGLE_UNIT ( ) );
#158055 = PLANE ( 'NONE',  #29331 ) ;
#158056 = DIRECTION ( 'NONE',  ( -1.000000000000000000, 0.000000000000000000, 1.465138070926357285E-17 ) ) ;
#158057 = CARTESIAN_POINT ( 'NONE',  ( 5.787976215063657115, -1.371286462501415837, -1.683233787797025371 ) ) ;
#158058 = CARTESIAN_POINT ( 'NONE',  ( 4.178209475066913647, -1.049361115903378883, 1.493786327181771068 ) ) ;
#158059 = CARTESIAN_POINT ( 'NONE',  ( 2.711707638535421960, 0.5279276851305572116, -1.889291386287835550 ) ) ;
#158060 = CARTESIAN_POINT ( 'NONE',  ( 0.000000000000000000, -0.5000000000000004441, 3.599999999999999201 ) ) ;
#158061 = CARTESIAN_POINT ( 'NONE',  ( -9.398826802771548472, 11.98838390803207865, -1.599625672291263179 ) ) ;
#158062 = CARTESIAN_POINT ( 'NONE',  ( 6.591235234537977661, 10.84152487360300299, 0.7998128361456462443 ) ) ;
#158063 = CARTESIAN_POINT ( 'NONE',  ( 3.475340844119988226, -1.870931441966826148, -0.9980012987173056960 ) ) ;
#158064 = CARTESIAN_POINT ( 'NONE',  ( -4.284013352238274841, 4.100363120473813794, -0.7216878364870207285 ) ) ;
#158065 =( NAMED_UNIT ( * ) SI_UNIT ( $, .STERADIAN. ) SOLID_ANGLE_UNIT ( ) );
#158066 = CARTESIAN_POINT ( 'NONE',  ( -5.320367241134011493, 6.379272830146158313, -1.120692317505559643 ) ) ;
#158067 = CARTESIAN_POINT ( 'NONE',  ( 0.9189038144036645317, -1.502058968113138437, 1.424965263859011122 ) ) ;
#158069 = CARTESIAN_POINT ( 'NONE',  ( 1.499999999999997113, 14.67708333401612997, -0.8660254037844378194 ) ) ;
#158068 = CARTESIAN_POINT ( 'NONE',  ( -10.47316218909242025, 3.890729455492532018, 5.858813772850529844 ) ) ;
#158071 = EDGE_LOOP ( 'NONE', ( #68412, #155569, #31742, #58520 ) ) ;
#158070 = CARTESIAN_POINT ( 'NONE',  ( 3.493049024619375054, -2.141166226970441233, -0.5910787634417090652 ) ) ;
#158072 = CARTESIAN_POINT ( 'NONE',  ( 0.7218034001665899480, 2.265987065647384835, 0.3856900369042133292 ) ) ;
#158074 = CARTESIAN_POINT ( 'NONE',  ( 6.895384927792009400, -1.844987169530726723, 0.9222207602926129066 ) ) ;
#158073 = CARTESIAN_POINT ( 'NONE',  ( 3.708318708537623021, 4.285125567170706695, -1.199719254218446718 ) ) ;
#158076 = CARTESIAN_POINT ( 'NONE',  ( -3.285556943750000514, -3.638541666188706891, -1.896917185911906500 ) ) ;
#158075 = CARTESIAN_POINT ( 'NONE',  ( 3.393283585170187688, 7.180857625999046867, 0.7998128361456271485 ) ) ;
#158077 = DIRECTION ( 'NONE',  ( 3.330669073875478989E-16, -3.540251991789410786E-16, -1.000000000000000000 ) ) ;
#158078 = CARTESIAN_POINT ( 'NONE',  ( 3.511198596259283544, 6.271927390929313617, 2.420000000000010587 ) ) ;
#158079 = DIRECTION ( 'NONE',  ( -0.000000000000000000, 1.000000000000000000, -0.000000000000000000 ) ) ;
#158080 = EDGE_CURVE ( 'NONE', #110706, #10766, #113618, .T. ) ;
#158081 = CARTESIAN_POINT ( 'NONE',  ( -0.2102771530458094895, 1.993718876163485421, -2.617492801249762913 ) ) ;
#158082 = CARTESIAN_POINT ( 'NONE',  ( 2.801416971846592219, -0.5432927088015163664, 1.637025921142007956 ) ) ;
#158083 = CARTESIAN_POINT ( 'NONE',  ( 1.165250339122084533, 1.861343190080061660, -0.7762330495894868010 ) ) ;
#158084 = CARTESIAN_POINT ( 'NONE',  ( 3.972163192483857408, 1.252710246566196783, 1.883753103390993777 ) ) ;
#158085 = CARTESIAN_POINT ( 'NONE',  ( 4.776057437618447921, 1.212020014983648863, 1.722159047642721541 ) ) ;
#158086 = CARTESIAN_POINT ( 'NONE',  ( -6.373741612200205076, 8.529394195690610303, 1.443375672974064550 ) ) ;
#158087 = CARTESIAN_POINT ( 'NONE',  ( 3.672906134817868651, 0.04599029964666952880, -1.769319831623831663 ) ) ;
#158088 = AXIS2_PLACEMENT_3D ( 'NONE', #206563, #87754, #127555 ) ;
#158090 = CARTESIAN_POINT ( 'NONE',  ( 6.444901331192640193, -1.838261776244881185, -1.369441068571846554 ) ) ;
#158089 = CARTESIAN_POINT ( 'NONE',  ( 3.675669042636310557, 6.342012078834061484, -1.082531754730549967 ) ) ;
#158091 = CARTESIAN_POINT ( 'NONE',  ( 5.771403949166884040, 1.100151190403714452, 1.476150860297696932 ) ) ;
#158092 = CARTESIAN_POINT ( 'NONE',  ( -3.100010679019018500, 6.768429558830820980, 1.040834085586084257E-14 ) ) ;
#158093 = CARTESIAN_POINT ( 'NONE',  ( 5.056828107772846082, 6.922718763866881453, -1.443375672974051449 ) ) ;
#158094 = CARTESIAN_POINT ( 'NONE',  ( -1.500000000000011324, 3.920833333333357817, 0.8660254037844403729 ) ) ;
#158095 = CARTESIAN_POINT ( 'NONE',  ( 5.033237522093748417, -1.548190877955179179, -1.551241237171486098 ) ) ;
#158096 = CARTESIAN_POINT ( 'NONE',  ( 0.000000000000000000, 13.49999999999999822, 0.000000000000000000 ) ) ;
#158097 = DIRECTION ( 'NONE',  ( -0.000000000000000000, -1.000000000000000000, -0.000000000000000000 ) ) ;
#158098 = CARTESIAN_POINT ( 'NONE',  ( 5.406714943436663035, 0.5975561702324573288, 1.982271326387271770 ) ) ;
#158099 = CARTESIAN_POINT ( 'NONE',  ( 0.09298292169932984019, 1.756857073293972116, 0.9896806593640145033 ) ) ;
#158100 = CARTESIAN_POINT ( 'NONE',  ( 1.364683531249988535, 4.363541667008090208, 0.7879004041258500513 ) ) ;
#158101 = CARTESIAN_POINT ( 'NONE',  ( 2.824735624865559735, 1.814154213653540237, 0.6486305857245775464 ) ) ;
#158102 = CARTESIAN_POINT ( 'NONE',  ( -1.364683531250014514, 10.08854166700806410, -0.7879004041258335089 ) ) ;
#158103 = CARTESIAN_POINT ( 'NONE',  ( -2.480778921620681921, 5.838066475291996404, 1.040834085586084257E-14 ) ) ;
#158104 = CARTESIAN_POINT ( 'NONE',  ( 6.539320575229233157, 0.001224430076711413356, 2.103502572931112091 ) ) ;
#158105 = ORIENTED_EDGE ( 'NONE', *, *, #62155, .F. ) ;
#158107 = CARTESIAN_POINT ( 'NONE',  ( 4.689424523294686509, 8.358602041046323095, -0.7454045323363467368 ) ) ;
#158106 = CARTESIAN_POINT ( 'NONE',  ( -3.851925040058337579, 6.547644075826416277, -1.082531754730546636 ) ) ;
#158108 = CARTESIAN_POINT ( 'NONE',  ( 3.520313441042647540, 7.258782781191745137, 0.7998128361456321445 ) ) ;
#158109 = CARTESIAN_POINT ( 'NONE',  ( -10.98546401119367566, 9.842594370796488690, 1.592223900679732518 ) ) ;
#158110 = DIRECTION ( 'NONE',  ( -5.578564026256490882E-16, -1.000000000000000000, -9.066213480720158442E-32 ) ) ;
#158111 = CARTESIAN_POINT ( 'NONE',  ( 8.717529583462633624, 13.11427558077437894, 0.7216878364870438212 ) ) ;
#158112 = CARTESIAN_POINT ( 'NONE',  ( 1.767943819387544968, -1.947426213878332035, 0.2369139692007388165 ) ) ;
#158113 = CARTESIAN_POINT ( 'NONE',  ( -1.364683531250014514, 1.301041667008083325, -0.7879004041258289570 ) ) ;
#158114 = DIRECTION ( 'NONE',  ( 0.5000000000000041078, 0.000000000000000000, 0.8660254037844363761 ) ) ;
#158115 = CARTESIAN_POINT ( 'NONE',  ( 5.705508943770692731, -1.545575431542939970, -1.208212526538715137 ) ) ;
#158116 = CARTESIAN_POINT ( 'NONE',  ( -8.158255747121117452, 10.54105100977322174, 1.599625672291295375 ) ) ;
#158117 = CARTESIAN_POINT ( 'NONE',  ( -5.300874872818844175, 7.207439989753867238, 1.443375672974064550 ) ) ;
#158118 = AXIS2_PLACEMENT_3D ( 'NONE', #130927, #99435, #197979 ) ;
#158119 = CARTESIAN_POINT ( 'NONE',  ( 6.631704542599726082, -1.407888343591977121, -1.640466528430361670 ) ) ;
#158121 = ORIENTED_EDGE ( 'NONE', *, *, #41574, .F. ) ;
#158120 = CARTESIAN_POINT ( 'NONE',  ( -8.832353407160665526, 3.956598013261175772, -7.432338980325321920 ) ) ;
#158122 = CARTESIAN_POINT ( 'NONE',  ( 1.499999999999985123, -1.172916665983846363, -0.8660254037844323793 ) ) ;
#158123 = CARTESIAN_POINT ( 'NONE',  ( 0.2978465640060874997, -1.869987984933557890, -0.05268733258671080832 ) ) ;
#158124 = CARTESIAN_POINT ( 'NONE',  ( 6.520799197568460492, 1.728869810328565793, -0.1316537485448170952 ) ) ;
#158126 = CARTESIAN_POINT ( 'NONE',  ( 3.368858348882136422, 0.05182064297618373117, -2.191103300807801801 ) ) ;
#158125 = CARTESIAN_POINT ( 'NONE',  ( -5.758872628492444169E-14, 0.4531250003414521998, 1.570758158831760287 ) ) ;
#158127 = CARTESIAN_POINT ( 'NONE',  ( 4.313705703444643547, -0.3987071732099633503, 2.272742389722400169 ) ) ;
#158128 = CARTESIAN_POINT ( 'NONE',  ( 6.749297902460969389, -1.652236475679531580, -1.231405567270830170 ) ) ;
#158129 = CARTESIAN_POINT ( 'NONE',  ( 1.886567394283003907, 1.689560458097194795, -0.9572515956587694941 ) ) ;
#158130 = CARTESIAN_POINT ( 'NONE',  ( -3.755245360860919757, 7.324943987738961049, -0.7216878364870257245 ) ) ;
#158131 = CARTESIAN_POINT ( 'NONE',  ( 11.78331023100045627, 11.29999999999998117, 1.799999999999999600 ) ) ;
#158132 = CARTESIAN_POINT ( 'NONE',  ( 4.799148092389167175, -0.2621723519393297508, -2.104289960152181393 ) ) ;
#158133 = CARTESIAN_POINT ( 'NONE',  ( -1.360316468750002450, 0.4114583336747319464, 0.7853790794158961308 ) ) ;
#158134 = CARTESIAN_POINT ( 'NONE',  ( 3.111954093273407107, 0.05229746705895028935, 2.015912966248374349 ) ) ;
#158135 = CARTESIAN_POINT ( 'NONE',  ( -4.975479186090865369, 6.827811688571220117, 1.443375672974064550 ) ) ;
#158136 = CARTESIAN_POINT ( 'NONE',  ( -7.095713291905736853, 9.371694488680407886, 1.599625672291269396 ) ) ;
#158137 = CARTESIAN_POINT ( 'NONE',  ( 9.236128959407556849, 11.79856975744075598, -1.599625672291262513 ) ) ;
#158138 = CARTESIAN_POINT ( 'NONE',  ( 1.523764310407935030, -1.012771255265769943, -1.518815351243132383 ) ) ;
#158139 = CARTESIAN_POINT ( 'NONE',  ( -6.123442655227560927, 7.173046514967467147, 1.199719254218452047 ) ) ;
#158140 = CARTESIAN_POINT ( 'NONE',  ( -5.601338601481473667, 5.735503837863156207, 0.2797457239998907275 ) ) ;
#158141 = CARTESIAN_POINT ( 'NONE',  ( -9.645001968711920171, 4.042125922905831281, 6.587946042608958663 ) ) ;
#158142 = ORIENTED_EDGE ( 'NONE', *, *, #123715, .T. ) ;
#158143 = CARTESIAN_POINT ( 'NONE',  ( 5.401267763076613271, 1.683455835520174526, 1.188505893847252581 ) ) ;
#158144 = CARTESIAN_POINT ( 'NONE',  ( -7.715998819508785189, 8.174622508947939181, -0.7216878364870338292 ) ) ;
#158145 = CARTESIAN_POINT ( 'NONE',  ( -3.928111819657352566, 5.605883094398769195, 1.599625672291267398 ) ) ;
#158146 = CARTESIAN_POINT ( 'NONE',  ( -4.976767969047747542, 6.813382189656114640, 1.452644713377107877 ) ) ;
#158147 = CARTESIAN_POINT ( 'NONE',  ( 4.424476369979273294, -0.8654530498428643082, -1.825003331238822746 ) ) ;
#158149 = ORIENTED_EDGE ( 'NONE', *, *, #116619, .F. ) ;
#158148 = CARTESIAN_POINT ( 'NONE',  ( 5.830790380266278383, 1.493519825859883854, -1.644436761705171612 ) ) ;
#158151 = CARTESIAN_POINT ( 'NONE',  ( 8.432808358020016826, 10.86136238915529084, 1.443375672974076540 ) ) ;
#158150 = CARTESIAN_POINT ( 'NONE',  ( -6.064239847062411926, 10.29697326487330500, 0.000000000000000000 ) ) ;
#158152 = CARTESIAN_POINT ( 'NONE',  ( 7.332262146892202459, 7.448727347662698506, -0.7998128361456281477 ) ) ;
#158153 = CARTESIAN_POINT ( 'NONE',  ( 4.329017481302106063, 0.09909362218092979124, 2.058626247020868494 ) ) ;
#158154 = CARTESIAN_POINT ( 'NONE',  ( 3.340470361411255418, 0.4872029778183217252, -1.956561305313428978 ) ) ;
#158155 = ORIENTED_EDGE ( 'NONE', *, *, #105692, .F. ) ;
#158156 =( NAMED_UNIT ( * ) PLANE_ANGLE_UNIT ( ) SI_UNIT ( $, .RADIAN. ) );
#158157 = CARTESIAN_POINT ( 'NONE',  ( 5.030238685870051185, 5.827365540725222282, -1.199719254218452047 ) ) ;
#158158 = MECHANICAL_DESIGN_GEOMETRIC_PRESENTATION_REPRESENTATION (  '', ( #68271 ), #182395 ) ;
#158160 = EDGE_LOOP ( 'NONE', ( #9920, #155928, #182080, #67700 ) ) ;
#158159 = CARTESIAN_POINT ( 'NONE',  ( 0.006158830626129450057, 7.078243236992583398, -2.121324627965403220 ) ) ;
#158161 = CARTESIAN_POINT ( 'NONE',  ( 5.694759483343039719, 7.307619849039811655, -1.219011658351103478 ) ) ;
#158162 = CARTESIAN_POINT ( 'NONE',  ( 2.530624857006387618, 1.977747929495787371, -0.3905373530270899174 ) ) ;
#158163 = CARTESIAN_POINT ( 'NONE',  ( 2.870863542623874221, 1.748142402769039760, -0.5779331317549916136 ) ) ;
#158164 = CARTESIAN_POINT ( 'NONE',  ( 1.454236823263599376, 0.6660240913333862478, -2.209497540817098038 ) ) ;
#158165 = CARTESIAN_POINT ( 'NONE',  ( 4.441177836928239309, 7.339068688795062911, 1.199719254218452047 ) ) ;
#158166 = EDGE_CURVE ( 'NONE', #118849, #51477, #10701, .T. ) ;
#158167 = CARTESIAN_POINT ( 'NONE',  ( 3.233815116076131257, -1.449111151313630996, -1.604113057997895053 ) ) ;
#158168 = CARTESIAN_POINT ( 'NONE',  ( -6.307567778855718288, 8.381915046796901692, -1.599625672291263179 ) ) ;
#158169 = AXIS2_PLACEMENT_3D ( 'NONE', #184511, #137928, #4674 ) ;
#158170 = VERTEX_POINT ( 'NONE', #142893 ) ;
#158171 = DIRECTION ( 'NONE',  ( -0.6507913734559640506, -0.7592566023653003482, 0.000000000000000000 ) ) ;
#158172 = CARTESIAN_POINT ( 'NONE',  ( 1.428351348257720588, 1.801920623737063520, 0.5021531274154652502 ) ) ;
#158173 = CARTESIAN_POINT ( 'NONE',  ( 6.016478623866945874, 1.324313071814016141, -1.460584582105582285 ) ) ;
#158175 = CARTESIAN_POINT ( 'NONE',  ( 8.229436053370669413, 10.62409470039771442, 1.443375672974076540 ) ) ;
#158174 = CARTESIAN_POINT ( 'NONE',  ( -1.001543065824772872E-14, 4.571875000341418804, 1.575800808251672791 ) ) ;
#158177 = CARTESIAN_POINT ( 'NONE',  ( 0.1709339574563934483, -1.438030690398562239, 1.674123062825278563 ) ) ;
#158176 = CARTESIAN_POINT ( 'NONE',  ( -6.521635583373313061, 7.567328587812373719, -1.199719254218446718 ) ) ;
#158178 = FACE_OUTER_BOUND ( 'NONE', #118922, .T. ) ;
#158179 = CARTESIAN_POINT ( 'NONE',  ( 5.626797444871351139, 6.523350759560078593, 1.199719254218462483 ) ) ;
#158180 = CARTESIAN_POINT ( 'NONE',  ( -6.250472511100020334, 7.250971670160158311, 1.199719254218450271 ) ) ;
#158181 = AXIS2_PLACEMENT_3D ( 'NONE', #71448, #88808, #158077 ) ;
#158182 = CARTESIAN_POINT ( 'NONE',  ( 6.539320575229247368, 1.232987345766973775, 2.316458022558224972 ) ) ;
#158183 = CARTESIAN_POINT ( 'NONE',  ( 4.645367602377043603, -1.523440194387800650, -1.251305281888495102 ) ) ;
#158184 = CARTESIAN_POINT ( 'NONE',  ( 5.830798129077900072, 2.222503408945066816, 0.6210771851366378993 ) ) ;
#158186 = EDGE_CURVE ( 'NONE', #160603, #170224, #146541, .T. ) ;
#158185 = CARTESIAN_POINT ( 'NONE',  ( 6.391040216397121831, 0.1834577666269270046, 1.851959058998996710 ) ) ;
#158187 = CARTESIAN_POINT ( 'NONE',  ( 2.623947407551871169, 2.023649216642096960, -0.3979924315659318923 ) ) ;
#158188 = CARTESIAN_POINT ( 'NONE',  ( 7.131225611108100715, 7.422110755822004968, 0.7216878364870317197 ) ) ;
#158189 = CARTESIAN_POINT ( 'NONE',  ( 5.508355548902068577, 9.648441583686274470, 0.7998128361456331437 ) ) ;
#158190 = CARTESIAN_POINT ( 'NONE',  ( 6.385527161912102123, 9.433236874664039817, -1.082531754730537976 ) ) ;
#158191 = CARTESIAN_POINT ( 'NONE',  ( -1.402160292154681736E-14, 1.509375000341420359, -1.575800808251659024 ) ) ;
#158192 = CARTESIAN_POINT ( 'NONE',  ( 1.270994156678442596E-16, -6.530144695498194096, -11.00000000000000178 ) ) ;
#158193 = CARTESIAN_POINT ( 'NONE',  ( 4.921246571636183731, 7.724909519342112674, -1.082531754730549078 ) ) ;
#158194 = CARTESIAN_POINT ( 'NONE',  ( 4.879425774075326849, -0.1113562312203674326, 2.168454086520410495 ) ) ;
#158196 = CARTESIAN_POINT ( 'NONE',  ( 4.177188522404684079, 1.205947341878073287, 1.391433828303423326 ) ) ;
#158195 = DIRECTION ( 'NONE',  ( 0.000000000000000000, 0.000000000000000000, 1.000000000000000000 ) ) ;
#158197 = MANIFOLD_SOLID_BREP ( 'Sweep1[3]', #140154 ) ;
#158199 = CARTESIAN_POINT ( 'NONE',  ( 6.620655732516649294, 4.698502813744664941, 2.488957606609870421 ) ) ;
#158198 = CARTESIAN_POINT ( 'NONE',  ( 1.364683531249992088, 5.384375000341417916, 1.214306433183764966E-14 ) ) ;
#158200 = CARTESIAN_POINT ( 'NONE',  ( 6.198795224570643470, 1.821041368708445907, 1.219022265761634971 ) ) ;
#158201 = CARTESIAN_POINT ( 'NONE',  ( 0.3282377607281126153, 0.2388354509981848728, -1.225000000000013411 ) ) ;
#158202 = CARTESIAN_POINT ( 'NONE',  ( 0.3161853103110903729, -2.218393710063219615, 0.4432750438988151687 ) ) ;
#158203 = CARTESIAN_POINT ( 'NONE',  ( -3.999074104275988972, 7.816954204906529924, 0.3413819327131896175 ) ) ;
#158204 = CARTESIAN_POINT ( 'NONE',  ( -3.231779075379149546, 6.036511184309971689, -0.9899555337401846344 ) ) ;
#158205 = CARTESIAN_POINT ( 'NONE',  ( 6.493754380866193721, 6.839952184459461293, 0.5864284347954504817 ) ) ;
#158206 = CARTESIAN_POINT ( 'NONE',  ( -4.787437638956939523, 5.718337012605431369, -1.082531754730549967 ) ) ;
#158207 = CARTESIAN_POINT ( 'NONE',  ( 0.04731519813723151363, -1.748418646119804354, 0.7749314921376223575 ) ) ;
#158208 = CARTESIAN_POINT ( 'NONE',  ( 0.5140565032336151807, 1.225199188247323878, -1.277449566202024656 ) ) ;
#158209 = CARTESIAN_POINT ( 'NONE',  ( 5.830732115328919996, 1.350214353519451960, -1.493314199452821178 ) ) ;
#158210 = CARTESIAN_POINT ( 'NONE',  ( 6.277588818327314080, 7.282607361925381717, 1.199719254218462483 ) ) ;
#158211 = CARTESIAN_POINT ( 'NONE',  ( 4.348724867337580235, 0.5594899878812797933, 2.030215228624824952 ) ) ;
#158212 = CARTESIAN_POINT ( 'NONE',  ( 3.708511580433976107, 1.820041504565768742, 0.5977543794245043784 ) ) ;
#158213 = CARTESIAN_POINT ( 'NONE',  ( 3.469446951953614189E-15, 5.167241622962441383, 1.214306433183764966E-14 ) ) ;
#158214 = CARTESIAN_POINT ( 'NONE',  ( 4.685976223243822680, -1.210123887884282601, -1.553869430650482997 ) ) ;
#158215 = CARTESIAN_POINT ( 'NONE',  ( 6.064714679231743233, 0.6376439298158544933, 1.916535431269225098 ) ) ;
#158216 = CARTESIAN_POINT ( 'NONE',  ( 3.256579335763456040, -1.417408692332474462, 1.220890361658559575 ) ) ;
#158219 = EDGE_LOOP ( 'NONE', ( #90344, #1547, #85634, #157077 ) ) ;
#158218 = CARTESIAN_POINT ( 'NONE',  ( 1.406358598101828283, -1.903450966454448334, -0.1843715739238485363 ) ) ;
#158217 = CARTESIAN_POINT ( 'NONE',  ( 4.740679804603589176, 0.2991043602584910199, 1.698571524128352994 ) ) ;
#158221 = CARTESIAN_POINT ( 'NONE',  ( 5.341549334104200852, 5.334155099317434257, 0.7216878364870317197 ) ) ;
#158220 = CARTESIAN_POINT ( 'NONE',  ( 1.981372325807278623, -0.1102420082176903682, -2.204251428397439483 ) ) ;
#158222 = CARTESIAN_POINT ( 'NONE',  ( -1.402160292154681736E-14, 2.259375000341416140, -1.575800808251660134 ) ) ;
#158223 = CARTESIAN_POINT ( 'NONE',  ( 6.725062055625550705, -1.793239977796506457, -0.7961783947641184467 ) ) ;
#158224 = CARTESIAN_POINT ( 'NONE',  ( 8.372323551638698902, 9.726464550788689323, 1.199719254218462483 ) ) ;
#158225 = CARTESIAN_POINT ( 'NONE',  ( 10.59781858645781405, 13.79999999999998295, 3.302687032930892830 ) ) ;
#158226 = CARTESIAN_POINT ( 'NONE',  ( 3.009610312849396951, 6.452363523749469643, -0.06592220986071165023 ) ) ;
#158227 = CARTESIAN_POINT ( 'NONE',  ( 7.626074735689158501, -6.442483420751605294, 8.280982046698079913 ) ) ;
#158228 = ORIENTED_EDGE ( 'NONE', *, *, #73977, .T. ) ;
#158229 = CARTESIAN_POINT ( 'NONE',  ( 2.365759603224312446, -0.4558734232973959966, 2.019384234097781228 ) ) ;
#158230 = CARTESIAN_POINT ( 'NONE',  ( 1.499999999999989120, 3.504166666666683749, 0.8660254037844524744 ) ) ;
#158231 = CARTESIAN_POINT ( 'NONE',  ( 4.611744806942754238, 8.532119374741881757, -0.7998128361456231517 ) ) ;
#158232 = CARTESIAN_POINT ( 'NONE',  ( -7.172426956829277778, 8.326585190177668849, -1.199719254218452935 ) ) ;
#158233 = CARTESIAN_POINT ( 'NONE',  ( 2.905190055078214595, 6.611415174225076186, 0.7998128361456271485 ) ) ;
#158235 = EDGE_CURVE ( 'NONE', #198538, #195414, #141808, .T. ) ;
#158234 = CARTESIAN_POINT ( 'NONE',  ( 6.481110812017948142, -1.938455339442773706, -0.8599551062365148324 ) ) ;
#158236 = CARTESIAN_POINT ( 'NONE',  ( -9.499771961674738918, -7.051679281653864706, -0.06642998979260299197 ) ) ;
#158237 = CARTESIAN_POINT ( 'NONE',  ( -0.6823417656250212460, 3.051041667008084879, 1.181850606188767472 ) ) ;
#158238 = EDGE_CURVE ( 'NONE', #86477, #114840, #164531, .T. ) ;
#158240 = CARTESIAN_POINT ( 'NONE',  ( 9.083599731475988648, 10.66024977721925104, 1.082531754730549967 ) ) ;
#158239 = CARTESIAN_POINT ( 'NONE',  ( 0.07602376731354228145, -7.154544010627095219, -9.579698345292676720 ) ) ;
#158241 = CARTESIAN_POINT ( 'NONE',  ( 5.079453798366286854, 1.392331892589277142, -1.458333960840517696 ) ) ;
#158242 = CARTESIAN_POINT ( 'NONE',  ( 4.839036869973236676, -1.621808105726432414, -1.019334933273335242 ) ) ;
#158243 = CARTESIAN_POINT ( 'NONE',  ( 2.138457411672203712, 0.4836887423533155483, 2.137355272389021899 ) ) ;
#158244 =( BOUNDED_SURFACE ( )  B_SPLINE_SURFACE ( 1, 2, ( 
 ( #133271, #199279, #18402, #134337, #127201, #50921, #183044, #179866, #15204, #213398, #150569, #200342, #118118, #193168, #184103, #35723, #101799, #47757, #31490, #97566, #163623, #20531, #123481, #119175, #53041, #105016, #72478, #5321, #137514, #69268, #120255, #139660, #103944, #102869, #122410, #107194, #152680, #23734, #19466, #185160, #36785, #168927, #85542, #203531, #86613, #106118, #70333, #41087, #151632, #21573, #4263, #136450, #7476, #22653, #171056, #202467, #201403, #3198, #87679, #38933, #169986, #55185, #186232, #54120, #154821, #37865, #205680, #88765, #153752, #71402, #135382, #121331, #138578, #187307, #6406, #204601, #56253, #188368, #189444, #40008, #172141, #89839, #155888, #73558, #57317, #44277, #24798, #191558, #77819, #161215, #45343, #76747, #75696, #176402, #174289, #177468, #25864, #28008, #190495, #78875, #193699, #94106, #11744, #12802, #140740, #43222, #95166, #143940, #144998, #93037, #141810, #160147, #90901, #109339, #110398, #59441, #8554, #206752, #159079, #60500, #156963, #29082, #175349, #61574, #207813, #26929, #74633, #125598, #111462, #58382, #10676, #128786, #173219, #142868, #209936, #62626, #208870, #126660, #124538, #46404, #194767, #42153, #108268, #192625, #211003, #127742, #91974, #158032, #9620, #146051, #34392, #99411, #98342, #81021, #100464, #166539, #30143, #97292, #162282, #163350, #179597, #18127, #84216, #195843, #17060, #178533, #212065, #134075, #50651, #200083, #82076, #49585, #181699, #79948, #13870, #199006, #47484, #63703, #147109, #148169, #129860, #164407, #112520, #1870, #150304, #32276, #15991, #214171, #14926, #182774, #213134, #64765, #165465, #96232, #113594, #114657, #65797, #115709, #130907, #67930, #131945, #31218, #196899, #197956, #48538, #180651, #33329, #133006, #83140, #149218, #793, #116777, #66861, #87430, #187046, #89581, #103685, #201144, #138321, #35459, #117855, #86355, #72214, #167606, #70075, #7215, #51732, #20271, #88506, #155630, #136189, #152426, #151369, #139392, #73289, #19204, #183847, #4005, #101537, #37604, #168667 ),
 ( #202207, #153498, #53861, #36525, #184901, #119994, #2938, #85283, #69010, #185971, #102612, #169734, #21323, #135127, #52782, #5068, #118921, #71143, #137260, #203280, #54927, #121079, #204337, #39745, #38678, #104757, #154568, #170806, #22397, #6144, #55995, #122146, #188114, #105850, #171877, #23473, #75445, #143695, #205425, #59187, #141558, #206496, #94919, #90648, #24540, #76501, #44029, #191305, #109083, #40829, #91725, #111215, #207565, #74384, #93856, #78632, #124286, #209687, #57063, #156709, #8299, #140485, #123227, #175098, #125342, #58127, #208620, #190245, #61331, #41903, #60254, #108014, #177217, #11501, #126411, #110147, #193461, #172961, #9374, #127490, #176160, #45105, #42973, #174040, #192373, #189192, #26685, #142612, #157776, #106938, #25613, #92787, #158832, #10429, #28831, #27760, #159894, #77572, #160968, #12558, #165218, #194518, #144757, #113352, #16809, #14688, #129615, #80784, #97054, #112280, #115469, #98115, #146872, #195602, #49350, #181461, #62388, #211824, #46166, #63461, #79704, #33091, #99165, #95988, #164166, #128553, #178296, #82894, #197708, #210768, #32029, #147920, #213936, #145819, #47237, #29903, #179357, #30979, #212894, #15752, #163108, #81836, #162040, #13631, #64526, #130671, #196659, #48300, #114411, #180411, #65557, #131703, #110848, #211467, #25258, #126048, #159533, #60967, #10072, #177930, #143326, #45809, #161686, #209320, #124988, #75085, #43675, #144403, #194162, #9010, #127122, #128201, #111929, #11131, #44742, #13281, #175801, #29544, #192012, #59897, #157419, #193093, #190947, #95636, #42611, #176855, #141198, #79354, #210404, #28468, #94560, #145472, #91358, #142252, #123929, #160602, #189897, #109793, #92432, #12205, #41539, #208264, #78276, #76148, #173682, #207209, #27393, #77208, #107652, #58833, #93493, #62046, #26320, #108720, #174746, #158472, #83605, #179002, #81486, #18599, #63101, #31682, #99869, #167007, #147563, #97758, #162755, #65208, #96706, #199473, #50053, #48998, #163816, #51115, #117240, #195241, #47952, #112990, #114067, #130318, #183240 ) ),
 .UNSPECIFIED., .F., .F., .T. ) 
 B_SPLINE_SURFACE_WITH_KNOTS ( ( 2, 2 ),
 ( 3, 2, 2, 2, 2, 2, 2, 2, 2, 2, 2, 2, 2, 2, 2, 2, 2, 2, 2, 2, 2, 2, 2, 2, 2, 2, 2, 2, 2, 2, 2, 2, 2, 2, 2, 2, 2, 2, 2, 2, 2, 2, 2, 2, 2, 2, 2, 2, 2, 2, 2, 2, 2, 2, 2, 2, 2, 2, 2, 2, 2, 2, 2, 2, 2, 2, 2, 2, 2, 2, 2, 2, 2, 2, 2, 2, 2, 2, 2, 2, 2, 2, 2, 2, 2, 2, 2, 2, 2, 2, 2, 2, 2, 2, 2, 2, 2, 2, 2, 2, 2, 2, 2, 2, 2, 2, 2, 2, 2, 2, 2, 2, 2, 2, 2, 2, 2, 2, 2, 2, 3 ),
 ( 0.000000000000000000, 1.000000000000000000 ),
 ( 0.000000000000000000, 0.008333333333333333218, 0.01666666666666666644, 0.02500000000000000139, 0.03333333333333333287, 0.04166666666666666435, 0.05000000000000000278, 0.05833333333333333426, 0.06666666666666666574, 0.07499999999999999722, 0.08333333333333332871, 0.09166666666666666019, 0.1000000000000000056, 0.1083333333333333370, 0.1166666666666666685, 0.1250000000000000000, 0.1333333333333333315, 0.1416666666666666630, 0.1499999999999999944, 0.1583333333333333259, 0.1666666666666666574, 0.1749999999999999889, 0.1833333333333333204, 0.1916666666666666796, 0.2000000000000000111, 0.2083333333333333426, 0.2166666666666666741, 0.2250000000000000056, 0.2333333333333333370, 0.2416666666666666685, 0.2500000000000000000, 0.2583333333333333592, 0.2666666666666666630, 0.2750000000000000222, 0.2833333333333333259, 0.2916666666666666852, 0.2999999999999999889, 0.3083333333333333481, 0.3166666666666666519, 0.3250000000000000111, 0.3333333333333333148, 0.3416666666666666741, 0.3499999999999999778, 0.3583333333333333370, 0.3666666666666666408, 0.3750000000000000000, 0.3833333333333333592, 0.3916666666666666630, 0.4000000000000000222, 0.4083333333333333259, 0.4166666666666666852, 0.4249999999999999889, 0.4333333333333333481, 0.4416666666666666519, 0.4500000000000000111, 0.4583333333333333148, 0.4666666666666666741, 0.4749999999999999778, 0.4833333333333333370, 0.4916666666666666408, 0.5000000000000000000, 0.5083333333333333037, 0.5166666666666667185, 0.5250000000000000222, 0.5333333333333333259, 0.5416666666666666297, 0.5500000000000000444, 0.5583333333333333481, 0.5666666666666666519, 0.5749999999999999556, 0.5833333333333333703, 0.5916666666666666741, 0.5999999999999999778, 0.6083333333333332815, 0.6166666666666666963, 0.6250000000000000000, 0.6333333333333333037, 0.6416666666666667185, 0.6500000000000000222, 0.6583333333333333259, 0.6666666666666666297, 0.6750000000000000444, 0.6833333333333333481, 0.6916666666666666519, 0.6999999999999999556, 0.7083333333333333703, 0.7166666666666666741, 0.7249999999999999778, 0.7333333333333332815, 0.7416666666666666963, 0.7500000000000000000, 0.7583333333333333037, 0.7666666666666667185, 0.7750000000000000222, 0.7833333333333333259, 0.7916666666666666297, 0.8000000000000000444, 0.8083333333333333481, 0.8166666666666666519, 0.8249999999999999556, 0.8333333333333333703, 0.8416666666666666741, 0.8499999999999999778, 0.8583333333333332815, 0.8666666666666666963, 0.8750000000000000000, 0.8833333333333333037, 0.8916666666666667185, 0.9000000000000000222, 0.9083333333333333259, 0.9166666666666666297, 0.9250000000000000444, 0.9333333333333333481, 0.9416666666666666519, 0.9499999999999999556, 0.9583333333333333703, 0.9666666666666666741, 0.9749999999999999778, 0.9833333333333332815, 0.9916666666666666963, 1.000000000000000000 ),
 .UNSPECIFIED. ) 
 GEOMETRIC_REPRESENTATION_ITEM ( )  RATIONAL_B_SPLINE_SURFACE ( (
 ( 1.000000000000000000, 0.8660254037844387076, 1.000000000000000000, 0.8660254037844387076, 1.000000000000000000, 0.8660254037844387076, 1.000000000000000000, 0.8660254037844387076, 1.000000000000000000, 0.8660254037844387076, 1.000000000000000000, 0.8660254037844387076, 1.000000000000000000, 0.8660254037844387076, 1.000000000000000000, 0.8660254037844387076, 1.000000000000000000, 0.8660254037844387076, 1.000000000000000000, 0.8660254037844387076, 1.000000000000000000, 0.8660254037844387076, 1.000000000000000000, 0.8660254037844387076, 1.000000000000000000, 0.8660254037844387076, 1.000000000000000000, 0.8660254037844387076, 1.000000000000000000, 0.8660254037844387076, 1.000000000000000000, 0.8660254037844387076, 1.000000000000000000, 0.8660254037844387076, 1.000000000000000000, 0.8660254037844387076, 1.000000000000000000, 0.8660254037844387076, 1.000000000000000000, 0.8660254037844387076, 1.000000000000000000, 0.8660254037844387076, 1.000000000000000000, 0.8660254037844387076, 1.000000000000000000, 0.8660254037844387076, 1.000000000000000000, 0.8660254037844387076, 1.000000000000000000, 0.8660254037844387076, 1.000000000000000000, 0.8660254037844387076, 1.000000000000000000, 0.8660254037844387076, 1.000000000000000000, 0.8660254037844387076, 1.000000000000000000, 0.8660254037844387076, 1.000000000000000000, 0.8660254037844387076, 1.000000000000000000, 0.8660254037844387076, 1.000000000000000000, 0.8660254037844387076, 1.000000000000000000, 0.8660254037844387076, 1.000000000000000000, 0.8660254037844387076, 1.000000000000000000, 0.8660254037844387076, 1.000000000000000000, 0.8660254037844387076, 1.000000000000000000, 0.8660254037844387076, 1.000000000000000000, 0.8660254037844387076, 1.000000000000000000, 0.8660254037844387076, 1.000000000000000000, 0.8660254037844387076, 1.000000000000000000, 0.8660254037844387076, 1.000000000000000000, 0.8660254037844387076, 1.000000000000000000, 0.8660254037844387076, 1.000000000000000000, 0.8660254037844387076, 1.000000000000000000, 0.8660254037844387076, 1.000000000000000000, 0.8660254037844387076, 1.000000000000000000, 0.8660254037844387076, 1.000000000000000000, 0.8660254037844387076, 1.000000000000000000, 0.8660254037844387076, 1.000000000000000000, 0.8660254037844387076, 1.000000000000000000, 0.8660254037844387076, 1.000000000000000000, 0.8660254037844387076, 1.000000000000000000, 0.8660254037844387076, 1.000000000000000000, 0.8660254037844387076, 1.000000000000000000, 0.8660254037844387076, 1.000000000000000000, 0.8660254037844387076, 1.000000000000000000, 0.8660254037844387076, 1.000000000000000000, 0.8660254037844387076, 1.000000000000000000, 0.8660254037844387076, 1.000000000000000000, 0.8660254037844387076, 1.000000000000000000, 0.8660254037844387076, 1.000000000000000000, 0.8660254037844387076, 1.000000000000000000, 0.8660254037844387076, 1.000000000000000000, 0.8660254037844387076, 1.000000000000000000, 0.8660254037844387076, 1.000000000000000000, 0.8660254037844387076, 1.000000000000000000, 0.8660254037844387076, 1.000000000000000000, 0.8660254037844387076, 1.000000000000000000, 0.8660254037844387076, 1.000000000000000000, 0.8660254037844387076, 1.000000000000000000, 0.8660254037844387076, 1.000000000000000000, 0.8660254037844387076, 1.000000000000000000, 0.8660254037844387076, 1.000000000000000000, 0.8660254037844387076, 1.000000000000000000, 0.8660254037844387076, 1.000000000000000000, 0.8660254037844387076, 1.000000000000000000, 0.8660254037844387076, 1.000000000000000000, 0.8660254037844387076, 1.000000000000000000, 0.8660254037844387076, 1.000000000000000000, 0.8660254037844387076, 1.000000000000000000, 0.8660254037844387076, 1.000000000000000000, 0.8660254037844387076, 1.000000000000000000, 0.8660254037844387076, 1.000000000000000000, 0.8660254037844387076, 1.000000000000000000, 0.8660254037844387076, 1.000000000000000000, 0.8660254037844387076, 1.000000000000000000, 0.8660254037844387076, 1.000000000000000000, 0.8660254037844387076, 1.000000000000000000, 0.8660254037844387076, 1.000000000000000000, 0.8660254037844387076, 1.000000000000000000, 0.8660254037844387076, 1.000000000000000000, 0.8660254037844387076, 1.000000000000000000, 0.8660254037844387076, 1.000000000000000000, 0.8660254037844387076, 1.000000000000000000, 0.8660254037844387076, 1.000000000000000000, 0.8660254037844387076, 1.000000000000000000, 0.8660254037844387076, 1.000000000000000000, 0.8660254037844387076, 1.000000000000000000, 0.8660254037844387076, 1.000000000000000000, 0.8660254037844387076, 1.000000000000000000, 0.8660254037844387076, 1.000000000000000000, 0.8660254037844387076, 1.000000000000000000, 0.8660254037844387076, 1.000000000000000000, 0.8660254037844387076, 1.000000000000000000, 0.8660254037844387076, 1.000000000000000000, 0.8660254037844387076, 1.000000000000000000, 0.8660254037844387076, 1.000000000000000000, 0.8660254037844387076, 1.000000000000000000, 0.8660254037844387076, 1.000000000000000000, 0.8660254037844387076, 1.000000000000000000, 0.8660254037844387076, 1.000000000000000000, 0.8660254037844387076, 1.000000000000000000, 0.8660254037844387076, 1.000000000000000000, 0.8660254037844387076, 1.000000000000000000, 0.8660254037844387076, 1.000000000000000000, 0.8660254037844387076, 1.000000000000000000, 0.8660254037844387076, 1.000000000000000000, 0.8660254037844387076, 1.000000000000000000, 0.8660254037844387076, 1.000000000000000000, 0.8660254037844387076, 1.000000000000000000),
 ( 1.000000000000000000, 0.8660254037844387076, 1.000000000000000000, 0.8660254037844387076, 1.000000000000000000, 0.8660254037844387076, 1.000000000000000000, 0.8660254037844387076, 1.000000000000000000, 0.8660254037844387076, 1.000000000000000000, 0.8660254037844387076, 1.000000000000000000, 0.8660254037844387076, 1.000000000000000000, 0.8660254037844387076, 1.000000000000000000, 0.8660254037844387076, 1.000000000000000000, 0.8660254037844387076, 1.000000000000000000, 0.8660254037844387076, 1.000000000000000000, 0.8660254037844387076, 1.000000000000000000, 0.8660254037844387076, 1.000000000000000000, 0.8660254037844387076, 1.000000000000000000, 0.8660254037844387076, 1.000000000000000000, 0.8660254037844387076, 1.000000000000000000, 0.8660254037844387076, 1.000000000000000000, 0.8660254037844387076, 1.000000000000000000, 0.8660254037844387076, 1.000000000000000000, 0.8660254037844387076, 1.000000000000000000, 0.8660254037844387076, 1.000000000000000000, 0.8660254037844387076, 1.000000000000000000, 0.8660254037844387076, 1.000000000000000000, 0.8660254037844387076, 1.000000000000000000, 0.8660254037844387076, 1.000000000000000000, 0.8660254037844387076, 1.000000000000000000, 0.8660254037844387076, 1.000000000000000000, 0.8660254037844387076, 1.000000000000000000, 0.8660254037844387076, 1.000000000000000000, 0.8660254037844387076, 1.000000000000000000, 0.8660254037844387076, 1.000000000000000000, 0.8660254037844387076, 1.000000000000000000, 0.8660254037844387076, 1.000000000000000000, 0.8660254037844387076, 1.000000000000000000, 0.8660254037844387076, 1.000000000000000000, 0.8660254037844387076, 1.000000000000000000, 0.8660254037844387076, 1.000000000000000000, 0.8660254037844387076, 1.000000000000000000, 0.8660254037844387076, 1.000000000000000000, 0.8660254037844387076, 1.000000000000000000, 0.8660254037844387076, 1.000000000000000000, 0.8660254037844387076, 1.000000000000000000, 0.8660254037844387076, 1.000000000000000000, 0.8660254037844387076, 1.000000000000000000, 0.8660254037844387076, 1.000000000000000000, 0.8660254037844387076, 1.000000000000000000, 0.8660254037844387076, 1.000000000000000000, 0.8660254037844387076, 1.000000000000000000, 0.8660254037844387076, 1.000000000000000000, 0.8660254037844387076, 1.000000000000000000, 0.8660254037844387076, 1.000000000000000000, 0.8660254037844387076, 1.000000000000000000, 0.8660254037844387076, 1.000000000000000000, 0.8660254037844387076, 1.000000000000000000, 0.8660254037844387076, 1.000000000000000000, 0.8660254037844387076, 1.000000000000000000, 0.8660254037844387076, 1.000000000000000000, 0.8660254037844387076, 1.000000000000000000, 0.8660254037844387076, 1.000000000000000000, 0.8660254037844387076, 1.000000000000000000, 0.8660254037844387076, 1.000000000000000000, 0.8660254037844387076, 1.000000000000000000, 0.8660254037844387076, 1.000000000000000000, 0.8660254037844387076, 1.000000000000000000, 0.8660254037844387076, 1.000000000000000000, 0.8660254037844387076, 1.000000000000000000, 0.8660254037844387076, 1.000000000000000000, 0.8660254037844387076, 1.000000000000000000, 0.8660254037844387076, 1.000000000000000000, 0.8660254037844387076, 1.000000000000000000, 0.8660254037844387076, 1.000000000000000000, 0.8660254037844387076, 1.000000000000000000, 0.8660254037844387076, 1.000000000000000000, 0.8660254037844387076, 1.000000000000000000, 0.8660254037844387076, 1.000000000000000000, 0.8660254037844387076, 1.000000000000000000, 0.8660254037844387076, 1.000000000000000000, 0.8660254037844387076, 1.000000000000000000, 0.8660254037844387076, 1.000000000000000000, 0.8660254037844387076, 1.000000000000000000, 0.8660254037844387076, 1.000000000000000000, 0.8660254037844387076, 1.000000000000000000, 0.8660254037844387076, 1.000000000000000000, 0.8660254037844387076, 1.000000000000000000, 0.8660254037844387076, 1.000000000000000000, 0.8660254037844387076, 1.000000000000000000, 0.8660254037844387076, 1.000000000000000000, 0.8660254037844387076, 1.000000000000000000, 0.8660254037844387076, 1.000000000000000000, 0.8660254037844387076, 1.000000000000000000, 0.8660254037844387076, 1.000000000000000000, 0.8660254037844387076, 1.000000000000000000, 0.8660254037844387076, 1.000000000000000000, 0.8660254037844387076, 1.000000000000000000, 0.8660254037844387076, 1.000000000000000000, 0.8660254037844387076, 1.000000000000000000, 0.8660254037844387076, 1.000000000000000000, 0.8660254037844387076, 1.000000000000000000, 0.8660254037844387076, 1.000000000000000000, 0.8660254037844387076, 1.000000000000000000, 0.8660254037844387076, 1.000000000000000000, 0.8660254037844387076, 1.000000000000000000, 0.8660254037844387076, 1.000000000000000000, 0.8660254037844387076, 1.000000000000000000, 0.8660254037844387076, 1.000000000000000000, 0.8660254037844387076, 1.000000000000000000, 0.8660254037844387076, 1.000000000000000000, 0.8660254037844387076, 1.000000000000000000, 0.8660254037844387076, 1.000000000000000000, 0.8660254037844387076, 1.000000000000000000, 0.8660254037844387076, 1.000000000000000000, 0.8660254037844387076, 1.000000000000000000, 0.8660254037844387076, 1.000000000000000000, 0.8660254037844387076, 1.000000000000000000, 0.8660254037844387076, 1.000000000000000000, 0.8660254037844387076, 1.000000000000000000, 0.8660254037844387076, 1.000000000000000000, 0.8660254037844387076, 1.000000000000000000, 0.8660254037844387076, 1.000000000000000000, 0.8660254037844387076, 1.000000000000000000) ) ) 
 REPRESENTATION_ITEM ( '' )  SURFACE ( )  );
#158245 = CARTESIAN_POINT ( 'NONE',  ( -3.280709984826931436, 6.771319382366050021, 0.7216878364870010776 ) ) ;
#158247 = CIRCLE ( 'NONE', #138033, 0.08000000000000020983 ) ;
#158246 = CARTESIAN_POINT ( 'NONE',  ( 0.7499999999999902300, 2.014583334016148530, 1.299038105676669330 ) ) ;
#158248 = CARTESIAN_POINT ( 'NONE',  ( 5.291276029577359985, -0.05376236717486576611, -2.012660120947160181 ) ) ;
#158249 = CARTESIAN_POINT ( 'NONE',  ( 1.546972149855216250, 0.1906517044060058452, 1.902890584052991718 ) ) ;
#158250 = CARTESIAN_POINT ( 'NONE',  ( -4.720210035852093533, 8.658662141802762946, -0.7998128361456281477 ) ) ;
#158252 = CARTESIAN_POINT ( 'NONE',  ( 0.4039230143318903177, -1.081087622585241714, -1.701935196855845822 ) ) ;
#158251 = CARTESIAN_POINT ( 'NONE',  ( -4.121315508874280553, 3.910548969882488901, -0.7216878364870207285 ) ) ;
#158253 = CARTESIAN_POINT ( 'NONE',  ( -8.012344526598182026E-15, 10.35937500034139624, -1.575800808251669460 ) ) ;
#158255 = CARTESIAN_POINT ( 'NONE',  ( -6.967964602780620353, 7.093989889524320525, 0.000000000000000000 ) ) ;
#158254 = CARTESIAN_POINT ( 'NONE',  ( 3.983990651536262195, -2.068283627568163308, -0.3046923749255076586 ) ) ;
#158257 = ORIENTED_EDGE ( 'NONE', *, *, #125247, .F. ) ;
#158256 = CARTESIAN_POINT ( 'NONE',  ( 2.115808521728879565, -0.8096002590626363293, -1.522937571937353241 ) ) ;
#158258 = CARTESIAN_POINT ( 'NONE',  ( 6.504144398916748671, -0.9053081408615070158, 1.915699539216948688 ) ) ;
#158259 = CARTESIAN_POINT ( 'NONE',  ( 5.449487677688982679, 8.445153826357429949, -1.199719254218446718 ) ) ;
#158260 = CARTESIAN_POINT ( 'NONE',  ( 11.92619526913699879, 19.00000000000000000, 1.328859060402684644 ) ) ;
#158261 = CARTESIAN_POINT ( 'NONE',  ( -1.737500000000000266, -2.464583332377416447, -3.009438278150923907 ) ) ;
#158262 = CARTESIAN_POINT ( 'NONE',  ( 0.000000000000000000, 0.08000000000000020983, -12.00000000000000178 ) ) ;
#158263 = CARTESIAN_POINT ( 'NONE',  ( 5.250031796989762967, 7.148123067953287446, 1.599625672291267398 ) ) ;
#158264 = EDGE_LOOP ( 'NONE', ( #185735, #34450, #181822 ) ) ;
#158265 = DIRECTION ( 'NONE',  ( 0.000000000000000000, -1.000000000000000000, 0.000000000000000000 ) ) ;
#158266 = CARTESIAN_POINT ( 'NONE',  ( 2.719172733320520674, 1.531317187073286901, 0.9673847807401686483 ) ) ;
#158267 = ORIENTED_EDGE ( 'NONE', *, *, #83921, .T. ) ;
#158268 = CARTESIAN_POINT ( 'NONE',  ( 4.029797971759831121, 5.724516938518342535, -1.599625672291255185 ) ) ;
#158269 = CARTESIAN_POINT ( 'NONE',  ( 5.248941747146098180, 6.152795455539095570, -1.199719254218452047 ) ) ;
#158270 = CARTESIAN_POINT ( 'NONE',  ( 3.562975276761202181, -1.478990456472810910, 1.045639718295880094 ) ) ;
#158271 = DIRECTION ( 'NONE',  ( 0.000000000000000000, 0.000000000000000000, -1.000000000000000000 ) ) ;
#158272 = CARTESIAN_POINT ( 'NONE',  ( -10.99931799034184365, -8.075210796978268490, 0.1485693272542949472 ) ) ;
#158273 = CARTESIAN_POINT ( 'NONE',  ( 5.886424920137334205, 5.980649323864647648, 0.1385726864747312270 ) ) ;
#158274 = CARTESIAN_POINT ( 'NONE',  ( 4.457361271359429722, 1.493968932455931542, 1.109517434556703597 ) ) ;
#158275 = CARTESIAN_POINT ( 'NONE',  ( 1.458442676765151269, -1.819496111524568027, -0.5994125798251969117 ) ) ;
#158276 = CARTESIAN_POINT ( 'NONE',  ( 0.6393319655835437709, -1.287349573739982933, -1.294668131371433661 ) ) ;
#158277 = DIRECTION ( 'NONE',  ( -0.6292706268317891372, -0.7771862570881751253, 0.000000000000000000 ) ) ;
#158278 = VECTOR ( 'NONE', #122950, 1000.000000000000000 ) ;
#158279 = CARTESIAN_POINT ( 'NONE',  ( 4.826264338009964128, 8.099924789650724932, 0.8724150771263041726 ) ) ;
#158280 = CARTESIAN_POINT ( 'NONE',  ( 4.968759571299464994, 8.067260998001806627, 1.096838584164006924 ) ) ;
#158281 = CARTESIAN_POINT ( 'NONE',  ( -3.707465945607718805, 7.355851012256872323, 0.5743249234583160945 ) ) ;
#158282 = CARTESIAN_POINT ( 'NONE',  ( 4.175484721775176489, 3.976419294354625933, -0.06592222766770190756 ) ) ;
#158283 = CARTESIAN_POINT ( 'NONE',  ( 6.805829924380105034, 9.923590097543378619, 1.082531754730558626 ) ) ;
#158284 = CARTESIAN_POINT ( 'NONE',  ( 5.225436369306192930, 0.1968503305618974075, -1.959608170402066696 ) ) ;
#158285 = CARTESIAN_POINT ( 'NONE',  ( -3.958090780185743451, 6.705190779270287393, -1.199719254218452047 ) ) ;
#158286 = CARTESIAN_POINT ( 'NONE',  ( -11.89942855770814134, 9.799999999999998934, -0.7000000000000009548 ) ) ;
#158287 = CARTESIAN_POINT ( 'NONE',  ( 0.4805627621443783193, -0.2577823606141148027, -2.074612465628209890 ) ) ;
#158288 = CARTESIAN_POINT ( 'NONE',  ( 7.202405917357655341, 9.425892875049191488, 1.599625672291281386 ) ) ;
#158289 = CARTESIAN_POINT ( 'NONE',  ( 5.772470297455748245, -1.221717764600898981, 1.489408783192472052 ) ) ;
#158290 = CARTESIAN_POINT ( 'NONE',  ( -4.880045225915050189, 7.780804299287790826, 1.199719254218464037 ) ) ;
#158291 = CARTESIAN_POINT ( 'NONE',  ( 1.113953379265147925, -0.8168401028521531382, -1.632710947565917170 ) ) ;
#158292 = CARTESIAN_POINT ( 'NONE',  ( 1.682535984017709874, -1.178549783888741320, 1.865657194899547733 ) ) ;
#158293 = CARTESIAN_POINT ( 'NONE',  ( 0.7500000000000006661, 10.33333333333333393, 1.299038105676657340 ) ) ;
#158294 = CARTESIAN_POINT ( 'NONE',  ( 1.459083999156213451, -1.613880964290700160, 1.025699646091532857 ) ) ;
#158295 = CARTESIAN_POINT ( 'NONE',  ( 6.948121156015312216, -0.8458062566301125518, 1.777170381402736865 ) ) ;
#158296 = CARTESIAN_POINT ( 'NONE',  ( 2.173291266613562644, 1.196360937402714875, 1.529712666019187761 ) ) ;
#158297 = CARTESIAN_POINT ( 'NONE',  ( 0.7728142736522191081, -2.006652962095498260, 0.1948079406639269262 ) ) ;
#158299 = CARTESIAN_POINT ( 'NONE',  ( 6.315283160355378733, -1.595611397598785564, -0.9574585435550940771 ) ) ;
#158298 = CARTESIAN_POINT ( 'NONE',  ( -4.793689830883590020, 7.750332681742931662, 1.199719254218452935 ) ) ;
#158300 = CARTESIAN_POINT ( 'NONE',  ( 3.576318658954677598, 7.394398545414291313, 0.7998128361456281477 ) ) ;
#158301 = CARTESIAN_POINT ( 'NONE',  ( -11.33772463945036968, 13.40000000000000036, -3.600000000000000977 ) ) ;
#158302 = CARTESIAN_POINT ( 'NONE',  ( 4.053833101416107532, 3.984115073677586327, -0.7711264060391578301 ) ) ;
#158303 = CARTESIAN_POINT ( 'NONE',  ( -4.822949958159302497, 6.649860922651058992, -1.599625672291256295 ) ) ;
#158304 = CARTESIAN_POINT ( 'NONE',  ( -5.152980901645737077, 8.169505597632108262, -1.199719254218453823 ) ) ;
#158305 = CARTESIAN_POINT ( 'NONE',  ( 2.542740116143254792, -1.820367712357463974, 1.220030464664762393 ) ) ;
#158306 = CARTESIAN_POINT ( 'NONE',  ( 4.853455804012228647, 4.764712647543454693, 0.7216878364870317197 ) ) ;
#158307 = CARTESIAN_POINT ( 'NONE',  ( 5.691390622686558487, 9.861982503101517139, 0.7998128361456341429 ) ) ;
#158308 = CARTESIAN_POINT ( 'NONE',  ( 1.342212891865499298E-15, -2.000000000000001776, -10.92000000000000171 ) ) ;
#158309 = CARTESIAN_POINT ( 'NONE',  ( 2.596107596775329540, -1.820790993511243849, -0.1344670722737417168 ) ) ;
#158310 = CARTESIAN_POINT ( 'NONE',  ( -1.500000000000008216, 13.03125000068279604, 3.469446951953614189E-15 ) ) ;
#158311 = CARTESIAN_POINT ( 'NONE',  ( -4.776550190716183586, 4.467063398790632966, 1.214306433183764966E-14 ) ) ;
#158312 = CIRCLE ( 'NONE', #109974, 0.05000000000000057176 ) ;
#158313 = CARTESIAN_POINT ( 'NONE',  ( -4.600441534204600558, 8.479163753367195966, -0.2584006677722027745 ) ) ;
#158314 = DIRECTION ( 'NONE',  ( 8.881784197001252323E-16, 0.000000000000000000, 1.000000000000000000 ) ) ;
#158315 = CARTESIAN_POINT ( 'NONE',  ( 9.185812768458653466, 10.67553530374532045, 1.199719254218453823 ) ) ;
#158316 = CARTESIAN_POINT ( 'NONE',  ( 1.295397306693826467, 1.458444760659328265, 1.258811869801695682 ) ) ;
#158317 = CARTESIAN_POINT ( 'NONE',  ( 6.139501739389007007, 1.813922436357641388, -0.7475906808915923074 ) ) ;
#158318 = AXIS2_PLACEMENT_3D ( 'NONE', #107617, #73984, #7896 ) ;
#158319 = CARTESIAN_POINT ( 'NONE',  ( 0.7500000000000006661, 15.16666666666666785, -1.299038105676657340 ) ) ;
#158320 = CARTESIAN_POINT ( 'NONE',  ( -5.703176172842872482, 9.805455968292021041, 0.000000000000000000 ) ) ;
#158321 = CARTESIAN_POINT ( 'NONE',  ( 5.660692828905515839, 6.562895374266609849, -1.199719254218445830 ) ) ;
#158322 = CARTESIAN_POINT ( 'NONE',  ( 5.460537066722415567, -1.980877156148381335, -0.9378266216248376530 ) ) ;
#158323 = CARTESIAN_POINT ( 'NONE',  ( 5.359550796103802917, 5.147230771742885125, -0.7998128361456231517 ) ) ;
#158324 = CARTESIAN_POINT ( 'NONE',  ( 4.909070852169226562, -1.665950775781706028, 1.228889460859562854 ) ) ;
#158326 = CARTESIAN_POINT ( 'NONE',  ( -1.364683531250012516, 3.301041667008084879, -0.7879004041258289570 ) ) ;
#158325 = CARTESIAN_POINT ( 'NONE',  ( 0.000000000000000000, -2.500000000000002220, -0.6500000000000000222 ) ) ;
#158327 = ORIENTED_EDGE ( 'NONE', *, *, #86537, .T. ) ;
#158328 = CARTESIAN_POINT ( 'NONE',  ( 4.676596114989339803, 1.702786692269612212, 1.544373632959222586 ) ) ;
#158329 = CARTESIAN_POINT ( 'NONE',  ( 6.480434237652124452, 8.583592582059388576, 1.443375672974076540 ) ) ;
#158330 = CARTESIAN_POINT ( 'NONE',  ( 3.933273961740286317, 7.602920365423422311, 0.7216878364870257245 ) ) ;
#158331 = CARTESIAN_POINT ( 'NONE',  ( 0.6215105264332577706, -2.174887359234744633, 0.7243307227927602288 ) ) ;
#158332 = CARTESIAN_POINT ( 'NONE',  ( 6.620655732516644854, 4.701125524277991907, 2.388986273831222640 ) ) ;
#158333 = CARTESIAN_POINT ( 'NONE',  ( -5.399890319992785237, 9.521898816625391504, 0.7998128361456291469 ) ) ;
#158334 = CARTESIAN_POINT ( 'NONE',  ( 5.085854714555574141, -1.927481041573789744, -0.2360958376807794079 ) ) ;
#158335 = EDGE_LOOP ( 'NONE', ( #90129, #60065, #37568, #34809, #159151, #197934, #104206, #157397, #21283, #72479, #193094, #168699, #47442, #75523, #3401, #17685, #24735, #81097, #10393 ) ) ;
#158336 = CARTESIAN_POINT ( 'NONE',  ( 7.551528372687370094, 11.75394083486988528, -0.7216878364870267237 ) ) ;
#158337 = ORIENTED_EDGE ( 'NONE', *, *, #148852, .T. ) ;
#158338 = CARTESIAN_POINT ( 'NONE',  ( 5.273660385517703553, 0.3669835118517566497, -1.876681294024808988 ) ) ;
#158339 = CARTESIAN_POINT ( 'NONE',  ( 6.756889588843246308, -1.328954913838266361, 1.099249449767102593 ) ) ;
#158340 = CARTESIAN_POINT ( 'NONE',  ( 5.260953973667149342, -0.05432152012316109058, -2.015980820358989511 ) ) ;
#158342 = CARTESIAN_POINT ( 'NONE',  ( -3.024877669624710386, 6.543124691288523920, 0.000000000000000000 ) ) ;
#158341 = CARTESIAN_POINT ( 'NONE',  ( -9.450196763925152510, 10.98398329845622001, -1.199719254218441611 ) ) ;
#158343 = CARTESIAN_POINT ( 'NONE',  ( -1.642778471875000035, -2.355208332855376341, -2.845375778867859751 ) ) ;
#158345 = CARTESIAN_POINT ( 'NONE',  ( 0.08049558579637566824, -0.1306036352819762714, -1.740669940395103366 ) ) ;
#158344 = CARTESIAN_POINT ( 'NONE',  ( 1.710996362105126511, -0.2544465352872951613, 2.075019263894110733 ) ) ;
#158346 = CARTESIAN_POINT ( 'NONE',  ( 6.117814597332064785, 0.2004318333163370436, 2.006446488866588496 ) ) ;
#158348 = CARTESIAN_POINT ( 'NONE',  ( 3.328363117612358479, 2.236410206915816268, 0.5022841181492423424 ) ) ;
#158347 = CARTESIAN_POINT ( 'NONE',  ( 5.923986774528332333, 5.876015756563318426, -0.7998128361456481317 ) ) ;
#158349 = CARTESIAN_POINT ( 'NONE',  ( 2.237881400472482962, 0.3803048411740033719, 1.698081864755231374 ) ) ;
#158350 = CARTESIAN_POINT ( 'NONE',  ( 2.935903058640790597, -2.042584291827519660, 0.5695675404085094318 ) ) ;
#158351 = DIRECTION ( 'NONE',  ( -1.000000000000000000, 0.000000000000000000, 0.000000000000000000 ) ) ;
#158352 = CARTESIAN_POINT ( 'NONE',  ( 1.879855919261735675, -0.2174549385326445539, 1.720076089969482469 ) ) ;
#158353 = CARTESIAN_POINT ( 'NONE',  ( -1.360316468750036645, 1.901041667008058988, -0.7853790794159222211 ) ) ;
#158354 = CARTESIAN_POINT ( 'NONE',  ( 2.031498134000471190, 1.782053568523461751, -0.5365169527500669444 ) ) ;
#158355 = CARTESIAN_POINT ( 'NONE',  ( 2.752568609338637895, -2.165203543660359387, -0.1620229588487445971 ) ) ;
#158356 = CARTESIAN_POINT ( 'NONE',  ( 3.151577601795185757, 1.966304690962265234, -0.4465026806126579095 ) ) ;
#158357 = CARTESIAN_POINT ( 'NONE',  ( 3.687500000000002665, -1.451031289060967788, 1.451031289061265550 ) ) ;
#158358 = CARTESIAN_POINT ( 'NONE',  ( -1.500000000000015099, 1.160416667349484898, -0.8660254037844313801 ) ) ;
#158359 = CARTESIAN_POINT ( 'NONE',  ( 6.551400848983751857, -1.549099897634421685, -1.145107510758677893 ) ) ;
#158360 = CARTESIAN_POINT ( 'NONE',  ( -0.6823417656250003738, 14.90104166700806410, 1.181850606188754593 ) ) ;
#158361 = CARTESIAN_POINT ( 'NONE',  ( 3.111816671419795011, 1.753586859115576324, 1.363618078755132634 ) ) ;
#158362 = ORIENTED_EDGE ( 'NONE', *, *, #148860, .T. ) ;
#158363 = FILL_AREA_STYLE_COLOUR ( '', #174229 ) ;
#158364 = CARTESIAN_POINT ( 'NONE',  ( -1.500000000000015099, 0.1291666666666918539, -0.8660254037844383745 ) ) ;
#158365 = CARTESIAN_POINT ( 'NONE',  ( 9.237182729612253951, 9.671134694169463586, 0.7998128361456462443 ) ) ;
#158366 = CARTESIAN_POINT ( 'NONE',  ( 1.364683531249986537, -0.8864583329919110133, 0.7879004041258500513 ) ) ;
#158367 = CARTESIAN_POINT ( 'NONE',  ( 0.01275469579824477576, -2.220946917248843189, -0.04775700320917666830 ) ) ;
#158368 = CARTESIAN_POINT ( 'NONE',  ( 4.422284181769401634, 0.9229163912191931107, 1.731201473044992944 ) ) ;
#158370 = CARTESIAN_POINT ( 'NONE',  ( -6.575341312947811545, 6.773579074634973551, 1.040834085586084257E-14 ) ) ;
#158369 = CARTESIAN_POINT ( 'NONE',  ( 3.979481780810941949, 4.601482484822914998, 1.199719254218464037 ) ) ;
#158371 = EDGE_CURVE ( 'NONE', #109059, #46131, #32299, .T. ) ;
#158372 = SURFACE_STYLE_USAGE ( .BOTH. , #73912 ) ;
#158373 = CARTESIAN_POINT ( 'NONE',  ( 5.624405936800197736, 1.354097840178031475, -1.812292894430814094 ) ) ;
#158374 = CARTESIAN_POINT ( 'NONE',  ( 2.365751517750969146, -0.4541778970535991777, 2.011898661289913903 ) ) ;
#158375 = CARTESIAN_POINT ( 'NONE',  ( -4.720210035852093533, 8.658662141802762946, -0.7998128361456281477 ) ) ;
#158376 = ORIENTED_EDGE ( 'NONE', *, *, #115282, .F. ) ;
#158377 = CARTESIAN_POINT ( 'NONE',  ( -0.7500000000000215383, 1.972916667349486453, 1.299038105676659116 ) ) ;
#158378 = CARTESIAN_POINT ( 'NONE',  ( 4.165207536865437099, 0.2314014899743311315, -1.856129391651973215 ) ) ;
#158379 = CARTESIAN_POINT ( 'NONE',  ( 2.900671442982618142, -0.8568821622233543378, -1.507568437789049032 ) ) ;
#158380 = CARTESIAN_POINT ( 'NONE',  ( 6.550331612656306035, -1.695486744446069727, 1.388264742925699569 ) ) ;
#158381 = CARTESIAN_POINT ( 'NONE',  ( 0.4994150495197279271, 1.833458848295946186, -1.227822027206025179 ) ) ;
#158382 = CARTESIAN_POINT ( 'NONE',  ( 5.999939506776140519, -0.7010436009657755596, -1.811167765765375526 ) ) ;
#158383 = CARTESIAN_POINT ( 'NONE',  ( 6.902720145097990034, 15.44736672593548299, 9.761920446463546952 ) ) ;
#158384 = CARTESIAN_POINT ( 'NONE',  ( 0.6861729220449981348, 1.650083401500940239, 1.158686392676591570 ) ) ;
#158385 = CARTESIAN_POINT ( 'NONE',  ( 0.1586465271753433603, 2.115359532055087310, 0.1496401998123952359 ) ) ;
#158386 = CARTESIAN_POINT ( 'NONE',  ( 6.557263107265463020, -1.238491779027944162, 1.591905563659588907 ) ) ;
#158387 = CARTESIAN_POINT ( 'NONE',  ( -8.371269781434001800, 11.85389961405997816, -1.199719254218446718 ) ) ;
#158388 = CARTESIAN_POINT ( 'NONE',  ( 6.928380191783277908, 8.041863964290678624, 1.199719254218462483 ) ) ;
#158389 = CARTESIAN_POINT ( 'NONE',  ( 4.564971734551386717, -1.632036996880025903, -0.8184370388232551363 ) ) ;
#158390 = CARTESIAN_POINT ( 'NONE',  ( 2.380145745526092593, 1.357289424207007489, 1.739932290444376584 ) ) ;
#158391 = EDGE_LOOP ( 'NONE', ( #13569, #121262, #16466, #156129 ) ) ;
#158392 = CARTESIAN_POINT ( 'NONE',  ( -4.516274566683622815, 5.401980094953223066, 1.082531754730549078 ) ) ;
#158393 = CARTESIAN_POINT ( 'NONE',  ( 3.285556943750000514, -2.851041666188706802, 1.896917185911906500 ) ) ;
#158394 = CARTESIAN_POINT ( 'NONE',  ( -7.507464373665155399, 9.781794407407920389, 1.599625672291295375 ) ) ;
#158395 = CARTESIAN_POINT ( 'NONE',  ( 0.9494800659552645739, -1.824215446917340389, 0.8674010940010259407 ) ) ;
#158396 = CARTESIAN_POINT ( 'NONE',  ( 0.9999999999999833467, 6.468705557303653819, 4.925226524755080604 ) ) ;
#158397 = ORIENTED_EDGE ( 'NONE', *, *, #50862, .T. ) ;
#158398 = CARTESIAN_POINT ( 'NONE',  ( -4.716257332707368910, 6.595662536282280719, -1.599625672291271394 ) ) ;
#158399 = CARTESIAN_POINT ( 'NONE',  ( 2.834617457269935414, -1.779228943046967437, -0.5452927797432933765 ) ) ;
#158400 = CARTESIAN_POINT ( 'NONE',  ( 3.704402285031850539, 5.344888637335695414, -1.599625672291262513 ) ) ;
#158401 = CARTESIAN_POINT ( 'NONE',  ( 11.41381675112460847, 10.06983264508522424, 3.704697986577264235 ) ) ;
#158402 = VERTEX_POINT ( 'NONE', #16015 ) ;
#158403 = CARTESIAN_POINT ( 'NONE',  ( -8.616370316684697883, 10.01118577667568132, -1.199719254218446718 ) ) ;
#158404 = CARTESIAN_POINT ( 'NONE',  ( 4.072732355924274295, -1.704239406772959153, -0.6552279023967976235 ) ) ;
#158405 = AXIS2_PLACEMENT_3D ( 'NONE', #92262, #126949, #60790 ) ;
#158406 = CARTESIAN_POINT ( 'NONE',  ( -4.462568837553487100, 5.235360394347691404, -1.199719254218453823 ) ) ;
#158407 = CARTESIAN_POINT ( 'NONE',  ( 5.461903044330952639, 7.609029316319980474, -1.335476589331906494 ) ) ;
#158408 = CARTESIAN_POINT ( 'NONE',  ( 0.7547592729708142434, -1.719773315039843986, -0.2198852240756724863 ) ) ;
#158409 = CARTESIAN_POINT ( 'NONE',  ( 5.490138966579363178, -0.4511402564183407127, -1.784887083484905768 ) ) ;
#158410 = CARTESIAN_POINT ( 'NONE',  ( 4.143447727350758392, -2.008842960899869912, 1.135675674892607345 ) ) ;
#158411 = CARTESIAN_POINT ( 'NONE',  ( 4.960304097753311936, 6.880383762169266504, 1.599625672291268286 ) ) ;
#158412 = CARTESIAN_POINT ( 'NONE',  ( 0.5618817370758311114, 2.038728707766800596, -0.2996719410968719521 ) ) ;
#158413 = CARTESIAN_POINT ( 'NONE',  ( 2.032666248472639214, -1.733752323498815029, 0.8752225562490000277 ) ) ;
#158414 = CARTESIAN_POINT ( 'NONE',  ( 6.028750418185333082, 2.265939813929934488, -0.3841603865788502103 ) ) ;
#158415 = CARTESIAN_POINT ( 'NONE',  ( 0.7500000000000006661, 11.36458333401613174, 1.299038105676657340 ) ) ;
#158416 = CARTESIAN_POINT ( 'NONE',  ( -3.492107083971660586, 6.231819477012331632, 1.199719254218452935 ) ) ;
#158417 = CARTESIAN_POINT ( 'NONE',  ( 5.612129163471575310, -0.8422657237196762292, -1.670366365510121742 ) ) ;
#158418 = ORIENTED_EDGE ( 'NONE', *, *, #123084, .F. ) ;
#158420 = AXIS2_PLACEMENT_3D ( 'NONE', #163083, #147895, #50378 ) ;
#158419 = CIRCLE ( 'NONE', #203372, 11.00000000000000000 ) ;
#158422 = CARTESIAN_POINT ( 'NONE',  ( -5.255720823952942489, 6.160704378480398979, -1.199719254218453823 ) ) ;
#158421 = CARTESIAN_POINT ( 'NONE',  ( 2.953266587970606150, -1.684550232849800544, 0.9053361341156559439 ) ) ;
#158423 = CARTESIAN_POINT ( 'NONE',  ( 3.844505992619148937, 2.196175933995975438, 0.2170506636963928093 ) ) ;
#158424 = CARTESIAN_POINT ( 'NONE',  ( -0.6125000000000158096, 0.1041666673494701101, 1.060881119635906700 ) ) ;
#158425 = CARTESIAN_POINT ( 'NONE',  ( -10.46647149127475451, 4.016265686976439042, 5.778904458337481564 ) ) ;
#158426 = CARTESIAN_POINT ( 'NONE',  ( 6.021229617800532452, 6.197391773621639288, 0.000000000000000000 ) ) ;
#158427 = CARTESIAN_POINT ( 'NONE',  ( -5.546694241322218666, 8.524874810634301525, 1.082531754730550855 ) ) ;
#158428 = CARTESIAN_POINT ( 'NONE',  ( 2.081525663035548757, -0.1140690627178981842, -2.304871973535598251 ) ) ;
#158430 = EDGE_CURVE ( 'NONE', #6901, #53793, #44735, .T. ) ;
#158429 = CARTESIAN_POINT ( 'NONE',  ( 2.400770673373255448, 0.4268909467371252431, 1.914702609522442867 ) ) ;
#158431 = LINE ( 'NONE', #10032, #147797 ) ;
#158432 = CARTESIAN_POINT ( 'NONE',  ( 6.315292642669888323, -1.766025379077978741, -1.065358839237473099 ) ) ;
#158433 = CARTESIAN_POINT ( 'NONE',  ( 3.036663219780971978, 6.486598156479028709, -0.7216878364870267237 ) ) ;
#158434 = CARTESIAN_POINT ( 'NONE',  ( 3.837125247982266174, -1.679222704393277921, -1.116210984008485507 ) ) ;
#158435 = CARTESIAN_POINT ( 'NONE',  ( 5.065906673361608270, 5.939254536123854677, -1.199719254218450271 ) ) ;
#158436 = VERTEX_POINT ( 'NONE', #131971 ) ;
#158437 = CARTESIAN_POINT ( 'NONE',  ( 4.364470425680367249, -1.957169923074707274, -0.4852690807995581057 ) ) ;
#158438 = CARTESIAN_POINT ( 'NONE',  ( -9.996439331977562404, 10.55693406359564790, 0.7998128361456462443 ) ) ;
#158439 = CARTESIAN_POINT ( 'NONE',  ( 11.84668730067608244, 13.50636224908217287, 1.399999999999998357 ) ) ;
#158440 = DIRECTION ( 'NONE',  ( 0.000000000000000000, 0.000000000000000000, 1.000000000000000000 ) ) ;
#158441 = CARTESIAN_POINT ( 'NONE',  ( 8.536830278099042602, 13.11138575775759563, -0.7998128361456352531 ) ) ;
#158442 = CARTESIAN_POINT ( 'NONE',  ( 2.465899347143265086, -0.4792435138091205027, 2.117354166282244599 ) ) ;
#158443 = FILL_AREA_STYLE_COLOUR ( '', #107007 ) ;
#158444 = SURFACE_STYLE_USAGE ( .BOTH. , #23076 ) ;
#158445 = DIRECTION ( 'NONE',  ( -0.9840448990078773939, -0.1067521860439751419, 0.1423362480586335133 ) ) ;
#158446 = CARTESIAN_POINT ( 'NONE',  ( 2.108475139129362574, 1.389272611029747750, -1.252756881873963168 ) ) ;
#158447 = CARTESIAN_POINT ( 'NONE',  ( 0.2279051764371925748, -1.265926261136205211, -1.626655886597817124 ) ) ;
#158449 = CARTESIAN_POINT ( 'NONE',  ( 3.490040298073151526, 6.290063075088925260, 1.146788136912090250 ) ) ;
#158448 = CARTESIAN_POINT ( 'NONE',  ( 0.07775346131141079586, 1.298946786380944074, -2.537735853881052162 ) ) ;
#158450 = CARTESIAN_POINT ( 'NONE',  ( 1.364683531249986537, 0.4052083336747511200, -0.7879004041258309554 ) ) ;
#158451 = EDGE_CURVE ( 'NONE', #110599, #202706, #197981, .T. ) ;
#158452 = CARTESIAN_POINT ( 'NONE',  ( 2.877492880751183257, 0.2784179829431778219, -1.891769048003589138 ) ) ;
#158453 = AXIS2_PLACEMENT_3D ( 'NONE', #186207, #22629, #37841 ) ;
#158454 = CARTESIAN_POINT ( 'NONE',  ( 4.680378828550276538, -1.717002404052007325, -0.4286406472287905278 ) ) ;
#158455 = CARTESIAN_POINT ( 'NONE',  ( 1.400873256076972329, -0.2815782128867699852, -1.891321520182134286 ) ) ;
#158456 = CARTESIAN_POINT ( 'NONE',  ( -3.405069135326500351, 7.124331091189553433, 1.040834085586084257E-14 ) ) ;
#158457 = CARTESIAN_POINT ( 'NONE',  ( 6.485945863600712791, -1.915068438110486770, 0.05257573307166327897 ) ) ;
#158458 = CARTESIAN_POINT ( 'NONE',  ( 1.499999999999987121, 0.2541666666666844154, 0.8660254037844524744 ) ) ;
#158459 = CARTESIAN_POINT ( 'NONE',  ( 0.6255436495894195481, 0.2045281481408110225, -2.060252820462626477 ) ) ;
#158460 = CARTESIAN_POINT ( 'NONE',  ( 0.6823417656249882723, -0.8447916663252494907, 1.181850606188755259 ) ) ;
#158461 = VECTOR ( 'NONE', #11981, 1000.000000000000000 ) ;
#158462 = CARTESIAN_POINT ( 'NONE',  ( 5.700035372616791385, -1.870836310086241294, 0.001406584917262864625 ) ) ;
#158463 = CARTESIAN_POINT ( 'NONE',  ( 1.330379832379691818, 1.758967509726565792, 0.4888242021733391618 ) ) ;
#158465 = CARTESIAN_POINT ( 'NONE',  ( 4.604167169973131912, 8.362045362587558373, -0.1994984680026238300 ) ) ;
#158464 = CARTESIAN_POINT ( 'NONE',  ( 5.725267921653402148, -0.05769419298589681389, 2.206291853148376170 ) ) ;
#158466 = CARTESIAN_POINT ( 'NONE',  ( -0.6823417656250246877, -0.6989583329919113464, 1.181850606188755259 ) ) ;
#158467 = CARTESIAN_POINT ( 'NONE',  ( 2.576693429754982390, 1.349077690114818040, -1.560390594356737104 ) ) ;
#158468 = CARTESIAN_POINT ( 'NONE',  ( -5.852315862593199469, 9.979452273000736895, 0.7998128361456481317 ) ) ;
#158469 = CARTESIAN_POINT ( 'NONE',  ( 8.215351014876830504, 11.67199438640995801, -1.199719254218446718 ) ) ;
#158470 = CARTESIAN_POINT ( 'NONE',  ( 11.88237264505823987, 11.25677038468308844, -0.9087825512663076921 ) ) ;
#158471 = CARTESIAN_POINT ( 'NONE',  ( 0.2105424042340813540, -0.9235240298187572527, -1.952328634516012684 ) ) ;
#158472 = CARTESIAN_POINT ( 'NONE',  ( 7.828907357248368726, 8.098423103070084395, 0.7998128361456281477 ) ) ;
#158473 = ORIENTED_EDGE ( 'NONE', *, *, #139797, .F. ) ;
#158474 = CARTESIAN_POINT ( 'NONE',  ( 5.353992430378140099, -0.7485205528568983357, 1.930488744064068785 ) ) ;
#158475 = CARTESIAN_POINT ( 'NONE',  ( 0.6823417656249882723, 0.4052083336747516751, 1.181850606188755259 ) ) ;
#158476 = CARTESIAN_POINT ( 'NONE',  ( 2.970174626046933053, 1.153603175066318931, 1.827835936144058371 ) ) ;
#158477 = CARTESIAN_POINT ( 'NONE',  ( -4.900660301121059881, 8.037431844279481652, -0.9627648694432132670 ) ) ;
#158480 = ADVANCED_FACE ( 'NONE', ( #181724 ), #68366, .F. ) ;
#158479 = CARTESIAN_POINT ( 'NONE',  ( 2.383191274269541360, -0.003000794896521400724, 1.962046632024143866 ) ) ;
#158478 = CARTESIAN_POINT ( 'NONE',  ( 3.281903422188407138, 1.969933747823931380, -0.4446889725447465413 ) ) ;
#158481 = CARTESIAN_POINT ( 'NONE',  ( 6.720655732516644498, 4.691561721546229968, 2.636312907496433322 ) ) ;
#158482 = EDGE_CURVE ( 'NONE', #213643, #6267, #103615, .T. ) ;
#158485 = CARTESIAN_POINT ( 'NONE',  ( 6.643132081016117851, 8.773406732650713025, 1.443375672974076540 ) ) ;
#158484 = CARTESIAN_POINT ( 'NONE',  ( -1.737499999999997824, -0.6416666666666653862, 3.009438278150925683 ) ) ;
#158483 =( NAMED_UNIT ( * ) SI_UNIT ( $, .STERADIAN. ) SOLID_ANGLE_UNIT ( ) );
#158486 = CARTESIAN_POINT ( 'NONE',  ( -6.933015448541747006, 9.181880338089085214, 1.599625672291269396 ) ) ;
#158487 = CARTESIAN_POINT ( 'NONE',  ( 1.182827746461931229, 1.645757370610765102, -1.164989914844760444 ) ) ;
#158489 = CARTESIAN_POINT ( 'NONE',  ( 6.146043800834426918, 0.6857851511376764631, 2.081541312870714311 ) ) ;
#158488 = CARTESIAN_POINT ( 'NONE',  ( -6.389970470742427189, 6.349387058821269747, -0.7998128361456291469 ) ) ;
#158490 = DIRECTION ( 'NONE',  ( 1.039099362110107450E-15, 1.000000000000000000, -4.583713267641621330E-32 ) ) ;
#158491 = CARTESIAN_POINT ( 'NONE',  ( 5.097880177178074845, 1.288836597028759634, 1.412999258680311510 ) ) ;
#158492 = CARTESIAN_POINT ( 'NONE',  ( -3.898132859128961236, 4.506575409527250997, -1.199719254218452047 ) ) ;
#158493 = CARTESIAN_POINT ( 'NONE',  ( 6.602457619730771832, 6.805214765881779648, 0.7216878364870317197 ) ) ;
#158495 = CARTESIAN_POINT ( 'NONE',  ( 2.882435586221145485, -0.5880402899147363360, -1.928746874286999979 ) ) ;
#158494 = CARTESIAN_POINT ( 'NONE',  ( -10.12757755928392456, 10.91785469536048758, 0.7216878364870438212 ) ) ;
#158496 = CARTESIAN_POINT ( 'NONE',  ( -1.402160292154681736E-14, 14.23437500034139624, 1.575800808251682339 ) ) ;
#158497 = CARTESIAN_POINT ( 'NONE',  ( 4.911038474854160896, 1.501934305467259145, 0.8478258478515336982 ) ) ;
#158498 = CARTESIAN_POINT ( 'NONE',  ( 6.821687566331318564, 7.987665577921906568, 1.199719254218452935 ) ) ;
#158499 = CARTESIAN_POINT ( 'NONE',  ( 9.029367117021314115, 12.51771682229149008, -1.082531754730543083 ) ) ;
#158500 = CARTESIAN_POINT ( 'NONE',  ( -11.35573736746281348, 11.11270414413282204, -3.554362808847921773 ) ) ;
#158501 = CARTESIAN_POINT ( 'NONE',  ( 4.798043669735932326, -1.870115615568968881, -0.04763329477865811679 ) ) ;
#158502 = LINE ( 'NONE', #170469, #175106 ) ;
#158503 = CARTESIAN_POINT ( 'NONE',  ( 0.5673436759025469733, 1.799520464221905369, 1.023488823764052480 ) ) ;
#158504 = FACE_OUTER_BOUND ( 'NONE', #207131, .T. ) ;
#158505 = ORIENTED_EDGE ( 'NONE', *, *, #36355, .T. ) ;
#158506 = CARTESIAN_POINT ( 'NONE',  ( 6.569024019911770651, -1.395121139060730542, 1.155258474184825745 ) ) ;
#158507 = CARTESIAN_POINT ( 'NONE',  ( 3.067887898442204442, 6.801229324816399746, 0.7998128361456271485 ) ) ;
#158508 = FACE_OUTER_BOUND ( 'NONE', #168197, .T. ) ;
#158509 = CARTESIAN_POINT ( 'NONE',  ( 0.7206316775285178666, 1.371080193274256676, -1.184091668402836639 ) ) ;
#158510 = CARTESIAN_POINT ( 'NONE',  ( 5.600926855776875435, 7.627776979863398310, -1.443375672974078761 ) ) ;
#158511 = VECTOR ( 'NONE', #4569, 1000.000000000000227 ) ;
#158512 = CARTESIAN_POINT ( 'NONE',  ( 12.00020500325193318, 7.639630528669115073, -0.2084710905185198637 ) ) ;
#158513 = EDGE_LOOP ( 'NONE', ( #122636, #200847 ) ) ;
#158514 = CARTESIAN_POINT ( 'NONE',  ( 9.558135107509954764, 10.25350516829085379, -0.7216878364870257245 ) ) ;
#158516 = CARTESIAN_POINT ( 'NONE',  ( 8.372323551638698902, 9.726464550788689323, 1.199719254218462483 ) ) ;
#158515 = CARTESIAN_POINT ( 'NONE',  ( 0.3968290921660848070, 0.3316028935436679537, 1.933473477243151439 ) ) ;
#158517 = CARTESIAN_POINT ( 'NONE',  ( 4.745656728581866268, 1.894139079640380086, -0.2851870984255585051 ) ) ;
#158518 = CARTESIAN_POINT ( 'NONE',  ( 0.1747926744264660381, 0.006858446013176254172, -1.855468577918440776 ) ) ;
#158519 = DIRECTION ( 'NONE',  ( 0.000000000000000000, 0.000000000000000000, 1.000000000000000000 ) ) ;
#158520 = CARTESIAN_POINT ( 'NONE',  ( -10.33293948230774184, 2.515145635913770494, 5.518992160705051830 ) ) ;
#158522 = ORIENTED_EDGE ( 'NONE', *, *, #162808, .F. ) ;
#158521 = CARTESIAN_POINT ( 'NONE',  ( 4.853455804012222430, 5.725081861844796727, 1.082531754730560403 ) ) ;
#158523 = CARTESIAN_POINT ( 'NONE',  ( -7.863365906246048809, 12.11775129068834289, -0.7216878364870267237 ) ) ;
#158524 = CARTESIAN_POINT ( 'NONE',  ( 2.026462046419864826, 1.244889377058140845, -1.767065586814352773 ) ) ;
#158525 = CARTESIAN_POINT ( 'NONE',  ( -5.307090785106547415, 5.156303768904543894, -0.7998128361456362523 ) ) ;
#158526 = CARTESIAN_POINT ( 'NONE',  ( 6.373741612200160667, 9.489763409991955001, 1.082531754730549078 ) ) ;
#158527 = CARTESIAN_POINT ( 'NONE',  ( -4.464712657601869417, 4.103252943490596216, 0.7998128361456341429 ) ) ;
#158528 = CARTESIAN_POINT ( 'NONE',  ( 5.174738384962677351, -1.719472664011096219, -0.6136495084824307167 ) ) ;
#158529 = CARTESIAN_POINT ( 'NONE',  ( 8.995095802688167552, 12.46245326214662086, -7.469535370069887215 ) ) ;
#158530 = CARTESIAN_POINT ( 'NONE',  ( 0.7902269029948695289, -1.955937164205447054, -0.2457751801602201802 ) ) ;
#158531 = CARTESIAN_POINT ( 'NONE',  ( 3.375170810042011915, -1.688748480992762868, -0.8973671847329609541 ) ) ;
#158532 = ORIENTED_EDGE ( 'NONE', *, *, #137043, .F. ) ;
#158533 = CARTESIAN_POINT ( 'NONE',  ( -0.5773502691896470473, -2.500000000000002220, 0.9999999999999991118 ) ) ;
#158534 = CARTESIAN_POINT ( 'NONE',  ( 4.035575377323636026, 1.855309441653162139, -0.6614512482757756162 ) ) ;
#158535 = ORIENTED_EDGE ( 'NONE', *, *, #31832, .F. ) ;
#158536 = CARTESIAN_POINT ( 'NONE',  ( 5.759312517635055251, 1.912593682650292060, -0.3362288579709416525 ) ) ;
#158537 = ORIENTED_EDGE ( 'NONE', *, *, #60236, .T. ) ;
#158538 = CARTESIAN_POINT ( 'NONE',  ( -5.773793314573309132, 7.829454515125894964, 1.599625672291263179 ) ) ;
#158540 = CARTESIAN_POINT ( 'NONE',  ( 6.064709079624690524, 0.6667526090060638122, 2.013086243192941716 ) ) ;
#158539 = CARTESIAN_POINT ( 'NONE',  ( -5.971440312176176768, 5.931378217152456500, 0.000000000000000000 ) ) ;
#158541 = CARTESIAN_POINT ( 'NONE',  ( 6.821160681006788629, 8.091013894996997635, 1.082531754730549967 ) ) ;
#158542 = CARTESIAN_POINT ( 'NONE',  ( 4.354103434560454566, 0.8146061972254794448, -1.730223316255767196 ) ) ;
#158543 = B_SPLINE_CURVE_WITH_KNOTS ( 'NONE', 3,
 ( #146286, #125827, #79114, #9849, #113828, #75924, #76977, #94334 ),
 .UNSPECIFIED., .F., .F.,
 ( 4, 2, 2, 4 ),
 ( 0.000000000000000000, 0.0005156231957999833160, 0.0007734347936999757872, 0.001031246391599968367 ),
 .UNSPECIFIED. ) ;
#158544 = CARTESIAN_POINT ( 'NONE',  ( 2.905190055078214595, 6.611415174225076186, 0.7998128361456271485 ) ) ;
#158545 = CARTESIAN_POINT ( 'NONE',  ( 9.367496997597640984, 4.518459255873318092, -7.499999999999949374 ) ) ;
#158546 = CARTESIAN_POINT ( 'NONE',  ( 4.635406539864527886, -0.09663638271006223801, 2.010879464324326626 ) ) ;
#158547 = DIRECTION ( 'NONE',  ( 1.000000000000000000, 0.000000000000000000, 0.000000000000000000 ) ) ;
#158548 = CARTESIAN_POINT ( 'NONE',  ( 5.742758765878789085, 0.3605303665093100851, 1.789564367143759327 ) ) ;
#158549 = LINE ( 'NONE', #206211, #103213 ) ;
#158550 = CARTESIAN_POINT ( 'NONE',  ( 1.486871883557450591, 1.994755712061954123, 0.5540851298423480342 ) ) ;
#158551 = CARTESIAN_POINT ( 'NONE',  ( -6.762819695118240659, 6.784377820593065600, 0.7998128361456341429 ) ) ;
#158552 = AXIS2_PLACEMENT_3D ( 'NONE', #83424, #183060, #68223 ) ;
#158553 = CARTESIAN_POINT ( 'NONE',  ( -5.056216892478136771, 7.878110338051091510, -1.109312559570382550 ) ) ;
#158554 = CARTESIAN_POINT ( 'NONE',  ( -7.015401035077384329, 6.062865449010541141, -2.437084766375293921 ) ) ;
#158555 = CARTESIAN_POINT ( 'NONE',  ( 6.807498166657679484, -0.4075194142965676836, 1.832415718333743282 ) ) ;
#158556 = CARTESIAN_POINT ( 'NONE',  ( 4.950698647284403009, 8.927565521807144577, 1.040834085586084257E-14 ) ) ;
#158557 = CARTESIAN_POINT ( 'NONE',  ( -4.816538118508267630, 5.092449105792602460, -0.9495590845017554127 ) ) ;
#158558 = CARTESIAN_POINT ( 'NONE',  ( 4.082413651490639062, 7.776916670132135501, 0.000000000000000000 ) ) ;
#158559 = DIRECTION ( 'NONE',  ( 0.000000000000000000, 1.000000000000000000, 0.000000000000000000 ) ) ;
#158560 = CARTESIAN_POINT ( 'NONE',  ( -1.364683531250010295, 12.19270833367473195, 0.7879004041258445001 ) ) ;
#158561 = CARTESIAN_POINT ( 'NONE',  ( -4.436542580169821726, 6.199052314996659874, 1.599625672291267398 ) ) ;
#158563 = CARTESIAN_POINT ( 'NONE',  ( -5.108390017298964914, 9.181815130149269422, 0.000000000000000000 ) ) ;
#158562 = CARTESIAN_POINT ( 'NONE',  ( 6.849482339516208995, -6.938199013094656920, -6.234224025626343924 ) ) ;
#158564 = CARTESIAN_POINT ( 'NONE',  ( 5.080564943346563389, -0.6172752100359213401, 1.620779670503540659 ) ) ;
#158565 = CARTESIAN_POINT ( 'NONE',  ( -5.915435094264120508, 5.795762452929912101, 0.000000000000000000 ) ) ;
#158566 = TOROIDAL_SURFACE ( 'NONE', #99815, 0.4800000000000000933, 0.08000000000000000167 ) ;
#158567 = CARTESIAN_POINT ( 'NONE',  ( 2.623957243734816647, 2.031168598393529034, -0.3995267358143372860 ) ) ;
#158568 = CARTESIAN_POINT ( 'NONE',  ( 3.972345043000875098, -2.094467101900459483, -0.3087697250930310222 ) ) ;
#158569 = CARTESIAN_POINT ( 'NONE',  ( 8.426556166093362776, 9.789735934319136135, -1.199719254218446718 ) ) ;
#158570 = CARTESIAN_POINT ( 'NONE',  ( -1.364683531250010740, 3.780208333674751398, 0.7879004041258379498 ) ) ;
#158571 = CARTESIAN_POINT ( 'NONE',  ( 2.166797266485945617, 1.462705959888461971, -1.319016900598804831 ) ) ;
#158572 = CARTESIAN_POINT ( 'NONE',  ( 6.067817914410090552, 6.045155426100865981, -0.3955105627355664510 ) ) ;
#158573 = CARTESIAN_POINT ( 'NONE',  ( 4.256897045010922476, 5.029096643009940415, -1.082531754730548412 ) ) ;
#158575 = CARTESIAN_POINT ( 'NONE',  ( 11.92045683181315141, 12.44724072120514791, -1.382340670101858571 ) ) ;
#158574 = CARTESIAN_POINT ( 'NONE',  ( -3.475000000000000533, -1.049999999999998934, 0.000000000000000000 ) ) ;
#158576 = CARTESIAN_POINT ( 'NONE',  ( 4.189605479905995189, -0.8790709274306067744, 2.117190895528203498 ) ) ;
#158577 = CARTESIAN_POINT ( 'NONE',  ( 0.4162703231485806454, 1.261427835099769634, -1.320066674804179385 ) ) ;
#158578 = CARTESIAN_POINT ( 'NONE',  ( 6.261886844665240481, 8.398896966899865646, 1.599625672291268286 ) ) ;
#158579 = CARTESIAN_POINT ( 'NONE',  ( 6.982085920913413624, 8.208483664896217391, -1.082531754730543971 ) ) ;
#158580 = CARTESIAN_POINT ( 'NONE',  ( -7.537443334193545397, 10.88110209227943770, -1.199719254218446718 ) ) ;
#158581 = CARTESIAN_POINT ( 'NONE',  ( 1.916272853804147136, -2.012662139290276819, 0.05368196500972129831 ) ) ;
#158582 = CARTESIAN_POINT ( 'NONE',  ( 2.518345088137901477, 0.8342845254802437882, 1.775630740545742992 ) ) ;
#158583 = CARTESIAN_POINT ( 'NONE',  ( -7.914208982075130905, 10.25632978388623684, -1.599625672291263179 ) ) ;
#158584 = CARTESIAN_POINT ( 'NONE',  ( -7.413611068574208041, 7.543634422958360730, 0.7998128361456341429 ) ) ;
#158585 = CARTESIAN_POINT ( 'NONE',  ( 0.000000000000000000, 13.79999999999999893, 0.000000000000000000 ) ) ;
#158587 = CARTESIAN_POINT ( 'NONE',  ( 3.731107905939319735, -1.635417248454105854, 0.6770700851450436319 ) ) ;
#158586 = CARTESIAN_POINT ( 'NONE',  ( 4.998031443873323099, -0.7039345487453112504, -1.968691415026160962 ) ) ;
#158588 = CARTESIAN_POINT ( 'NONE',  ( -9.117697077659890681, 14.00000000000575007, 7.299999999991188204 ) ) ;
#158589 = CARTESIAN_POINT ( 'NONE',  ( 6.052705554163346768, -1.962971892542137553, -1.183510860282228405 ) ) ;
#158590 = CARTESIAN_POINT ( 'NONE',  ( 5.911982399937937949, 1.163873415549965262, -1.294066288734674997 ) ) ;
#158591 = EDGE_CURVE ( 'NONE', #173148, #64464, #165769, .T. ) ;
#158592 = CARTESIAN_POINT ( 'NONE',  ( 9.264299036839600987, 9.702770385934682551, -0.7998128361456281477 ) ) ;
#158593 = CARTESIAN_POINT ( 'NONE',  ( 6.047535252586548893, -1.628406021067085874, 1.622660289872903006 ) ) ;
#158594 = CARTESIAN_POINT ( 'NONE',  ( -1.737499999999997824, -1.297916665710750150, 3.009438278150925683 ) ) ;
#158595 = CARTESIAN_POINT ( 'NONE',  ( 5.219963594993116018, -1.465640877661518626, -0.9259742478883812300 ) ) ;
#158596 = CARTESIAN_POINT ( 'NONE',  ( 5.863789056686759871, -0.5331677977272324398, 2.104577851170267078 ) ) ;
#158597 = CARTESIAN_POINT ( 'NONE',  ( 0.000000000000000000, 13.49999999999999822, 0.000000000000000000 ) ) ;
#158598 = CARTESIAN_POINT ( 'NONE',  ( 0.1107727185766090999, 2.028241449780379568, 0.6078911015285259900 ) ) ;
#158599 = CARTESIAN_POINT ( 'NONE',  ( 5.812500000000003553, 1.451031289061346818, 1.451031289060879637 ) ) ;
#158600 = FACE_OUTER_BOUND ( 'NONE', #115146, .T. ) ;
#158601 = CARTESIAN_POINT ( 'NONE',  ( 3.856402372034730686, 0.6923319331257683507, 1.797858303039111982 ) ) ;
#158602 = CARTESIAN_POINT ( 'NONE',  ( 0.7500000000000006661, 11.19791666734946212, -1.299038105676657340 ) ) ;
#158603 = CARTESIAN_POINT ( 'NONE',  ( 0.4697634657386277612, -1.879787550458272394, -1.183196895768683365 ) ) ;
#158604 = ORIENTED_EDGE ( 'NONE', *, *, #8637, .F. ) ;
#158605 = CARTESIAN_POINT ( 'NONE',  ( 1.499999999999990896, 5.025000000000022560, 1.214306433183764966E-14 ) ) ;
#158606 = CARTESIAN_POINT ( 'NONE',  ( 4.904298879841284098, 6.744767997946721216, 1.599625672291267398 ) ) ;
#158607 = CARTESIAN_POINT ( 'NONE',  ( 5.621827251160867789, 9.710548892996357040, 1.040834085586084257E-14 ) ) ;
#158609 = EDGE_CURVE ( 'NONE', #45686, #133392, #10208, .T. ) ;
#158608 = VECTOR ( 'NONE', #131360, 1000.000000000000000 ) ;
#158610 = CARTESIAN_POINT ( 'NONE',  ( 2.526306204038858194, -2.196730012672935661, 0.3287970392919815632 ) ) ;
#158611 = DIRECTION ( 'NONE',  ( 8.638326563840809144E-31, 5.962633348652903386E-61, -1.000000000000000000 ) ) ;
#158612 = CARTESIAN_POINT ( 'NONE',  ( 6.995644074971448134, 7.263932296995902149, -0.7216878364870257245 ) ) ;
#158613 = EDGE_CURVE ( 'NONE', #23152, #197638, #159801, .T. ) ;
#158614 = CARTESIAN_POINT ( 'NONE',  ( -8.283668667825340393, 12.60810451253083997, 0.7216878364870458196 ) ) ;
#158615 = CARTESIAN_POINT ( 'NONE',  ( 7.078765600110826561, 8.391552967285011988, -1.082531754730548412 ) ) ;
#158616 = CARTESIAN_POINT ( 'NONE',  ( 1.072888940501380839, -0.9041080511620370741, 1.802418165037560138 ) ) ;
#158618 = CARTESIAN_POINT ( 'NONE',  ( 5.512196432965448700, 2.060465348046951917, -0.09781390707789237859 ) ) ;
#158617 = CARTESIAN_POINT ( 'NONE',  ( 7.228468454380276853, 11.58496363008569574, 1.040834085586084257E-14 ) ) ;
#158619 = CARTESIAN_POINT ( 'NONE',  ( -11.41176686791169281, 11.25950803486852081, 3.404018756831824533 ) ) ;
#158620 = CARTESIAN_POINT ( 'NONE',  ( -2.415323921528888196, 5.969628341758991930, 0.7998128361456341429 ) ) ;
#158621 = CARTESIAN_POINT ( 'NONE',  ( 7.471952054462754234, 8.850270497362297206, 1.082531754730549078 ) ) ;
#158622 = CARTESIAN_POINT ( 'NONE',  ( -3.059665831784952651E-14, 3.479999999999999538, 2.000000000000000000 ) ) ;
#158623 = CARTESIAN_POINT ( 'NONE',  ( -1.364683531250000748, 0.5093750003414208027, 0.000000000000000000 ) ) ;
#158624 = CARTESIAN_POINT ( 'NONE',  ( 0.2625039974461966241, -1.576774366707566433, -0.8037556782162450508 ) ) ;
#158625 = CARTESIAN_POINT ( 'NONE',  ( 5.871638708485903635, -0.2633594344273459398, -1.713904792762838136 ) ) ;
#158626 = CARTESIAN_POINT ( 'NONE',  ( 6.075711799444424521, -0.9231013878284710650, 1.475285791177717076 ) ) ;
#158627 = CARTESIAN_POINT ( 'NONE',  ( 3.562334897874219308, -1.538608923441080689, 1.699488912218325654 ) ) ;
#158628 = CARTESIAN_POINT ( 'NONE',  ( 1.364683531249986537, -0.3447916663252443836, -0.7879004041258309554 ) ) ;
#158629 = CARTESIAN_POINT ( 'NONE',  ( 1.780954670855667388, 1.268887097626215876, 1.334285251370644021 ) ) ;
#158630 = CARTESIAN_POINT ( 'NONE',  ( 8.289920859751990889, 11.75899253876431416, 1.199719254218450271 ) ) ;
#158631 = DIRECTION ( 'NONE',  ( 0.000000000000000000, -1.445602896647338917E-16, 1.000000000000000000 ) ) ;
#158632 = CARTESIAN_POINT ( 'NONE',  ( 2.783998052563033010, -0.9402290988879957734, 1.564698673013890984 ) ) ;
#158633 = CARTESIAN_POINT ( 'NONE',  ( 3.428361437285933455, -1.528740797599713153, -1.314997250469025936 ) ) ;
#158634 = CARTESIAN_POINT ( 'NONE',  ( -7.980945979938748103, 12.46285407657057220, 0.000000000000000000 ) ) ;
#158635 = CARTESIAN_POINT ( 'NONE',  ( -1.580000000000022276, 6.280000000000042881, 2.500000000000011102 ) ) ;
#158636 = CARTESIAN_POINT ( 'NONE',  ( 5.104563850188495344, -0.7068653695375884949, -1.983929190867816494 ) ) ;
#158637 = CARTESIAN_POINT ( 'NONE',  ( 9.571964790107170273, 13.80900892610533859, 8.297589824372789025 ) ) ;
#158638 = CARTESIAN_POINT ( 'NONE',  ( 2.893098739488662030, 0.2508700648995808025, 2.055025655848155886 ) ) ;
#158639 = CARTESIAN_POINT ( 'NONE',  ( 4.487912541323413329, 5.194651705420806564, 1.199719254218462483 ) ) ;
#158640 = CARTESIAN_POINT ( 'NONE',  ( -1.360316468750030428, 1.171875000341417117, -4.336808689942017736E-14 ) ) ;
#158641 = CARTESIAN_POINT ( 'NONE',  ( 4.723349490952149843, 1.845327050471495367, 1.044454997443218236 ) ) ;
#158642 = CARTESIAN_POINT ( 'NONE',  ( 1.207505077391484161, -0.4687122323817956571, 1.868500445134027466 ) ) ;
#158643 = EDGE_LOOP ( 'NONE', ( #152104, #43345, #173715, #118963 ) ) ;
#158644 = CARTESIAN_POINT ( 'NONE',  ( -5.679940009482361774, 5.591294530676332641, 0.7998128361456281477 ) ) ;
#158645 = CARTESIAN_POINT ( 'NONE',  ( 7.639129486296027061, 10.99973593639901814, 1.199719254218460707 ) ) ;
#158646 = CARTESIAN_POINT ( 'NONE',  ( 5.573810548549551491, 6.635772073796838200, -1.082531754730548412 ) ) ;
#158647 = CARTESIAN_POINT ( 'NONE',  ( -1.737500000000000266, -1.064583332377418090, -3.009438278150923907 ) ) ;
#158648 = CARTESIAN_POINT ( 'NONE',  ( -5.915435094264120508, 5.795762452929912101, 0.000000000000000000 ) ) ;
#158649 = CARTESIAN_POINT ( 'NONE',  ( 6.433838290133602200, -2.056603270127650429, 0.5165238393732355382 ) ) ;
#158650 = CARTESIAN_POINT ( 'NONE',  ( 1.817543918834242378, -0.2582919827684154179, 2.089997942319920199 ) ) ;
#158651 = CARTESIAN_POINT ( 'NONE',  ( -6.168033539574333979, 6.160736982450306876, 0.7998128361456281477 ) ) ;
#158652 = CARTESIAN_POINT ( 'NONE',  ( 7.938462636001388795, 9.220293482545153907, -1.199719254218441611 ) ) ;
#158653 = CARTESIAN_POINT ( 'NONE',  ( 6.666864641256595725, 1.379314998728842445, -1.249469950728621326 ) ) ;
#158654 = CARTESIAN_POINT ( 'NONE',  ( 7.962716289927667113, 8.184257181204083409, -0.7998128361456291469 ) ) ;
#158655 =( BOUNDED_CURVE ( )  B_SPLINE_CURVE ( 2, ( #168891, #188336, #122379, #8519, #71367 ),
 .UNSPECIFIED., .F., .T. ) 
 B_SPLINE_CURVE_WITH_KNOTS ( ( 3, 2, 3 ),
 ( 0.2851678736916871681, 0.2874999999999999778, 0.2884211393480570207 ),
 .UNSPECIFIED. ) 
 CURVE ( )  GEOMETRIC_REPRESENTATION_ITEM ( )  RATIONAL_B_SPLINE_CURVE ( ( 0.9339680269349972530, 0.9250130366848245966, 1.000000000000000000, 0.9703817746685905465, 0.9538591554679238804 ) ) 
 REPRESENTATION_ITEM ( '' )  );
#158656 = CARTESIAN_POINT ( 'NONE',  ( 11.86145016429273191, 10.19999999999999929, 1.099999999999996980 ) ) ;
#158657 = CARTESIAN_POINT ( 'NONE',  ( -4.014095998097799267, 6.840806543492835345, -1.199719254218450271 ) ) ;
#158658 = CARTESIAN_POINT ( 'NONE',  ( -9.029367117021344313, 9.636609179387466639, 0.7216878364870438212 ) ) ;
#158659 = CARTESIAN_POINT ( 'NONE',  ( 0.5629301599625028407, 0.6213668382478373386, 2.027498709647377773 ) ) ;
#158660 = CARTESIAN_POINT ( 'NONE',  ( 0.7641400526929170711, -4.157144623729202237, 0.6764706046374659998 ) ) ;
#158662 = CARTESIAN_POINT ( 'NONE',  ( 3.683996026499200660, -1.166640140252427793, -1.577160851978461009 ) ) ;
#158661 = CARTESIAN_POINT ( 'NONE',  ( -0.6125000000000262457, -0.5416666666666763996, -1.060881119635976200 ) ) ;
#158663 = CARTESIAN_POINT ( 'NONE',  ( 1.305796196612364124, -0.5247483525172502716, 2.096912610238470975 ) ) ;
#158665 = CARTESIAN_POINT ( 'NONE',  ( -6.136274411746873270, 5.997031558969919018, 0.08344787587596068368 ) ) ;
#158664 = CARTESIAN_POINT ( 'NONE',  ( -3.637330350216213759, 7.465578851886037093, -0.7998128361456481317 ) ) ;
#158666 = CARTESIAN_POINT ( 'NONE',  ( -1.364683531250012516, 2.238541667008087988, -0.7879004041258289570 ) ) ;
#158667 = CARTESIAN_POINT ( 'NONE',  ( 2.888294976258547475, 1.492474662269949182, -0.8948698564717886272 ) ) ;
#158668 = MECHANICAL_DESIGN_GEOMETRIC_PRESENTATION_REPRESENTATION (  '', ( #44419 ), #210440 ) ;
#158669 = CARTESIAN_POINT ( 'NONE',  ( 4.839897650398541806, 8.590371658866210680, 1.040834085586084257E-14 ) ) ;
#158670 = CARTESIAN_POINT ( 'NONE',  ( -11.30310531956832776, 5.150576456239970291, 5.742040133384030298 ) ) ;
#158671 = CARTESIAN_POINT ( 'NONE',  ( 2.495470048217228065, 1.954872899240958972, 0.4925676099705801891 ) ) ;
#158672 = CARTESIAN_POINT ( 'NONE',  ( 6.825078400183555161, 2.003297025668087983, 2.546134486959560572 ) ) ;
#158673 = CARTESIAN_POINT ( 'NONE',  ( -3.851398154733808088, 6.650992392901508232, -1.199719254218450271 ) ) ;
#158674 = CARTESIAN_POINT ( 'NONE',  ( 2.852367248507085229, 0.6625980423298013511, 1.856917580869015039 ) ) ;
#158676 = CARTESIAN_POINT ( 'NONE',  ( -4.963693636378939011, 8.805076652501815815, 0.7216878364870267237 ) ) ;
#158675 = CARTESIAN_POINT ( 'NONE',  ( 5.906500813101932756, -1.903809282439900219, -0.1807861040028224398 ) ) ;
#158677 = CARTESIAN_POINT ( 'NONE',  ( -5.980555156959541208, 7.110307450275150210, 1.082531754730549078 ) ) ;
#158678 = CARTESIAN_POINT ( 'NONE',  ( 4.701645408888975197, 8.707279753670952971, 0.000000000000000000 ) ) ;
#158679 = CARTESIAN_POINT ( 'NONE',  ( -6.038177310039794854, 8.137902509836795417, -1.599625672291271394 ) ) ;
#158680 = CARTESIAN_POINT ( 'NONE',  ( 1.717450570094357865, 1.680397536943441406, 1.120097702336475987 ) ) ;
#158681 = DIRECTION ( 'NONE',  ( -3.491481338843133750E-15, 0.000000000000000000, -1.000000000000000000 ) ) ;
#158682 = CARTESIAN_POINT ( 'NONE',  ( 5.684705870536221894, -2.249774798156725986, -0.5126945500162644054 ) ) ;
#158684 = EDGE_CURVE ( 'NONE', #140464, #123984, #194434, .T. ) ;
#158683 = CARTESIAN_POINT ( 'NONE',  ( 5.881297811770386907, -0.04968318840743202180, 1.961410508136133712 ) ) ;
#158685 = CARTESIAN_POINT ( 'NONE',  ( 3.502741298630154709, 0.4721981695934416856, 1.903977903881831191 ) ) ;
#158686 = CARTESIAN_POINT ( 'NONE',  ( 8.422639742587595180, 10.84949900448412130, -1.599625672291268286 ) ) ;
#158687 = CARTESIAN_POINT ( 'NONE',  ( 0.8619541869999207684, -0.05229984143813663777, -2.015912905633105101 ) ) ;
#158688 = ORIENTED_EDGE ( 'NONE', *, *, #35615, .F. ) ;
#158689 = CARTESIAN_POINT ( 'NONE',  ( 1.235738130824210357, 0.6087300624019938988, -2.027988197625143929 ) ) ;
#158691 = CARTESIAN_POINT ( 'NONE',  ( -5.208303565944065738, 9.228104593576741621, -0.7998128361456231517 ) ) ;
#158690 = CARTESIAN_POINT ( 'NONE',  ( -4.460796234096120472, 5.163016013655583158, 1.199719254218462483 ) ) ;
#158692 = CARTESIAN_POINT ( 'NONE',  ( 1.605144257462550517, -1.827384369528777031, 0.2241066044648756805 ) ) ;
#158693 = VERTEX_POINT ( 'NONE', #178201 ) ;
#158694 = CARTESIAN_POINT ( 'NONE',  ( 11.82867183089590135, 7.768921039415717544, 1.758246007359564933 ) ) ;
#158695 = CARTESIAN_POINT ( 'NONE',  ( 2.900754761704402274, -2.089926006748676457, -0.3584049868644647585 ) ) ;
#158696 = CARTESIAN_POINT ( 'NONE',  ( -1.001543065824772872E-14, 4.993750000682814161, 1.732050807568877637 ) ) ;
#158697 = CARTESIAN_POINT ( 'NONE',  ( 8.925345196497941558, 9.307324238869423283, 1.040834085586084257E-14 ) ) ;
#158698 = CARTESIAN_POINT ( 'NONE',  ( 7.700104897918568447, 7.948153567185284096, 0.000000000000000000 ) ) ;
#158699 = CARTESIAN_POINT ( 'NONE',  ( 2.794271844819782302, -2.055044804604218456, -0.1548302833056774130 ) ) ;
#158701 = CARTESIAN_POINT ( 'NONE',  ( 1.434833617064284805, -1.334073193498284793, -1.269287082821937362 ) ) ;
#158700 = CARTESIAN_POINT ( 'NONE',  ( -8.202846631467911820, 9.528741477256060577, 1.199719254218462483 ) ) ;
#158702 = CARTESIAN_POINT ( 'NONE',  ( 1.364683531249990311, 4.863541667008084879, 0.7879004041258500513 ) ) ;
#158703 = CARTESIAN_POINT ( 'NONE',  ( 1.446922511646519860, 4.325961798920477719, 0.4002501213623005927 ) ) ;
#158704 = DIRECTION ( 'NONE',  ( -1.000000000000000000, 0.000000000000000000, 0.000000000000000000 ) ) ;
#158705 =( BOUNDED_SURFACE ( )  B_SPLINE_SURFACE ( 3, 3, ( 
 ( #143487, #26483, #27555, #93651, #159694, #23262, #89374, #190050, #107812, #15551, #13433, #30779, #178089, #81638, #96858, #211624, #162906, #147723 ),
 ( #213740, #65363, #179155, #148778, #348, #14488, #146676, #210567, #212691, #95788, #112088, #131510, #113149, #197513, #80578, #97916, #66421, #64333 ),
 ( #114219, #94720, #82697, #132564, #28633, #130474, #111011, #29707, #163975, #196465, #44903, #31840, #161845, #16616, #45967, #48107, #49157, #115273 ),
 ( #177016, #160763, #181266, #79509, #32892, #145627, #98970, #195404, #165022, #63259, #194325, #12358, #47034, #180218, #78437, #144557, #62201, #128357 ),
 ( #129421, #199636, #2489, #19825, #85910, #200695, #151984, #52346, #186600, #18754, #51282, #37150, #202830, #35007, #54478, #117407, #67488, #17678 ),
 ( #1425, #133634, #102160, #21935, #183403, #53402, #38227, #101078, #68564, #167167, #198565, #182323, #118474, #84838, #150928, #33952, #5686, #134691 ),
 ( #3558, #184459, #104301, #136804, #36077, #116333, #169290, #168228, #166090, #69630, #135739, #201761, #86974, #119540, #149857, #120624, #185525, #103230 ) ),
 .UNSPECIFIED., .T., .F., .T. ) 
 B_SPLINE_SURFACE_WITH_KNOTS ( ( 4, 3, 4 ),
 ( 4, 2, 2, 2, 2, 2, 2, 2, 4 ),
 ( 0.000000000000000000, 0.5000000000000000000, 1.000000000000000000 ),
 ( 0.1651814497726892539, 0.1751754979096289411, 0.1851695460465686560, 0.2051576423204480859, 0.2251452996291458120, 0.2351391282834946750, 0.2401360426106691204, 0.2426344997742563292, 0.2451329569378435380 ),
 .UNSPECIFIED. ) 
 GEOMETRIC_REPRESENTATION_ITEM ( )  RATIONAL_B_SPLINE_SURFACE ( (
 ( 1.000000000000000000, 1.000000000000000000, 1.000000000000000000, 1.000000000000000000, 1.000000000000000000, 1.000000000000000000, 1.000000000000000000, 1.000000000000000000, 1.000000000000000000, 1.000000000000000000, 1.000000000000000000, 1.000000000000000000, 1.000000000000000000, 1.000000000000000000, 1.000000000000000000, 1.000000000000000000, 1.000000000000000000, 1.000000000000000000),
 ( 0.3333333333333333703, 0.3333333333333333703, 0.3333333333333333703, 0.3333333333333333703, 0.3333333333333333703, 0.3333333333333333703, 0.3333333333333333703, 0.3333333333333333703, 0.3333333333333333703, 0.3333333333333333703, 0.3333333333333333703, 0.3333333333333333703, 0.3333333333333333703, 0.3333333333333333703, 0.3333333333333333703, 0.3333333333333333703, 0.3333333333333333703, 0.3333333333333333703),
 ( 0.3333333333333333703, 0.3333333333333333703, 0.3333333333333333703, 0.3333333333333333703, 0.3333333333333333703, 0.3333333333333333703, 0.3333333333333333703, 0.3333333333333333703, 0.3333333333333333703, 0.3333333333333333703, 0.3333333333333333703, 0.3333333333333333703, 0.3333333333333333703, 0.3333333333333333703, 0.3333333333333333703, 0.3333333333333333703, 0.3333333333333333703, 0.3333333333333333703),
 ( 1.000000000000000000, 1.000000000000000000, 1.000000000000000000, 1.000000000000000000, 1.000000000000000000, 1.000000000000000000, 1.000000000000000000, 1.000000000000000000, 1.000000000000000000, 1.000000000000000000, 1.000000000000000000, 1.000000000000000000, 1.000000000000000000, 1.000000000000000000, 1.000000000000000000, 1.000000000000000000, 1.000000000000000000, 1.000000000000000000),
 ( 0.3333333333333333703, 0.3333333333333333703, 0.3333333333333333703, 0.3333333333333333703, 0.3333333333333333703, 0.3333333333333333703, 0.3333333333333333703, 0.3333333333333333703, 0.3333333333333333703, 0.3333333333333333703, 0.3333333333333333703, 0.3333333333333333703, 0.3333333333333333703, 0.3333333333333333703, 0.3333333333333333703, 0.3333333333333333703, 0.3333333333333333703, 0.3333333333333333703),
 ( 0.3333333333333333703, 0.3333333333333333703, 0.3333333333333333703, 0.3333333333333333703, 0.3333333333333333703, 0.3333333333333333703, 0.3333333333333333703, 0.3333333333333333703, 0.3333333333333333703, 0.3333333333333333703, 0.3333333333333333703, 0.3333333333333333703, 0.3333333333333333703, 0.3333333333333333703, 0.3333333333333333703, 0.3333333333333333703, 0.3333333333333333703, 0.3333333333333333703),
 ( 1.000000000000000000, 1.000000000000000000, 1.000000000000000000, 1.000000000000000000, 1.000000000000000000, 1.000000000000000000, 1.000000000000000000, 1.000000000000000000, 1.000000000000000000, 1.000000000000000000, 1.000000000000000000, 1.000000000000000000, 1.000000000000000000, 1.000000000000000000, 1.000000000000000000, 1.000000000000000000, 1.000000000000000000, 1.000000000000000000) ) ) 
 REPRESENTATION_ITEM ( '' )  SURFACE ( )  );
#158706 = AXIS2_PLACEMENT_3D ( 'NONE', #17886, #82908, #49363 ) ;
#158707 = CARTESIAN_POINT ( 'NONE',  ( 0.9618826090718561872, 0.4271145061440981272, -2.164990749644220447 ) ) ;
#158708 = CARTESIAN_POINT ( 'NONE',  ( 2.144175119285938180, 0.8672398327666650530, -2.089775168228876545 ) ) ;
#158709 = CARTESIAN_POINT ( 'NONE',  ( -9.192064960385334160, 9.826423329978791088, 0.7216878364870438212 ) ) ;
#158710 = CARTESIAN_POINT ( 'NONE',  ( 2.707043852439145581, 1.551706383644942289, -0.9346757785875584590 ) ) ;
#158711 = CARTESIAN_POINT ( 'NONE',  ( 3.098755142807321672, 1.734096097442457518, 0.8144269386064789673 ) ) ;
#158712 = CARTESIAN_POINT ( 'NONE',  ( 4.721179655770254335, -1.847879960204744432, -0.9338546512941485744 ) ) ;
#158713 = CARTESIAN_POINT ( 'NONE',  ( -1.364683531249997417, 3.321875000341423245, 1.214306433183764966E-14 ) ) ;
#158714 = CARTESIAN_POINT ( 'NONE',  ( 2.764479830724082543, -1.360639549628063882, 1.426867346614549836 ) ) ;
#158715 = CARTESIAN_POINT ( 'NONE',  ( 0.2703664580724125521, -1.260843473572888396, 1.456531361591931972 ) ) ;
#158716 = CARTESIAN_POINT ( 'NONE',  ( 4.047608660086319254, 0.6306619223146043840, -1.761260876548931709 ) ) ;
#158718 = CARTESIAN_POINT ( 'NONE',  ( 4.595652554671352696, 8.489339133230261680, -0.03962354257190832396 ) ) ;
#158717 = CARTESIAN_POINT ( 'NONE',  ( 1.875998176474055423, 2.207483416130914478, -0.6726682516732527262 ) ) ;
#158719 = CARTESIAN_POINT ( 'NONE',  ( 3.332308176975990577, -1.110599006344037853, 1.493168399320473627 ) ) ;
#158720 = CARTESIAN_POINT ( 'NONE',  ( -1.364683531249997417, 3.759375000341423689, 1.214306433183764966E-14 ) ) ;
#158721 = AXIS2_PLACEMENT_3D ( 'NONE', #193170, #8005, #74096 ) ;
#158722 = CARTESIAN_POINT ( 'NONE',  ( -5.447678794592645701, 5.250046769979851646, 0.000000000000000000 ) ) ;
#158723 = CARTESIAN_POINT ( 'NONE',  ( 4.937140493670735708, 8.911747675924535983, -0.7998128361456281477 ) ) ;
#158724 = CARTESIAN_POINT ( 'NONE',  ( -1.424678450204426516, 3.742891979394406210, 0.4927150456334949413 ) ) ;
#158725 = CARTESIAN_POINT ( 'NONE',  ( 0.3289212212809545788, 2.016005455721520345, 0.6092940615431781115 ) ) ;
#158726 = CARTESIAN_POINT ( 'NONE',  ( -1.201851678989727383E-14, 4.009375000341416140, -1.575800808251660134 ) ) ;
#158727 = CARTESIAN_POINT ( 'NONE',  ( 6.309879873373573922, -2.146112031266556919, 0.2576265230809087758 ) ) ;
#158729 = EDGE_CURVE ( 'NONE', #201530, #6442, #41333, .T. ) ;
#158728 = CARTESIAN_POINT ( 'NONE',  ( 0.1057309665696047341, 1.499486454312322525, 1.353398366655131246 ) ) ;
#158730 = CARTESIAN_POINT ( 'NONE',  ( 0.6823417656249864960, -0.5739583329919112353, -1.181850606188749264 ) ) ;
#158731 = CARTESIAN_POINT ( 'NONE',  ( -5.599154252763867134, 5.634694171087028636, 0.000000000000000000 ) ) ;
#158732 = EDGE_CURVE ( 'NONE', #32900, #57699, #179689, .T. ) ;
#158735 = CARTESIAN_POINT ( 'NONE',  ( 4.202664430556257713, 4.965825259479493603, 1.082531754730560403 ) ) ;
#158734 = CARTESIAN_POINT ( 'NONE',  ( -3.285556943750000514, -0.8385416661887076240, -1.896917185911906500 ) ) ;
#158733 = CARTESIAN_POINT ( 'NONE',  ( 6.886615681098613884, 6.999082814228660077, 0.000000000000000000 ) ) ;
#158736 = CARTESIAN_POINT ( 'NONE',  ( -4.248501033035892327, 6.049946853332221153, -1.599625672291271394 ) ) ;
#158737 = CARTESIAN_POINT ( 'NONE',  ( 4.505092375653735992, -0.09411930587044713137, 2.014432893821124004 ) ) ;
#158739 = CARTESIAN_POINT ( 'NONE',  ( -7.715998819508785189, 8.174622508947939181, -0.7216878364870338292 ) ) ;
#158738 = CARTESIAN_POINT ( 'NONE',  ( -8.012505595996376684, 12.29174759539704986, 0.000000000000000000 ) ) ;
#158740 =( LENGTH_UNIT ( ) NAMED_UNIT ( * ) SI_UNIT ( .MILLI., .METRE. ) );
#158742 = CARTESIAN_POINT ( 'NONE',  ( -1.364683531250014514, 10.33854166700806587, -0.7879004041258335089 ) ) ;
#158741 = CARTESIAN_POINT ( 'NONE',  ( 6.227428301493934448, -2.037140905555033576, 0.7235935974677574212 ) ) ;
#158743 = CARTESIAN_POINT ( 'NONE',  ( -8.611400122974211868, 13.19838391011195888, 1.040834085586084257E-14 ) ) ;
#158745 = CARTESIAN_POINT ( 'NONE',  ( 6.169546029190325243, 1.392557221580101423, 1.458547251757099650 ) ) ;
#158744 = CARTESIAN_POINT ( 'NONE',  ( -7.510853911846401942, 7.865010440016681592, 1.040834085586084257E-14 ) ) ;
#158746 = CARTESIAN_POINT ( 'NONE',  ( -1.364683531250012516, 0.8427083336747532849, 0.7879004041258379498 ) ) ;
#158747 = CARTESIAN_POINT ( 'NONE',  ( 0.4373225248172846746, -5.223431457505083308, 10.96785329849814694 ) ) ;
#158748 = CARTESIAN_POINT ( 'NONE',  ( 11.94105721237523277, 10.90000000000000036, 1.187919463087248273 ) ) ;
#158749 = CARTESIAN_POINT ( 'NONE',  ( 1.295042460130943152, 1.303850460046240833, 1.129354085073847491 ) ) ;
#158750 = CARTESIAN_POINT ( 'NONE',  ( 6.749980374757213575, 8.968339418673846097, 1.599625672291268286 ) ) ;
#158751 = CARTESIAN_POINT ( 'NONE',  ( 4.505052181490820651, 8.477920988373101707, -0.7998128361456381397 ) ) ;
#158752 = AXIS2_PLACEMENT_3D ( 'NONE', #85373, #167690, #99496 ) ;
#158753 = CARTESIAN_POINT ( 'NONE',  ( -1.364683531250014514, -0.6572916663252459379, 0.7879004041258379498 ) ) ;
#158754 = CARTESIAN_POINT ( 'NONE',  ( 0.8074156707096367125, -1.761990802586909766, 0.1653023320123351292 ) ) ;
#158755 = CARTESIAN_POINT ( 'NONE',  ( 2.192043262494451916, 1.240095455230303401, 1.585687145212981042 ) ) ;
#158756 = CARTESIAN_POINT ( 'NONE',  ( 2.806174607904299734, 5.257325561654889512, -1.082531754730543083 ) ) ;
#158757 = CARTESIAN_POINT ( 'NONE',  ( 4.120313900606538127, -1.131812998600056241, -1.894281110011143632 ) ) ;
#158758 = CARTESIAN_POINT ( 'NONE',  ( 5.682552277248558603, 1.299237613850280360, -1.739252610423980938 ) ) ;
#158759 = ORIENTED_EDGE ( 'NONE', *, *, #131446, .T. ) ;
#158760 = CARTESIAN_POINT ( 'NONE',  ( 1.499999999999987566, -0.2249999999999821587, 0.000000000000000000 ) ) ;
#158761 = CARTESIAN_POINT ( 'NONE',  ( 8.066738210006674237, 11.39464976410773467, 1.082531754730558626 ) ) ;
#158763 = CARTESIAN_POINT ( 'NONE',  ( 2.355092412869797869, 0.09611577090188135053, -2.014234804981252847 ) ) ;
#158762 = CARTESIAN_POINT ( 'NONE',  ( 3.545663791850160784, -1.958584582392399742, 0.8131309587096480218 ) ) ;
#158765 = ORIENTED_EDGE ( 'NONE', *, *, #183072, .F. ) ;
#158764 = CARTESIAN_POINT ( 'NONE',  ( 3.375094514129430845, -1.600109896321648462, -0.8493348278759412784 ) ) ;
#158766 = CARTESIAN_POINT ( 'NONE',  ( 5.712781623311797397, 7.758274208654143855, -1.599625672291283607 ) ) ;
#158767 = VERTEX_POINT ( 'NONE', #63374 ) ;
#158768 = CARTESIAN_POINT ( 'NONE',  ( 0.2154177506630133854, -1.835460468737951878, 0.3602540799089171131 ) ) ;
#158769 = EDGE_CURVE ( 'NONE', #49308, #139590, #16993, .T. ) ;
#158770 = CARTESIAN_POINT ( 'NONE',  ( 5.690036971771410101, -0.8169618954828453683, 1.632782195682795257 ) ) ;
#158772 = CARTESIAN_POINT ( 'NONE',  ( 1.112342557844925750, 1.847186106069747646, 0.5076494344821417259 ) ) ;
#158771 = CARTESIAN_POINT ( 'NONE',  ( -3.144601563365788444, 5.756120026313656268, -1.199719254218452935 ) ) ;
#158773 = CARTESIAN_POINT ( 'NONE',  ( -9.587917471435847716, 4.026361754648488223, -6.670783315233271615 ) ) ;
#158774 = CARTESIAN_POINT ( 'NONE',  ( -1.364683531250014514, 1.801041667008085767, -0.7879004041258289570 ) ) ;
#158775 = FILL_AREA_STYLE_COLOUR ( '', #81182 ) ;
#158776 = CARTESIAN_POINT ( 'NONE',  ( 7.024532985656128936, 9.288650798055913427, 1.443375672974065660 ) ) ;
#158777 = CARTESIAN_POINT ( 'NONE',  ( -4.502716413514296079, 8.267269892493059658, -0.7216878364870338292 ) ) ;
#158778 = CARTESIAN_POINT ( 'NONE',  ( -5.641074431737709283, 8.738948049406083385, -1.199719254218452047 ) ) ;
#158779 = CARTESIAN_POINT ( 'NONE',  ( 3.340189922722580196, -1.266226476691566738, -1.700888996046201029 ) ) ;
#158781 = CARTESIAN_POINT ( 'NONE',  ( -10.78402850230606447, 8.013881820625746499, 4.046242669647421408 ) ) ;
#158780 = CARTESIAN_POINT ( 'NONE',  ( -0.1298852118744100725, 0.003815113116375101580, -1.726395881205537330 ) ) ;
#158782 = CARTESIAN_POINT ( 'NONE',  ( 4.727780648284140241, -1.210341919374293473, -1.556009220651358715 ) ) ;
#158783 = CARTESIAN_POINT ( 'NONE',  ( 6.099862406061942188, 1.323743610676546334, 1.380425988546908567 ) ) ;
#158784 = ORIENTED_EDGE ( 'NONE', *, *, #170968, .T. ) ;
#158785 = CARTESIAN_POINT ( 'NONE',  ( 0.3162073025194310771, 1.084344979787469354, -1.818339158833045976 ) ) ;
#158786 = CARTESIAN_POINT ( 'NONE',  ( 7.322686252399450701, 14.46639250110529673, 9.509740026712064420 ) ) ;
#158787 = CARTESIAN_POINT ( 'NONE',  ( 1.100149375694438714, 0.8407228983892693908, -1.892171374333020406 ) ) ;
#158788 = CARTESIAN_POINT ( 'NONE',  ( 3.011592816664434569, -0.9578117005206161494, -1.689242170645321339 ) ) ;
#158789 = ORIENTED_EDGE ( 'NONE', *, *, #204906, .F. ) ;
#158790 = CARTESIAN_POINT ( 'NONE',  ( 4.355912491740495440, 8.303924683664389406, 0.000000000000000000 ) ) ;
#158791 = CARTESIAN_POINT ( 'NONE',  ( 5.189738938980948291, 9.276722205444929870, 0.000000000000000000 ) ) ;
#158793 = CARTESIAN_POINT ( 'NONE',  ( 6.667912619822566000, 6.673652899414787676, 1.040834085586084257E-14 ) ) ;
#158792 = CARTESIAN_POINT ( 'NONE',  ( 3.222686667372671732, 0.05170946606813638102, 2.090169120961588245 ) ) ;
#158794 = CARTESIAN_POINT ( 'NONE',  ( 4.136646265500957043, 5.919449624541475607, -1.443375672974068769 ) ) ;
#158796 = ORIENTED_EDGE ( 'NONE', *, *, #13528, .T. ) ;
#158795 = CARTESIAN_POINT ( 'NONE',  ( 0.6624192275643402406, 0.5246805835648783445, 1.733790746550630146 ) ) ;
#158797 = CARTESIAN_POINT ( 'NONE',  ( 5.180388087185870738, -1.228261608319089149, 1.833297759731546073 ) ) ;
#158798 = AXIS2_PLACEMENT_3D ( 'NONE', #193080, #198397, #182148 ) ;
#158799 = FACE_OUTER_BOUND ( 'NONE', #82706, .T. ) ;
#158800 = CARTESIAN_POINT ( 'NONE',  ( 3.294164632606086940, -0.8960083017303889230, 2.016869484631748310 ) ) ;
#158801 = CARTESIAN_POINT ( 'NONE',  ( 8.932124273304774320, 9.315233161810734686, 0.7998128361456462443 ) ) ;
#158802 = DIRECTION ( 'NONE',  ( 0.000000000000000000, 0.000000000000000000, -1.000000000000000000 ) ) ;
#158803 = CARTESIAN_POINT ( 'NONE',  ( 1.787617358713189386, 1.829539840090635749, -0.5563488465884156575 ) ) ;
#158804 = CARTESIAN_POINT ( 'NONE',  ( 7.750457368506414646, 12.19395069656619945, 0.7998128361456462443 ) ) ;
#158805 = CARTESIAN_POINT ( 'NONE',  ( 4.967269779104159788, 1.799668380515654142, 1.023422521214325309 ) ) ;
#158806 = EDGE_CURVE ( 'NONE', #45318, #201145, #182525, .T. ) ;
#158808 = CARTESIAN_POINT ( 'NONE',  ( 3.063507763784904192, 0.3185916186679502715, -2.137983152197140413 ) ) ;
#158807 = CARTESIAN_POINT ( 'NONE',  ( 9.623628927379545672, -9.094708467121352058, -0.4567741993462098860 ) ) ;
#158809 = CARTESIAN_POINT ( 'NONE',  ( 4.722331747100577459, 2.097238624054961864, 0.6360808509995665716 ) ) ;
#158810 = ORIENTED_EDGE ( 'NONE', *, *, #64709, .F. ) ;
#158811 = CIRCLE ( 'NONE', #117283, 0.08000000000000020983 ) ;
#158812 = DIRECTION ( 'NONE',  ( 1.000000000000000000, 0.000000000000000000, 0.000000000000000000 ) ) ;
#158813 = CARTESIAN_POINT ( 'NONE',  ( -9.512045263456270661, -8.176568542494905500, 0.4655551865852137206 ) ) ;
#158814 = CARTESIAN_POINT ( 'NONE',  ( 9.499386779316314033, -9.999529051968279347, -0.1207253440361106545 ) ) ;
#158815 = CARTESIAN_POINT ( 'NONE',  ( 3.736153849017632922, 6.516540702899320081, -1.199719254218453823 ) ) ;
#158816 = CARTESIAN_POINT ( 'NONE',  ( 1.586093632162032474, -3.231214742333746059, 2.878102786335113183 ) ) ;
#158817 = FACE_OUTER_BOUND ( 'NONE', #13908, .T. ) ;
#158818 = CARTESIAN_POINT ( 'NONE',  ( -8.107412671292051343, 10.48173408797264194, 1.443375672974090751 ) ) ;
#158819 = CARTESIAN_POINT ( 'NONE',  ( 5.037736595929563244, 8.035053907629919223, -1.199719254218452047 ) ) ;
#158820 = CARTESIAN_POINT ( 'NONE',  ( 6.332887962430945983, -1.963924782908726296, -0.6550794379977520343 ) ) ;
#158821 = CARTESIAN_POINT ( 'NONE',  ( 4.828697303143684394, 1.844096510799615674, 0.5574245839122073942 ) ) ;
#158822 = CARTESIAN_POINT ( 'NONE',  ( 6.380470236391142080, -0.5646626916907444560, -2.040458243955853401 ) ) ;
#158823 = SURFACE_STYLE_FILL_AREA ( #58118 ) ;
#158824 = CARTESIAN_POINT ( 'NONE',  ( 5.983225862332436584, 5.874851682342960402, 0.7998128361456341429 ) ) ;
#158825 = CARTESIAN_POINT ( 'NONE',  ( 5.346851039111033543, 6.199209027673978412, -1.009771797811720884 ) ) ;
#158826 = CARTESIAN_POINT ( 'NONE',  ( 4.996905641018499544, 0.3326216897534995387, 1.940969171785451364 ) ) ;
#158827 = CARTESIAN_POINT ( 'NONE',  ( 0.2346725361867564585, 0.3788711812165134196, 2.158297013397599162 ) ) ;
#158828 = CARTESIAN_POINT ( 'NONE',  ( 4.846238042176662653, 1.821038859956089606, 0.1311717439725426648 ) ) ;
#158829 = CARTESIAN_POINT ( 'NONE',  ( 7.539742822975472158, 7.968990512992423447, -0.7216878364870317197 ) ) ;
#158830 = CARTESIAN_POINT ( 'NONE',  ( 3.673896439178923057, 5.309298483840612093, 1.443375672974066548 ) ) ;
#158831 = CARTESIAN_POINT ( 'NONE',  ( -5.655686355556086120, 6.627330832017406692, 1.199719254218452935 ) ) ;
#158832 = CARTESIAN_POINT ( 'NONE',  ( 4.583538449871731757, 7.505156070562471804, 1.199719254218451159 ) ) ;
#158833 = VERTEX_POINT ( 'NONE', #30891 ) ;
#158835 = CARTESIAN_POINT ( 'NONE',  ( 5.818613517226002507, -0.7285450932710479943, -1.876915101588324974 ) ) ;
#158834 = CARTESIAN_POINT ( 'NONE',  ( 2.647807870277216757, 0.6224553824519338807, 1.732961026760751366 ) ) ;
#158836 = CARTESIAN_POINT ( 'NONE',  ( 1.265469760322552206, -2.298542322993640141, 0.001328286606278733300 ) ) ;
#158837 = CARTESIAN_POINT ( 'NONE',  ( 5.366048076001885825, -1.952644961629325548, 0.1885061251027941032 ) ) ;
#158838 = CARTESIAN_POINT ( 'NONE',  ( -6.417086777969760902, 6.381022750586497594, 0.7998128361456341429 ) ) ;
#158839 = CARTESIAN_POINT ( 'NONE',  ( -5.977437402589944604, 6.146301162042552058, -0.1694826866821088351 ) ) ;
#158840 = CARTESIAN_POINT ( 'NONE',  ( -4.298098390732130625, 4.973201863064262263, 1.199719254218462483 ) ) ;
#158841 = CARTESIAN_POINT ( 'NONE',  ( 0.7134375191242479097, -1.748147108003229810, -1.108949491591210146 ) ) ;
#158842 = CARTESIAN_POINT ( 'NONE',  ( -5.632486471834530661, 5.535932070087196344, -0.7998128361456362523 ) ) ;
#158844 = CARTESIAN_POINT ( 'NONE',  ( 6.649276393164253562, -1.424495517243940856, -1.050074490644896441 ) ) ;
#158843 = CARTESIAN_POINT ( 'NONE',  ( 1.189138979623612480, 1.585436599910443611, 1.363068659274695893 ) ) ;
#158845 = CARTESIAN_POINT ( 'NONE',  ( 0.1638468497727625650, 7.035416012003046227, -1.994423973928960869 ) ) ;
#158846 = CARTESIAN_POINT ( 'NONE',  ( 0.6823417656249917140, 3.405208333674754506, 1.181850606188765695 ) ) ;
#158847 = CARTESIAN_POINT ( 'NONE',  ( 1.610509732637079638, -0.2130687159686726062, 1.727248725346673952 ) ) ;
#158848 = CARTESIAN_POINT ( 'NONE',  ( 6.094553744542824170, 7.069066442510145265, 1.199719254218462483 ) ) ;
#158850 = CARTESIAN_POINT ( 'NONE',  ( 1.555203039002687859, 8.692270211428450466, 2.503634413632319866 ) ) ;
#158849 = CYLINDRICAL_SURFACE ( 'NONE', #16890, 1.500000000000000222 ) ;
#158851 = CARTESIAN_POINT ( 'NONE',  ( 2.314726122855132129, 1.540323329518531903, 0.7764098835694576151 ) ) ;
#158852 = CARTESIAN_POINT ( 'NONE',  ( 2.437293137456029157, -1.626093413141915134, -1.469474007205706645 ) ) ;
#158853 = CARTESIAN_POINT ( 'NONE',  ( 5.303435803989668074, 1.802500012205746183, 1.273053691228965389 ) ) ;
#158854 = CARTESIAN_POINT ( 'NONE',  ( -10.32649671959996596, 5.020010808682577874, -7.354824260697566451 ) ) ;
#158855 = VECTOR ( 'NONE', #50968, 1000.000000000000000 ) ;
#158856 = CARTESIAN_POINT ( 'NONE',  ( 2.922911270491454161, -1.500192211782652718, 1.569583652781519012 ) ) ;
#158857 = CARTESIAN_POINT ( 'NONE',  ( 1.330379832379691818, 1.758967509726565792, 0.4888242021733391618 ) ) ;
#158858 = CARTESIAN_POINT ( 'NONE',  ( 3.450509668567053545, -1.418736885945747428, 1.571922360790501738 ) ) ;
#158859 = DIRECTION ( 'NONE',  ( 0.9885327375000381167, 0.000000000000000000, -0.1510067114093955609 ) ) ;
#158860 = ORIENTED_EDGE ( 'NONE', *, *, #33468, .T. ) ;
#158862 = CARTESIAN_POINT ( 'NONE',  ( -1.201851678989727383E-14, 1.384375000341419693, 1.575800808251672791 ) ) ;
#158861 = CARTESIAN_POINT ( 'NONE',  ( 3.878722286802076535, -0.2252994024176681598, -2.281293266731793778 ) ) ;
#158863 = CARTESIAN_POINT ( 'NONE',  ( 11.86239285000045740, 12.21999999999998288, 1.812080536912751061 ) ) ;
#158864 = CARTESIAN_POINT ( 'NONE',  ( 4.539282502477016479, 4.190251095844947926, 0.7998128361456341429 ) ) ;
#158865 = EDGE_CURVE ( 'NONE', #214101, #194102, #110057, .T. ) ;
#158866 = CARTESIAN_POINT ( 'NONE',  ( 6.270221287042929248, 2.215581787426896376, -0.1604564985231044516 ) ) ;
#158867 = CARTESIAN_POINT ( 'NONE',  ( -4.433153041988574294, 8.115836282387899558, 1.040834085586084257E-14 ) ) ;
#158868 = CARTESIAN_POINT ( 'NONE',  ( 4.582292731738905722, 5.408724944192588424, -1.082531754730548412 ) ) ;
#158869 = CARTESIAN_POINT ( 'NONE',  ( -6.141480396866151992, 9.148515648777049591, 1.082531754730548412 ) ) ;
#158870 = CARTESIAN_POINT ( 'NONE',  ( 3.607878275012313285, 6.262922849939428716, 1.082531754730549078 ) ) ;
#158871 = ORIENTED_EDGE ( 'NONE', *, *, #53693, .F. ) ;
#158872 = CARTESIAN_POINT ( 'NONE',  ( 3.990861413484114273, -2.010826503599131065, 0.1511389102963680842 ) ) ;
#158874 = CARTESIAN_POINT ( 'NONE',  ( 2.096602096640389767, 2.039512422605322950, 0.3069443246750125365 ) ) ;
#158873 = CARTESIAN_POINT ( 'NONE',  ( 6.124532705071213279, 8.168374127381657246, -1.599625672291262513 ) ) ;
#158875 = CARTESIAN_POINT ( 'NONE',  ( 7.180978637093494044, 8.406838493811077839, -1.199719254218452047 ) ) ;
#158876 = CARTESIAN_POINT ( 'NONE',  ( 3.553645660113312399, 7.160020680191912845, -1.734723475976807094E-15 ) ) ;
#158877 = CARTESIAN_POINT ( 'NONE',  ( -3.285556943749998737, -3.930208332855377407, 1.896917185911908499 ) ) ;
#158878 = CARTESIAN_POINT ( 'NONE',  ( -1.001543065824772872E-14, 5.071875000341421469, 1.575800808251672791 ) ) ;
#158879 = CARTESIAN_POINT ( 'NONE',  ( 5.103566685217446164, -2.181124530238859993, 0.2125310249164805709 ) ) ;
#158880 = CARTESIAN_POINT ( 'NONE',  ( 3.832657856672664565, 0.6767144645295587457, -1.899618369658891748 ) ) ;
#158881 = CARTESIAN_POINT ( 'NONE',  ( 2.261056740009634414, 1.805359621025553363, -0.3608742708730780513 ) ) ;
#158882 = CARTESIAN_POINT ( 'NONE',  ( 5.445571254183207088, 9.504916896522420444, -0.7998128361456281477 ) ) ;
#158884 = EDGE_CURVE ( 'NONE', #91043, #151085, #14599, .T. ) ;
#158883 = FILL_AREA_STYLE ('',( #39802 ) ) ;
#158885 = CARTESIAN_POINT ( 'NONE',  ( 6.159193757800505153, -1.567253032978152660, -0.9359774744091067245 ) ) ;
#158886 = CARTESIAN_POINT ( 'NONE',  ( -6.847031270101295419, 7.946956888995021728, -1.199719254218446718 ) ) ;
#158888 = CARTESIAN_POINT ( 'NONE',  ( -5.818384198920079520, 6.817144982608731141, 1.199719254218452935 ) ) ;
#158887 = CARTESIAN_POINT ( 'NONE',  ( 6.157125652023562878, -1.936745554134344349, -1.169425401991762259 ) ) ;
#158889 = CARTESIAN_POINT ( 'NONE',  ( 1.963634227113943087, 0.3588053174017143965, -2.075111507017588064 ) ) ;
#158890 = CARTESIAN_POINT ( 'NONE',  ( -6.557303570864871034, 7.679217583210999010, -1.199719254218452047 ) ) ;
#158891 = CARTESIAN_POINT ( 'NONE',  ( 7.377608144130607393, 11.75895993479440982, -0.7998128361456291469 ) ) ;
#158892 = CARTESIAN_POINT ( 'NONE',  ( 7.146556367734764770, 9.431011410480991231, 1.443375672974063439 ) ) ;
#158893 =( NAMED_UNIT ( * ) SI_UNIT ( $, .STERADIAN. ) SOLID_ANGLE_UNIT ( ) );
#158894 = MANIFOLD_SOLID_BREP ( 'Sweep1[6]', #63736 ) ;
#158895 = CARTESIAN_POINT ( 'NONE',  ( -6.852756576703439961, 10.08230087520760954, 1.199719254218453823 ) ) ;
#158896 = CARTESIAN_POINT ( 'NONE',  ( -3.824766175154623582, 7.348582304423016964, -0.7466790275774716212 ) ) ;
#158897 = CARTESIAN_POINT ( 'NONE',  ( 7.307481607641395094, 8.588111966078864512, -1.082531754730537976 ) ) ;
#158898 = CARTESIAN_POINT ( 'NONE',  ( 4.058723290341089474, 7.748532961531467755, 0.5319316551511514835 ) ) ;
#158899 = CARTESIAN_POINT ( 'NONE',  ( -7.836249599018719536, 12.08611559892311504, 0.7216878364870478180 ) ) ;
#158900 = CARTESIAN_POINT ( 'NONE',  ( 2.725082634249659463, 1.605975871135911559, -1.534981474645187971 ) ) ;
#158901 = CARTESIAN_POINT ( 'NONE',  ( -0.01666059994226073634, -0.1612322585618740090, -2.171656592459796808 ) ) ;
#158903 = VECTOR ( 'NONE', #84084, 1000.000000000000000 ) ;
#158902 = CARTESIAN_POINT ( 'NONE',  ( -4.936050443827081580, 7.916420063510339666, 1.199719254218452935 ) ) ;
#158904 = CARTESIAN_POINT ( 'NONE',  ( 5.847644326195776010, 5.716673223516856694, -0.7998128361456281477 ) ) ;
#158905 = CARTESIAN_POINT ( 'NONE',  ( 4.351973852746993110, -0.7528527933186466292, 1.811862133468461922 ) ) ;
#158906 = CARTESIAN_POINT ( 'NONE',  ( 7.730120138085914583, 12.17022392774227768, 0.7998128361456462443 ) ) ;
#158907 = CARTESIAN_POINT ( 'NONE',  ( -4.820845164874406841, 6.759277571458118139, 1.248045366310134741 ) ) ;
#158908 = CARTESIAN_POINT ( 'NONE',  ( 4.207107738942202246, 3.802713871720993399, 1.214306433183764966E-14 ) ) ;
#158909 = CARTESIAN_POINT ( 'NONE',  ( 0.6823417656249882723, 0.6760416670080898749, -1.181850606188749264 ) ) ;
#158910 = CARTESIAN_POINT ( 'NONE',  ( -4.177320726786319049, 6.927272377009067839, -1.082531754730551743 ) ) ;
#158912 = ORIENTED_EDGE ( 'NONE', *, *, #9318, .F. ) ;
#158911 = CARTESIAN_POINT ( 'NONE',  ( -4.582292731738899505, 8.289832587096611860, 0.7216878364870458196 ) ) ;
#158913 = CARTESIAN_POINT ( 'NONE',  ( 3.269896953881154644, 0.5115095171020591636, -2.057881918134551125 ) ) ;
#158914 = CARTESIAN_POINT ( 'NONE',  ( -5.041653019435350380, 6.975290837464928728, -1.599625672291271394 ) ) ;
#158915 = CARTESIAN_POINT ( 'NONE',  ( 4.715790015261832835, -2.120648752638915724, 0.4184459369844309440 ) ) ;
#158916 = CARTESIAN_POINT ( 'NONE',  ( 4.405690278861111864, -0.7914791229979671883, -1.662609734262666894 ) ) ;
#158917 = CARTESIAN_POINT ( 'NONE',  ( -4.588080609115144703, 6.965600104441714180, 1.189663598451236926 ) ) ;
#158918 = CARTESIAN_POINT ( 'NONE',  ( 1.364683531249986537, -0.03229166632525094088, -0.7879004041258309554 ) ) ;
#158919 = CARTESIAN_POINT ( 'NONE',  ( 6.210887288261135453, -0.2055507460125911567, 1.728089712739445671 ) ) ;
#158920 = CARTESIAN_POINT ( 'NONE',  ( 6.727182134110200273, 2.469373133786161745, 2.195552656936059055 ) ) ;
#158921 = CARTESIAN_POINT ( 'NONE',  ( 3.009546912553647147, 5.494593250412460606, -1.082531754730543083 ) ) ;
#158922 = CARTESIAN_POINT ( 'NONE',  ( 9.980956060213129533, 9.821313066029905059, 6.688669764353187830 ) ) ;
#158923 = CARTESIAN_POINT ( 'NONE',  ( 2.501032641837992454, 1.736685530831501456, -1.287010829427559289 ) ) ;
#158924 = STYLED_ITEM ( 'NONE', ( #109553 ), #10376 ) ;
#158925 = CARTESIAN_POINT ( 'NONE',  ( 6.011092252151500226, 2.013677719867816851, 0.1017325769363253418 ) ) ;
#158926 = CARTESIAN_POINT ( 'NONE',  ( -9.300530188850304469, 9.952966096521256745, 1.040834085586084257E-14 ) ) ;
#158927 = CARTESIAN_POINT ( 'NONE',  ( 2.008865009297224447, 1.601992838228694316, -1.451600824242594845 ) ) ;
#158928 = CARTESIAN_POINT ( 'NONE',  ( 4.024654096683129900, 1.870930367033913688, 0.6213144229534044438 ) ) ;
#158929 = DIRECTION ( 'NONE',  ( -2.168404344971003188E-14, 0.000000000000000000, 1.000000000000000000 ) ) ;
#158930 = CARTESIAN_POINT ( 'NONE',  ( 1.378406844460399405, 1.376398589878137013, 1.852031911770692263 ) ) ;
#158931 = CARTESIAN_POINT ( 'NONE',  ( 3.966302600639686204, -1.813262256789631266, -0.6959421042645166366 ) ) ;
#158934 = VERTEX_POINT ( 'NONE', #103334 ) ;
#158933 = CARTESIAN_POINT ( 'NONE',  ( -1.284279953904152949, 3.171639714193937198, 0.7750000000000152323 ) ) ;
#158932 = CARTESIAN_POINT ( 'NONE',  ( -7.985389288324685531, 12.26011190311341537, -0.7216878364870267237 ) ) ;
#158935 = CARTESIAN_POINT ( 'NONE',  ( -5.956828388357799042, 8.042995434541133193, 1.599625672291263179 ) ) ;
#158936 = CARTESIAN_POINT ( 'NONE',  ( 11.80251051724250821, 9.799999999999982947, 1.695257889419128361 ) ) ;
#158938 = EDGE_LOOP ( 'NONE', ( #22763, #85506, #211362, #83451 ) ) ;
#158937 = CARTESIAN_POINT ( 'NONE',  ( -5.438755897737433287, 6.374245297895642537, -1.199719254218453823 ) ) ;
#158939 = CARTESIAN_POINT ( 'NONE',  ( -6.954969613686107444, 10.09758640173367894, 1.082531754730549967 ) ) ;
#158940 = CARTESIAN_POINT ( 'NONE',  ( 2.345003271878861373, 0.4830727525354863716, 2.153096645625157457 ) ) ;
#158942 = EDGE_CURVE ( 'NONE', #45474, #118849, #30271, .T. ) ;
#158941 = CARTESIAN_POINT ( 'NONE',  ( 1.642778471875000035, -0.5760416661887077794, -2.845375778867859751 ) ) ;
#158943 = CARTESIAN_POINT ( 'NONE',  ( 6.244970037249994554, -0.2844439363869250004, -1.940879991452467479 ) ) ;
#158944 = CARTESIAN_POINT ( 'NONE',  ( -1.364683531249997417, 5.071875000341417916, 1.214306433183764966E-14 ) ) ;
#158945 = CARTESIAN_POINT ( 'NONE',  ( 0.7499999999999920064, 4.014583334016149863, 1.299038105676669330 ) ) ;
#158946 = CARTESIAN_POINT ( 'NONE',  ( 6.006184860439112150, 6.084034629330242971, -0.5924424362405518174 ) ) ;
#158948 = DIRECTION ( 'NONE',  ( -0.000000000000000000, 1.000000000000000000, -0.000000000000000000 ) ) ;
#158947 = CARTESIAN_POINT ( 'NONE',  ( 0.1749903794560566661, 7.629137130509112907, -2.555305779167945435 ) ) ;
#158949 = CARTESIAN_POINT ( 'NONE',  ( 5.173706384855800700, -1.019854773079221344, 1.532662130498331887 ) ) ;
#158950 = ORIENTED_EDGE ( 'NONE', *, *, #65893, .F. ) ;
#158951 = CARTESIAN_POINT ( 'NONE',  ( 0.6124999999999846123, 2.645833334016141514, 1.060881119635910252 ) ) ;
#158952 = CARTESIAN_POINT ( 'NONE',  ( -6.531277313481209212, 8.642909503859968368, 1.599625672291283607 ) ) ;
#158953 = CARTESIAN_POINT ( 'NONE',  ( 10.91828647086817661, -9.953005061877725268, -0.1753736836078278460 ) ) ;
#158954 = CARTESIAN_POINT ( 'NONE',  ( 1.040949779275250140E-15, 0.2000000000000057288, 8.500000000000000000 ) ) ;
#158955 = CARTESIAN_POINT ( 'NONE',  ( 11.35777274796318359, 7.533313121839867676, -3.739796408902939628 ) ) ;
#158956 = CARTESIAN_POINT ( 'NONE',  ( 4.123651276850781144, 7.962676922967908411, -0.7998128361456221525 ) ) ;
#158957 = CARTESIAN_POINT ( 'NONE',  ( 0.7607050128039081205, -1.493160483426679841, 1.420726879377065988 ) ) ;
#158960 = CARTESIAN_POINT ( 'NONE',  ( 5.196754805642953556, 1.508532920973480795, 1.055450849767838317 ) ) ;
#158959 = CARTESIAN_POINT ( 'NONE',  ( 2.207255083745041979, -1.492367883816644314, -1.111680554738720073 ) ) ;
#158958 = LINE ( 'NONE', #207695, #66035 ) ;
#158961 = CARTESIAN_POINT ( 'NONE',  ( 7.741869408603235136, 8.990934717247309749, 1.199719254218462483 ) ) ;
#158962 = CARTESIAN_POINT ( 'NONE',  ( -9.489836703503209847, 14.79794462677083011, -7.238794765906159334 ) ) ;
#158963 = CARTESIAN_POINT ( 'NONE',  ( -4.796552484184649856, 8.818004674849227342, -0.7998128361456362523 ) ) ;
#158964 = B_SPLINE_CURVE_WITH_KNOTS ( 'NONE', 3,
 ( #15471, #80495, #116252, #197431, #115192, #146592, #182240, #212610 ),
 .UNSPECIFIED., .F., .F.,
 ( 4, 2, 2, 4 ),
 ( 0.002867044791237291414, 0.003303366235547880534, 0.003521526957703175094, 0.003739687679858470087 ),
 .UNSPECIFIED. ) ;
#158966 = ORIENTED_EDGE ( 'NONE', *, *, #195936, .F. ) ;
#158965 = CARTESIAN_POINT ( 'NONE',  ( -1.500000000000015099, 10.47916666666666607, -0.8660254037844309360 ) ) ;
#158967 = CARTESIAN_POINT ( 'NONE',  ( 4.828867971087246858, 2.111205472107956282, 0.6427781511747706622 ) ) ;
#158968 = CARTESIAN_POINT ( 'NONE',  ( 6.538354595224527444, 2.236366790538524718, 0.3417416818044561877 ) ) ;
#158969 = CARTESIAN_POINT ( 'NONE',  ( -4.772106882330223954, 8.511282429453158827, -0.7216878364870267237 ) ) ;
#158970 = CARTESIAN_POINT ( 'NONE',  ( 5.941655795435678122, -1.702662506596404279, 0.6190658298997688824 ) ) ;
#158971 = CARTESIAN_POINT ( 'NONE',  ( 0.05782782957228919940, 1.164991625563294386, 1.645756161228327130 ) ) ;
#158972 = DIRECTION ( 'NONE',  ( 1.000000000000000000, -5.578564026256504688E-16, 0.000000000000000000 ) ) ;
#158973 = CARTESIAN_POINT ( 'NONE',  ( 0.07933194154487524519, -9.900000000000005684, 9.499668754385634628 ) ) ;
#158974 = CARTESIAN_POINT ( 'NONE',  ( 5.584596538761582352, -1.209766832763665034, 1.480987728393488023 ) ) ;
#158975 = CARTESIAN_POINT ( 'NONE',  ( 0.9361565222895779081, 1.842281575443193375, 0.3236747858033904302 ) ) ;
#158976 = CARTESIAN_POINT ( 'NONE',  ( 2.817592499383800853, -1.357869084745389809, -1.490969456672403881 ) ) ;
#158978 = CARTESIAN_POINT ( 'NONE',  ( 3.826872495277617414, 1.999758222635793947, 0.6608955202877621060 ) ) ;
#158977 = CARTESIAN_POINT ( 'NONE',  ( -9.992522908471816123, 11.61669713376064372, 1.199719254218462483 ) ) ;
#158979 = CARTESIAN_POINT ( 'NONE',  ( 8.585337585951586803, 11.03931315507545108, -1.599625672291255185 ) ) ;
#158981 = CARTESIAN_POINT ( 'NONE',  ( -7.828943636887387925, 11.22118577875556156, 1.199719254218453823 ) ) ;
#158980 = CARTESIAN_POINT ( 'NONE',  ( -1.500000000000015099, -0.5791666666666476226, 0.8660254037844403729 ) ) ;
#158982 = DIRECTION ( 'NONE',  ( 0.000000000000000000, -1.000000000000000000, 0.000000000000000000 ) ) ;
#158984 = EDGE_CURVE ( 'NONE', #17367, #12050, #133740, .T. ) ;
#158983 = CARTESIAN_POINT ( 'NONE',  ( 3.146744605306639908, 1.971464920705681800, 0.4384460897248109723 ) ) ;
#158985 = CARTESIAN_POINT ( 'NONE',  ( 1.364683531249988535, 3.613541667008086211, 0.7879004041258500513 ) ) ;
#158986 = CARTESIAN_POINT ( 'NONE',  ( 4.369805582306193870, 3.992528022312320957, 1.214306433183764966E-14 ) ) ;
#158987 = CARTESIAN_POINT ( 'NONE',  ( 3.954491917119377753, 0.7739500986865335275, 2.018479124525011770 ) ) ;
#158988 = CARTESIAN_POINT ( 'NONE',  ( -3.474999999999997868, -1.677083332377419245, 2.006292185433951047 ) ) ;
#158989 = CARTESIAN_POINT ( 'NONE',  ( 0.7499999999999902300, 5.066666666666684193, -1.299038105676658228 ) ) ;
#158991 = SURFACE_STYLE_FILL_AREA ( #172045 ) ;
#158990 = CARTESIAN_POINT ( 'NONE',  ( 7.614839552730775729, 8.913009562054615031, 1.199719254218452047 ) ) ;
#158993 = EDGE_CURVE ( 'NONE', #18633, #70036, #99082, .T. ) ;
#158992 = CARTESIAN_POINT ( 'NONE',  ( 6.927853306458731986, 11.02631992426980112, 0.7216878364870438212 ) ) ;
#158995 = CARTESIAN_POINT ( 'NONE',  ( 9.319929085041183114, 13.69254449485596226, -7.486148048470657734 ) ) ;
#158994 = CARTESIAN_POINT ( 'NONE',  ( 1.750661792711872611, -2.160631921778751519, -0.2139166996905516871 ) ) ;
#158997 = CARTESIAN_POINT ( 'NONE',  ( 0.5734669319550633748, -1.023298125840161887, 1.530493987491374330 ) ) ;
#158996 = CARTESIAN_POINT ( 'NONE',  ( -6.724481002698126098, 8.868313807946373473, -1.443375672974059665 ) ) ;
#158998 = ADVANCED_FACE ( 'NONE', ( #115386 ), #55068, .T. ) ;
#158999 = CARTESIAN_POINT ( 'NONE',  ( -0.6823417656250212460, 2.551041667008084435, 1.181850606188767472 ) ) ;
#159000 = CARTESIAN_POINT ( 'NONE',  ( 1.945129482973105839, -1.762486321751283835, -1.302348873264857820 ) ) ;
#159001 = CARTESIAN_POINT ( 'NONE',  ( 6.883263157960367806, 6.035304072343574688, 2.648703854151325032 ) ) ;
#159002 = CARTESIAN_POINT ( 'NONE',  ( 2.589068414660402606, -0.3862909535316555454, -2.229145898733439157 ) ) ;
#159003 = CARTESIAN_POINT ( 'NONE',  ( -7.182068686937172153, 9.402166106225269715, 1.599625672291283607 ) ) ;
#159004 = CARTESIAN_POINT ( 'NONE',  ( -1.364683531250012516, 4.301041667008089320, -0.7879004041258300672 ) ) ;
#159005 = CARTESIAN_POINT ( 'NONE',  ( 5.606371582794006159, 7.377293116531995487, 1.238817421570908905 ) ) ;
#159006 = CARTESIAN_POINT ( 'NONE',  ( -1.500000000000008216, 11.74999999999999645, 3.469446951953614189E-15 ) ) ;
#159007 = CARTESIAN_POINT ( 'NONE',  ( 6.129694847154206983, 8.244672969803623630, -1.443375672974078761 ) ) ;
#159008 = CARTESIAN_POINT ( 'NONE',  ( 4.411239408862893008, -0.3036837672792407905, 1.743313046103856179 ) ) ;
#159009 = CARTESIAN_POINT ( 'NONE',  ( 8.748035429315576650, 11.22912730566677553, -1.599625672291255185 ) ) ;
#159010 = CARTESIAN_POINT ( 'NONE',  ( 0.5519644926167607268, 0.6605455615449079554, -1.999741160550670527 ) ) ;
#159012 = CARTESIAN_POINT ( 'NONE',  ( 1.499999999999987121, 1.045833333333352266, -0.8660254037844253849 ) ) ;
#159011 = CARTESIAN_POINT ( 'NONE',  ( -0.6823417656250039265, 10.06770833367473550, -1.181850606188755259 ) ) ;
#159013 = CARTESIAN_POINT ( 'NONE',  ( -3.623772196602547346, 7.449761006003425834, 0.000000000000000000 ) ) ;
#159014 = CARTESIAN_POINT ( 'NONE',  ( 6.257435441360899908, 1.928747933193178721, -0.5880367767025842518 ) ) ;
#159016 = VERTEX_POINT ( 'NONE', #117513 ) ;
#159015 = CARTESIAN_POINT ( 'NONE',  ( 5.256058454422637638, 0.7267480909730811289, -1.659609831382781397 ) ) ;
#159017 = CARTESIAN_POINT ( 'NONE',  ( 9.585778300061798873, 11.14216175728232550, -1.199719254218440723 ) ) ;
#159018 = CARTESIAN_POINT ( 'NONE',  ( 3.256579335763456040, -1.417408692332474462, 1.220890361658559575 ) ) ;
#159019 = CARTESIAN_POINT ( 'NONE',  ( 3.889561532384703924, -1.914723906051108315, 0.7877538119766480662 ) ) ;
#159020 = EDGE_CURVE ( 'NONE', #202678, #181670, #181380, .T. ) ;
#159021 = CARTESIAN_POINT ( 'NONE',  ( -6.251718229232857915, 7.426664367927358512, -1.082531754730549967 ) ) ;
#159022 =( NAMED_UNIT ( * ) SI_UNIT ( $, .STERADIAN. ) SOLID_ANGLE_UNIT ( ) );
#159023 = CARTESIAN_POINT ( 'NONE',  ( 9.023114925094663619, 10.48572115315399245, 1.199719254218453823 ) ) ;
#159024 = CARTESIAN_POINT ( 'NONE',  ( -8.306341666666730461, 12.84248237775322643, 1.040834085586084257E-14 ) ) ;
#159025 = CARTESIAN_POINT ( 'NONE',  ( 6.156284269057003655, 9.340026192945279249, -1.199719254218452047 ) ) ;
#159026 = DIRECTION ( 'NONE',  ( 0.000000000000000000, 0.000000000000000000, -1.000000000000000000 ) ) ;
#159027 = CARTESIAN_POINT ( 'NONE',  ( 0.6823417656249899377, 5.738541667008087543, -1.181850606188754593 ) ) ;
#159028 = CARTESIAN_POINT ( 'NONE',  ( 3.930091730393743710, 1.087902980620155891, 1.632394305395828304 ) ) ;
#159029 = CARTESIAN_POINT ( 'NONE',  ( 1.054064285791616262, 1.779355684154381834, -0.9478921834336280217 ) ) ;
#159030 = CARTESIAN_POINT ( 'NONE',  ( -4.604929450496978660, 5.401447776115099408, -1.199719254218453823 ) ) ;
#159031 = SURFACE_SIDE_STYLE ('',( #94053 ) ) ;
#159032 = CARTESIAN_POINT ( 'NONE',  ( 0.4384654110765589530, 0.3132546388123040870, 1.843968665737522050 ) ) ;
#159033 = CARTESIAN_POINT ( 'NONE',  ( 1.364683531249988535, 4.405208333674754506, -0.7879004041258300672 ) ) ;
#159034 = CARTESIAN_POINT ( 'NONE',  ( 3.252200647028923974, 0.9015175226297014177, -1.800113812977667038 ) ) ;
#159036 = CARTESIAN_POINT ( 'NONE',  ( 2.988026824963069927, -2.114671507216555391, 0.1067447620008883935 ) ) ;
#159035 = CARTESIAN_POINT ( 'NONE',  ( -6.778713617152821058, 7.971215977175476475, 1.082531754730549967 ) ) ;
#159037 = CARTESIAN_POINT ( 'NONE',  ( 6.825078400183555161, 2.951006455646577820, 2.596623860847916188 ) ) ;
#159038 = CARTESIAN_POINT ( 'NONE',  ( 4.879381568908511824, -0.1049739508458477355, 2.067839077007492143 ) ) ;
#159039 = CARTESIAN_POINT ( 'NONE',  ( 5.982890925380405456, 10.20206618957764100, 0.000000000000000000 ) ) ;
#159041 = CARTESIAN_POINT ( 'NONE',  ( 3.379006598303866848, 4.965260336153046516, -1.599625672291262513 ) ) ;
#159040 = CARTESIAN_POINT ( 'NONE',  ( 0.1696251593464107033, 1.207222248521317765, 1.706790159955206887 ) ) ;
#159043 = VERTEX_POINT ( 'NONE', #134794 ) ;
#159042 = CARTESIAN_POINT ( 'NONE',  ( 5.754876975610782708, -1.437719105923901841, 1.124948175183659638 ) ) ;
#159044 = CARTESIAN_POINT ( 'NONE',  ( 8.860417081730671995, 10.29590700256267155, 1.199719254218453823 ) ) ;
#159045 = CYLINDRICAL_SURFACE ( 'NONE', #81912, 0.7499999999999997780 ) ;
#159046 = CARTESIAN_POINT ( 'NONE',  ( 11.60282415082483531, 8.761450460988655209, -2.711552276110228199 ) ) ;
#159047 = AXIS2_PLACEMENT_3D ( 'NONE', #40444, #6830, #120688 ) ;
#159048 = CARTESIAN_POINT ( 'NONE',  ( 6.791986947960565679, -0.9495855537378706801, 1.990061496475347802 ) ) ;
#159049 = CARTESIAN_POINT ( 'NONE',  ( -1.364683531250014514, 12.15104166700806765, -0.7879004041258335089 ) ) ;
#159050 = CARTESIAN_POINT ( 'NONE',  ( 6.633470332280523074, -0.1331818211787652029, 1.881796397474523541 ) ) ;
#159051 = CARTESIAN_POINT ( 'NONE',  ( -9.806625181386236179, 10.33548422123910449, -0.7998128361456291469 ) ) ;
#159052 = CARTESIAN_POINT ( 'NONE',  ( 5.361359679200154105, 8.342337828120466980, 1.199719254218462483 ) ) ;
#159053 = CARTESIAN_POINT ( 'NONE',  ( 4.053524740361575063, 4.791828954252362216, -1.082531754730543083 ) ) ;
#159054 = CARTESIAN_POINT ( 'NONE',  ( 1.499999999999996891, 9.895833333333333925, -0.8660254037844378194 ) ) ;
#159055 = CARTESIAN_POINT ( 'NONE',  ( 5.345992642490140057, 5.131412925860272090, 1.040834085586084257E-14 ) ) ;
#159056 = ORIENTED_EDGE ( 'NONE', *, *, #39268, .T. ) ;
#159057 = CARTESIAN_POINT ( 'NONE',  ( -6.343235766347277149, 8.493804042195527870, -1.599625672291271394 ) ) ;
#159058 = CARTESIAN_POINT ( 'NONE',  ( 0.07700591528349286230, 5.724620991219308230, -2.504819247423330175 ) ) ;
#159060 = CARTESIAN_POINT ( 'NONE',  ( 7.191674137406095291, 7.354984346587396082, 0.000000000000000000 ) ) ;
#159059 = CARTESIAN_POINT ( 'NONE',  ( 0.1329251406260184842, -9.135512438678594194, -9.499304248211862145 ) ) ;
#159061 =( NAMED_UNIT ( * ) PLANE_ANGLE_UNIT ( ) SI_UNIT ( $, .RADIAN. ) );
#159062 = CARTESIAN_POINT ( 'NONE',  ( 0.1394461523056772234, 0.2496508530322391062, -1.754170159799403717 ) ) ;
#159063 = CARTESIAN_POINT ( 'NONE',  ( -5.666945020832185875, 7.634521829102760115, 1.443375672974064550 ) ) ;
#159064 = CARTESIAN_POINT ( 'NONE',  ( 4.196412238629597447, 4.854568018944682706, -1.199719254218452047 ) ) ;
#159065 = CARTESIAN_POINT ( 'NONE',  ( 1.850388327615314799, -1.959487253598888312, -0.1980615517182797158 ) ) ;
#159066 = CARTESIAN_POINT ( 'NONE',  ( 3.655875201264874974, 1.122517324909186653, 1.674876314423722423 ) ) ;
#159067 = CARTESIAN_POINT ( 'NONE',  ( -6.832419346282942563, 10.05857410638369487, 1.199719254218453823 ) ) ;
#159068 = CARTESIAN_POINT ( 'NONE',  ( 6.827182134110222123, -0.006956174471953178659, 2.188967759425272330 ) ) ;
#159069 = CARTESIAN_POINT ( 'NONE',  ( 3.855584222106961612, 2.174980185927982923, -0.2676557845137442215 ) ) ;
#159070 = CARTESIAN_POINT ( 'NONE',  ( 11.92619526913699879, 19.00000000000000000, -1.328859060402686199 ) ) ;
#159071 = CARTESIAN_POINT ( 'NONE',  ( 1.764547866544708521, -1.364041108321904616, 1.360535031132574568 ) ) ;
#159072 = CARTESIAN_POINT ( 'NONE',  ( -7.147119532698295252, 11.49005655479003174, 0.000000000000000000 ) ) ;
#159073 = CARTESIAN_POINT ( 'NONE',  ( -1.854049621773913525, 5.499999999999998224, 0.7500000000000006661 ) ) ;
#159074 = CARTESIAN_POINT ( 'NONE',  ( 0.2331563151865486683, 2.034376611827843906, -2.362208330281903024 ) ) ;
#159075 = CARTESIAN_POINT ( 'NONE',  ( -2.232280211084506583, 15.51994262677984082, -11.79897380041492916 ) ) ;
#159076 = CARTESIAN_POINT ( 'NONE',  ( 6.598014311344812199, 10.84943379654430906, 1.040834085586084257E-14 ) ) ;
#159077 = CARTESIAN_POINT ( 'NONE',  ( 5.983225862332436584, 5.874851682342960402, 0.7998128361456341429 ) ) ;
#159078 = CARTESIAN_POINT ( 'NONE',  ( -6.764644832401259578, -7.632775601084016870, 6.764644832398700736 ) ) ;
#159079 = CARTESIAN_POINT ( 'NONE',  ( 5.885648082108199119, 6.999582529615296700, 1.082531754730549967 ) ) ;
#159080 = ORIENTED_EDGE ( 'NONE', *, *, #164952, .F. ) ;
#159082 = CARTESIAN_POINT ( 'NONE',  ( 2.578773234406753101, -1.386572882437474341, 1.459666011457598556 ) ) ;
#159081 = CARTESIAN_POINT ( 'NONE',  ( 5.882333747326812023, -0.2767177626767613474, -1.820229446528654371 ) ) ;
#159083 = CARTESIAN_POINT ( 'NONE',  ( 4.165566195501821056, -0.7159155550505342802, -2.184124419653421523 ) ) ;
#159085 = CARTESIAN_POINT ( 'NONE',  ( 2.289708051090312058, -1.211253549455925338, -1.412920978024762908 ) ) ;
#159084 = CARTESIAN_POINT ( 'NONE',  ( -0.02900071798685177615, 6.946858727649162901, -2.768864135414349281 ) ) ;
#159086 = CARTESIAN_POINT ( 'NONE',  ( 1.001543065824772753E-15, -1.071874999522043792, 3.793834371823811669 ) ) ;
#159087 = DIRECTION ( 'NONE',  ( 0.000000000000000000, 0.000000000000000000, 1.000000000000000000 ) ) ;
#159088 = CARTESIAN_POINT ( 'NONE',  ( -7.320512876374914768, 10.62801655815766999, 1.199719254218453823 ) ) ;
#159089 = CARTESIAN_POINT ( 'NONE',  ( -6.644904684473536882, 6.925012684740138980, 0.7216878364870317197 ) ) ;
#159091 = CARTESIAN_POINT ( 'NONE',  ( 4.364026845288040413, 0.8817440624687390427, 1.649792572839225091 ) ) ;
#159090 = CARTESIAN_POINT ( 'NONE',  ( 4.898031494525131535, -0.7058569028579181337, -1.968109489924846356 ) ) ;
#159092 = CARTESIAN_POINT ( 'NONE',  ( 6.155038550924144758, 8.203964280876741455, 1.443375672974076540 ) ) ;
#159093 = CARTESIAN_POINT ( 'NONE',  ( 1.889141968554370221, 3.755428628636679811, 0.3999999999999819811 ) ) ;
#159094 = CARTESIAN_POINT ( 'NONE',  ( 6.656889574143706412, -1.327764893807031221, 1.100862838992909598 ) ) ;
#159095 = CARTESIAN_POINT ( 'NONE',  ( -6.575868197828002693, 7.630599971342813426, 1.199719254218450271 ) ) ;
#159096 = CARTESIAN_POINT ( 'NONE',  ( 1.371252568922965098, -0.2536805693413109464, -1.715349781374966742 ) ) ;
#159097 = DIRECTION ( 'NONE',  ( 0.000000000000000000, 1.000000000000000000, 0.000000000000000000 ) ) ;
#159098 = CARTESIAN_POINT ( 'NONE',  ( -1.500000000000016209, 5.452083334016153415, 0.8660254037844375974 ) ) ;
#159099 = DIRECTION ( 'NONE',  ( 1.000000000000000000, 0.000000000000000000, -3.491481338843133355E-15 ) ) ;
#159100 = CARTESIAN_POINT ( 'NONE',  ( 6.227409518260961896, 0.1680337313966096258, -2.164657318592048352 ) ) ;
#159101 = CARTESIAN_POINT ( 'NONE',  ( 4.951681858558426796, 0.5695450498939165218, -1.734646904759745700 ) ) ;
#159102 = CARTESIAN_POINT ( 'NONE',  ( 1.709737484509077143, 0.5745576563440238926, -1.875703277996950469 ) ) ;
#159103 = B_SPLINE_CURVE_WITH_KNOTS ( 'NONE', 3,
 ( #95116, #161165, #144946, #80969, #180598, #179548 ),
 .UNSPECIFIED., .F., .F.,
 ( 4, 2, 4 ),
 ( 0.000000000000000000, 0.0003239988925529257036, 0.0006479977851058514073 ),
 .UNSPECIFIED. ) ;
#159104 = LINE ( 'NONE', #61602, #172001 ) ;
#159105 = DIRECTION ( 'NONE',  ( 0.000000000000000000, -1.000000000000000000, 0.000000000000000000 ) ) ;
#159106 = CARTESIAN_POINT ( 'NONE',  ( 7.914208982075123799, 10.25632978388623684, -1.599625672291262513 ) ) ;
#159108 = EDGE_CURVE ( 'NONE', #161726, #67975, #120480, .T. ) ;
#159107 = AXIS2_PLACEMENT_3D ( 'NONE', #91969, #158026, #124531 ) ;
#159109 = CARTESIAN_POINT ( 'NONE',  ( 2.438272501909013901, -1.223040458498025673, -1.732039452853536776 ) ) ;
#159110 = DIRECTION ( 'NONE',  ( 0.000000000000000000, -1.000000000000000000, 0.000000000000000000 ) ) ;
#159111 = FILL_AREA_STYLE_COLOUR ( '', #201545 ) ;
#159112 = CARTESIAN_POINT ( 'NONE',  ( -4.965152591087599099, 6.642004417359813395, -1.244917454897740861 ) ) ;
#159113 = CARTESIAN_POINT ( 'NONE',  ( 0.4618902312403838639, -0.5555351291045197426, 1.994226918997483500 ) ) ;
#159115 = CARTESIAN_POINT ( 'NONE',  ( -1.500000000000008216, 14.53125000068279604, 3.469446951953614189E-15 ) ) ;
#159114 = CARTESIAN_POINT ( 'NONE',  ( -10.66890663286052465, 4.188823345043420687, 5.493879390884747416 ) ) ;
#159117 = ORIENTED_EDGE ( 'NONE', *, *, #84646, .T. ) ;
#159116 = CARTESIAN_POINT ( 'NONE',  ( 3.159039748919801216, 0.5414197367904579616, 2.154182169225922205 ) ) ;
#159118 = CARTESIAN_POINT ( 'NONE',  ( 0.5987520574620349700, -0.3298207119002970478, 2.274815185769126114 ) ) ;
#159120 = CARTESIAN_POINT ( 'NONE',  ( 6.842638575262629530, -2.021612500624434539, -0.4081942145969327251 ) ) ;
#159119 = CARTESIAN_POINT ( 'NONE',  ( 3.225950485047770933, 5.851027101609320269, 1.199719254218450271 ) ) ;
#159122 = CARTESIAN_POINT ( 'NONE',  ( -3.475000000000000533, -2.450000000000000622, 0.000000000000000000 ) ) ;
#159121 = CARTESIAN_POINT ( 'NONE',  ( 5.388439706788500594, 5.251210844200210559, 0.7998128361456352531 ) ) ;
#159123 = CARTESIAN_POINT ( 'NONE',  ( 0.1331565106231571705, 4.092041177288479048, -2.500854978060399691 ) ) ;
#159124 = CARTESIAN_POINT ( 'NONE',  ( 5.952668924537682038, -1.582617586749142102, -0.9407850039931386910 ) ) ;
#159125 = CARTESIAN_POINT ( 'NONE',  ( -10.79929312474869008, -8.526088927970988607, 0.1885023626713056288 ) ) ;
#159126 = CARTESIAN_POINT ( 'NONE',  ( -0.1104750535120043037, 1.338503269012698116, -2.356272470560859755 ) ) ;
#159127 = CARTESIAN_POINT ( 'NONE',  ( 3.293694421395336303, -0.6999868571894217739, 1.576533365092074757 ) ) ;
#159128 = CARTESIAN_POINT ( 'NONE',  ( 1.358611653602972869, -1.916354379050893009, -0.6279873632355145174 ) ) ;
#159129 = CARTESIAN_POINT ( 'NONE',  ( 3.340769233699531604, 0.5564940052410914939, -2.230230389815818892 ) ) ;
#159130 = CARTESIAN_POINT ( 'NONE',  ( 2.601149388587006950, 1.818552668380982951, -1.345706882341807242 ) ) ;
#159131 = CARTESIAN_POINT ( 'NONE',  ( 4.846364118386396136, 2.100373345016784743, 0.1556085008114059531 ) ) ;
#159132 = CARTESIAN_POINT ( 'NONE',  ( -7.621091744657483069, 8.063897588288083895, 0.7216878364870317197 ) ) ;
#159133 = CARTESIAN_POINT ( 'NONE',  ( 3.321328847770131709, -1.706417891748934546, 0.4689366942724793041 ) ) ;
#159135 = CARTESIAN_POINT ( 'NONE',  ( 6.603114554492313104, -0.5110835225830052675, 2.243201349117603716 ) ) ;
#159134 = CARTESIAN_POINT ( 'NONE',  ( 3.540087506499646874, 7.144202834309300698, -0.7216878364870338292 ) ) ;
#159136 = CARTESIAN_POINT ( 'NONE',  ( 4.910013284106277354, 1.267360923890372693, -1.335742228452965863 ) ) ;
#159137 = CARTESIAN_POINT ( 'NONE',  ( -4.786191920824102830, 5.542644314838231168, 1.199719254218462483 ) ) ;
#159138 = CARTESIAN_POINT ( 'NONE',  ( 4.324687812634874895, 7.989293514808604613, 0.7216878364870317197 ) ) ;
#159139 = CARTESIAN_POINT ( 'NONE',  ( -1.499999999999997780, 3.400000000000021227, 1.214306433183764966E-14 ) ) ;
#159140 = CARTESIAN_POINT ( 'NONE',  ( 4.347736757272717689, 2.190986304709115373, -0.05254992341368477232 ) ) ;
#159141 = CARTESIAN_POINT ( 'NONE',  ( -4.761938266897808525, 6.578680616179308771, 1.599625672291267398 ) ) ;
#159142 = DIRECTION ( 'NONE',  ( 0.6507913734559640506, -0.7592566023653004592, 0.000000000000000000 ) ) ;
#159143 = CARTESIAN_POINT ( 'NONE',  ( 4.387213907293201487, 0.09840592021137170575, 2.068135374880715638 ) ) ;
#159144 = CARTESIAN_POINT ( 'NONE',  ( -0.03006412033006514162, -0.9462945741195265548, 1.780671068589256834 ) ) ;
#159145 = STYLED_ITEM ( 'NONE', ( #117404 ), #112039 ) ;
#159146 = CARTESIAN_POINT ( 'NONE',  ( 0.6823417656249917140, 4.092708333674755394, 1.181850606188765695 ) ) ;
#159147 = CARTESIAN_POINT ( 'NONE',  ( 3.633351821168579132, -1.779675539450284560, 0.7381315413402672609 ) ) ;
#159148 = LINE ( 'NONE', #118998, #137583 ) ;
#159149 = CARTESIAN_POINT ( 'NONE',  ( -2.982430605326328532, 5.462957558647244305, -1.082531754730543971 ) ) ;
#159150 = CARTESIAN_POINT ( 'NONE',  ( 0.4752230700786713169, -1.603524673181003779, 1.537559121520514660 ) ) ;
#159151 = ORIENTED_EDGE ( 'NONE', *, *, #95454, .T. ) ;
#159153 = DIRECTION ( 'NONE',  ( -1.000000000000000000, 0.000000000000000000, 0.000000000000000000 ) ) ;
#159152 = CARTESIAN_POINT ( 'NONE',  ( 4.327421620524169121, 8.660439266295391292, 0.7750000000000001332 ) ) ;
#159154 = CARTESIAN_POINT ( 'NONE',  ( 4.867540842506059562, 5.637551390133895168, -1.199719254218452047 ) ) ;
#159155 = CARTESIAN_POINT ( 'NONE',  ( 4.067155351693835485E-15, 0.2500000006828133059, -1.225000000000014300 ) ) ;
#159156 = CARTESIAN_POINT ( 'NONE',  ( -0.003376046620573100454, -7.161464053357560644, -9.586610838029425707 ) ) ;
#159157 = CARTESIAN_POINT ( 'NONE',  ( 11.94524591058472041, 7.576283193003019889, -0.4340265584551949996 ) ) ;
#159158 = CARTESIAN_POINT ( 'NONE',  ( 0.000000000000000000, -1.000000000000000888, 0.000000000000000000 ) ) ;
#159159 = CARTESIAN_POINT ( 'NONE',  ( 1.820681965693775162, -1.389665069980907663, 1.385087887197037571 ) ) ;
#159160 = CARTESIAN_POINT ( 'NONE',  ( 1.364683531249988757, 1.946875000341415030, 0.000000000000000000 ) ) ;
#159161 = DIRECTION ( 'NONE',  ( 1.000000000000000000, -7.387867266669436732E-31, 0.000000000000000000 ) ) ;
#159162 = CARTESIAN_POINT ( 'NONE',  ( 5.055110333045015558, 1.632132345252810035, -1.088295032039228172 ) ) ;
#159163 = CARTESIAN_POINT ( 'NONE',  ( -2.676845263694313637, 5.210404343363602919, -1.199719254218446718 ) ) ;
#159164 = CARTESIAN_POINT ( 'NONE',  ( -4.717874267431199087, 8.448011045404303587, 1.040834085586084257E-14 ) ) ;
#159165 = CARTESIAN_POINT ( 'NONE',  ( 6.614160618316515361, -1.014195557614630205, -1.909021090911746654 ) ) ;
#159167 = ORIENTED_EDGE ( 'NONE', *, *, #53808, .T. ) ;
#159166 = CARTESIAN_POINT ( 'NONE',  ( -0.1106727585416019261, 7.629137130509112907, -2.603481208547548054 ) ) ;
#159168 = CARTESIAN_POINT ( 'NONE',  ( -1.201851678989727383E-14, 4.446875000341417916, -1.575800808251660134 ) ) ;
#159169 = CARTESIAN_POINT ( 'NONE',  ( 0.7021627906659900775, -0.6242572379067250488, -1.763460184394528341 ) ) ;
#159170 = CARTESIAN_POINT ( 'NONE',  ( 6.538463365017005202, 1.657764536579940495, -0.5080105315169358704 ) ) ;
#159172 = CARTESIAN_POINT ( 'NONE',  ( 2.841561854484982774, 0.7863008361240211297, -2.045831095052422555 ) ) ;
#159171 = CARTESIAN_POINT ( 'NONE',  ( 0.6801582343749970061, 0.5572916670080683144, -1.178068619123862515 ) ) ;
#159173 = CARTESIAN_POINT ( 'NONE',  ( 4.120403395486138542, -1.183043222452788257, -1.981120964393435768 ) ) ;
#159174 = CARTESIAN_POINT ( 'NONE',  ( 5.589157960464589792, 1.819533713976368094, -0.9674792931896135650 ) ) ;
#159175 = CARTESIAN_POINT ( 'NONE',  ( 2.273291157499750526, 1.194718917728957885, 1.530869066462538619 ) ) ;
#159176 = CARTESIAN_POINT ( 'NONE',  ( -5.653386866774179786, 8.579073197003079798, 1.082531754730548412 ) ) ;
#159177 = CARTESIAN_POINT ( 'NONE',  ( 4.922192346260840345, -2.110166376318895587, 0.2103620946037400852 ) ) ;
#159178 = CARTESIAN_POINT ( 'NONE',  ( 2.777970385693105726, 1.728001979019553325, -1.038993764437286416 ) ) ;
#159179 = CARTESIAN_POINT ( 'NONE',  ( -4.514501963226242864, 7.250374142863800664, 1.082531754730560403 ) ) ;
#159180 = CARTESIAN_POINT ( 'NONE',  ( 5.297975422827020608, -0.7987165953184969247, 2.057335881587420534 ) ) ;
#159181 = CARTESIAN_POINT ( 'NONE',  ( -6.957269102468015554, 8.145844036748005834, 1.199719254218452047 ) ) ;
#159182 = CARTESIAN_POINT ( 'NONE',  ( 8.563946585326370098, 13.14302144952281814, 0.7998128361456462443 ) ) ;
#159183 = CARTESIAN_POINT ( 'NONE',  ( 0.1877650043593872553, -0.8638833939697135866, 1.608357707688967242 ) ) ;
#159184 = CARTESIAN_POINT ( 'NONE',  ( -6.774234028683526532, 7.932303117332766718, 1.199719254218452047 ) ) ;
#159186 = CARTESIAN_POINT ( 'NONE',  ( -5.010620288702242853, 8.003418215864698482, -1.199719254218453823 ) ) ;
#159185 = CARTESIAN_POINT ( 'NONE',  ( -5.274058703912462676, 7.771439464937274444, 1.305864451146660388 ) ) ;
#159187 = CARTESIAN_POINT ( 'NONE',  ( 1.501062075862685363, 8.754928401006200289, -2.503798761944566742 ) ) ;
#159188 = ORIENTED_EDGE ( 'NONE', *, *, #84048, .T. ) ;
#159189 = CARTESIAN_POINT ( 'NONE',  ( 5.330957127283824981, 0.1492067265368417217, 2.055538663769764796 ) ) ;
#159190 = CARTESIAN_POINT ( 'NONE',  ( 4.119726892546750285, 7.639700203672255441, -0.7297710838231908914 ) ) ;
#159191 = UNCERTAINTY_MEASURE_WITH_UNIT (LENGTH_MEASURE( 1.000000000000000082E-05 ), #22164, 'distance_accuracy_value', 'NONE');
#159192 = CARTESIAN_POINT ( 'NONE',  ( 0.09463244300324949454, -8.038540703696430256, 9.499633399276474321 ) ) ;
#159193 = CARTESIAN_POINT ( 'NONE',  ( -3.405069135326500351, 7.124331091189553433, 1.040834085586084257E-14 ) ) ;
#159194 = CARTESIAN_POINT ( 'NONE',  ( -3.006876207180748217, 6.730049018344652190, -0.7998128361456481317 ) ) ;
#159195 = CARTESIAN_POINT ( 'NONE',  ( 4.266274442087925500, 2.019191850312745284, -0.05169103710895606163 ) ) ;
#159196 = CARTESIAN_POINT ( 'NONE',  ( -1.402160292154681736E-14, 0.4625000000000214495, 1.732050807568877637 ) ) ;
#159198 = CARTESIAN_POINT ( 'NONE',  ( 9.585251415181632595, 10.28514086057449184, 0.000000000000000000 ) ) ;
#159197 = CARTESIAN_POINT ( 'NONE',  ( -5.438755897737433287, 6.374245297895642537, -1.199719254218453823 ) ) ;
#159199 = CARTESIAN_POINT ( 'NONE',  ( 7.202405917357655341, 9.425892875049191488, 1.599625672291281386 ) ) ;
#159200 = CARTESIAN_POINT ( 'NONE',  ( 4.047771301309529335, 0.6961604498142616171, -1.939876652229477028 ) ) ;
#159201 = CARTESIAN_POINT ( 'NONE',  ( 2.303361484738715159, 1.314996338066702242, -1.528741580717301263 ) ) ;
#159202 = ORIENTED_EDGE ( 'NONE', *, *, #113502, .T. ) ;
#159203 = CARTESIAN_POINT ( 'NONE',  ( 1.889772045536109779, 3.296949564223924156, -0.4024211290685810183 ) ) ;
#159204 = CARTESIAN_POINT ( 'NONE',  ( 5.054492339796319733, 4.791329239384148231, -0.7998128361456211532 ) ) ;
#159206 = ORIENTED_EDGE ( 'NONE', *, *, #101605, .F. ) ;
#159205 = CARTESIAN_POINT ( 'NONE',  ( 0.2999999999999842792, 3.975028841772351829, 0.9637995837462106641 ) ) ;
#159207 = CARTESIAN_POINT ( 'NONE',  ( 3.391953724946984661, 0.04666865176591524639, 2.015725201127672506 ) ) ;
#159208 = CARTESIAN_POINT ( 'NONE',  ( 1.939159035295745959, 0.7054217538491479589, -1.700835786604155242 ) ) ;
#159209 = CARTESIAN_POINT ( 'NONE',  ( 0.4875218067809834466, -0.2886260216827610803, -2.289518885299694606 ) ) ;
#159210 = CARTESIAN_POINT ( 'NONE',  ( 4.213551878797002992, 8.137837301896977849, 0.000000000000000000 ) ) ;
#159211 = CARTESIAN_POINT ( 'NONE',  ( 2.636181727411972098, 1.021492356387411427, -1.905029093917938399 ) ) ;
#159212 = CARTESIAN_POINT ( 'NONE',  ( -5.575427483717760424, 7.527751369135936343, 1.599625672291269396 ) ) ;
#159213 = CARTESIAN_POINT ( 'NONE',  ( 2.900137762625193183, 0.2794712830477152354, 2.281260185934708140 ) ) ;
#159214 = ORIENTED_EDGE ( 'NONE', *, *, #182569, .T. ) ;
#159215 = CARTESIAN_POINT ( 'NONE',  ( 0.6124999999999637401, 2.416666666666629659, -1.060881119635962211 ) ) ;
#159216 = CARTESIAN_POINT ( 'NONE',  ( 1.076777757339364205, -0.04213119042271313425, -1.870346338061685154 ) ) ;
#159217 =( BOUNDED_SURFACE ( )  B_SPLINE_SURFACE ( 3, 2, ( 
 ( #183887, #104801, #86399 ),
 ( #170846, #169775, #5108 ),
 ( #37646, #201185, #54970 ),
 ( #118961, #151408, #121122 ) ),
 .UNSPECIFIED., .F., .F., .T. ) 
 B_SPLINE_SURFACE_WITH_KNOTS ( ( 4, 4 ),
 ( 3, 3 ),
 ( -1.355252715606880543E-20, 3.124373798652707124E-05 ),
 ( 0.000000000000000000, 1.000000000000000000 ),
 .UNSPECIFIED. ) 
 GEOMETRIC_REPRESENTATION_ITEM ( )  RATIONAL_B_SPLINE_SURFACE ( (
 ( 1.000000000000000000, 0.7071067811870692665, 1.000000000000000000),
 ( 1.000000000000000000, 0.7053575014263949727, 1.000000000000000000),
 ( 1.000000000000000000, 0.7044883013754549284, 1.000000000000000000),
 ( 1.000000000000000000, 0.7045118851643193958, 1.000000000000000000) ) ) 
 REPRESENTATION_ITEM ( '' )  SURFACE ( )  );
#159218 = CARTESIAN_POINT ( 'NONE',  ( 6.157099186568592231, -1.690597638883487797, -1.013973547023840460 ) ) ;
#159220 = CARTESIAN_POINT ( 'NONE',  ( 8.880227426826641235, 10.42298208846167284, 1.082531754730549967 ) ) ;
#159219 = CARTESIAN_POINT ( 'NONE',  ( 0.6823417656249899377, 3.092708333674754062, 1.181850606188765695 ) ) ;
#159222 = CARTESIAN_POINT ( 'NONE',  ( 0.7157882511714327434, -0.3199875008889854766, 2.183444778895065941 ) ) ;
#159221 = CARTESIAN_POINT ( 'NONE',  ( -4.900382456335551140, 7.804531068111707270, 1.199719254218464037 ) ) ;
#159223 = CARTESIAN_POINT ( 'NONE',  ( 3.845709127770629010, 7.638411082374393146, 0.7998128361456321445 ) ) ;
#159224 = CARTESIAN_POINT ( 'NONE',  ( -3.927058049452637700, 7.733318157670055371, -0.7998128361456281477 ) ) ;
#159225 = DIRECTION ( 'NONE',  ( -1.000000000000000000, 0.000000000000000000, 0.000000000000000000 ) ) ;
#159226 = CARTESIAN_POINT ( 'NONE',  ( 4.873880070992254510, 1.134317645522317175, 1.612277344948910285 ) ) ;
#159227 = CARTESIAN_POINT ( 'NONE',  ( 6.258070668236964451, 0.7691888804484037223, -1.867794269369964066 ) ) ;
#159228 = CARTESIAN_POINT ( 'NONE',  ( 4.002764008144163554, -0.7221186334790052896, -2.191863981390995253 ) ) ;
#159229 = CARTESIAN_POINT ( 'NONE',  ( 2.588800687925230992, 1.999571085336487641, 0.5053362289856622169 ) ) ;
#159230 = CARTESIAN_POINT ( 'NONE',  ( 5.341549334104176872, 9.175631956522799726, 0.7216878364870438212 ) ) ;
#159231 = CARTESIAN_POINT ( 'NONE',  ( 4.854701522145073334, 7.821512988214679218, -1.199719254218450271 ) ) ;
#159232 = CARTESIAN_POINT ( 'NONE',  ( 5.411639590510088027, 6.342609606130419131, -1.199719254218452047 ) ) ;
#159233 = CARTESIAN_POINT ( 'NONE',  ( -1.201851678989727383E-14, 2.634375000341417916, 1.575800808251672791 ) ) ;
#159234 = CARTESIAN_POINT ( 'NONE',  ( 0.1448469644582885130, 14.55305575109302829, 11.95498533988372891 ) ) ;
#159235 = CARTESIAN_POINT ( 'NONE',  ( 6.927853306458752414, 7.184843067064434763, 0.7216878364870317197 ) ) ;
#159236 = CARTESIAN_POINT ( 'NONE',  ( 5.617690636765501289, 0.4290425436993560715, -2.128212118068722347 ) ) ;
#159238 = CARTESIAN_POINT ( 'NONE',  ( 4.440845869443198701, -1.426288408191313639, -1.164454570719307469 ) ) ;
#159237 = CARTESIAN_POINT ( 'NONE',  ( -3.633221978782290140, 6.222214161012547429, -1.082531754730549967 ) ) ;
#159239 = ADVANCED_FACE ( 'NONE', ( #165134 ), #46272, .F. ) ;
#159241 = CARTESIAN_POINT ( 'NONE',  ( 6.720655732516650716, 2.984497329163855461, 2.280179935440066252 ) ) ;
#159240 = CARTESIAN_POINT ( 'NONE',  ( -9.797921721691023933, 3.956598013261175772, -6.103348209225892163 ) ) ;
#159242 = CARTESIAN_POINT ( 'NONE',  ( 5.126606437771586755, 0.1607948393855564151, 2.185736094377451089 ) ) ;
#159243 = DIRECTION ( 'NONE',  ( -0.000000000000000000, 1.000000000000000000, -0.000000000000000000 ) ) ;
#159244 = CARTESIAN_POINT ( 'NONE',  ( 0.1931282604852417040, -0.5026490872193057902, -2.214429643963564232 ) ) ;
#159245 = CARTESIAN_POINT ( 'NONE',  ( -4.055257346293188014, 7.741894102302186553, 0.6119906029944787162 ) ) ;
#159246 = CARTESIAN_POINT ( 'NONE',  ( -4.415768667553308270E-15, 0.1250000006828069499, 1.224999999999963229 ) ) ;
#159247 = CARTESIAN_POINT ( 'NONE',  ( 4.873468316212648865, 8.167532512703042258, 0.9812947938723035612 ) ) ;
#159248 = CARTESIAN_POINT ( 'NONE',  ( -3.784134271545645412, 7.428924060196286483, 0.7216878364870338292 ) ) ;
#159249 = CARTESIAN_POINT ( 'NONE',  ( 3.092668437693027794, 6.622213920701574885, -0.7216878364870338292 ) ) ;
#159250 = CARTESIAN_POINT ( 'NONE',  ( 1.322737547172361472, -0.04825712817433693014, 1.769365563168373345 ) ) ;
#159251 = CARTESIAN_POINT ( 'NONE',  ( 5.619794420184654804, -0.4867899507037063422, 1.953244479579784976 ) ) ;
#159252 = CARTESIAN_POINT ( 'NONE',  ( 5.982172092127724383, 8.002286745614243912, -1.599625672291262513 ) ) ;
#159253 = CARTESIAN_POINT ( 'NONE',  ( 4.506922906144382956, 1.629430921360131679, -1.334182900473983135 ) ) ;
#159254 = CARTESIAN_POINT ( 'NONE',  ( 3.462411278976515128, -1.846996576941996482, -0.5078680121572733963 ) ) ;
#159255 = CARTESIAN_POINT ( 'NONE',  ( 2.683624340501134853, 5.218313266304903664, -1.199719254218446718 ) ) ;
#159256 = CARTESIAN_POINT ( 'NONE',  ( 4.281674416708352027, -1.885371899234816739, 0.5696992939150746782 ) ) ;
#159257 = CARTESIAN_POINT ( 'NONE',  ( 5.414321571020942692, -2.019972751022606872, 0.004158903309840755735 ) ) ;
#159258 = CARTESIAN_POINT ( 'NONE',  ( 1.516246529245099284, 1.258767711876613848, -1.383943980506313398 ) ) ;
#159261 = ORIENTED_EDGE ( 'NONE', *, *, #80012, .T. ) ;
#159260 = CARTESIAN_POINT ( 'NONE',  ( 1.300873410958070409, -0.2835801433653042380, -1.891145142470892715 ) ) ;
#159259 = CARTESIAN_POINT ( 'NONE',  ( 5.320820994898000755, 1.595919931443249951, 0.6549295409969541071 ) ) ;
#159263 = CARTESIAN_POINT ( 'NONE',  ( 3.497640442645619796, 6.064035702186436616, -1.082531754730543083 ) ) ;
#159262 = CARTESIAN_POINT ( 'NONE',  ( 2.016531038934398445, -1.041976349804032420, -1.945408382319254503 ) ) ;
#159264 = AXIS2_PLACEMENT_3D ( 'NONE', #208599, #79685, #192350 ) ;
#159265 = CARTESIAN_POINT ( 'NONE',  ( 0.6823417656249899377, 2.655208333674753618, 1.181850606188767472 ) ) ;
#159266 = CARTESIAN_POINT ( 'NONE',  ( 6.285602425426498385, -1.847771260692541162, 0.6596951833430019230 ) ) ;
#159267 = CARTESIAN_POINT ( 'NONE',  ( 9.088043039861931405, 9.497138389460751284, 1.040834085586084257E-14 ) ) ;
#159268 = CARTESIAN_POINT ( 'NONE',  ( 11.44779965693254198, 12.60313923201305641, -3.599999932276613634 ) ) ;
#159269 = CARTESIAN_POINT ( 'NONE',  ( -8.787802685836078709, 3.956598013261175772, -7.485281629513451662 ) ) ;
#159270 = CARTESIAN_POINT ( 'NONE',  ( -5.416646063859567484, 6.278174148379618735, 1.199719254218450271 ) ) ;
#159271 = CARTESIAN_POINT ( 'NONE',  ( -9.855659161987910366, -6.334709917115479705, 0.4359479416626658166 ) ) ;
#159272 = EDGE_CURVE ( 'NONE', #108645, #128754, #143088, .T. ) ;
#159273 = VERTEX_POINT ( 'NONE', #141510 ) ;
#159274 = CARTESIAN_POINT ( 'NONE',  ( 2.383334800519558705, -0.002349189141126820958, 2.070544812199434315 ) ) ;
#159275 = CARTESIAN_POINT ( 'NONE',  ( 1.499999999999989120, 2.525000000000020339, 1.214306433183764966E-14 ) ) ;
#159276 = CARTESIAN_POINT ( 'NONE',  ( 4.462605117192430804, 8.358123070033169455, 1.040834085586084257E-14 ) ) ;
#159277 = CARTESIAN_POINT ( 'NONE',  ( -7.888146445052511169, 8.097259028849730811, 1.040834085586084257E-14 ) ) ;
#159278 = CARTESIAN_POINT ( 'NONE',  ( 4.228163802615382494, 6.026220084508304708, -1.599625672291269396 ) ) ;
#159279 = CARTESIAN_POINT ( 'NONE',  ( 6.410795937096152919, -0.5649949523399040441, -2.043744576961013859 ) ) ;
#159280 = PRESENTATION_STYLE_ASSIGNMENT (( #93246 ) ) ;
#159281 = CARTESIAN_POINT ( 'NONE',  ( 1.364683531249988535, 3.113541667008083991, 0.7879004041258500513 ) ) ;
#159283 = CARTESIAN_POINT ( 'NONE',  ( 4.304877467538922531, 4.981110786005563007, 1.199719254218464037 ) ) ;
#159282 = CARTESIAN_POINT ( 'NONE',  ( -1.500000000000001110, 11.77083333333333570, 0.8660254037844418162 ) ) ;
#159284 = CARTESIAN_POINT ( 'NONE',  ( 5.290388671387995068, -1.915306256023458831, 0.6297802918850337051 ) ) ;
#159285 = CARTESIAN_POINT ( 'NONE',  ( 4.294081978838642399, -0.8244651323695743050, -1.729401801750865442 ) ) ;
#159286 = DIRECTION ( 'NONE',  ( 0.000000000000000000, 0.000000000000000000, 1.000000000000000000 ) ) ;
#159287 = CARTESIAN_POINT ( 'NONE',  ( 2.911879292414457865, -1.082406496695037301, -1.905547650945007554 ) ) ;
#159288 = CARTESIAN_POINT ( 'NONE',  ( 0.1335669894368292088, 2.005130876877735613, -2.568368839946821414 ) ) ;
#159289 = CARTESIAN_POINT ( 'NONE',  ( 1.499999999999989120, 1.306250000682816825, 0.000000000000000000 ) ) ;
#159290 = CARTESIAN_POINT ( 'NONE',  ( 5.449481901252090310, -1.818156339564154012, 0.8647962134734816786 ) ) ;
#159291 = CARTESIAN_POINT ( 'NONE',  ( 1.828231037913151447, -0.9045423626323212396, -1.684975973026317408 ) ) ;
#159292 = CARTESIAN_POINT ( 'NONE',  ( -7.152089726408780379, 8.302858421353754181, -1.199719254218446718 ) ) ;
#159294 = CARTESIAN_POINT ( 'NONE',  ( -0.07068620461728526705, -1.560437159073333468, -1.276799021846956705 ) ) ;
#159293 = CARTESIAN_POINT ( 'NONE',  ( -4.460269349215930212, 4.305995116947750390, 1.214306433183764966E-14 ) ) ;
#159295 = CARTESIAN_POINT ( 'NONE',  ( 1.364683531250000303, 9.567708333674735499, -0.7879004041258355073 ) ) ;
#159297 = CARTESIAN_POINT ( 'NONE',  ( -5.772739544368596043, 9.956889578397179363, -0.7998128361456362523 ) ) ;
#159296 = CARTESIAN_POINT ( 'NONE',  ( 3.298458272841266137, 1.646618950329106434, -1.288217307904614639 ) ) ;
#159299 = ORIENTED_EDGE ( 'NONE', *, *, #173426, .F. ) ;
#159298 = CARTESIAN_POINT ( 'NONE',  ( 2.309205411980755240, -0.3811568730716380915, 1.681943839628738058 ) ) ;
#159300 = CARTESIAN_POINT ( 'NONE',  ( 6.381110825713084189, -1.939362502171553482, -0.8581636585355472135 ) ) ;
#159301 = CARTESIAN_POINT ( 'NONE',  ( 6.094553744542824170, 7.069066442510145265, 1.199719254218462483 ) ) ;
#159302 = CARTESIAN_POINT ( 'NONE',  ( -15.75000000000000000, 13.40000000000000036, -1.800000000000001155 ) ) ;
#159303 = CARTESIAN_POINT ( 'NONE',  ( 0.09999999999999592548, -9.999999999999994671, 9.579478065113978147 ) ) ;
#159304 = CARTESIAN_POINT ( 'NONE',  ( 6.984891963203275544, -8.199734048663231079, -6.439526774796777708 ) ) ;
#159305 = CARTESIAN_POINT ( 'NONE',  ( 6.817052309572890323, 6.847649204123507083, 0.7998128361456341429 ) ) ;
#159306 = ORIENTED_EDGE ( 'NONE', *, *, #208716, .F. ) ;
#159308 =( BOUNDED_SURFACE ( )  B_SPLINE_SURFACE ( 1, 2, ( 
 ( #138439, #155747, #89697, #187162, #168783, #87545, #104873, #7332, #38791, #73409, #154677, #204457, #58241, #4122, #6262, #202325, #70191, #8410, #123338, #105975, #189302, #186091, #5185, #56111, #24655, #122269, #139512, #188226, #206611, #39866, #205539, #190355, #57176, #40942, #107048, #173074, #90762, #91836, #129728, #157894, #44139, #77683, #9486, #141669, #162153, #43087, #143804, #207680, #75559, #128664, #161078, #59300, #144867, #211937, #93967, #96098, #92899, #78743, #30014, #61437, #63572, #127603, #126526, #110260, #13740, #193569, #42017, #79813, #145925, #125458, #191420, #108126, #109200, #45212, #175212, #26794, #194632, #209801, #210874, #178402, #158945, #111327, #10540, #62499, #46274, #76614, #142727, #208736, #176269, #192487, #60363, #177330, #28944, #27871, #174153, #160008, #25726, #12668, #11609, #95028, #112390, #151230, #114525, #35317, #150166, #197824, #84078, #65667, #101395, #166397, #179466, #2799, #196770, #17988, #50518, #133941, #117719, #167469, #1734, #19065, #212999, #195712, #99282, #67791, #199948, #149079, #165330, #47347, #49456, #131815, #48413, #130775, #51595, #97163, #183709, #68871, #180520, #163218, #85143, #33199, #146982, #113461, #657, #31091, #14801, #80892, #32141, #64636, #98221, #164273, #116641, #15863, #81948, #16923, #148031, #214041, #182636, #115574, #181570, #83003, #66724, #132867, #198871, #34258, #100330, #171727, #152286, #122003, #185828, #37459, #3860, #103538, #118776, #202057, #53717, #69933, #54783, #136045, #119850, #169598, #93443, #21180, #175750, #87283, #159482, #23326, #27341, #43624, #153352, #11082, #4922, #134991, #201001, #109739, #104613, #70999, #7068, #52646, #137112, #86215, #203141, #120930, #205277, #22247, #186903, #38535, #184760, #55847, #170660, #59846, #36387, #89434, #102465, #88357, #168531, #154422, #155485, #139246, #6000, #72071, #20129, #138181, #204191, #187969, #39597, #73141, #105700, #125998, #191957, #144351, #44691, #131314, #129215, #28419, #77158, #96647, #31630, #32679, #181061, #61992, #115065, #81435, #48945, #212481, #128148, #97707, #112940, #147514, #98758, #64124, #209271, #111876, #213535, #94512, #145418, #127075, #130267, #46827, #114013, #160550, #196256, #194108, #45757, #12158, #177880, #60916, #210353, #29493, #78229, #211418, #95585, #161634, #13228, #164814, #79302, #143280, #63050, #193037, #180008, #110799, #197306, #195191, #176802, #178953, #30567, #162701, #14273, #80368, #146464, #163765, #47903, #15343, #65158, #99817, #67278, #86760, #118260, #68351, #84623, #142, #151776, #33738, #85688, #182109, #119325, #20670, #17468, #199423, #83552, #18547, #100870, #165882, #168012, #3348, #150715, #82486, #183190, #148573, #135524, #202617, #104087, #186379, #38015, #149634, #70478, #185311, #2275, #36933, #166957, #136593, #201548, #66208, #16406, #1215, #53194, #69417, #169071 ),
 ( #103016, #54267, #132355, #198358, #49998, #133417, #120403, #152829, #134484, #4407, #200486, #116121, #51067, #117190, #34796, #52132, #184244, #35871, #101946, #19616, #75840, #58525, #207959, #187452, #170136, #73706, #124680, #174435, #123623, #139803, #21721, #23874, #40151, #171204, #105165, #206894, #71553, #92122, #125742, #22797, #137661, #9766, #7620, #121481, #87832, #189587, #190638, #191703, #59585, #154966, #43362, #26011, #141947, #91048, #6551, #42298, #205831, #158174, #153903, #157109, #5473, #204746, #203682, #39080, #89980, #55330, #8698, #57463, #108412, #88912, #74782, #72629, #138728, #56397, #122558, #188519, #106264, #172286, #156030, #41233, #107340, #173362, #24944, #140881, #160290, #147250, #28155, #131057, #146200, #213282, #15080, #11893, #64908, #210085, #197045, #175492, #81170, #79030, #110543, #195998, #109484, #77967, #60648, #192767, #144089, #179747, #211152, #161370, #177620, #93186, #30297, #126811, #178684, #44426, #212214, #113743, #176544, #61724, #209012, #27079, #94251, #62776, #127892, #143017, #47632, #14010, #193843, #63851, #159219, #12952, #163497, #45492, #130007, #97441, #128938, #10819, #194916, #111609, #29229, #76893, #46554, #95321, #145146, #112674, #96382, #162434, #80096, #31365, #51878, #132094, #33481, #201288, #2014, #85430, #185045, #98489, #34542, #3083, #165619, #115860, #214313, #151515, #16138, #164552, #114798, #168813, #183990, #116926, #136333, #17207, #181845, #99554, #83283, #149368, #32422, #950, #65945, #68083, #20417, #100612, #48682, #67016, #198103, #82223, #200227, #18279, #133152, #35604, #49732, #199154, #50799, #182926, #180797, #52929, #166688, #148314, #84362, #101681, #69153, #70222, #150453, #134218, #102758, #118000, #167751, #19350, #135273, #119063, #36669, #86499, #152564, #4151, #89730, #121223, #138467, #8440, #202353, #104904, #169874, #186119, #173107, #57208, #172028, #123368, #120141, #21464, #6292, #107085, #37752, #23621, #54003, #103826, #87573, #55074, #153643, #189335, #40974, #187193, #205570, #24687, #203418, #5213, #38821, #155778, #73440, #170945, #71288, #90791, #74528, #137401, #22545, #7363, #88651, #154711, #72366, #204489, #156855, #56139, #122300, #188257, #39898, #106007, #139544, #141081, #204942, #143219, #106458, #42495, #122754, #24069, #191898, #207091, #76036, #175683, #89107, #25140, #208153, #156238, #172482, #56593, #142138, #6743, #155161, #105362, #159415, #174631, #107537, #127011, #7815, #90172, #73908, #140001, #206022, #22989, #57659, #188716, #58719, #11016, #91242, #39267, #123818, #40353, #72821, #190835, #8892, #189778, #26207, #41429, #173569, #157302, #74971, #171399, #43560, #124869, #138925, #108603, #92324, #59783, #60848, #158366, #9959, #93379, #125940, #109680, #27272, #77092, #209208, #177812, #195121, #31562, #161567, #179938, #13155, #162628, #148505, #44622, #145350 ) ),
 .UNSPECIFIED., .F., .F., .T. ) 
 B_SPLINE_SURFACE_WITH_KNOTS ( ( 2, 2 ),
 ( 3, 2, 2, 2, 2, 2, 2, 2, 2, 2, 2, 2, 2, 2, 2, 2, 2, 2, 2, 2, 2, 2, 2, 2, 2, 2, 2, 2, 2, 2, 2, 2, 2, 2, 2, 2, 2, 2, 2, 2, 2, 2, 2, 2, 2, 2, 2, 2, 2, 2, 2, 2, 2, 2, 2, 2, 2, 2, 2, 2, 2, 2, 2, 2, 2, 2, 2, 2, 2, 2, 2, 2, 2, 2, 2, 2, 2, 2, 2, 2, 2, 2, 2, 2, 2, 2, 2, 2, 2, 2, 2, 2, 2, 2, 2, 2, 2, 2, 2, 2, 2, 2, 2, 2, 2, 2, 2, 2, 2, 2, 2, 2, 2, 2, 2, 2, 2, 2, 2, 2, 2, 2, 2, 2, 2, 2, 2, 2, 2, 2, 2, 2, 2, 2, 2, 2, 2, 2, 2, 2, 2, 2, 2, 2, 2, 2, 2, 2, 2, 2, 2, 2, 2, 2, 2, 2, 2, 2, 2, 2, 2, 2, 2, 2, 2, 2, 2, 2, 3 ),
 ( 0.000000000000000000, 1.000000000000000000 ),
 ( 0.000000000000000000, 0.005952380952380952051, 0.01190476190476190410, 0.01785714285714285615, 0.02380952380952380820, 0.02976190476190476025, 0.03571428571428571230, 0.04166666666666666435, 0.04761904761904761640, 0.05357142857142856845, 0.05952380952380952051, 0.06547619047619047949, 0.07142857142857142461, 0.07738095238095238360, 0.08333333333333332871, 0.08928571428571428770, 0.09523809523809523281, 0.1011904761904761918, 0.1071428571428571369, 0.1130952380952380959, 0.1190476190476190410, 0.1250000000000000000, 0.1309523809523809590, 0.1369047619047619180, 0.1428571428571428492, 0.1488095238095238082, 0.1547619047619047672, 0.1607142857142857262, 0.1666666666666666574, 0.1726190476190476164, 0.1785714285714285754, 0.1845238095238095344, 0.1904761904761904656, 0.1964285714285714246, 0.2023809523809523836, 0.2083333333333333426, 0.2142857142857142738, 0.2202380952380952328, 0.2261904761904761918, 0.2321428571428571508, 0.2380952380952380820, 0.2440476190476190410, 0.2500000000000000000, 0.2559523809523809312, 0.2619047619047619180, 0.2678571428571428492, 0.2738095238095238360, 0.2797619047619047672, 0.2857142857142856984, 0.2916666666666666852, 0.2976190476190476164, 0.3035714285714285476, 0.3095238095238095344, 0.3154761904761904656, 0.3214285714285714524, 0.3273809523809523836, 0.3333333333333333148, 0.3392857142857143016, 0.3452380952380952328, 0.3511904761904761640, 0.3571428571428571508, 0.3630952380952380820, 0.3690476190476190688, 0.3750000000000000000, 0.3809523809523809312, 0.3869047619047619180, 0.3928571428571428492, 0.3988095238095238360, 0.4047619047619047672, 0.4107142857142856984, 0.4166666666666666852, 0.4226190476190476164, 0.4285714285714285476, 0.4345238095238095344, 0.4404761904761904656, 0.4464285714285714524, 0.4523809523809523836, 0.4583333333333333148, 0.4642857142857143016, 0.4702380952380952328, 0.4761904761904761640, 0.4821428571428571508, 0.4880952380952380820, 0.4940476190476190688, 0.5000000000000000000, 0.5059523809523809312, 0.5119047619047618625, 0.5178571428571429047, 0.5238095238095238360, 0.5297619047619047672, 0.5357142857142856984, 0.5416666666666666297, 0.5476190476190476719, 0.5535714285714286031, 0.5595238095238095344, 0.5654761904761904656, 0.5714285714285713969, 0.5773809523809523281, 0.5833333333333333703, 0.5892857142857143016, 0.5952380952380952328, 0.6011904761904761640, 0.6071428571428570953, 0.6130952380952381375, 0.6190476190476190688, 0.6250000000000000000, 0.6309523809523809312, 0.6369047619047618625, 0.6428571428571429047, 0.6488095238095238360, 0.6547619047619047672, 0.6607142857142856984, 0.6666666666666666297, 0.6726190476190476719, 0.6785714285714286031, 0.6845238095238095344, 0.6904761904761904656, 0.6964285714285713969, 0.7023809523809523281, 0.7083333333333333703, 0.7142857142857143016, 0.7202380952380952328, 0.7261904761904761640, 0.7321428571428570953, 0.7380952380952381375, 0.7440476190476190688, 0.7500000000000000000, 0.7559523809523809312, 0.7619047619047618625, 0.7678571428571429047, 0.7738095238095238360, 0.7797619047619047672, 0.7857142857142856984, 0.7916666666666666297, 0.7976190476190476719, 0.8035714285714286031, 0.8095238095238095344, 0.8154761904761904656, 0.8214285714285713969, 0.8273809523809523281, 0.8333333333333333703, 0.8392857142857143016, 0.8452380952380952328, 0.8511904761904761640, 0.8571428571428570953, 0.8630952380952381375, 0.8690476190476190688, 0.8750000000000000000, 0.8809523809523809312, 0.8869047619047618625, 0.8928571428571429047, 0.8988095238095238360, 0.9047619047619047672, 0.9107142857142856984, 0.9166666666666666297, 0.9226190476190476719, 0.9285714285714286031, 0.9345238095238095344, 0.9404761904761904656, 0.9464285714285713969, 0.9523809523809523281, 0.9583333333333333703, 0.9642857142857143016, 0.9702380952380952328, 0.9761904761904761640, 0.9821428571428570953, 0.9880952380952381375, 0.9940476190476190688, 1.000000000000000000 ),
 .UNSPECIFIED. ) 
 GEOMETRIC_REPRESENTATION_ITEM ( )  RATIONAL_B_SPLINE_SURFACE ( (
 ( 1.000000000000000000, 0.8660254037844387076, 1.000000000000000000, 0.8660254037844387076, 1.000000000000000000, 0.8660254037844387076, 1.000000000000000000, 0.8660254037844387076, 1.000000000000000000, 0.8660254037844387076, 1.000000000000000000, 0.8660254037844387076, 1.000000000000000000, 0.8660254037844387076, 1.000000000000000000, 0.8660254037844387076, 1.000000000000000000, 0.8660254037844387076, 1.000000000000000000, 0.8660254037844387076, 1.000000000000000000, 0.8660254037844387076, 1.000000000000000000, 0.8660254037844387076, 1.000000000000000000, 0.8660254037844387076, 1.000000000000000000, 0.8660254037844387076, 1.000000000000000000, 0.8660254037844387076, 1.000000000000000000, 0.8660254037844387076, 1.000000000000000000, 0.8660254037844387076, 1.000000000000000000, 0.8660254037844387076, 1.000000000000000000, 0.8660254037844387076, 1.000000000000000000, 0.8660254037844387076, 1.000000000000000000, 0.8660254037844387076, 1.000000000000000000, 0.8660254037844387076, 1.000000000000000000, 0.8660254037844387076, 1.000000000000000000, 0.8660254037844387076, 1.000000000000000000, 0.8660254037844387076, 1.000000000000000000, 0.8660254037844387076, 1.000000000000000000, 0.8660254037844387076, 1.000000000000000000, 0.8660254037844387076, 1.000000000000000000, 0.8660254037844387076, 1.000000000000000000, 0.8660254037844387076, 1.000000000000000000, 0.8660254037844387076, 1.000000000000000000, 0.8660254037844387076, 1.000000000000000000, 0.8660254037844387076, 1.000000000000000000, 0.8660254037844387076, 1.000000000000000000, 0.8660254037844387076, 1.000000000000000000, 0.8660254037844387076, 1.000000000000000000, 0.8660254037844387076, 1.000000000000000000, 0.8660254037844387076, 1.000000000000000000, 0.8660254037844387076, 1.000000000000000000, 0.8660254037844387076, 1.000000000000000000, 0.8660254037844387076, 1.000000000000000000, 0.8660254037844387076, 1.000000000000000000, 0.8660254037844387076, 1.000000000000000000, 0.8660254037844387076, 1.000000000000000000, 0.8660254037844387076, 1.000000000000000000, 0.8660254037844387076, 1.000000000000000000, 0.8660254037844387076, 1.000000000000000000, 0.8660254037844387076, 1.000000000000000000, 0.8660254037844387076, 1.000000000000000000, 0.8660254037844387076, 1.000000000000000000, 0.8660254037844387076, 1.000000000000000000, 0.8660254037844387076, 1.000000000000000000, 0.8660254037844387076, 1.000000000000000000, 0.8660254037844387076, 1.000000000000000000, 0.8660254037844387076, 1.000000000000000000, 0.8660254037844387076, 1.000000000000000000, 0.8660254037844387076, 1.000000000000000000, 0.8660254037844387076, 1.000000000000000000, 0.8660254037844387076, 1.000000000000000000, 0.8660254037844387076, 1.000000000000000000, 0.8660254037844387076, 1.000000000000000000, 0.8660254037844387076, 1.000000000000000000, 0.8660254037844387076, 1.000000000000000000, 0.8660254037844387076, 1.000000000000000000, 0.8660254037844387076, 1.000000000000000000, 0.8660254037844387076, 1.000000000000000000, 0.8660254037844387076, 1.000000000000000000, 0.8660254037844387076, 1.000000000000000000, 0.8660254037844387076, 1.000000000000000000, 0.8660254037844387076, 1.000000000000000000, 0.8660254037844387076, 1.000000000000000000, 0.8660254037844387076, 1.000000000000000000, 0.8660254037844387076, 1.000000000000000000, 0.8660254037844387076, 1.000000000000000000, 0.8660254037844387076, 1.000000000000000000, 0.8660254037844387076, 1.000000000000000000, 0.8660254037844387076, 1.000000000000000000, 0.8660254037844387076, 1.000000000000000000, 0.8660254037844387076, 1.000000000000000000, 0.8660254037844387076, 1.000000000000000000, 0.8660254037844387076, 1.000000000000000000, 0.8660254037844387076, 1.000000000000000000, 0.8660254037844387076, 1.000000000000000000, 0.8660254037844387076, 1.000000000000000000, 0.8660254037844387076, 1.000000000000000000, 0.8660254037844387076, 1.000000000000000000, 0.8660254037844387076, 1.000000000000000000, 0.8660254037844387076, 1.000000000000000000, 0.8660254037844387076, 1.000000000000000000, 0.8660254037844387076, 1.000000000000000000, 0.8660254037844387076, 1.000000000000000000, 0.8660254037844387076, 1.000000000000000000, 0.8660254037844387076, 1.000000000000000000, 0.8660254037844387076, 1.000000000000000000, 0.8660254037844387076, 1.000000000000000000, 0.8660254037844387076, 1.000000000000000000, 0.8660254037844387076, 1.000000000000000000, 0.8660254037844387076, 1.000000000000000000, 0.8660254037844387076, 1.000000000000000000, 0.8660254037844387076, 1.000000000000000000, 0.8660254037844387076, 1.000000000000000000, 0.8660254037844387076, 1.000000000000000000, 0.8660254037844387076, 1.000000000000000000, 0.8660254037844387076, 1.000000000000000000, 0.8660254037844387076, 1.000000000000000000, 0.8660254037844387076, 1.000000000000000000, 0.8660254037844387076, 1.000000000000000000, 0.8660254037844387076, 1.000000000000000000, 0.8660254037844387076, 1.000000000000000000, 0.8660254037844387076, 1.000000000000000000, 0.8660254037844387076, 1.000000000000000000, 0.8660254037844387076, 1.000000000000000000, 0.8660254037844387076, 1.000000000000000000, 0.8660254037844387076, 1.000000000000000000, 0.8660254037844387076, 1.000000000000000000, 0.8660254037844387076, 1.000000000000000000, 0.8660254037844387076, 1.000000000000000000, 0.8660254037844387076, 1.000000000000000000, 0.8660254037844387076, 1.000000000000000000, 0.8660254037844387076, 1.000000000000000000, 0.8660254037844387076, 1.000000000000000000, 0.8660254037844387076, 1.000000000000000000, 0.8660254037844387076, 1.000000000000000000, 0.8660254037844387076, 1.000000000000000000, 0.8660254037844387076, 1.000000000000000000, 0.8660254037844387076, 1.000000000000000000, 0.8660254037844387076, 1.000000000000000000, 0.8660254037844387076, 1.000000000000000000, 0.8660254037844387076, 1.000000000000000000, 0.8660254037844387076, 1.000000000000000000, 0.8660254037844387076, 1.000000000000000000, 0.8660254037844387076, 1.000000000000000000, 0.8660254037844387076, 1.000000000000000000, 0.8660254037844387076, 1.000000000000000000, 0.8660254037844387076, 1.000000000000000000, 0.8660254037844387076, 1.000000000000000000, 0.8660254037844387076, 1.000000000000000000, 0.8660254037844387076, 1.000000000000000000, 0.8660254037844387076, 1.000000000000000000, 0.8660254037844387076, 1.000000000000000000, 0.8660254037844387076, 1.000000000000000000, 0.8660254037844387076, 1.000000000000000000, 0.8660254037844387076, 1.000000000000000000, 0.8660254037844387076, 1.000000000000000000, 0.8660254037844387076, 1.000000000000000000, 0.8660254037844387076, 1.000000000000000000, 0.8660254037844387076, 1.000000000000000000, 0.8660254037844387076, 1.000000000000000000, 0.8660254037844387076, 1.000000000000000000, 0.8660254037844387076, 1.000000000000000000, 0.8660254037844387076, 1.000000000000000000, 0.8660254037844387076, 1.000000000000000000, 0.8660254037844387076, 1.000000000000000000, 0.8660254037844387076, 1.000000000000000000, 0.8660254037844387076, 1.000000000000000000, 0.8660254037844387076, 1.000000000000000000, 0.8660254037844387076, 1.000000000000000000, 0.8660254037844387076, 1.000000000000000000, 0.8660254037844387076, 1.000000000000000000, 0.8660254037844387076, 1.000000000000000000, 0.8660254037844387076, 1.000000000000000000, 0.8660254037844387076, 1.000000000000000000, 0.8660254037844387076, 1.000000000000000000, 0.8660254037844387076, 1.000000000000000000, 0.8660254037844387076, 1.000000000000000000, 0.8660254037844387076, 1.000000000000000000, 0.8660254037844387076, 1.000000000000000000, 0.8660254037844387076, 1.000000000000000000),
 ( 1.000000000000000000, 0.8660254037844387076, 1.000000000000000000, 0.8660254037844387076, 1.000000000000000000, 0.8660254037844387076, 1.000000000000000000, 0.8660254037844387076, 1.000000000000000000, 0.8660254037844387076, 1.000000000000000000, 0.8660254037844387076, 1.000000000000000000, 0.8660254037844387076, 1.000000000000000000, 0.8660254037844387076, 1.000000000000000000, 0.8660254037844387076, 1.000000000000000000, 0.8660254037844387076, 1.000000000000000000, 0.8660254037844387076, 1.000000000000000000, 0.8660254037844387076, 1.000000000000000000, 0.8660254037844387076, 1.000000000000000000, 0.8660254037844387076, 1.000000000000000000, 0.8660254037844387076, 1.000000000000000000, 0.8660254037844387076, 1.000000000000000000, 0.8660254037844387076, 1.000000000000000000, 0.8660254037844387076, 1.000000000000000000, 0.8660254037844387076, 1.000000000000000000, 0.8660254037844387076, 1.000000000000000000, 0.8660254037844387076, 1.000000000000000000, 0.8660254037844387076, 1.000000000000000000, 0.8660254037844387076, 1.000000000000000000, 0.8660254037844387076, 1.000000000000000000, 0.8660254037844387076, 1.000000000000000000, 0.8660254037844387076, 1.000000000000000000, 0.8660254037844387076, 1.000000000000000000, 0.8660254037844387076, 1.000000000000000000, 0.8660254037844387076, 1.000000000000000000, 0.8660254037844387076, 1.000000000000000000, 0.8660254037844387076, 1.000000000000000000, 0.8660254037844387076, 1.000000000000000000, 0.8660254037844387076, 1.000000000000000000, 0.8660254037844387076, 1.000000000000000000, 0.8660254037844387076, 1.000000000000000000, 0.8660254037844387076, 1.000000000000000000, 0.8660254037844387076, 1.000000000000000000, 0.8660254037844387076, 1.000000000000000000, 0.8660254037844387076, 1.000000000000000000, 0.8660254037844387076, 1.000000000000000000, 0.8660254037844387076, 1.000000000000000000, 0.8660254037844387076, 1.000000000000000000, 0.8660254037844387076, 1.000000000000000000, 0.8660254037844387076, 1.000000000000000000, 0.8660254037844387076, 1.000000000000000000, 0.8660254037844387076, 1.000000000000000000, 0.8660254037844387076, 1.000000000000000000, 0.8660254037844387076, 1.000000000000000000, 0.8660254037844387076, 1.000000000000000000, 0.8660254037844387076, 1.000000000000000000, 0.8660254037844387076, 1.000000000000000000, 0.8660254037844387076, 1.000000000000000000, 0.8660254037844387076, 1.000000000000000000, 0.8660254037844387076, 1.000000000000000000, 0.8660254037844387076, 1.000000000000000000, 0.8660254037844387076, 1.000000000000000000, 0.8660254037844387076, 1.000000000000000000, 0.8660254037844387076, 1.000000000000000000, 0.8660254037844387076, 1.000000000000000000, 0.8660254037844387076, 1.000000000000000000, 0.8660254037844387076, 1.000000000000000000, 0.8660254037844387076, 1.000000000000000000, 0.8660254037844387076, 1.000000000000000000, 0.8660254037844387076, 1.000000000000000000, 0.8660254037844387076, 1.000000000000000000, 0.8660254037844387076, 1.000000000000000000, 0.8660254037844387076, 1.000000000000000000, 0.8660254037844387076, 1.000000000000000000, 0.8660254037844387076, 1.000000000000000000, 0.8660254037844387076, 1.000000000000000000, 0.8660254037844387076, 1.000000000000000000, 0.8660254037844387076, 1.000000000000000000, 0.8660254037844387076, 1.000000000000000000, 0.8660254037844387076, 1.000000000000000000, 0.8660254037844387076, 1.000000000000000000, 0.8660254037844387076, 1.000000000000000000, 0.8660254037844387076, 1.000000000000000000, 0.8660254037844387076, 1.000000000000000000, 0.8660254037844387076, 1.000000000000000000, 0.8660254037844387076, 1.000000000000000000, 0.8660254037844387076, 1.000000000000000000, 0.8660254037844387076, 1.000000000000000000, 0.8660254037844387076, 1.000000000000000000, 0.8660254037844387076, 1.000000000000000000, 0.8660254037844387076, 1.000000000000000000, 0.8660254037844387076, 1.000000000000000000, 0.8660254037844387076, 1.000000000000000000, 0.8660254037844387076, 1.000000000000000000, 0.8660254037844387076, 1.000000000000000000, 0.8660254037844387076, 1.000000000000000000, 0.8660254037844387076, 1.000000000000000000, 0.8660254037844387076, 1.000000000000000000, 0.8660254037844387076, 1.000000000000000000, 0.8660254037844387076, 1.000000000000000000, 0.8660254037844387076, 1.000000000000000000, 0.8660254037844387076, 1.000000000000000000, 0.8660254037844387076, 1.000000000000000000, 0.8660254037844387076, 1.000000000000000000, 0.8660254037844387076, 1.000000000000000000, 0.8660254037844387076, 1.000000000000000000, 0.8660254037844387076, 1.000000000000000000, 0.8660254037844387076, 1.000000000000000000, 0.8660254037844387076, 1.000000000000000000, 0.8660254037844387076, 1.000000000000000000, 0.8660254037844387076, 1.000000000000000000, 0.8660254037844387076, 1.000000000000000000, 0.8660254037844387076, 1.000000000000000000, 0.8660254037844387076, 1.000000000000000000, 0.8660254037844387076, 1.000000000000000000, 0.8660254037844387076, 1.000000000000000000, 0.8660254037844387076, 1.000000000000000000, 0.8660254037844387076, 1.000000000000000000, 0.8660254037844387076, 1.000000000000000000, 0.8660254037844387076, 1.000000000000000000, 0.8660254037844387076, 1.000000000000000000, 0.8660254037844387076, 1.000000000000000000, 0.8660254037844387076, 1.000000000000000000, 0.8660254037844387076, 1.000000000000000000, 0.8660254037844387076, 1.000000000000000000, 0.8660254037844387076, 1.000000000000000000, 0.8660254037844387076, 1.000000000000000000, 0.8660254037844387076, 1.000000000000000000, 0.8660254037844387076, 1.000000000000000000, 0.8660254037844387076, 1.000000000000000000, 0.8660254037844387076, 1.000000000000000000, 0.8660254037844387076, 1.000000000000000000, 0.8660254037844387076, 1.000000000000000000, 0.8660254037844387076, 1.000000000000000000, 0.8660254037844387076, 1.000000000000000000, 0.8660254037844387076, 1.000000000000000000, 0.8660254037844387076, 1.000000000000000000, 0.8660254037844387076, 1.000000000000000000, 0.8660254037844387076, 1.000000000000000000, 0.8660254037844387076, 1.000000000000000000, 0.8660254037844387076, 1.000000000000000000, 0.8660254037844387076, 1.000000000000000000, 0.8660254037844387076, 1.000000000000000000, 0.8660254037844387076, 1.000000000000000000, 0.8660254037844387076, 1.000000000000000000, 0.8660254037844387076, 1.000000000000000000, 0.8660254037844387076, 1.000000000000000000, 0.8660254037844387076, 1.000000000000000000, 0.8660254037844387076, 1.000000000000000000, 0.8660254037844387076, 1.000000000000000000, 0.8660254037844387076, 1.000000000000000000, 0.8660254037844387076, 1.000000000000000000, 0.8660254037844387076, 1.000000000000000000, 0.8660254037844387076, 1.000000000000000000, 0.8660254037844387076, 1.000000000000000000, 0.8660254037844387076, 1.000000000000000000, 0.8660254037844387076, 1.000000000000000000, 0.8660254037844387076, 1.000000000000000000, 0.8660254037844387076, 1.000000000000000000, 0.8660254037844387076, 1.000000000000000000, 0.8660254037844387076, 1.000000000000000000, 0.8660254037844387076, 1.000000000000000000, 0.8660254037844387076, 1.000000000000000000, 0.8660254037844387076, 1.000000000000000000, 0.8660254037844387076, 1.000000000000000000, 0.8660254037844387076, 1.000000000000000000, 0.8660254037844387076, 1.000000000000000000, 0.8660254037844387076, 1.000000000000000000, 0.8660254037844387076, 1.000000000000000000, 0.8660254037844387076, 1.000000000000000000, 0.8660254037844387076, 1.000000000000000000, 0.8660254037844387076, 1.000000000000000000, 0.8660254037844387076, 1.000000000000000000, 0.8660254037844387076, 1.000000000000000000) ) ) 
 REPRESENTATION_ITEM ( '' )  SURFACE ( )  );
#159307 = CARTESIAN_POINT ( 'NONE',  ( -11.89317557362582356, 13.76275843837616542, -1.599935658896116664 ) ) ;
#159309 = AXIS2_PLACEMENT_3D ( 'NONE', #173023, #90713, #205490 ) ;
#159310 = CARTESIAN_POINT ( 'NONE',  ( 2.385177931559249398, 0.08740048966574034961, -1.809473338476126569 ) ) ;
#159311 = CARTESIAN_POINT ( 'NONE',  ( -6.878064000834399394, 6.918829510595249310, -0.7998128361456291469 ) ) ;
#159312 = ORIENTED_EDGE ( 'NONE', *, *, #144045, .F. ) ;
#159313 = CARTESIAN_POINT ( 'NONE',  ( 4.864678189204997949, 4.569879397027603929, 0.7998128361456341429 ) ) ;
#159314 = ORIENTED_EDGE ( 'NONE', *, *, #21930, .F. ) ;
#159315 = CARTESIAN_POINT ( 'NONE',  ( 5.061990249855835344, 6.999017606288844284, -1.599625672291273171 ) ) ;
#159316 = CARTESIAN_POINT ( 'NONE',  ( 4.266123773889715309, 1.810994338341217480, -0.04873877536224096446 ) ) ;
#159317 = CARTESIAN_POINT ( 'NONE',  ( 6.639320575229290533, 2.050619746573784763, 2.302922995531462291 ) ) ;
#159318 = FACE_OUTER_BOUND ( 'NONE', #59442, .T. ) ;
#159319 = CARTESIAN_POINT ( 'NONE',  ( 4.815628398899983509, 6.730757278346135131, 1.248813279183153657 ) ) ;
#159320 = ORIENTED_EDGE ( 'NONE', *, *, #44682, .F. ) ;
#159321 = CARTESIAN_POINT ( 'NONE',  ( 3.965176940185519250, 1.595341564286660629, 0.9581005465538834365 ) ) ;
#159322 = CARTESIAN_POINT ( 'NONE',  ( 1.405720392582618938, -1.065544983005232371, -1.591680324291492310 ) ) ;
#159323 = CARTESIAN_POINT ( 'NONE',  ( 1.395219695971817941, 1.379742824092672349, 1.195523663710513995 ) ) ;
#159324 = CARTESIAN_POINT ( 'NONE',  ( 1.499902018610889343, 4.449786617651237286, -0.08390812002217802601 ) ) ;
#159325 = DIRECTION ( 'NONE',  ( 3.330669073875478989E-16, -3.540251991789410786E-16, -1.000000000000000000 ) ) ;
#159326 = CARTESIAN_POINT ( 'NONE',  ( 5.886377668569586774, 7.162856863344262415, 1.137212067324339104 ) ) ;
#159327 = CARTESIAN_POINT ( 'NONE',  ( 6.095239321792044862, 7.114357098804711121, 1.141570887979098448 ) ) ;
#159328 = CARTESIAN_POINT ( 'NONE',  ( 0.000000000000000000, -1.000000000000000888, 10.24999999999998934 ) ) ;
#159329 = CARTESIAN_POINT ( 'NONE',  ( -4.092446641025072829, 3.979529022206003575, 0.4031905389056175126 ) ) ;
#159330 = CARTESIAN_POINT ( 'NONE',  ( 7.280365300858406385, 11.43758391773608984, 1.040834085586084257E-14 ) ) ;
#159331 = CARTESIAN_POINT ( 'NONE',  ( 5.541845313694261144, 1.319919544752303331, 1.461889559981154108 ) ) ;
#159332 = CARTESIAN_POINT ( 'NONE',  ( -4.904298879841297421, 6.744767997946721216, 1.599625672291267398 ) ) ;
#159333 = CARTESIAN_POINT ( 'NONE',  ( -11.96535697748077887, 9.847373329355578520, -0.9148528286455027692 ) ) ;
#159334 = CARTESIAN_POINT ( 'NONE',  ( 0.3047781727255130524, 1.820093451774043691, 1.028452505696121344 ) ) ;
#159335 = CARTESIAN_POINT ( 'NONE',  ( 7.259501185113382604, 10.55683625168592243, -1.199719254218441611 ) ) ;
#159336 = CARTESIAN_POINT ( 'NONE',  ( 5.315425438393720725, -0.2827910679824903184, 1.905415604636887750 ) ) ;
#159337 = CARTESIAN_POINT ( 'NONE',  ( -5.555090253297260361, 7.504024600312024340, 1.599625672291269396 ) ) ;
#159338 = CARTESIAN_POINT ( 'NONE',  ( 1.324926479183065497, -0.04897172810776688479, 1.825096452545173609 ) ) ;
#159339 = CARTESIAN_POINT ( 'NONE',  ( 1.928631425534212074, 1.268998755960360603, -1.805353087401928569 ) ) ;
#159340 = CARTESIAN_POINT ( 'NONE',  ( 0.8965662283535699162, -1.866366896104875162, -0.4163465257057268332 ) ) ;
#159341 = B_SPLINE_CURVE_WITH_KNOTS ( 'NONE', 3,
 ( #42610, #121786, #89220, #156348, #108719, #7932, #205061, #24175, #142251, #208263, #192011, #43674, #40466, #64176, #78275, #176854 ),
 .UNSPECIFIED., .F., .F.,
 ( 4, 3, 3, 3, 3, 4 ),
 ( 0.000000000000000000, 2.209015272824978271E-05, 5.594181769345698359E-05, 8.979300607464787737E-05, 0.0001236442050441801050, 0.0001574956163004470730 ),
 .UNSPECIFIED. ) ;
#159342 = CARTESIAN_POINT ( 'NONE',  ( 6.860212146170862724, -1.969081375482661267, 0.04489377202578949400 ) ) ;
#159343 = CARTESIAN_POINT ( 'NONE',  ( 3.069799403425711226, -1.154559939549955949, 1.561474065217777207 ) ) ;
#159344 = ORIENTED_EDGE ( 'NONE', *, *, #144969, .F. ) ;
#159345 = CARTESIAN_POINT ( 'NONE',  ( 1.106795812180675798, 0.8196504822069600182, -1.842164015508622521 ) ) ;
#159347 = CARTESIAN_POINT ( 'NONE',  ( 6.473497990634856869, -0.2285008921534004422, 1.846817554525240990 ) ) ;
#159346 = CARTESIAN_POINT ( 'NONE',  ( -6.143779885648060102, 7.196773283791382703, 1.199719254218452047 ) ) ;
#159348 = CARTESIAN_POINT ( 'NONE',  ( 4.655245641445829641, 6.524482229810530498, 1.599625672291269396 ) ) ;
#159349 = CARTESIAN_POINT ( 'NONE',  ( 0.03870269234684881043, -9.454881121928412568, -9.603712783164930045 ) ) ;
#159350 = CARTESIAN_POINT ( 'NONE',  ( -7.719547554928817945, -5.360178282914185743, -7.836475020641948674 ) ) ;
#159351 = CARTESIAN_POINT ( 'NONE',  ( -4.066556009095094737, 6.831733546331167695, 1.199719254218464037 ) ) ;
#159352 = CARTESIAN_POINT ( 'NONE',  ( -5.237192476628793614, 9.332084666034067055, 0.7998128361456291469 ) ) ;
#159353 = CARTESIAN_POINT ( 'NONE',  ( 3.087623348389135547, -0.8860277256741244667, 2.004638750299721828 ) ) ;
#159354 = CARTESIAN_POINT ( 'NONE',  ( 3.226477370372302644, 5.747678784534228313, 1.082531754730546636 ) ) ;
#159355 = CARTESIAN_POINT ( 'NONE',  ( 7.014364370223726830, 9.276787413384745662, -1.599625672291269396 ) ) ;
#159356 = CARTESIAN_POINT ( 'NONE',  ( 1.195384358724066508E-16, -4.140708350189171938, 1.000000000000004441 ) ) ;
#159357 = CARTESIAN_POINT ( 'NONE',  ( 2.314841291766779108, 1.630546960418734148, 0.8213866120303781049 ) ) ;
#159358 = DIRECTION ( 'NONE',  ( 0.000000000000000000, 0.000000000000000000, 1.000000000000000000 ) ) ;
#159359 = CARTESIAN_POINT ( 'NONE',  ( -2.428882075142555497, 5.985446187641602300, 1.040834085586084257E-14 ) ) ;
#159360 = CARTESIAN_POINT ( 'NONE',  ( -5.880564528862151974, 7.271459349814712425, -1.272365726499018246 ) ) ;
#159361 = CARTESIAN_POINT ( 'NONE',  ( -0.02968770228137588424, 5.725071598255107475, -2.420367217772397606 ) ) ;
#159362 = CARTESIAN_POINT ( 'NONE',  ( 9.028840231696797503, 12.62106513936658203, -1.199719254218446718 ) ) ;
#159363 = CARTESIAN_POINT ( 'NONE',  ( 1.488762753728092969, -0.2822029396061729867, -1.905608977972670370 ) ) ;
#159364 = CARTESIAN_POINT ( 'NONE',  ( 5.506681978947471912, 0.5658967987182733639, 1.878394690154854496 ) ) ;
#159365 = CARTESIAN_POINT ( 'NONE',  ( -0.7500000000000006661, 14.70833333333333748, -1.299038105676657340 ) ) ;
#159366 = CARTESIAN_POINT ( 'NONE',  ( -6.204827856548512877, 10.39071626594860476, -0.7998128361456291469 ) ) ;
#159367 = CARTESIAN_POINT ( 'NONE',  ( 3.811813743736467419, 7.598866467667865443, 1.040834085586084257E-14 ) ) ;
#159368 = ADVANCED_FACE ( 'NONE', ( #91675 ), #32330, .F. ) ;
#159369 = CARTESIAN_POINT ( 'NONE',  ( 5.390230798962840630, -0.5317533105795355652, -2.125930911514521959 ) ) ;
#159370 = COLOUR_RGB ( '', 0.72549020, 0.75294118, 0.79215686) ;
#159371 = CARTESIAN_POINT ( 'NONE',  ( 4.174301041578287297, 5.728379888396370134, 1.537733183400904036 ) ) ;
#159372 = CARTESIAN_POINT ( 'NONE',  ( 3.573154620739454224, 1.869565233029608198, 0.8895530118792621677 ) ) ;
#159374 = CARTESIAN_POINT ( 'NONE',  ( -1.201851678989727383E-14, 1.634375000341421025, 1.575800808251672791 ) ) ;
#159373 = DIRECTION ( 'NONE',  ( -1.000000000000000000, 0.000000000000000000, 0.000000000000000000 ) ) ;
#159375 = ORIENTED_EDGE ( 'NONE', *, *, #63361, .T. ) ;
#159376 = CARTESIAN_POINT ( 'NONE',  ( 4.465672607755381662, -2.229637596627360718, -0.5588700134179708234 ) ) ;
#159377 = CARTESIAN_POINT ( 'NONE',  ( 6.968527767744098433, 9.153035033833367251, 1.443375672974076540 ) ) ;
#159379 = CARTESIAN_POINT ( 'NONE',  ( -1.642778471874998480, -0.7510416661887092671, 2.845375778867863303 ) ) ;
#159378 = CARTESIAN_POINT ( 'NONE',  ( 6.373741612200174878, 6.608655767087927124, 0.7216878364870328300 ) ) ;
#159380 = CARTESIAN_POINT ( 'NONE',  ( -7.808923410443597390, -5.575271019048065213, -7.747753938335034007 ) ) ;
#159381 = CARTESIAN_POINT ( 'NONE',  ( -5.901542003698421190, 10.10715911428198055, 0.000000000000000000 ) ) ;
#159382 = CARTESIAN_POINT ( 'NONE',  ( 3.978411374042570170, -0.1916562231945718731, -1.932471992628071789 ) ) ;
#159383 = ORIENTED_EDGE ( 'NONE', *, *, #197793, .T. ) ;
#159385 = ADVANCED_FACE ( 'NONE', ( #45052 ), #93804, .T. ) ;
#159384 = CARTESIAN_POINT ( 'NONE',  ( 8.378575743120986630, 12.71882943370911789, 1.040834085586084257E-14 ) ) ;
#159386 = ORIENTED_EDGE ( 'NONE', *, *, #156570, .F. ) ;
#159387 = CARTESIAN_POINT ( 'NONE',  ( 5.431871263539022721, -1.864374737420209760, 0.4251265778823994368 ) ) ;
#159388 = CARTESIAN_POINT ( 'NONE',  ( 6.792093547228882144, -0.7321312287554645470, 1.560492760358098918 ) ) ;
#159389 = CARTESIAN_POINT ( 'NONE',  ( 4.839077477813122918, -1.706110771555340744, -1.074664961451990308 ) ) ;
#159391 = FACE_OUTER_BOUND ( 'NONE', #3526, .T. ) ;
#159390 = CARTESIAN_POINT ( 'NONE',  ( -7.804689982961090955, 12.25722208009664094, 0.7998128361456481317 ) ) ;
#159392 = CARTESIAN_POINT ( 'NONE',  ( -3.285556943750000514, -0.1385416661887106660, -1.896917185911906500 ) ) ;
#159394 = CARTESIAN_POINT ( 'NONE',  ( 6.889980056308100842, -0.7542815031014777905, 1.599730008835710482 ) ) ;
#159393 = CARTESIAN_POINT ( 'NONE',  ( 1.218821504741087969, -0.04963993015681333193, 2.090216850290891326 ) ) ;
#159395 = CARTESIAN_POINT ( 'NONE',  ( 5.889296118903345700, -0.7283762112263308941, -1.880435897373772258 ) ) ;
#159397 = CARTESIAN_POINT ( 'NONE',  ( 3.609589514692018053, -2.258491968568816066, 0.3911977494595666460 ) ) ;
#159396 = CARTESIAN_POINT ( 'NONE',  ( 4.573896719763862251, 6.429575154514868274, -1.599625672291273171 ) ) ;
#159398 = CARTESIAN_POINT ( 'NONE',  ( 0.6908507670086707630, -0.6304954947415147837, 1.622297741125192427 ) ) ;
#159399 = CARTESIAN_POINT ( 'NONE',  ( 3.164422831683691761, 2.120778211551369807, -0.003951117757632071313 ) ) ;
#159400 = DIRECTION ( 'NONE',  ( -1.000000000000000000, 5.578564026256504688E-16, 0.000000000000000000 ) ) ;
#159401 = CARTESIAN_POINT ( 'NONE',  ( 0.5437846328400409712, 1.620832503561630666, -0.6162787013818531445 ) ) ;
#159402 = CARTESIAN_POINT ( 'NONE',  ( -0.6801582343750177673, 1.713541667008065872, 1.178068619123799898 ) ) ;
#159403 = CARTESIAN_POINT ( 'NONE',  ( 1.275590745840638363, -1.816738662498600165, 0.4029602180237248366 ) ) ;
#159404 = CARTESIAN_POINT ( 'NONE',  ( 0.7839114044838908502, -2.061656150924387365, 0.6811309647984428173 ) ) ;
#159405 = CARTESIAN_POINT ( 'NONE',  ( 2.993375309983861143, -0.3886322325962355273, 1.978555244300662874 ) ) ;
#159406 = CARTESIAN_POINT ( 'NONE',  ( 4.187500000000002665, -1.451031289060945584, 1.451031289061284646 ) ) ;
#159407 = CARTESIAN_POINT ( 'NONE',  ( -1.500000000000013101, 1.202083334016148974, 0.8660254037844403729 ) ) ;
#159408 = CARTESIAN_POINT ( 'NONE',  ( 6.639296574806412110, -1.719437650081551139, 0.8690664522189944785 ) ) ;
#159409 = CARTESIAN_POINT ( 'NONE',  ( 1.364683531249997417, 13.98437500034140157, 2.602085213965210642E-15 ) ) ;
#159410 = CARTESIAN_POINT ( 'NONE',  ( 2.918465973627711652, -2.218669909917521998, 0.1131645065166643205 ) ) ;
#159411 = EDGE_LOOP ( 'NONE', ( #146620, #60293, #62055, #152751 ) ) ;
#159412 = PRESENTATION_STYLE_ASSIGNMENT (( #22986 ) ) ;
#159414 = EDGE_CURVE ( 'NONE', #37959, #182199, #9542, .T. ) ;
#159413 = CARTESIAN_POINT ( 'NONE',  ( 8.938903350111612411, 9.323142084752035430, -0.7998128361456221525 ) ) ;
#159415 = CARTESIAN_POINT ( 'NONE',  ( 0.6823417656249882723, -0.1572916663252488245, 1.181850606188755259 ) ) ;
#159416 = CARTESIAN_POINT ( 'NONE',  ( 6.398696371038459674, -2.178289998122169280, -0.4347530419120289036 ) ) ;
#159418 = CARTESIAN_POINT ( 'NONE',  ( 4.967221142815226642, 1.706001049663580460, 0.9686458024478412643 ) ) ;
#159417 = MECHANICAL_DESIGN_GEOMETRIC_PRESENTATION_REPRESENTATION (  '', ( #45191 ), #197441 ) ;
#159420 = CARTESIAN_POINT ( 'NONE',  ( -6.724481002698130538, 7.907944593645035880, -1.082531754730544860 ) ) ;
#159419 = CARTESIAN_POINT ( 'NONE',  ( 8.568389894156670294, 12.94027927658408217, -0.7216878364870257245 ) ) ;
#159421 = DIRECTION ( 'NONE',  ( 1.039099362110107450E-15, 1.000000000000000000, -4.583713267641621330E-32 ) ) ;
#159422 = CARTESIAN_POINT ( 'NONE',  ( 6.186863813140405455, -0.3229369685709322924, -2.239133911541963506 ) ) ;
#159423 = CARTESIAN_POINT ( 'NONE',  ( 2.277848244636628827, -2.001361501815647870, 0.4987805053587587856 ) ) ;
#159424 = CARTESIAN_POINT ( 'NONE',  ( -6.552668314106420588, 6.539201209412602189, -0.7998128361456291469 ) ) ;
#159425 = ORIENTED_EDGE ( 'NONE', *, *, #207810, .T. ) ;
#159427 = EDGE_CURVE ( 'NONE', #1801, #113056, #62178, .T. ) ;
#159426 = CARTESIAN_POINT ( 'NONE',  ( -1.402160292154681736E-14, 0.8687500006828192678, -1.732050807568863648 ) ) ;
#159428 = CARTESIAN_POINT ( 'NONE',  ( 3.268673085221412311, -1.727008210369033847, -0.7190761260571986169 ) ) ;
#159429 = CARTESIAN_POINT ( 'NONE',  ( 2.338123177510130102, 0.4612838472501363252, -1.671594290515050041 ) ) ;
#159430 = CARTESIAN_POINT ( 'NONE',  ( 0.1524363970008953684, 0.8851206712186098224, 2.114804356544320640 ) ) ;
#159431 = CARTESIAN_POINT ( 'NONE',  ( 1.079469989902905214, -0.05558308599296066244, -2.206230565744627281 ) ) ;
#159432 = CARTESIAN_POINT ( 'NONE',  ( 3.520547545725543515, 1.372905562624787024, -1.669742455111824286 ) ) ;
#159433 = CARTESIAN_POINT ( 'NONE',  ( 5.437426780092255996, 0.7852709207246920675, -1.776270868113111856 ) ) ;
#159434 = ADVANCED_FACE ( 'NONE', ( #143642 ), #13584, .F. ) ;
#159435 = CARTESIAN_POINT ( 'NONE',  ( 0.000000000000000000, 0.000000000000000000, 0.000000000000000000 ) ) ;
#159436 = CARTESIAN_POINT ( 'NONE',  ( 0.03128095451081137207, -0.7860540964617872550, -1.895863743164089676 ) ) ;
#159437 = CARTESIAN_POINT ( 'NONE',  ( -0.1399997263889594112, -0.002789056014654289761, -2.000146600338557956 ) ) ;
#159438 = CARTESIAN_POINT ( 'NONE',  ( -15.75000000000000000, 10.90000000000000036, 1.099999999999996758 ) ) ;
#159439 = CARTESIAN_POINT ( 'NONE',  ( -1.360316468750056851, 2.119791667008092073, -0.7853790794159083433 ) ) ;
#159440 =( LENGTH_UNIT ( ) NAMED_UNIT ( * ) SI_UNIT ( .MILLI., .METRE. ) );
#159441 = CARTESIAN_POINT ( 'NONE',  ( -7.343712760096452463, 11.71941532008788833, -0.7998128361456291469 ) ) ;
#159442 = CARTESIAN_POINT ( 'NONE',  ( 7.308008492965924141, 8.484763649003774333, -1.199719254218451159 ) ) ;
#159443 = CARTESIAN_POINT ( 'NONE',  ( 2.665936209291948078, -0.4260822056534815938, -0.1252292841820018543 ) ) ;
#159444 = CARTESIAN_POINT ( 'NONE',  ( 3.580510235063854019, -1.759844519496515325, -0.4856381957471164745 ) ) ;
#159445 = CARTESIAN_POINT ( 'NONE',  ( 2.485638465518677176, 2.017858404210779888, -0.8937526715337427152 ) ) ;
#159446 = EDGE_LOOP ( 'NONE', ( #211783, #25842, #208081, #40652, #130884 ) ) ;
#159447 = CARTESIAN_POINT ( 'NONE',  ( -6.312203035614172286, 9.521931420595302953, -1.199719254218452047 ) ) ;
#159448 = UNCERTAINTY_MEASURE_WITH_UNIT (LENGTH_MEASURE( 1.000000000000000082E-05 ), #213381, 'distance_accuracy_value', 'NONE');
#159449 = CARTESIAN_POINT ( 'NONE',  ( -1.642778471875000035, -3.055208332855375630, -2.845375778867859751 ) ) ;
#159450 = CARTESIAN_POINT ( 'NONE',  ( -6.970863535720637216, 11.28442455831609337, 0.7998128361456481317 ) ) ;
#159451 = CARTESIAN_POINT ( 'NONE',  ( 0.7561249178302269502, 0.8145892717734238841, -1.848413388458100215 ) ) ;
#159452 = CARTESIAN_POINT ( 'NONE',  ( 1.418772191123615078, -0.7664089246972278779, -1.977313068770427229 ) ) ;
#159453 = CARTESIAN_POINT ( 'NONE',  ( 6.224601922449876312, 6.434659462379210382, 0.000000000000000000 ) ) ;
#159454 = CARTESIAN_POINT ( 'NONE',  ( -6.147696309153835692, 6.137010213626392208, 0.7998128361456281477 ) ) ;
#159455 = CARTESIAN_POINT ( 'NONE',  ( 3.502650316321722634, 0.4479755722775873861, 1.806107967122023927 ) ) ;
#159456 = CARTESIAN_POINT ( 'NONE',  ( 3.029357257649615054, 5.621668336311468117, -1.199719254218446718 ) ) ;
#159457 = CARTESIAN_POINT ( 'NONE',  ( 0.6378455412261313517, -1.529572671500577297, -1.527792216034072670 ) ) ;
#159458 = CARTESIAN_POINT ( 'NONE',  ( 5.731092321990707283, 2.014232586630093191, 0.09613807139101374077 ) ) ;
#159459 = EDGE_LOOP ( 'NONE', ( #17525, #192713, #205797, #37556, #74400, #179721 ) ) ;
#159460 = CARTESIAN_POINT ( 'NONE',  ( -0.01814341541641998484, -1.915199053885572988, -0.04638162876333290496 ) ) ;
#159461 = CARTESIAN_POINT ( 'NONE',  ( -8.286004436246233951, 12.81875560892930466, 1.040834085586084257E-14 ) ) ;
#159462 = CARTESIAN_POINT ( 'NONE',  ( 4.160648861918358143, -1.351394993475165673, 1.227733137840483879 ) ) ;
#159463 = VECTOR ( 'NONE', #8423, 1000.000000000000000 ) ;
#159465 = CARTESIAN_POINT ( 'NONE',  ( -5.642163961945882988, 6.318168449258962482, -1.169820551124676422 ) ) ;
#159464 = CARTESIAN_POINT ( 'NONE',  ( -5.330290668828105538, 6.247702530834755130, 1.199719254218452935 ) ) ;
#159466 = CARTESIAN_POINT ( 'NONE',  ( 6.265786130652515773, 6.994708711910199384, -0.9640221254198673151 ) ) ;
#159467 = CARTESIAN_POINT ( 'NONE',  ( 6.591172692507557329, 1.163088239368128773, -1.646588791553056152 ) ) ;
#159468 = CARTESIAN_POINT ( 'NONE',  ( 5.507694354943953208, -0.8313836724207699369, -1.642813217252625524 ) ) ;
#159469 = AXIS2_PLACEMENT_3D ( 'NONE', #152335, #1786, #196816 ) ;
#159470 = CARTESIAN_POINT ( 'NONE',  ( 2.979005374030806230, 6.489267109963819280, 0.4299785398500996503 ) ) ;
#159471 = CARTESIAN_POINT ( 'NONE',  ( 4.371882800840491967, 2.239072524489620353, -0.5581132647194796403 ) ) ;
#159472 = CARTESIAN_POINT ( 'NONE',  ( 6.703580607314123085, 6.785541894813420072, 0.000000000000000000 ) ) ;
#159473 = CARTESIAN_POINT ( 'NONE',  ( 0.2630567961459496784, -1.839733103847444928, -0.9287307787974752316 ) ) ;
#159474 = CARTESIAN_POINT ( 'NONE',  ( 5.309989718046547402, 9.346738437696316737, 0.7998128361456462443 ) ) ;
#159475 = CARTESIAN_POINT ( 'NONE',  ( 1.856878829904203165, 0.3300924852138227283, -1.913646475244117795 ) ) ;
#159476 = CARTESIAN_POINT ( 'NONE',  ( 5.694729993868760332, -1.451380474000956156, -1.782189233907914838 ) ) ;
#159477 = DIRECTION ( 'NONE',  ( -1.000000000000000000, 4.336808689942017736E-16, 0.000000000000000000 ) ) ;
#159478 = CARTESIAN_POINT ( 'NONE',  ( -4.516801452008150086, 5.298631777878131111, 1.199719254218452935 ) ) ;
#159479 = CARTESIAN_POINT ( 'NONE',  ( 4.047608660086319254, 0.6306619223146043840, -1.761260876548931709 ) ) ;
#159480 = VERTEX_POINT ( 'NONE', #127438 ) ;
#159483 = CARTESIAN_POINT ( 'NONE',  ( -6.310394152517827315, 6.326824364217716656, 0.7998128361456281477 ) ) ;
#159482 = CARTESIAN_POINT ( 'NONE',  ( 0.7499999999999885647, 1.847916667349486231, -1.299038105676652899 ) ) ;
#159481 = CARTESIAN_POINT ( 'NONE',  ( 2.127084423382288314, 1.709874882824816478, 0.8565708355050825062 ) ) ;
#159484 = CARTESIAN_POINT ( 'NONE',  ( 3.616033620774202983, -2.174319932014677548, 0.3768175846284789743 ) ) ;
#159485 = CARTESIAN_POINT ( 'NONE',  ( 1.224999999999969225, 0.6666666673495352802, 0.7072540797572596238 ) ) ;
#159486 = CARTESIAN_POINT ( 'NONE',  ( 6.883263157960391787, 1.249388486322531078, 2.158948101847418144 ) ) ;
#159487 = CARTESIAN_POINT ( 'NONE',  ( 4.529832720297257254, 8.298905583739861314, 0.000000000000000000 ) ) ;
#159488 = CARTESIAN_POINT ( 'NONE',  ( -5.275531169048901958, 8.208517892982092334, -1.082531754730549967 ) ) ;
#159489 = CARTESIAN_POINT ( 'NONE',  ( 1.440630571055816489, 0.3805203625029949799, 1.934124978983255527 ) ) ;
#159490 = CARTESIAN_POINT ( 'NONE',  ( 1.624504772527136875, -1.283422126333678692, -1.917570747650028551 ) ) ;
#159491 = CARTESIAN_POINT ( 'NONE',  ( 2.488659587246494276, 1.902222718079676689, 0.4795239450603656084 ) ) ;
#159492 = FACE_OUTER_BOUND ( 'NONE', #174431, .T. ) ;
#159493 = CARTESIAN_POINT ( 'NONE',  ( 6.614137777011339203, 2.057435194276434842, -0.1460075293888435377 ) ) ;
#159494 = CARTESIAN_POINT ( 'NONE',  ( 5.016153647376217606, 4.954526798134778254, 0.7216878364870317197 ) ) ;
#159495 = CARTESIAN_POINT ( 'NONE',  ( 4.012907874177486178, 0.1037781579101039742, 2.014008197856680393 ) ) ;
#159496 = CARTESIAN_POINT ( 'NONE',  ( 4.583538449871731757, 7.505156070562471804, 1.199719254218451159 ) ) ;
#159497 = ORIENTED_EDGE ( 'NONE', *, *, #84476, .F. ) ;
#159498 =( BOUNDED_CURVE ( )  B_SPLINE_CURVE ( 2, ( #66106, #49897, #2170, #118158, #82384, #86654, #18444, #119219, #133312 ),
 .UNSPECIFIED., .F., .T. ) 
 B_SPLINE_CURVE_WITH_KNOTS ( ( 3, 2, 2, 2, 3 ),
 ( 0.3281250000000001665, 0.3333333333333333148, 0.3437500000000000000, 0.3541666666666666852, 0.3593749999999999445 ),
 .UNSPECIFIED. ) 
 CURVE ( )  GEOMETRIC_REPRESENTATION_ITEM ( )  RATIONAL_B_SPLINE_CURVE ( ( 0.9330127018922194093, 0.9330127018922215187, 1.000000000000000000, 0.8660254037844387076, 1.000000000000000000, 0.8660254037844387076, 1.000000000000000000, 0.9330127018922200755, 0.9330127018922194093 ) ) 
 REPRESENTATION_ITEM ( '' )  );
#159499 = CARTESIAN_POINT ( 'NONE',  ( -8.435144125996554720, 12.99275191363802229, 0.7998128361456341429 ) ) ;
#159500 = DIRECTION ( 'NONE',  ( 1.000000000000000000, 0.000000000000000000, 0.000000000000000000 ) ) ;
#159501 = CARTESIAN_POINT ( 'NONE',  ( 9.911173986789782120, 11.52179005846497972, -1.199719254218440723 ) ) ;
#159502 = CARTESIAN_POINT ( 'NONE',  ( 1.833130710876787584, -2.060620742141227701, -0.6837463184809766670 ) ) ;
#159503 = CARTESIAN_POINT ( 'NONE',  ( 6.042093733545556233, 7.078139439671806699, -1.199719254218452047 ) ) ;
#159504 = EDGE_CURVE ( 'NONE', #170226, #54971, #12513, .T. ) ;
#159505 = CARTESIAN_POINT ( 'NONE',  ( -3.111406510290429139, 14.52977256516549964, -11.59832018432755163 ) ) ;
#159506 = CARTESIAN_POINT ( 'NONE',  ( 1.950266909631480861, 0.5821006739541793040, 1.777759251391328510 ) ) ;
#159507 = CARTESIAN_POINT ( 'NONE',  ( 6.186834690482100108, -0.3103498281695793448, -2.139073744226393181 ) ) ;
#159509 = CARTESIAN_POINT ( 'NONE',  ( 6.827182134110219458, 2.993868409037139688, 2.165198344177218903 ) ) ;
#159508 = CARTESIAN_POINT ( 'NONE',  ( 0.07775346131144718342, 5.719027203068962173, -2.882954358279002260 ) ) ;
#159510 = CARTESIAN_POINT ( 'NONE',  ( 0.6823417656249864960, -0.5739583329919112353, -1.181850606188749264 ) ) ;
#159511 = DIRECTION ( 'NONE',  ( 0.6507913734559627184, -0.7592566023653016805, 0.000000000000000000 ) ) ;
#159512 = CARTESIAN_POINT ( 'NONE',  ( 2.279812546382542493, 1.875032136476075584, -0.3747091278499328770 ) ) ;
#159513 = CARTESIAN_POINT ( 'NONE',  ( 4.029968384200533826, 0.9465192177370416182, -1.495271383057869441 ) ) ;
#159514 = CARTESIAN_POINT ( 'NONE',  ( 1.910667195161031007, -0.5113573046386342691, -1.842555643073694238 ) ) ;
#159515 = CARTESIAN_POINT ( 'NONE',  ( -4.822949958159302497, 6.649860922651058992, -1.599625672291256295 ) ) ;
#159517 = CARTESIAN_POINT ( 'NONE',  ( -0.06540554862877968889, -1.536972603800386361, 1.143280314369120587 ) ) ;
#159516 = CARTESIAN_POINT ( 'NONE',  ( 1.781714131423858791E-15, -3.430288072414404179E-15, 0.2598076211376221800 ) ) ;
#159518 = CARTESIAN_POINT ( 'NONE',  ( -1.402160292154681736E-14, -0.5374999999999753308, 1.732050807568877637 ) ) ;
#159519 = CARTESIAN_POINT ( 'NONE',  ( 1.047426762419433777, 1.826728496382063582, -0.9743617655595809834 ) ) ;
#159520 = CARTESIAN_POINT ( 'NONE',  ( -1.500000000000011324, 5.629166666666693963, -0.8660254037844313801 ) ) ;
#159521 = CARTESIAN_POINT ( 'NONE',  ( 5.014452206985246185, 1.289541220462528504, -1.355370375751355105 ) ) ;
#159522 = CARTESIAN_POINT ( 'NONE',  ( 1.664397423953474009, -1.292156093668932693, 1.290017532847971271 ) ) ;
#159524 = CARTESIAN_POINT ( 'NONE',  ( 5.015976829175539109, 7.901154160799176651, 1.084432410706299477 ) ) ;
#159523 = CARTESIAN_POINT ( 'NONE',  ( 5.549527019956425278, -1.737703232767298545, -1.360318885177333570 ) ) ;
#159525 = CARTESIAN_POINT ( 'NONE',  ( 1.364683531249992088, 5.446875000341417916, 1.214306433183764966E-14 ) ) ;
#159526 = CARTESIAN_POINT ( 'NONE',  ( 3.227062719040986405, -1.904794013395166186, -0.7919108894221676964 ) ) ;
#159527 = CARTESIAN_POINT ( 'NONE',  ( -6.177711549321182716, 10.35908057418338402, 0.7998128361456481317 ) ) ;
#159528 = CARTESIAN_POINT ( 'NONE',  ( -1.225000000000005640, 1.387778780781445676E-14, -1.387778780781445676E-14 ) ) ;
#159529 = CARTESIAN_POINT ( 'NONE',  ( 9.077347539549325717, 10.54899253668443393, -1.199719254218446718 ) ) ;
#159530 = CARTESIAN_POINT ( 'NONE',  ( 1.445379498298573928, 3.562780597991719755, 0.4160626371120853539 ) ) ;
#159531 = VECTOR ( 'NONE', #34812, 1000.000000000000000 ) ;
#159532 = CARTESIAN_POINT ( 'NONE',  ( 0.000000000000000000, 9.200000000000020606, -0.3999999999999941380 ) ) ;
#159533 = CARTESIAN_POINT ( 'NONE',  ( 7.028976294042106332, 7.165170195996068969, 0.000000000000000000 ) ) ;
#159534 = EDGE_LOOP ( 'NONE', ( #4262, #203247, #29545, #90259 ) ) ;
#159535 = CARTESIAN_POINT ( 'NONE',  ( 5.705552448923417508, -1.629793913574303588, -1.276656259598766940 ) ) ;
#159536 = CARTESIAN_POINT ( 'NONE',  ( -1.364683531250014514, -0.4072916663252447167, 0.7879004041258379498 ) ) ;
#159537 = CARTESIAN_POINT ( 'NONE',  ( 2.319794969891198821, -2.097318901067245722, 0.5227781780692899449 ) ) ;
#159538 = CARTESIAN_POINT ( 'NONE',  ( -4.693116838625758014, 8.272874032808440248, 0.5769273507626712094 ) ) ;
#159539 = CARTESIAN_POINT ( 'NONE',  ( 3.053383268589305644, -1.780226508164801213, 0.9538969713841909392 ) ) ;
#159540 = CARTESIAN_POINT ( 'NONE',  ( 6.620655732516651071, -0.002413161512292844035, 2.173887093218453082 ) ) ;
#159541 = PRODUCT_DEFINITION_SHAPE ( 'NONE', 'NONE',  #95911 ) ;
#159544 = CARTESIAN_POINT ( 'NONE',  ( 7.131225611108088280, 9.342849184424693476, 1.443375672974076540 ) ) ;
#159543 = CARTESIAN_POINT ( 'NONE',  ( -3.475000000000000533, -0.6999999999999992895, 0.000000000000000000 ) ) ;
#159542 = CARTESIAN_POINT ( 'NONE',  ( -1.201851678989727383E-14, 3.743750000682817713, 1.732050807568877637 ) ) ;
#159545 = CARTESIAN_POINT ( 'NONE',  ( -7.293360289508603600, 7.473618190706972086, 0.000000000000000000 ) ) ;
#159546 = CARTESIAN_POINT ( 'NONE',  ( 1.815639016007553730, -1.320828798922760949, -1.523793687088881299 ) ) ;
#159548 = CARTESIAN_POINT ( 'NONE',  ( 6.567925981381852907, -1.350348970527824211, 1.726830949945204363 ) ) ;
#159547 = CARTESIAN_POINT ( 'NONE',  ( -6.064574784014443942, 5.969758757638621738, -0.7998128361456291469 ) ) ;
#159549 = CARTESIAN_POINT ( 'NONE',  ( 0.7499999999999902300, 4.597916667349482012, -1.299038105676658228 ) ) ;
#159550 = CARTESIAN_POINT ( 'NONE',  ( 4.218947473185084007, 1.474887410857337100, -1.217315437338606365 ) ) ;
#159551 = CARTESIAN_POINT ( 'NONE',  ( -2.279742385392243165, 5.811449882932888222, -0.7998128361456281477 ) ) ;
#159552 = CARTESIAN_POINT ( 'NONE',  ( 6.819388077549422889, 8.018669514304889390, -1.082531754730543971 ) ) ;
#159554 = CARTESIAN_POINT ( 'NONE',  ( 3.849232595480827079, 0.2440098934328518987, -2.001514877671112025 ) ) ;
#159553 = CARTESIAN_POINT ( 'NONE',  ( -8.310784975052671442, 11.67937098999472667, -1.082531754730543083 ) ) ;
#159555 = B_SPLINE_CURVE_WITH_KNOTS ( 'NONE', 3,
 ( #150590, #149512, #133293, #199299, #50944, #116003, #32558 ),
 .UNSPECIFIED., .F., .F.,
 ( 4, 3, 4 ),
 ( -0.0002318125648490629992, 2.710505431213761085E-20, 0.0004044109710639540861 ),
 .UNSPECIFIED. ) ;
#159556 = CARTESIAN_POINT ( 'NONE',  ( 1.364683531249997417, 13.04687500034139980, 2.602085213965210642E-15 ) ) ;
#159557 = CARTESIAN_POINT ( 'NONE',  ( 5.051616488536272875, 0.5384910649316194675, -1.638604462054549238 ) ) ;
#159558 = CARTESIAN_POINT ( 'NONE',  ( 5.580062740476173566, 8.667767742934335828, 1.199719254218451159 ) ) ;
#159559 = CARTESIAN_POINT ( 'NONE',  ( 2.361091307074211887, 5.906356958228550447, 0.7998128361456462443 ) ) ;
#159560 =( GEOMETRIC_REPRESENTATION_CONTEXT ( 3 ) GLOBAL_UNCERTAINTY_ASSIGNED_CONTEXT ( ( #148036 ) ) GLOBAL_UNIT_ASSIGNED_CONTEXT ( ( #49298, #83898, #183534 ) ) REPRESENTATION_CONTEXT ( 'NONE', 'WORKASPACE' ) );
#159561 = CARTESIAN_POINT ( 'NONE',  ( 1.806654366501771136, 2.480000000000016858, 2.499999999999998668 ) ) ;
#159562 = CARTESIAN_POINT ( 'NONE',  ( 3.848780967690920374, -1.530814235938406931, 1.074699354247290017 ) ) ;
#159563 = ORIENTED_EDGE ( 'NONE', *, *, #94249, .F. ) ;
#159564 = CARTESIAN_POINT ( 'NONE',  ( 1.446235060908855008, -0.9343481645287862181, 1.847524432027500385 ) ) ;
#159565 = DIRECTION ( 'NONE',  ( 5.551115123125764213E-17, 0.000000000000000000, -1.000000000000000000 ) ) ;
#159566 = ORIENTED_EDGE ( 'NONE', *, *, #6025, .T. ) ;
#159567 = CARTESIAN_POINT ( 'NONE',  ( 5.918593472536316291, -0.6585524616501952089, -1.687715565691887187 ) ) ;
#159568 = CARTESIAN_POINT ( 'NONE',  ( 3.691562964670865199, 7.528850235416478576, -0.7998128361456362523 ) ) ;
#159569 = DIRECTION ( 'NONE',  ( 0.05872483221476459958, 0.000000000000000000, -0.9982742078614211811 ) ) ;
#159570 = CARTESIAN_POINT ( 'NONE',  ( 0.4042039562905282435, -1.797914468929398879, -0.2212116797051487393 ) ) ;
#159571 = CARTESIAN_POINT ( 'NONE',  ( 4.204437033569277560, 7.919277282557212416, 0.000000000000000000 ) ) ;
#159572 = CARTESIAN_POINT ( 'NONE',  ( 9.979653537509710404, 11.54805711219047382, 6.669254315307292735 ) ) ;
#159573 = EDGE_LOOP ( 'NONE', ( #39441, #180049, #91988, #164757 ) ) ;
#159574 = AXIS2_PLACEMENT_3D ( 'NONE', #138821, #35964, #169169 ) ;
#159575 = EDGE_CURVE ( 'NONE', #183003, #27525, #69632, .T. ) ;
#159577 = CARTESIAN_POINT ( 'NONE',  ( 8.423693512792301163, 8.722063941212843119, 0.7998128361456481317 ) ) ;
#159576 = CARTESIAN_POINT ( 'NONE',  ( 0.6780837441340243910, -1.046368970337024473, -1.659334490400856454 ) ) ;
#159578 = CARTESIAN_POINT ( 'NONE',  ( 4.728101222851567975, 1.910784947378706855, 0.1365434035073622987 ) ) ;
#159579 = CYLINDRICAL_SURFACE ( 'NONE', #41988, 1.500000000000000222 ) ;
#159580 = CARTESIAN_POINT ( 'NONE',  ( -5.488562097922137895, 7.488332829134150437, 1.250156803814896245 ) ) ;
#159581 = DIRECTION ( 'NONE',  ( 0.000000000000000000, 0.000000000000000000, -1.000000000000000000 ) ) ;
#159583 = VERTEX_POINT ( 'NONE', #47189 ) ;
#159582 = CARTESIAN_POINT ( 'NONE',  ( 4.365362273920230685, 8.036747052974847705, 0.7216878364870298324 ) ) ;
#159584 = CARTESIAN_POINT ( 'NONE',  ( -7.673551755654729689, 11.89630144833179060, 0.7216878364870458196 ) ) ;
#159585 = CARTESIAN_POINT ( 'NONE',  ( 1.833122199354455972, 0.2117775504973731793, 2.151289291301178075 ) ) ;
#159586 = CARTESIAN_POINT ( 'NONE',  ( -4.821859908315634158, 5.654533310236863564, 1.199719254218452935 ) ) ;
#159587 = CARTESIAN_POINT ( 'NONE',  ( 6.699137298928145690, 8.909022496873262753, 1.443375672974065660 ) ) ;
#159588 = CARTESIAN_POINT ( 'NONE',  ( -4.600294193738529103, 4.261431402316699035, -0.7998128361456221525 ) ) ;
#159589 = CARTESIAN_POINT ( 'NONE',  ( 4.682524874021861017, -1.770931954651306262, -0.4427778663074270482 ) ) ;
#159590 = CARTESIAN_POINT ( 'NONE',  ( 8.433970489975340712, 12.79606745324766059, -8.483499499578806891 ) ) ;
#159591 = CARTESIAN_POINT ( 'NONE',  ( 1.510939727685528311, 1.736590689682067756, 0.9330581202648262629 ) ) ;
#159592 = CARTESIAN_POINT ( 'NONE',  ( 3.181800181368432678, 1.864768544494728175, -0.4233684943922080834 ) ) ;
#159593 = EDGE_LOOP ( 'NONE', ( #153456, #199278, #109014, #13210 ) ) ;
#159594 = CARTESIAN_POINT ( 'NONE',  ( -10.91944002402978775, -9.999999999999994671, 0.1905873483556694281 ) ) ;
#159595 = CARTESIAN_POINT ( 'NONE',  ( 4.246515029176777034, -1.947796394531702280, -0.2911330189915450339 ) ) ;
#159596 = ORIENTED_EDGE ( 'NONE', *, *, #22298, .F. ) ;
#159597 = CARTESIAN_POINT ( 'NONE',  ( 5.513211315966105808, -1.893842782867664054, 0.4293952855863486517 ) ) ;
#159598 = ORIENTED_EDGE ( 'NONE', *, *, #574, .F. ) ;
#159599 = CARTESIAN_POINT ( 'NONE',  ( -6.343235766347277149, 8.493804042195527870, -1.599625672291271394 ) ) ;
#159601 = CARTESIAN_POINT ( 'NONE',  ( 5.924112389714110805, -2.104401743431310923, 0.2612745606217213856 ) ) ;
#159600 = CARTESIAN_POINT ( 'NONE',  ( -3.474632506852224356, 7.275764701294714420, -0.7998128361456481317 ) ) ;
#159602 = CARTESIAN_POINT ( 'NONE',  ( 6.007671464186823407, 9.062681570643055906, 1.082531754730549967 ) ) ;
#159604 = ORIENTED_EDGE ( 'NONE', *, *, #94595, .F. ) ;
#159603 = CARTESIAN_POINT ( 'NONE',  ( 4.002528454542265024, -1.891902218777557598, -0.2775262981309714605 ) ) ;
#159605 = CARTESIAN_POINT ( 'NONE',  ( 5.196774945655527667, 6.645529799594804388, -1.392961322168507765 ) ) ;
#159606 = EDGE_CURVE ( 'NONE', #157195, #193155, #163059, .T. ) ;
#159607 = CARTESIAN_POINT ( 'NONE',  ( 0.2331563151865486683, 0.005903526429595904942, -1.945944850731482934 ) ) ;
#159608 = CARTESIAN_POINT ( 'NONE',  ( 3.444653546323793947, 6.176457016423196222, 1.199719254218451159 ) ) ;
#159609 = SURFACE_STYLE_FILL_AREA ( #175876 ) ;
#159610 = CARTESIAN_POINT ( 'NONE',  ( 5.461592787958983841, -1.588467041389821421, -1.236575366846304647 ) ) ;
#159611 = CARTESIAN_POINT ( 'NONE',  ( 0.000000000000000000, 13.49999999999999822, 0.000000000000000000 ) ) ;
#159612 = CARTESIAN_POINT ( 'NONE',  ( 6.498675964634617941, -0.4922777150685350156, -1.758009983081544991 ) ) ;
#159613 = CARTESIAN_POINT ( 'NONE',  ( 2.137250951388528275, -0.09934309608320913976, -2.068088366144354318 ) ) ;
#159614 = CARTESIAN_POINT ( 'NONE',  ( -8.188761592974051595, 9.616271948966963024, -1.082531754730543971 ) ) ;
#159615 = AXIS2_PLACEMENT_3D ( 'NONE', #24780, #74613, #129586 ) ;
#159616 = CARTESIAN_POINT ( 'NONE',  ( -5.591215426272092337, 7.404592667505576209, -1.242541652263975172 ) ) ;
#159617 = CARTESIAN_POINT ( 'NONE',  ( 0.6125000000000019318, 1.833333333333346582, 1.060881119635934455 ) ) ;
#159618 = CARTESIAN_POINT ( 'NONE',  ( 6.526239545637954720, 1.075124705556152138, -1.530631868311462362 ) ) ;
#159619 = CARTESIAN_POINT ( 'NONE',  ( 5.986088515633498197, 6.942523675449257858, -1.199719254218446718 ) ) ;
#159620 = AXIS2_PLACEMENT_3D ( 'NONE', #167053, #183287, #1314 ) ;
#159621 = CARTESIAN_POINT ( 'NONE',  ( 0.000000000000000000, -4.000000000000003553, 0.000000000000000000 ) ) ;
#159622 = ADVANCED_FACE ( 'NONE', ( #64480 ), #115422, .F. ) ;
#159623 = CARTESIAN_POINT ( 'NONE',  ( 6.238160076063542725, 6.450477308261824305, -0.7216878364870458196 ) ) ;
#159624 = CARTESIAN_POINT ( 'NONE',  ( -11.33772463945036968, 10.90000000000000036, -3.600000000000002309 ) ) ;
#159625 = CARTESIAN_POINT ( 'NONE',  ( 0.6823417656249934904, 11.25520833367473017, 1.181850606188764807 ) ) ;
#159626 = CARTESIAN_POINT ( 'NONE',  ( -4.029797971759847997, 5.724516938518342535, -1.599625672291256295 ) ) ;
#159628 = CARTESIAN_POINT ( 'NONE',  ( -7.605197822622922210, 7.837428646007010613, -0.7998128361456362523 ) ) ;
#159627 = CARTESIAN_POINT ( 'NONE',  ( -11.96533679318059917, 11.25246011187005202, -0.9151144679398750537 ) ) ;
#159629 = CARTESIAN_POINT ( 'NONE',  ( 3.867547151669390448, -0.1745043776680033631, -1.725349009328189576 ) ) ;
#159630 = CARTESIAN_POINT ( 'NONE',  ( -3.893162665418476109, 7.693773542963529444, 1.040834085586084257E-14 ) ) ;
#159631 = CARTESIAN_POINT ( 'NONE',  ( 1.498975721005956219, 0.3999860688887920679, 2.031077231357696355 ) ) ;
#159632 = CARTESIAN_POINT ( 'NONE',  ( 3.234098929720787385, 2.117403153491578927, -0.002560228748609005411 ) ) ;
#159633 = CARTESIAN_POINT ( 'NONE',  ( 6.913768267964901071, 10.15348118167935709, -1.199719254218441611 ) ) ;
#159634 = CARTESIAN_POINT ( 'NONE',  ( 0.09630943990283219458, -9.919512026728389387, 10.99957837791002468 ) ) ;
#159635 = CARTESIAN_POINT ( 'NONE',  ( 0.3210686601547476093, -1.756690599571947065, -0.8905566435374636658 ) ) ;
#159636 = CARTESIAN_POINT ( 'NONE',  ( 5.915399107357110609, 6.142141269072955545, 0.7871259410536131096 ) ) ;
#159637 = CARTESIAN_POINT ( 'NONE',  ( 4.446711195602238931, 6.210915699667823198, -1.443375672974051449 ) ) ;
#159639 = CARTESIAN_POINT ( 'NONE',  ( -0.03509584499547176162, -1.534781374734139670, 1.140672443274578729 ) ) ;
#159638 = CARTESIAN_POINT ( 'NONE',  ( 1.737500000000001155, -2.333333333333333037, 3.009438278150922130 ) ) ;
#159640 = CARTESIAN_POINT ( 'NONE',  ( 3.328363117612358479, 2.236410206915816268, 0.5022841181492423424 ) ) ;
#159641 = CARTESIAN_POINT ( 'NONE',  ( 1.049113529465800054, -1.437755431736492673, -1.125068434497819680 ) ) ;
#159642 = CARTESIAN_POINT ( 'NONE',  ( 3.375170810042011915, -1.688748480992762868, -0.8973671847329609541 ) ) ;
#159643 = CARTESIAN_POINT ( 'NONE',  ( 5.773793314573267388, 7.829454515125894964, 1.599625672291268286 ) ) ;
#159645 = EDGE_CURVE ( 'NONE', #96467, #149119, #51827, .T. ) ;
#159644 = CARTESIAN_POINT ( 'NONE',  ( 5.951666246274792016, 8.927065806420504401, 1.082531754730558626 ) ) ;
#159646 = CARTESIAN_POINT ( 'NONE',  ( -8.483651433849100698, 10.92067931095586886, 1.599625672291269396 ) ) ;
#159647 = CARTESIAN_POINT ( 'NONE',  ( 2.127199591969671122, 1.800101769773830185, 0.9015413830680671925 ) ) ;
#159648 = CARTESIAN_POINT ( 'NONE',  ( 2.289831844592318255, -1.277571413231039399, -1.488851726829776068 ) ) ;
#159649 = CARTESIAN_POINT ( 'NONE',  ( -9.134442807305063639, 11.67993591332117376, 1.599625672291281386 ) ) ;
#159650 = CARTESIAN_POINT ( 'NONE',  ( -4.726989112658928072, 8.666571064744069020, 1.040834085586084257E-14 ) ) ;
#159651 = CARTESIAN_POINT ( 'NONE',  ( -11.33183379859914552, 6.587777300838509653, -3.814615888199307747 ) ) ;
#159653 = CARTESIAN_POINT ( 'NONE',  ( 2.957584522866180343, 1.761491525812574510, -0.1715649573520404425 ) ) ;
#159652 = CARTESIAN_POINT ( 'NONE',  ( 5.490208796768200727, -0.5072484191241812823, -2.028029781992314096 ) ) ;
#159654 = CARTESIAN_POINT ( 'NONE',  ( 0.3263184169969229886, 16.00000000000058265, 11.67999999558625213 ) ) ;
#159655 = CARTESIAN_POINT ( 'NONE',  ( 6.158190107012026182, -1.625331280325162053, 1.616661686624631944 ) ) ;
#159656 = CARTESIAN_POINT ( 'NONE',  ( 5.068161541800582093, -1.640353732806285825, -0.5817517365288951137 ) ) ;
#159657 = CARTESIAN_POINT ( 'NONE',  ( 8.320953590485093088, 10.73086516036454618, 1.599625672291281386 ) ) ;
#159658 = CARTESIAN_POINT ( 'NONE',  ( 4.358545522520183013, -0.6637924119957930857, 1.601953373104019418 ) ) ;
#159659 = CARTESIAN_POINT ( 'NONE',  ( 5.494640824104591204, 2.138133990741352353, 0.3765844856341519775 ) ) ;
#159660 = CARTESIAN_POINT ( 'NONE',  ( 0.5853561509586381328, 1.734793994416533369, 1.213709793590052932 ) ) ;
#159661 = CARTESIAN_POINT ( 'NONE',  ( 5.468750000000003553, 0.7852924748297082091, -1.895863743164194704 ) ) ;
#159662 = CARTESIAN_POINT ( 'NONE',  ( -0.1909996267163149852, 7.629137130509101361, -2.600377616606447617 ) ) ;
#159663 = CARTESIAN_POINT ( 'NONE',  ( 3.452094016638465490, 1.926566264197142830, 0.001310335549949831480 ) ) ;
#159664 = CARTESIAN_POINT ( 'NONE',  ( 1.500000000000001332, 11.40625000068279427, 0.000000000000000000 ) ) ;
#159665 = CARTESIAN_POINT ( 'NONE',  ( 0.06548277170575435291, -1.780103896928236118, 1.328506668625312859 ) ) ;
#159666 = ORIENTED_EDGE ( 'NONE', *, *, #199418, .F. ) ;
#159667 = CARTESIAN_POINT ( 'NONE',  ( 0.7499999999999902300, 3.816666666666690411, -1.299038105676658228 ) ) ;
#159668 = CARTESIAN_POINT ( 'NONE',  ( 6.986529229743720926, 7.045372277656132276, -0.7998128361456281477 ) ) ;
#159669 = CARTESIAN_POINT ( 'NONE',  ( 2.051734446849303506, -1.982521776546506853, 1.002060208660388474 ) ) ;
#159670 = CARTESIAN_POINT ( 'NONE',  ( 0.000000000000000000, 0.000000000000000000, 0.000000000000000000 ) ) ;
#159671 = CARTESIAN_POINT ( 'NONE',  ( 7.673551755654734130, 9.015193805427763607, -1.082531754730537976 ) ) ;
#159672 = CARTESIAN_POINT ( 'NONE',  ( -9.286972035236630063, 10.89751746493999107, -1.082531754730537976 ) ) ;
#159673 = CARTESIAN_POINT ( 'NONE',  ( 6.780486220610169035, 9.003929572168926754, -1.443375672974078761 ) ) ;
#159674 = CARTESIAN_POINT ( 'NONE',  ( 1.266250242576156815, 1.862016182229693673, -0.7743172429433076154 ) ) ;
#159676 = CARTESIAN_POINT ( 'NONE',  ( 5.406706549104464798, 0.5953045380993631230, 1.974924460807401028 ) ) ;
#159675 = CARTESIAN_POINT ( 'NONE',  ( 9.511208455186636712, 11.05516360492796935, 1.199719254218453823 ) ) ;
#159677 = CARTESIAN_POINT ( 'NONE',  ( -0.4288785890453234995, 3.049942316455299451, -0.4196807566834767078 ) ) ;
#159678 = CARTESIAN_POINT ( 'NONE',  ( -3.090368948911150770, 5.692848642783215674, 1.199719254218462483 ) ) ;
#159680 = EDGE_CURVE ( 'NONE', #203624, #69840, #17153, .T. ) ;
#159679 = SURFACE_STYLE_FILL_AREA ( #93637 ) ;
#159681 = CARTESIAN_POINT ( 'NONE',  ( -0.6823417656250003738, 1.467708333674752730, -1.181850606188749264 ) ) ;
#159682 = CARTESIAN_POINT ( 'NONE',  ( 0.5613125002107671735, 1.751697300359332798, -0.2511290008074765212 ) ) ;
#159683 = CARTESIAN_POINT ( 'NONE',  ( 5.748594953515238082, 1.706903099953221759, -0.3051902176867369865 ) ) ;
#159684 = CARTESIAN_POINT ( 'NONE',  ( 5.372502291033079302, -0.05049805449116586548, -1.739898325138872215 ) ) ;
#159685 = CARTESIAN_POINT ( 'NONE',  ( 3.491970780479057179, -2.289775125716007054, -0.1112369151145074092 ) ) ;
#159686 = CARTESIAN_POINT ( 'NONE',  ( -0.6823417656250003738, 0.2177083336747515085, -1.181850606188749264 ) ) ;
#159687 = CARTESIAN_POINT ( 'NONE',  ( 2.730204174461122069, 0.2256132759956077649, 1.827196471909063202 ) ) ;
#159688 = EDGE_CURVE ( 'NONE', #196234, #99096, #112745, .T. ) ;
#159689 = CARTESIAN_POINT ( 'NONE',  ( 7.750457368506414646, 12.19395069656619945, 0.7998128361456462443 ) ) ;
#159690 = SURFACE_STYLE_USAGE ( .BOTH. , #27551 ) ;
#159691 = CARTESIAN_POINT ( 'NONE',  ( 2.696107482849848580, -1.820545782403935720, -0.1364615833806467338 ) ) ;
#159692 = CARTESIAN_POINT ( 'NONE',  ( 4.342422763466713853, 0.4390309838058319425, -1.967887491402267486 ) ) ;
#159693 = CARTESIAN_POINT ( 'NONE',  ( -2.426546306721660606, 5.774795091243142053, 0.7216878364870317197 ) ) ;
#159694 = CARTESIAN_POINT ( 'NONE',  ( 7.948861177221683505, 14.94981965669310853, -9.879624537148666619 ) ) ;
#159695 = CARTESIAN_POINT ( 'NONE',  ( 4.506922906144382956, 1.629430921360131679, -1.334182900473983135 ) ) ;
#159696 = CARTESIAN_POINT ( 'NONE',  ( -6.749261541504576911, 6.768559974710451677, 1.040834085586084257E-14 ) ) ;
#159697 = CARTESIAN_POINT ( 'NONE',  ( 9.163219433650940715, 13.31059121366393860, 9.059053262848197008 ) ) ;
#159698 = CARTESIAN_POINT ( 'NONE',  ( 2.647004975520852454, -0.3514972095969396970, -2.040143077068845123 ) ) ;
#159699 = CARTESIAN_POINT ( 'NONE',  ( 5.027376032568989572, 4.759693547618927489, 0.7998128361456341429 ) ) ;
#159700 = CARTESIAN_POINT ( 'NONE',  ( -3.755786496842897795E-14, 1.109375000341423112, -1.570758158831814466 ) ) ;
#159701 = CARTESIAN_POINT ( 'NONE',  ( 4.319064098534145302, 1.638436671179326787, -1.346072318137331969 ) ) ;
#159702 = CARTESIAN_POINT ( 'NONE',  ( 6.727182134110220701, 0.005875948494733078051, 1.810970247402940103 ) ) ;
#159703 = B_SPLINE_CURVE_WITH_KNOTS ( 'NONE', 3,
 ( #104094, #88920, #173369, #21729 ),
 .UNSPECIFIED., .F., .F.,
 ( 4, 4 ),
 ( 0.000000000000000000, 0.0003126726301078944139 ),
 .UNSPECIFIED. ) ;
#159704 = VERTEX_POINT ( 'NONE', #168371 ) ;
#159705 = CARTESIAN_POINT ( 'NONE',  ( -3.142457743317409680, 6.888227477170756785, 0.7998128361456352531 ) ) ;
#159706 = CARTESIAN_POINT ( 'NONE',  ( 9.745613490124728884, 10.26430391476735338, 0.7998128361456462443 ) ) ;
#159707 = CARTESIAN_POINT ( 'NONE',  ( 6.658462837642799670, 6.940830530104329377, 0.7216878364870328300 ) ) ;
#159708 = CARTESIAN_POINT ( 'NONE',  ( 0.000000000000000000, -1.093749999044084431, -4.012584370867899430 ) ) ;
#159709 = CARTESIAN_POINT ( 'NONE',  ( -4.985647801523292344, 6.839675073242382553, -1.599625672291256295 ) ) ;
#159710 = CARTESIAN_POINT ( 'NONE',  ( 6.187751663909415001, 2.028806014889028120, -0.6170373231123224000 ) ) ;
#159711 = CARTESIAN_POINT ( 'NONE',  ( 1.307801118376609839, -0.5120802815330603996, 2.042612192628911139 ) ) ;
#159713 = CARTESIAN_POINT ( 'NONE',  ( -4.308458954092677651, 8.248562223075252220, -0.7998128361456362523 ) ) ;
#159712 = TOROIDAL_SURFACE ( 'NONE', #166671, 6.909076424898650259, 0.08000000000000000167 ) ;
#159714 = CARTESIAN_POINT ( 'NONE',  ( 6.726816770674637347, 10.99970333242910669, -0.7998128361456291469 ) ) ;
#159715 = CARTESIAN_POINT ( 'NONE',  ( 6.209776894639321476, 0.5414253987558427239, -1.780396208465367280 ) ) ;
#159716 = CARTESIAN_POINT ( 'NONE',  ( 7.588813295347141441, 9.876701482703580837, -1.599625672291262513 ) ) ;
#159717 = CARTESIAN_POINT ( 'NONE',  ( -1.734723475976807094E-15, 2.999999999999988898, -6.938893903907228378E-15 ) ) ;
#159718 = CARTESIAN_POINT ( 'NONE',  ( -3.474632506852224356, 7.275764701294714420, -0.7998128361456481317 ) ) ;
#159719 = CARTESIAN_POINT ( 'NONE',  ( -9.381879110976678149, 11.00824238663667565, 1.082531754730558626 ) ) ;
#159720 = CARTESIAN_POINT ( 'NONE',  ( 0.5980879788009090259, 1.428637019467562830, 1.567290143595565066 ) ) ;
#159721 = DIRECTION ( 'NONE',  ( 1.000000000000000000, 0.000000000000000000, 0.000000000000000000 ) ) ;
#159723 = CARTESIAN_POINT ( 'NONE',  ( 2.295295855072278624, -1.753792786583353580, 0.8793850528211948347 ) ) ;
#159722 = CARTESIAN_POINT ( 'NONE',  ( 1.224999999999949241, -0.6041666666666428709, -0.7072540797572917093 ) ) ;
#159724 = CARTESIAN_POINT ( 'NONE',  ( 1.569428280142046717, 0.1587979871724466974, -2.155937297210829495 ) ) ;
#159726 = CARTESIAN_POINT ( 'NONE',  ( -5.593616938499215152, 6.351546440420595019, 1.211061620805883532 ) ) ;
#159725 = CARTESIAN_POINT ( 'NONE',  ( -4.938913097128142304, 8.984092056616635347, -0.7998128361456362523 ) ) ;
#159727 = CARTESIAN_POINT ( 'NONE',  ( 1.364683531249986537, 1.155208333674754728, -0.7879004041258239610 ) ) ;
#159728 = CARTESIAN_POINT ( 'NONE',  ( 3.215853349543820183, -1.415750056632815168, -1.000566135699741066 ) ) ;
#159729 = CARTESIAN_POINT ( 'NONE',  ( 2.150002804924430411, -1.345968700644652349, 1.103203096369822056 ) ) ;
#159730 = CARTESIAN_POINT ( 'NONE',  ( 5.748293942514166588, 7.729428904398431222, -1.443375672974057666 ) ) ;
#159731 = CARTESIAN_POINT ( 'NONE',  ( -10.97400665845581536, 4.893988168282350948, 4.351071648605314479 ) ) ;
#159732 = PRESENTATION_LAYER_ASSIGNMENT (  '', '', ( #38659 ) ) ;
#159733 = CARTESIAN_POINT ( 'NONE',  ( 2.600935288962639369, 0.9528664403582010056, -1.776738882381201812 ) ) ;
#159734 = CARTESIAN_POINT ( 'NONE',  ( 6.825078400183546279, 2.419143596098617621, 2.525240329153962904 ) ) ;
#159735 = CARTESIAN_POINT ( 'NONE',  ( -4.984557751679625781, 5.844347460828191565, 1.199719254218452935 ) ) ;
#159736 = CARTESIAN_POINT ( 'NONE',  ( 1.323050886902911616, -0.05057411593789931659, 1.970981584096524575 ) ) ;
#159738 = CARTESIAN_POINT ( 'NONE',  ( -4.814553946628611136, 8.631080347793099961, 0.000000000000000000 ) ) ;
#159737 = CARTESIAN_POINT ( 'NONE',  ( 5.256085721135645095, 0.7693902824621422498, -1.750971482026221437 ) ) ;
#159739 = CARTESIAN_POINT ( 'NONE',  ( -4.299344108864949554, 8.030002203735486788, -0.7216878364870338292 ) ) ;
#159740 = CARTESIAN_POINT ( 'NONE',  ( 5.631432701629774051, 7.663367133358481631, 1.599625672291269396 ) ) ;
#159741 = CARTESIAN_POINT ( 'NONE',  ( -7.469616286486262524, 7.679250187180907794, 0.7998128361456341429 ) ) ;
#159742 = CARTESIAN_POINT ( 'NONE',  ( 1.348313414878389294, 0.9933643222376374871, -1.758399455230485575 ) ) ;
#159743 = CARTESIAN_POINT ( 'NONE',  ( -0.4500000000000232703, 4.000000000000003553, 0.8338124244295432863 ) ) ;
#159744 = CARTESIAN_POINT ( 'NONE',  ( 5.614422408412740317, -1.031215703586242149, -2.064428503307714546 ) ) ;
#159745 = CARTESIAN_POINT ( 'NONE',  ( 6.074655751228532630, 1.318658252384183438, -1.452748870126779890 ) ) ;
#159746 = CARTESIAN_POINT ( 'NONE',  ( 3.063279882407277999, 1.654721480355027863, 1.053479689057647217 ) ) ;
#159747 = CARTESIAN_POINT ( 'NONE',  ( 9.271078113646423091, 9.710679308875986848, 1.040834085586084257E-14 ) ) ;
#159748 = CARTESIAN_POINT ( 'NONE',  ( 0.2818752512256904597, 1.674885806461807958, -1.122501178855893400 ) ) ;
#159750 = ORIENTED_EDGE ( 'NONE', *, *, #42362, .T. ) ;
#159749 = B_SPLINE_CURVE_WITH_KNOTS ( 'NONE', 3,
 ( #106644, #8007, #74098, #21742, #153922, #85707 ),
 .UNSPECIFIED., .F., .F.,
 ( 4, 2, 4 ),
 ( 0.001511140261635257956, 0.001555921757587612041, 0.001600703253539966127 ),
 .UNSPECIFIED. ) ;
#159751 = CARTESIAN_POINT ( 'NONE',  ( 1.516979485257620608, 0.2134662686405098542, 2.106589464619255558 ) ) ;
#159753 = CARTESIAN_POINT ( 'NONE',  ( -7.670162217029145246, 9.971608557999250166, 1.599625672291295375 ) ) ;
#159752 = CARTESIAN_POINT ( 'NONE',  ( -3.100010679019018500, 6.768429558830820980, 1.040834085586084257E-14 ) ) ;
#159754 = CARTESIAN_POINT ( 'NONE',  ( 1.569984571489828173, -1.747861548559765721, -0.5788160320587890650 ) ) ;
#159755 = ORIENTED_EDGE ( 'NONE', *, *, #117424, .F. ) ;
#159756 = CARTESIAN_POINT ( 'NONE',  ( 11.99415247035267029, 7.596933813522314338, -0.4356545883255271701 ) ) ;
#159757 = CARTESIAN_POINT ( 'NONE',  ( 2.637105894733019262, 1.998242115483703341, 0.7103459930332192140 ) ) ;
#159758 = CARTESIAN_POINT ( 'NONE',  ( 1.499999999999989120, 4.785416667349486453, 0.8660254037844524744 ) ) ;
#159759 = CARTESIAN_POINT ( 'NONE',  ( 7.751511138711133064, 10.06651563329490529, -1.599625672291262513 ) ) ;
#159760 = CARTESIAN_POINT ( 'NONE',  ( 2.829428133295128323, -1.924058217741884125, 0.7386292696346643538 ) ) ;
#159762 = CARTESIAN_POINT ( 'NONE',  ( -0.1121326479804653220, -0.4008509640632436088, -1.803546454093779561 ) ) ;
#159761 = CARTESIAN_POINT ( 'NONE',  ( -7.877450944739929461, 9.149113176073413456, 1.199719254218462483 ) ) ;
#159763 = CARTESIAN_POINT ( 'NONE',  ( 0.6823417656249917140, 4.092708333674755394, 1.181850606188765695 ) ) ;
#159764 = CARTESIAN_POINT ( 'NONE',  ( -2.324088772396477673E-16, -2.887500000000000178, -3.475000000000000089 ) ) ;
#159765 = CARTESIAN_POINT ( 'NONE',  ( 1.443823057115801056, 4.128576303019145577, 0.4219843264276020856 ) ) ;
#159766 = AXIS2_PLACEMENT_3D ( 'NONE', #165814, #85621, #35799 ) ;
#159767 = CARTESIAN_POINT ( 'NONE',  ( 0.03028722099337673168, -1.361824662662258767, -1.737358624739212543 ) ) ;
#159768 = CARTESIAN_POINT ( 'NONE',  ( 3.075713870353123713, 2.149355976742998831, -0.7065000242163150812 ) ) ;
#159769 = CARTESIAN_POINT ( 'NONE',  ( -9.503902493499651882, 10.19023378527882784, 1.040834085586084257E-14 ) ) ;
#159770 = CARTESIAN_POINT ( 'NONE',  ( 2.865264419611464941, -1.483432276133073380, -1.039550242524535539 ) ) ;
#159771 = CARTESIAN_POINT ( 'NONE',  ( 3.186650014752292925, 1.506923149468800682, -1.182699731353755501 ) ) ;
#159772 = CARTESIAN_POINT ( 'NONE',  ( 4.193848433072798088, -1.425472641756184489, -1.501718461524886195 ) ) ;
#159773 = CARTESIAN_POINT ( 'NONE',  ( -0.6823417656250212460, 2.863541667008084879, 1.181850606188767472 ) ) ;
#159774 = CARTESIAN_POINT ( 'NONE',  ( 2.201972163173575137, -1.971069923813788982, 0.04663598398449429056 ) ) ;
#159775 = CARTESIAN_POINT ( 'NONE',  ( 6.498663727319215155, -0.5164181641097148612, -1.855934172746701583 ) ) ;
#159776 = CARTESIAN_POINT ( 'NONE',  ( 3.045614982896325262, 0.6747646648952825288, -1.744891315567910439 ) ) ;
#159778 = CARTESIAN_POINT ( 'NONE',  ( 4.655672573246532941, 8.415299432525721102, 0.4976263304441782553 ) ) ;
#159777 = CARTESIAN_POINT ( 'NONE',  ( 2.754834555525199846, 0.7783630933865728352, 2.172589714749242784 ) ) ;
#159779 = CARTESIAN_POINT ( 'NONE',  ( 2.541259301162884121, 1.702954558545258346, -0.7510573925902948034 ) ) ;
#159780 = CARTESIAN_POINT ( 'NONE',  ( 1.364683531249990311, 2.884375000341422801, 1.214306433183764966E-14 ) ) ;
#159781 = CARTESIAN_POINT ( 'NONE',  ( 6.566849514013569866, 1.531126396248701171, -1.382332999690039754 ) ) ;
#159782 = CARTESIAN_POINT ( 'NONE',  ( -4.894657149733403045, 5.669187081899118574, -1.199719254218446718 ) ) ;
#159783 = CARTESIAN_POINT ( 'NONE',  ( -1.367525579689991000, 3.416241981124319871, 0.2571629661623351382 ) ) ;
#159784 = CARTESIAN_POINT ( 'NONE',  ( 0.7859291816119529095, 1.415994179718871759, 1.559173624910270783 ) ) ;
#159785 = CARTESIAN_POINT ( 'NONE',  ( 1.364683531249988535, 3.676041667008087099, 0.7879004041258500513 ) ) ;
#159786 = CARTESIAN_POINT ( 'NONE',  ( 5.641917277892137150, 0.8817427965214555963, -1.973778517010720490 ) ) ;
#159787 = CARTESIAN_POINT ( 'NONE',  ( 6.533853655515883041, -1.958494339806987394, 0.4928751659435038901 ) ) ;
#159788 = CARTESIAN_POINT ( 'NONE',  ( -1.364683531250014514, -0.7197916663252461600, 0.7879004041258379498 ) ) ;
#159789 = CARTESIAN_POINT ( 'NONE',  ( -3.131570295076647525, 6.597323077657299528, 1.040834085586084257E-14 ) ) ;
#159792 = CARTESIAN_POINT ( 'NONE',  ( 5.504247177468190699, 5.523969249908757817, 0.7216878364870317197 ) ) ;
#159791 = CARTESIAN_POINT ( 'NONE',  ( 6.825078400183573812, 0.002648415797040087893, 1.855566311045192540 ) ) ;
#159790 = CARTESIAN_POINT ( 'NONE',  ( 5.712781623311797397, 7.758274208654143855, -1.599625672291283607 ) ) ;
#159793 = CARTESIAN_POINT ( 'NONE',  ( -2.844178363816758814, 6.540234867753325076, -0.7998128361456481317 ) ) ;
#159794 = CARTESIAN_POINT ( 'NONE',  ( 4.294157853547872605, -0.8666056138363428252, -1.820986994602634024 ) ) ;
#159795 = CARTESIAN_POINT ( 'NONE',  ( -8.715193815486133033, 9.062147627688959872, 0.7998128361456462443 ) ) ;
#159797 = CARTESIAN_POINT ( 'NONE',  ( -7.553300976144794454, 7.984808358356614733, -0.7216878364870338292 ) ) ;
#159796 = CARTESIAN_POINT ( 'NONE',  ( -9.490344339885981029, 10.17441593939621924, -0.7216878364870267237 ) ) ;
#159798 = CARTESIAN_POINT ( 'NONE',  ( 7.015401035077338143, 6.062865449010541141, 2.437084766375292144 ) ) ;
#159800 = CARTESIAN_POINT ( 'NONE',  ( 1.364683531249997417, 10.73437500034139802, 2.602085213965210642E-15 ) ) ;
#159799 = CARTESIAN_POINT ( 'NONE',  ( 6.526263005029544928, 1.249015235541932167, -1.764162671312206498 ) ) ;
#159801 = LINE ( 'NONE', #128466, #120846 ) ;
#159802 = CARTESIAN_POINT ( 'NONE',  ( -8.622095623286845978, 12.14652976288826913, 1.199719254218462483 ) ) ;
#159804 = CARTESIAN_POINT ( 'NONE',  ( 6.187125092307005580, 1.678016663812756937, 1.117817459622950649 ) ) ;
#159803 = CARTESIAN_POINT ( 'NONE',  ( -6.439759776366783761, 8.536139043893143707, 1.443375672974078761 ) ) ;
#159805 = CARTESIAN_POINT ( 'NONE',  ( -1.402160292154681736E-14, 0.5093750003414236893, -1.575800808251659024 ) ) ;
#159806 = CARTESIAN_POINT ( 'NONE',  ( 0.07968937631763337026, 14.48280408365269345, 11.99973206003984316 ) ) ;
#159807 = EDGE_CURVE ( 'NONE', #96549, #69400, #195615, .T. ) ;
#159808 = CARTESIAN_POINT ( 'NONE',  ( 11.96215121607992771, 11.32833553780823799, 0.9565349792967585696 ) ) ;
#159809 = CARTESIAN_POINT ( 'NONE',  ( 2.103723633838894713, -1.724574586359624906, 0.04069764719066489012 ) ) ;
#159810 = CARTESIAN_POINT ( 'NONE',  ( 8.018721507839716267, 8.319872945426633137, -0.7998128361456341429 ) ) ;
#159811 = CARTESIAN_POINT ( 'NONE',  ( 6.367489420273535039, 7.457767740854454708, -1.199719254218452047 ) ) ;
#159812 = CARTESIAN_POINT ( 'NONE',  ( 0.2304661401069136861, 2.567903733459023119, -1.989664166560570324 ) ) ;
#159813 = CARTESIAN_POINT ( 'NONE',  ( 1.141466271755723794, 0.7239738643088615699, -1.615086939138086652 ) ) ;
#159814 = CARTESIAN_POINT ( 'NONE',  ( 1.945949197151348509, -1.316483196816301549, -1.523026451717986784 ) ) ;
#159815 = CYLINDRICAL_SURFACE ( 'NONE', #40272, 0.3999999999999997446 ) ;
#159816 = CARTESIAN_POINT ( 'NONE',  ( 4.190592561755676293, -2.182319254149690302, -0.3268587364041104504 ) ) ;
#159817 = CARTESIAN_POINT ( 'NONE',  ( 4.944265959323273840, -1.029449158807031361, 1.911525048081736955 ) ) ;
#159818 = ORIENTED_EDGE ( 'NONE', *, *, #17272, .F. ) ;
#159819 = CARTESIAN_POINT ( 'NONE',  ( -1.500000000000015099, -0.8708333333333129200, -0.8660254037844383745 ) ) ;
#159820 = CARTESIAN_POINT ( 'NONE',  ( 8.392133896734668141, 9.853539636687704828, 1.082531754730558626 ) ) ;
#159822 = CARTESIAN_POINT ( 'NONE',  ( 3.110954007106698338, 0.05231540665236523308, 2.015913653835194719 ) ) ;
#159821 = CARTESIAN_POINT ( 'NONE',  ( 3.035902975225315714, -2.043024508941180706, 0.5676086983019896781 ) ) ;
#159824 = EDGE_LOOP ( 'NONE', ( #19893, #201074, #147595 ) ) ;
#159823 = CARTESIAN_POINT ( 'NONE',  ( 3.287185820011778947, 0.03942761580559561718, -1.811315726287704431 ) ) ;
#159825 = CARTESIAN_POINT ( 'NONE',  ( 6.561219994370630637, 6.619454513046008515, 0.000000000000000000 ) ) ;
#159826 = EDGE_CURVE ( 'NONE', #65209, #157888, #13765, .T. ) ;
#159827 = VERTEX_POINT ( 'NONE', #52484 ) ;
#159828 = CARTESIAN_POINT ( 'NONE',  ( 0.6900581440293825919, -1.856003987442723657, -0.2331820809091043056 ) ) ;
#159829 = ADVANCED_FACE ( 'NONE', ( #118613 ), #72511, .T. ) ;
#159830 = CARTESIAN_POINT ( 'NONE',  ( 5.986088515633498197, 6.942523675449257858, -1.199719254218446718 ) ) ;
#159831 = AXIS2_PLACEMENT_3D ( 'NONE', #2010, #104900, #53997 ) ;
#159832 = CARTESIAN_POINT ( 'NONE',  ( 6.481070005604858686, -0.09514881109910081070, -1.823337098959529001 ) ) ;
#159834 = CARTESIAN_POINT ( 'NONE',  ( 1.762754532109143124, -0.09793373165993285445, -1.913366418544469205 ) ) ;
#159833 = CARTESIAN_POINT ( 'NONE',  ( -2.767835915484202047, 6.380892334706859792, -0.7998128361456281477 ) ) ;
#159835 = DIRECTION ( 'NONE',  ( -0.6507913734559627184, 0.7592566023653016805, 0.000000000000000000 ) ) ;
#159836 = DIRECTION ( 'NONE',  ( 0.000000000000000000, -1.000000000000000000, 0.000000000000000000 ) ) ;
#159837 = CARTESIAN_POINT ( 'NONE',  ( -0.6823417656250212460, 1.363541667008083547, 1.181850606188755259 ) ) ;
#159838 = DIRECTION ( 'NONE',  ( 0.01745240643728004568, 0.000000000000000000, 0.9998476951563913806 ) ) ;
#159839 = CARTESIAN_POINT ( 'NONE',  ( -6.997979842947967377, 11.31606025008131233, -0.7998128361456291469 ) ) ;
#159840 = CARTESIAN_POINT ( 'NONE',  ( 5.190363053866647647, -2.144918610114197488, -0.2683968819863768451 ) ) ;
#159841 = CARTESIAN_POINT ( 'NONE',  ( -3.838366886444665393, 7.492195444245147939, 0.000000000000000000 ) ) ;
#159842 = CARTESIAN_POINT ( 'NONE',  ( -6.587282531393266360, 8.778525268082516320, 1.599625672291269396 ) ) ;
#159843 = CARTESIAN_POINT ( 'NONE',  ( 2.584367824843319283, 1.138156186954141003, 1.789115803205274080 ) ) ;
#159845 = CARTESIAN_POINT ( 'NONE',  ( -10.02504487015220569, 5.769816241140256707, -5.888073156868665059 ) ) ;
#159844 = CARTESIAN_POINT ( 'NONE',  ( -0.1296875068448125334, 4.095146142119266308, -2.381513845672214913 ) ) ;
#159846 = CARTESIAN_POINT ( 'NONE',  ( 4.147701676541888816, 0.6670536769024897339, -1.855179015784082619 ) ) ;
#159847 = CARTESIAN_POINT ( 'NONE',  ( 6.433860211133586304, -1.853236450885078712, 0.4715264990977630077 ) ) ;
#159848 = ORIENTED_EDGE ( 'NONE', *, *, #50413, .F. ) ;
#159849 = CARTESIAN_POINT ( 'NONE',  ( 5.173117096678320870, 1.865890646727845326, -1.000864459693462383 ) ) ;
#159850 = DIRECTION ( 'NONE',  ( 0.000000000000000000, -1.000000000000000000, -0.000000000000000000 ) ) ;
#159851 = CARTESIAN_POINT ( 'NONE',  ( 6.760212172060996672, -1.969150147884619173, 0.04690145372830689663 ) ) ;
#159852 = CARTESIAN_POINT ( 'NONE',  ( 2.994010707676255212, -0.5641155714235489560, -1.858205125314008832 ) ) ;
#159853 = ORIENTED_EDGE ( 'NONE', *, *, #94104, .T. ) ;
#159854 = CARTESIAN_POINT ( 'NONE',  ( -3.363304624641834106, 6.081549941127532222, -1.199719254218452047 ) ) ;
#159855 = CARTESIAN_POINT ( 'NONE',  ( 6.013923656113508542, 9.173938811177871244, -1.199719254218452047 ) ) ;
#159857 = CARTESIAN_POINT ( 'NONE',  ( 5.307127064745490230, 8.279066444590018392, -1.199719254218452935 ) ) ;
#159856 = CARTESIAN_POINT ( 'NONE',  ( 3.328152359787967640, 2.039751367458849884, 0.4576943786474896858 ) ) ;
#159858 = CARTESIAN_POINT ( 'NONE',  ( 5.546694241322223107, 5.643767167730274537, -0.7216878364870458196 ) ) ;
#159860 = VERTEX_POINT ( 'NONE', #183543 ) ;
#159859 = CARTESIAN_POINT ( 'NONE',  ( 0.1701768659465550948, 0.6913354060617262764, 1.674562877054022625 ) ) ;
#159861 = CARTESIAN_POINT ( 'NONE',  ( 5.584669497696876483, -2.152379054646291756, -0.4867646435422824935 ) ) ;
#159862 = CARTESIAN_POINT ( 'NONE',  ( -0.4265819271709386240, -6.701306620466009889, -10.99180900346563661 ) ) ;
#159863 = AXIS2_PLACEMENT_3D ( 'NONE', #110477, #176477, #126741 ) ;
#159864 = CARTESIAN_POINT ( 'NONE',  ( 2.555956245031346885, 0.5892994983645870599, -2.126554282292691500 ) ) ;
#159865 = CARTESIAN_POINT ( 'NONE',  ( 8.945682426918439845, 9.331051007693339727, 1.040834085586084257E-14 ) ) ;
#159866 = FACE_OUTER_BOUND ( 'NONE', #191334, .T. ) ;
#159867 = CARTESIAN_POINT ( 'NONE',  ( 1.295406243800485635, 1.766531960031037407, -0.7327172462580702206 ) ) ;
#159868 = CARTESIAN_POINT ( 'NONE',  ( 8.398386088661320414, 11.88553530582519357, -1.199719254218446718 ) ) ;
#159869 = CARTESIAN_POINT ( 'NONE',  ( 5.670397268163976712, -0.9275489576153757021, -1.851018422006404096 ) ) ;
#159871 = CARTESIAN_POINT ( 'NONE',  ( 2.870174731959000525, 1.155358403710282866, 1.826860881501219280 ) ) ;
#159870 = CARTESIAN_POINT ( 'NONE',  ( -3.009396220815599321, 6.452359640394901952, 0.6004564335717228474 ) ) ;
#159872 = CARTESIAN_POINT ( 'NONE',  ( 4.493798347139664529, -2.191065130646638437, -0.05333993539427539510 ) ) ;
#159873 = VERTEX_POINT ( 'NONE', #132706 ) ;
#159874 = CARTESIAN_POINT ( 'NONE',  ( 1.369155121446740960E-15, 1.016439536705160407E-16, -11.18000000000000149 ) ) ;
#159875 = CARTESIAN_POINT ( 'NONE',  ( 0.007473969438118412655, 8.279395425053873936, 1.999986034896453324 ) ) ;
#159876 = CARTESIAN_POINT ( 'NONE',  ( 3.790386463472274148, 6.579812086429759788, 1.199719254218452047 ) ) ;
#159877 = CARTESIAN_POINT ( 'NONE',  ( 0.000000000000000000, -3.084374999522043304, -3.793834371823813445 ) ) ;
#159878 = CARTESIAN_POINT ( 'NONE',  ( -4.085803189671902480, 5.860132702740892263, -1.599625672291271394 ) ) ;
#159879 = CARTESIAN_POINT ( 'NONE',  ( 0.6685925339881376717, 1.356301626434471164, 1.492253803477984642 ) ) ;
#159880 = CARTESIAN_POINT ( 'NONE',  ( -9.002250809794006159, 10.56534270192358704, -1.082531754730543971 ) ) ;
#159881 = CARTESIAN_POINT ( 'NONE',  ( 5.910428620914669473, 5.860197910680708944, 0.000000000000000000 ) ) ;
#159882 = CARTESIAN_POINT ( 'NONE',  ( 5.401260523219934662, -1.778462342247935979, 1.059464396209061521 ) ) ;
#159883 = CARTESIAN_POINT ( 'NONE',  ( 4.178288987252887665, -1.108116244417625573, 1.575729328202896573 ) ) ;
#159884 = CARTESIAN_POINT ( 'NONE',  ( 6.275037739279882842, 1.841983620878117733, -1.043829292874172143 ) ) ;
#159885 = CARTESIAN_POINT ( 'NONE',  ( 4.822949958159288286, 6.649860922651058992, -1.599625672291256295 ) ) ;
#159886 = CARTESIAN_POINT ( 'NONE',  ( -0.008622056139523381901, 15.44694768828586540, 11.95585894197802013 ) ) ;
#159887 = CARTESIAN_POINT ( 'NONE',  ( 4.276189508915988036, -1.008629908464111269, -1.691384299763159182 ) ) ;
#159888 = CARTESIAN_POINT ( 'NONE',  ( 0.3577192552456122665, 2.167005522336755696, -0.3256184645209562190 ) ) ;
#159889 = CARTESIAN_POINT ( 'NONE',  ( 3.773894676421325034, 1.015518775504126614, 1.516979517045339287 ) ) ;
#159890 = CARTESIAN_POINT ( 'NONE',  ( 6.699137298928153683, 7.948653282571920720, 1.082531754730549967 ) ) ;
#159892 = EDGE_CURVE ( 'NONE', #113025, #11785, #35208, .T. ) ;
#159891 = CARTESIAN_POINT ( 'NONE',  ( 4.161989969270902812, 4.918371721313249623, 1.082531754730560403 ) ) ;
#159893 = CARTESIAN_POINT ( 'NONE',  ( -5.610041701004606196, 9.767075427805856691, -0.7998128361456362523 ) ) ;
#159894 = CARTESIAN_POINT ( 'NONE',  ( 6.215487077222150880, 6.216099443039444949, 0.000000000000000000 ) ) ;
#159895 = ORIENTED_EDGE ( 'NONE', *, *, #155782, .T. ) ;
#159897 = CARTESIAN_POINT ( 'NONE',  ( 5.502202757749218520, -0.9014697883563610459, 1.800137906301606305 ) ) ;
#159896 = CARTESIAN_POINT ( 'NONE',  ( 1.276629239279066574, 1.701104413791530767, -0.7050613402737049284 ) ) ;
#159898 = CARTESIAN_POINT ( 'NONE',  ( 1.300659708833833861, -2.077133573725042037, 0.9841232947556498578 ) ) ;
#159899 = CARTESIAN_POINT ( 'NONE',  ( 5.436364959771895045, -1.092926877770916017, 1.628904810760459121 ) ) ;
#159900 = CARTESIAN_POINT ( 'NONE',  ( -5.148345644887285744, 7.029489223833707001, -1.599625672291256295 ) ) ;
#159901 = CARTESIAN_POINT ( 'NONE',  ( 4.074186250656476993, 7.493853916489129574, -0.5595503573846259959 ) ) ;
#159902 = CARTESIAN_POINT ( 'NONE',  ( -8.611400122974211868, 13.19838391011195888, 1.040834085586084257E-14 ) ) ;
#159903 = CARTESIAN_POINT ( 'NONE',  ( 0.8013346216862862192, -1.776568573310655985, 1.062853015585236482 ) ) ;
#159904 = CARTESIAN_POINT ( 'NONE',  ( -4.878955176071358757, 6.785476686873604280, -1.599625672291271394 ) ) ;
#159906 = CARTESIAN_POINT ( 'NONE',  ( 6.789980064821725669, -0.7525070324889830964, 1.600651327395278711 ) ) ;
#159905 = CARTESIAN_POINT ( 'NONE',  ( 1.909825778081200909, -0.9882315549833411428, -1.842464674945838654 ) ) ;
#159907 = CARTESIAN_POINT ( 'NONE',  ( -11.86145016429273191, 10.19999999999999929, 1.099999999999996758 ) ) ;
#159908 = VERTEX_POINT ( 'NONE', #80218 ) ;
#159909 = CARTESIAN_POINT ( 'NONE',  ( -0.2102771530458277249, 4.081134801423261571, -2.758393064927369576 ) ) ;
#159910 = CARTESIAN_POINT ( 'NONE',  ( 2.313636755748917473, 1.135937956827288042, -1.318730690005095241 ) ) ;
#159911 = CARTESIAN_POINT ( 'NONE',  ( 3.825371897350130723, 7.614684313550482031, 0.7998128361456321445 ) ) ;
#159913 = CARTESIAN_POINT ( 'NONE',  ( 1.579999999999991189, 8.674529973577531194, 2.500000000000000444 ) ) ;
#159912 = DIRECTION ( 'NONE',  ( 0.000000000000000000, -1.000000000000000000, 0.000000000000000000 ) ) ;
#159914 = CARTESIAN_POINT ( 'NONE',  ( 3.140908386031955324, -1.520905784971425589, 0.8136546746303519040 ) ) ;
#159915 =( BOUNDED_CURVE ( )  B_SPLINE_CURVE ( 3, ( #22821, #156057, #88936, #39105 ),
 .UNSPECIFIED., .F., .T. ) 
 B_SPLINE_CURVE_WITH_KNOTS ( ( 4, 4 ),
 ( 0.5000000000000018874, 1.000000000000000000 ),
 .UNSPECIFIED. ) 
 CURVE ( )  GEOMETRIC_REPRESENTATION_ITEM ( )  RATIONAL_B_SPLINE_CURVE ( ( 0.9999999999999974465, 0.3333333333333333703, 0.3333333333333358683, 1.000000000000000000 ) ) 
 REPRESENTATION_ITEM ( '' )  );
#159917 = EDGE_CURVE ( 'NONE', #164105, #39288, #10180, .T. ) ;
#159916 = CARTESIAN_POINT ( 'NONE',  ( 1.083813775577105565, -0.9808430935620198188, 1.959877696171570927 ) ) ;
#159918 = CARTESIAN_POINT ( 'NONE',  ( 3.967548030458594166, 0.2710504330169676845, -2.190103208553782821 ) ) ;
#159919 = CARTESIAN_POINT ( 'NONE',  ( -10.57449672806501262, 3.061848070889987561, -7.008429158759065913 ) ) ;
#159920 = AXIS2_PLACEMENT_3D ( 'NONE', #167503, #103575, #34293 ) ;
#159921 = CARTESIAN_POINT ( 'NONE',  ( 2.325261487346420797, -1.983500291700568852, -0.8831872222036639686 ) ) ;
#159922 = CARTESIAN_POINT ( 'NONE',  ( 0.8381832108898427114, 1.798179982845280467, 0.3147962740308178353 ) ) ;
#159923 = CARTESIAN_POINT ( 'NONE',  ( 2.975892561826110505, -0.8538584053617600533, 1.937700190512989362 ) ) ;
#159924 = CIRCLE ( 'NONE', #135660, 0.04999999999999989869 ) ;
#159925 = CARTESIAN_POINT ( 'NONE',  ( 6.539320575229274013, 7.053493080409727334, 2.394893457813539683 ) ) ;
#159926 = ORIENTED_EDGE ( 'NONE', *, *, #179458, .F. ) ;
#159928 = CARTESIAN_POINT ( 'NONE',  ( 1.364683531249986537, 0.9677083336747538400, -0.7879004041258239610 ) ) ;
#159927 = CARTESIAN_POINT ( 'NONE',  ( 4.124787647867947271, 0.1125639427311639490, 2.289740828591101174 ) ) ;
#159929 = CARTESIAN_POINT ( 'NONE',  ( 4.369805582306193870, 3.992528022312320957, 1.214306433183764966E-14 ) ) ;
#159930 = CARTESIAN_POINT ( 'NONE',  ( 3.018661757337009810, 6.673522483535157868, 0.000000000000000000 ) ) ;
#159931 = CARTESIAN_POINT ( 'NONE',  ( 6.024141157665446222, -2.204869988984262896, 0.2693334978098835264 ) ) ;
#159932 = CARTESIAN_POINT ( 'NONE',  ( -5.246642258808529746, 9.064907035344523578, 0.000000000000000000 ) ) ;
#159933 = CARTESIAN_POINT ( 'NONE',  ( 3.863710590214593399, 7.451486755318259547, 1.040834085586084257E-14 ) ) ;
#159934 = CARTESIAN_POINT ( 'NONE',  ( -5.951666246274811556, 7.966696592119163256, 1.443375672974064550 ) ) ;
#159935 = CARTESIAN_POINT ( 'NONE',  ( 0.05648045292896410746, -9.990726591626527764, 10.91961852020055979 ) ) ;
#159936 = ORIENTED_EDGE ( 'NONE', *, *, #54326, .T. ) ;
#159937 = CARTESIAN_POINT ( 'NONE',  ( 4.236954046275762664, 2.015912997090345549, -0.05229627655192746472 ) ) ;
#159939 = CARTESIAN_POINT ( 'NONE',  ( 2.166912933460037660, 1.531321095959611966, -1.381971985785889423 ) ) ;
#159938 = CARTESIAN_POINT ( 'NONE',  ( 6.799577732453452761, 7.891594428405881878, -1.199719254218446718 ) ) ;
#159940 = FACE_BOUND ( 'NONE', #42903, .T. ) ;
#159941 = CARTESIAN_POINT ( 'NONE',  ( 4.217995187182922656, 6.014356699837137832, 1.443375672974058777 ) ) ;
#159943 = EDGE_CURVE ( 'NONE', #73840, #81936, #97560, .T. ) ;
#159942 = CARTESIAN_POINT ( 'NONE',  ( -3.285556943750000070, -3.609374999522043659, 0.000000000000000000 ) ) ;
#159944 = CARTESIAN_POINT ( 'NONE',  ( 1.364683531249990311, 4.884375000341417916, 1.214306433183764966E-14 ) ) ;
#159945 = CARTESIAN_POINT ( 'NONE',  ( 4.752002516643937469, 0.8370584164609263800, 2.025481692006773748 ) ) ;
#159946 = CARTESIAN_POINT ( 'NONE',  ( 2.479138880926802901, -2.011204309026824344, -0.1455328587063598189 ) ) ;
#159947 = CARTESIAN_POINT ( 'NONE',  ( 2.559893532628489954, -1.268187297466142338, 1.335118840784771166 ) ) ;
#159948 = EDGE_CURVE ( 'NONE', #137219, #205352, #163924, .T. ) ;
#159949 = CARTESIAN_POINT ( 'NONE',  ( 6.982612806237943559, 8.105135347821125436, -1.199719254218446718 ) ) ;
#159950 = SURFACE_STYLE_FILL_AREA ( #31030 ) ;
#159951 = CARTESIAN_POINT ( 'NONE',  ( 5.913091143547532624, 1.611232972626057247, 0.8583240166551919792 ) ) ;
#159952 = CARTESIAN_POINT ( 'NONE',  ( -7.660520486921249983, 8.896027641951645748, -1.199719254218446718 ) ) ;
#159954 = CARTESIAN_POINT ( 'NONE',  ( -4.197131071882288289, 7.054347462908075350, -1.199719254218455378 ) ) ;
#159953 = CARTESIAN_POINT ( 'NONE',  ( 5.559536883401111851, 0.4474127746876849221, -2.217688626266269392 ) ) ;
#159955 = CARTESIAN_POINT ( 'NONE',  ( 1.981218818260335413, -0.1044028718686483975, -2.103608768903475035 ) ) ;
#159956 = CARTESIAN_POINT ( 'NONE',  ( -5.074494633264801990, 9.142270515442742607, 0.7998128361456291469 ) ) ;
#159957 = CARTESIAN_POINT ( 'NONE',  ( 7.214910300766615769, 11.56914578420308715, -0.7998128361456291469 ) ) ;
#159958 = CARTESIAN_POINT ( 'NONE',  ( 6.278834536460164983, 9.379038488295265097, -1.082531754730548412 ) ) ;
#159959 = CARTESIAN_POINT ( 'NONE',  ( -7.069687034522070590, 10.33538640932937724, -1.199719254218440723 ) ) ;
#159960 = CARTESIAN_POINT ( 'NONE',  ( -0.07933194154558138866, -7.215597533182092960, 9.499668754385638181 ) ) ;
#159961 = CARTESIAN_POINT ( 'NONE',  ( 6.588899466117086767, 10.63087377720454363, 1.040834085586084257E-14 ) ) ;
#159962 = CARTESIAN_POINT ( 'NONE',  ( 4.031617349472986334, 7.784614636675013521, 0.3993128758026931457 ) ) ;
#159963 = CARTESIAN_POINT ( 'NONE',  ( -9.680158490477310806, 10.39586578175276266, 0.7216878364870438212 ) ) ;
#159964 = CARTESIAN_POINT ( 'NONE',  ( 2.707538781118669302, 1.902989223989959067, -1.145821276547890122 ) ) ;
#159965 = AXIS2_PLACEMENT_3D ( 'NONE', #19971, #36222, #118618 ) ;
#159966 = CARTESIAN_POINT ( 'NONE',  ( 6.883263157960371359, 7.052674735402435502, 2.544342468817725855 ) ) ;
#159967 = CARTESIAN_POINT ( 'NONE',  ( -6.961185525973791144, 7.086080966583015339, 0.7998128361456341429 ) ) ;
#159968 = CARTESIAN_POINT ( 'NONE',  ( 5.820528018968444961, 5.685037531751635953, 0.7998128361456341429 ) ) ;
#159969 = CARTESIAN_POINT ( 'NONE',  ( 4.035565188342554954, 1.848088059160474694, -0.6588067414724924076 ) ) ;
#159970 = CARTESIAN_POINT ( 'NONE',  ( 9.053093885623066939, 11.58502883802551153, -1.599625672291262513 ) ) ;
#159971 = CARTESIAN_POINT ( 'NONE',  ( -5.195561487237588594, 6.467898337602993486, 1.183867312878450484 ) ) ;
#159972 = CARTESIAN_POINT ( 'NONE',  ( 2.683624340501134853, 5.218313266304903664, -1.199719254218446718 ) ) ;
#159973 = CARTESIAN_POINT ( 'NONE',  ( -1.364683531250000748, 0.2593750003414205252, 0.000000000000000000 ) ) ;
#159974 = CARTESIAN_POINT ( 'NONE',  ( -5.343321937561608337, 5.406499480009534508, 0.7216878364870257245 ) ) ;
#159976 = VERTEX_POINT ( 'NONE', #1068 ) ;
#159975 = CARTESIAN_POINT ( 'NONE',  ( -7.131225611108100715, 9.342849184424693476, 1.443375672974078761 ) ) ;
#159977 =( BOUNDED_CURVE ( )  B_SPLINE_CURVE ( 2, ( #37588, #123211, #169718, #137243, #168650, #20254, #5051, #90632, #40812, #184884, #23452, #71127, #187028, #103670, #21307, #87415, #38662, #140468, #104740, #155614, #106920, #170787, #22378, #72197, #172944, #39726, #88489, #102593, #154548, #204320, #105832, #3989, #55978, #156692, #36509, #24522, #7199, #206481, #58111, #73272, #86338, #152409, #122131, #139375, #205406, #57045, #176143, #162025, #111196, #42955, #95971, #125328, #27743, #78615, #210750, #177200, #41887, #25595, #144740, #109065, #62373, #175081, #79689, #26667, #76484, #93838, #28815, #127473, #209669, #141541, #128535, #59168, #10412, #61312, #110132, #145801, #29887, #159877, #94899, #193444, #45087, #126395, #112263, #158816, #191289 ),
 .UNSPECIFIED., .F., .T. ) 
 B_SPLINE_CURVE_WITH_KNOTS ( ( 3, 2, 2, 2, 2, 2, 2, 2, 2, 2, 2, 2, 2, 2, 2, 2, 2, 2, 2, 2, 2, 2, 2, 2, 2, 2, 2, 2, 2, 2, 2, 2, 2, 2, 2, 2, 2, 2, 2, 2, 2, 2, 3 ),
 ( 0.1645590526585348767, 0.1666666666666666574, 0.1805555555555555525, 0.1944444444444444475, 0.2083333333333333426, 0.2222222222222222099, 0.2361111111111111049, 0.2500000000000000000, 0.2638888888888888951, 0.2777777777777777901, 0.2916666666666666852, 0.3055555555555555802, 0.3194444444444444198, 0.3333333333333333148, 0.3472222222222222099, 0.3611111111111111049, 0.3750000000000000000, 0.3888888888888888951, 0.4027777777777777901, 0.4166666666666666852, 0.4305555555555555802, 0.4444444444444444198, 0.4583333333333333148, 0.4722222222222222099, 0.4861111111111111049, 0.5000000000000000000, 0.5138888888888888395, 0.5277777777777777901, 0.5416666666666666297, 0.5555555555555555802, 0.5694444444444444198, 0.5833333333333333703, 0.5972222222222222099, 0.6111111111111111605, 0.6250000000000000000, 0.6388888888888888395, 0.6527777777777777901, 0.6666666666666666297, 0.6805555555555555802, 0.6944444444444444198, 0.7083333333333333703, 0.7222222222222222099, 0.7227726656456107124 ),
 .UNSPECIFIED. ) 
 CURVE ( )  GEOMETRIC_REPRESENTATION_ITEM ( )  RATIONAL_B_SPLINE_CURVE ( ( 0.9655093951251874085, 0.9796695950283244025, 1.000000000000000000, 0.8660254037844387076, 1.000000000000000000, 0.8660254037844387076, 1.000000000000000000, 0.8660254037844387076, 1.000000000000000000, 0.8660254037844387076, 1.000000000000000000, 0.8660254037844387076, 1.000000000000000000, 0.8660254037844387076, 1.000000000000000000, 0.8660254037844387076, 1.000000000000000000, 0.8660254037844387076, 1.000000000000000000, 0.8660254037844387076, 1.000000000000000000, 0.8660254037844387076, 1.000000000000000000, 0.8660254037844387076, 1.000000000000000000, 0.8660254037844387076, 1.000000000000000000, 0.8660254037844387076, 1.000000000000000000, 0.8660254037844387076, 1.000000000000000000, 0.8660254037844387076, 1.000000000000000000, 0.8660254037844387076, 1.000000000000000000, 0.8660254037844387076, 1.000000000000000000, 0.8660254037844387076, 1.000000000000000000, 0.8660254037844387076, 1.000000000000000000, 0.8660254037844387076, 1.000000000000000000, 0.8660254037844387076, 1.000000000000000000, 0.8660254037844387076, 1.000000000000000000, 0.8660254037844387076, 1.000000000000000000, 0.8660254037844387076, 1.000000000000000000, 0.8660254037844387076, 1.000000000000000000, 0.8660254037844387076, 1.000000000000000000, 0.8660254037844387076, 1.000000000000000000, 0.8660254037844387076, 1.000000000000000000, 0.8660254037844387076, 1.000000000000000000, 0.8660254037844387076, 1.000000000000000000, 0.8660254037844387076, 1.000000000000000000, 0.8660254037844387076, 1.000000000000000000, 0.8660254037844387076, 1.000000000000000000, 0.8660254037844387076, 1.000000000000000000, 0.8660254037844387076, 1.000000000000000000, 0.8660254037844387076, 1.000000000000000000, 0.8660254037844387076, 1.000000000000000000, 0.8660254037844387076, 1.000000000000000000, 0.8660254037844387076, 1.000000000000000000, 0.8660254037844387076, 1.000000000000000000, 0.9946903286520650811, 0.9898015223131609863 ) ) 
 REPRESENTATION_ITEM ( '' )  );
#159978 = CARTESIAN_POINT ( 'NONE',  ( 2.988655875014298857, -1.259908772670719657, 1.705623289672608678 ) ) ;
#159979 = CARTESIAN_POINT ( 'NONE',  ( -4.502189528189771472, 7.410248995266807803, -1.199719254218453823 ) ) ;
#159980 = CARTESIAN_POINT ( 'NONE',  ( 4.926735330553584369, 2.067573386176469796, 0.6309256262674377558 ) ) ;
#159981 = CARTESIAN_POINT ( 'NONE',  ( 3.473999211503727036, -1.775402473473717935, -0.4878004006634574230 ) ) ;
#159982 = CARTESIAN_POINT ( 'NONE',  ( -4.295139169456660078, 7.266651303919805294, 0.9588947021764819834 ) ) ;
#159983 = CARTESIAN_POINT ( 'NONE',  ( 0.6823417656249882723, -0.3447916663252489911, 1.181850606188755259 ) ) ;
#159984 = CARTESIAN_POINT ( 'NONE',  ( 5.331890987662370129, 1.715487909331077310, 0.2919898797263379975 ) ) ;
#159985 = CARTESIAN_POINT ( 'NONE',  ( 6.727182134110201162, 0.6069527724139511804, 1.765151538780465712 ) ) ;
#159986 = CARTESIAN_POINT ( 'NONE',  ( 2.724825686666657809, 6.122787701178987518, 0.000000000000000000 ) ) ;
#159987 = CARTESIAN_POINT ( 'NONE',  ( 10.98194350564910415, -7.666862915010147717, -0.6300133639306100264 ) ) ;
#159988 = CARTESIAN_POINT ( 'NONE',  ( 3.274459119871219848, -1.289031633699176949, 1.735169069618908821 ) ) ;
#159989 = VECTOR ( 'NONE', #191775, 1000.000000000000000 ) ;
#159990 = CARTESIAN_POINT ( 'NONE',  ( 5.413435409655408925, 0.5825687168248098180, 1.930121546480124461 ) ) ;
#159991 = CARTESIAN_POINT ( 'NONE',  ( -7.822691444960709006, 10.14955932391940330, -1.443375672974058777 ) ) ;
#159992 = CARTESIAN_POINT ( 'NONE',  ( 2.413140945657660907, 1.930630709398067246, 0.9725960170764782475 ) ) ;
#159993 = CARTESIAN_POINT ( 'NONE',  ( 3.743400255998735382, -1.490684086824107357, -1.290067496309046158 ) ) ;
#159994 = CARTESIAN_POINT ( 'NONE',  ( -0.005964567173097347699, -2.191213315851054944, -0.04726126812268362232 ) ) ;
#159995 = CARTESIAN_POINT ( 'NONE',  ( 4.300292543067584461, 1.499173285595749583, -1.234514081855079048 ) ) ;
#159998 = ORIENTED_EDGE ( 'NONE', *, *, #20380, .T. ) ;
#159997 = CARTESIAN_POINT ( 'NONE',  ( 0.007072395215912408162, 7.009756401597622144, -2.079987976222381629 ) ) ;
#159996 = CARTESIAN_POINT ( 'NONE',  ( -7.646435447983039424, 11.86466575604815787, 0.000000000000000000 ) ) ;
#159999 = CARTESIAN_POINT ( 'NONE',  ( -6.119526231721793330, 8.232809585132461194, 1.599625672291263179 ) ) ;
#160000 = DIRECTION ( 'NONE',  ( 0.000000000000000000, 1.000000000000000000, 0.000000000000000000 ) ) ;
#160002 = ORIENTED_EDGE ( 'NONE', *, *, #21559, .F. ) ;
#160001 = CARTESIAN_POINT ( 'NONE',  ( -5.829079699232685208, 5.765290835385048496, 0.000000000000000000 ) ) ;
#160003 = CARTESIAN_POINT ( 'NONE',  ( -7.646435447983039424, 11.86466575604815787, 0.000000000000000000 ) ) ;
#160004 = CARTESIAN_POINT ( 'NONE',  ( 2.327434156339613924, -0.0004056629378437063877, 2.206952907597827362 ) ) ;
#160005 = CARTESIAN_POINT ( 'NONE',  ( 0.000000000000000000, -1.596874999522041705, -3.793834371823813001 ) ) ;
#160006 = CARTESIAN_POINT ( 'NONE',  ( 6.227397112613878960, 0.1477489091250457076, -1.956280406615627854 ) ) ;
#160007 = CARTESIAN_POINT ( 'NONE',  ( -1.364683531250010295, 5.092708333674757171, 0.7879004041258379498 ) ) ;
#160008 = CARTESIAN_POINT ( 'NONE',  ( -1.500000000000011324, 3.702083334016152971, 0.8660254037844403729 ) ) ;
#160009 = CARTESIAN_POINT ( 'NONE',  ( 5.922464229660435286, 6.137557782886555735, -0.7752440879994120237 ) ) ;
#160011 = CARTESIAN_POINT ( 'NONE',  ( 3.834746474454188013E-15, 9.062500000000001776, 1.500000000000001554 ) ) ;
#160010 = CYLINDRICAL_SURFACE ( 'NONE', #31709, 1.250000000000000000 ) ;
#160012 = CARTESIAN_POINT ( 'NONE',  ( 5.630750141678076304, -1.662707896839428434, 0.7909858098210584831 ) ) ;
#160013 = ORIENTED_EDGE ( 'NONE', *, *, #120127, .F. ) ;
#160014 = CARTESIAN_POINT ( 'NONE',  ( 1.224999999999963007, 2.458333334016087335, -0.7072540797572877125 ) ) ;
#160015 = EDGE_CURVE ( 'NONE', #212450, #30458, #134333, .T. ) ;
#160016 = CARTESIAN_POINT ( 'NONE',  ( -6.320072162264675164, 10.52516795595079557, 0.7998128361456481317 ) ) ;
#160017 = DIRECTION ( 'NONE',  ( 1.000000000000000000, -0.000000000000000000, -0.000000000000000000 ) ) ;
#160018 = CARTESIAN_POINT ( 'NONE',  ( 6.064709079624690524, 0.6667526090060638122, 2.013086243192941716 ) ) ;
#160019 = CARTESIAN_POINT ( 'NONE',  ( 9.005029904505741811, 12.36406115350124502, 7.861980445344781465 ) ) ;
#160020 = CARTESIAN_POINT ( 'NONE',  ( 5.148345644887269756, 7.029489223833707001, -1.599625672291256295 ) ) ;
#160021 = AXIS2_PLACEMENT_3D ( 'NONE', #157255, #43515, #144244 ) ;
#160022 = CARTESIAN_POINT ( 'NONE',  ( 0.1103218441215253337, -0.8811044119183660817, -1.861458889230242164 ) ) ;
#160025 = CARTESIAN_POINT ( 'NONE',  ( 3.895923546780861724, -0.5813109859279729230, -1.747131793041277970 ) ) ;
#160024 = CARTESIAN_POINT ( 'NONE',  ( 2.277597300015369086, -1.806044765408962194, 0.4486390909646633118 ) ) ;
#160023 = CARTESIAN_POINT ( 'NONE',  ( -9.960032942013363311, 4.511256714876205720, 6.620518269535303091 ) ) ;
#160026 = CARTESIAN_POINT ( 'NONE',  ( 6.259060471003163428, 10.45398764947904624, -0.7998128361456291469 ) ) ;
#160027 = CARTESIAN_POINT ( 'NONE',  ( -9.351030442090584316, 14.56056703928365259, -7.441731297699171854 ) ) ;
#160028 = CARTESIAN_POINT ( 'NONE',  ( -5.824109505522200081, 8.952488968821326054, -1.199719254218452047 ) ) ;
#160029 = ORIENTED_EDGE ( 'NONE', *, *, #132358, .T. ) ;
#160030 = CARTESIAN_POINT ( 'NONE',  ( 4.354274438496381627, 2.206422198305586058, -0.05263853172451230661 ) ) ;
#160031 = CARTESIAN_POINT ( 'NONE',  ( 6.415309710857563630, -0.2865549832780675543, 2.244158528320794765 ) ) ;
#160032 = CARTESIAN_POINT ( 'NONE',  ( -5.965224400332865606, 7.022145224218852455, 1.082531754730549967 ) ) ;
#160033 = CARTESIAN_POINT ( 'NONE',  ( 5.660388270892238616, 1.809938998256973575, 0.08008182766248285456 ) ) ;
#160034 = CARTESIAN_POINT ( 'NONE',  ( 0.005092704479254389627, -0.09411098085002241043, 2.014433268766747887 ) ) ;
#160035 = CARTESIAN_POINT ( 'NONE',  ( -4.588064261291555646, 5.348899678044550576, 1.213891745583789872 ) ) ;
#160036 = CARTESIAN_POINT ( 'NONE',  ( 6.526239545637954720, 1.075124705556152138, -1.530631868311462362 ) ) ;
#160037 = CARTESIAN_POINT ( 'NONE',  ( 5.127564033545165323, -0.2766344828325461025, 1.892035409188079997 ) ) ;
#160038 = CARTESIAN_POINT ( 'NONE',  ( 5.016153647376212277, 5.914896012436124728, 1.082531754730558626 ) ) ;
#160039 = CARTESIAN_POINT ( 'NONE',  ( 1.024039198018782626, 1.117340804906666873, -1.500143343703803422 ) ) ;
#160040 = CARTESIAN_POINT ( 'NONE',  ( 0.7433754753295095385, 0.3886281223182270761, -1.978556061772406505 ) ) ;
#160042 = CARTESIAN_POINT ( 'NONE',  ( 3.686240278715931851, -1.037925599752804739, 1.832463683143903399 ) ) ;
#160041 = CARTESIAN_POINT ( 'NONE',  ( -8.910733272679575379, 11.41894145625809820, -1.599625672291263179 ) ) ;
#160043 = CARTESIAN_POINT ( 'NONE',  ( 7.262363838414439776, 11.62450824479221900, 0.7998128361456462443 ) ) ;
#160045 = CARTESIAN_POINT ( 'NONE',  ( -9.691380875670077444, 10.20103253123691189, 0.7998128361456462443 ) ) ;
#160044 = CARTESIAN_POINT ( 'NONE',  ( -0.7500000000000249800, -0.5583333333333134751, 1.299038105676659116 ) ) ;
#160046 = DIRECTION ( 'NONE',  ( -5.551115123125765446E-17, 0.000000000000000000, 1.000000000000000000 ) ) ;
#160047 = CARTESIAN_POINT ( 'NONE',  ( 3.392836290029502155, -1.947660480455270404, -0.5347636834307776255 ) ) ;
#160048 = CARTESIAN_POINT ( 'NONE',  ( -1.201851678989727383E-14, 3.321875000341421025, 1.575800808251672791 ) ) ;
#160049 = CARTESIAN_POINT ( 'NONE',  ( 3.765413976293345844, 5.416068943807445635, 1.599625672291267398 ) ) ;
#160050 = CARTESIAN_POINT ( 'NONE',  ( 3.866626755795209203, -1.454868229745639008, 1.598846606682593929 ) ) ;
#160051 = CARTESIAN_POINT ( 'NONE',  ( 7.526711554241970248, 8.810193563817646734, -1.199719254218452047 ) ) ;
#160052 = CARTESIAN_POINT ( 'NONE',  ( -1.001543065824772872E-14, 4.712500000000017231, 1.732050807568877637 ) ) ;
#160054 = CARTESIAN_POINT ( 'NONE',  ( 1.250000000000037526, 8.500000000000000000, 11.02939254900286237 ) ) ;
#160053 = CARTESIAN_POINT ( 'NONE',  ( 7.679767667498067496, 7.924426798361372093, 0.000000000000000000 ) ) ;
#160055 = CARTESIAN_POINT ( 'NONE',  ( 9.381879110532285182, 10.04787317181692075, 0.000000000000000000 ) ) ;
#160057 = DIRECTION ( 'NONE',  ( -0.000000000000000000, -1.000000000000000000, -0.000000000000000000 ) ) ;
#160056 = CARTESIAN_POINT ( 'NONE',  ( 1.153041021216383299, -0.5271860560512993121, -2.106100485105724562 ) ) ;
#160058 = CARTESIAN_POINT ( 'NONE',  ( -5.748293942514172805, 8.689798118699771479, -1.082531754730538864 ) ) ;
#160059 = CARTESIAN_POINT ( 'NONE',  ( -1.402160292154681736E-14, 2.196875000341423689, -1.575800808251660134 ) ) ;
#160060 = CARTESIAN_POINT ( 'NONE',  ( 1.892365914234435120, -0.5883382831698009685, -2.111031122750434808 ) ) ;
#160061 = CARTESIAN_POINT ( 'NONE',  ( 6.507146750061663099, 6.764461114227863447, -0.3103342489862369602 ) ) ;
#160062 = CARTESIAN_POINT ( 'NONE',  ( 2.606633135955916725, -0.8653751708443763180, -2.090666874703292599 ) ) ;
#160063 = CARTESIAN_POINT ( 'NONE',  ( -7.867809214632013770, 8.073532260025807261, 1.040834085586084257E-14 ) ) ;
#160064 = CARTESIAN_POINT ( 'NONE',  ( 0.6823417656249917140, 4.155208333674755394, 1.181850606188765695 ) ) ;
#160065 = CARTESIAN_POINT ( 'NONE',  ( 5.015976829175539109, 7.901154160799176651, 1.084432410706299477 ) ) ;
#160066 = CARTESIAN_POINT ( 'NONE',  ( -1.402160292154681736E-14, 12.56250000000000355, 1.732050807568881190 ) ) ;
#160067 = CARTESIAN_POINT ( 'NONE',  ( 7.539742822975472158, 7.968990512992423447, -0.7216878364870317197 ) ) ;
#160068 = CARTESIAN_POINT ( 'NONE',  ( 3.954177229731909549, 0.6350985098286399122, 1.652046152411037694 ) ) ;
#160069 = MECHANICAL_DESIGN_GEOMETRIC_PRESENTATION_REPRESENTATION (  '', ( #149722 ), #80605 ) ;
#160070 = CARTESIAN_POINT ( 'NONE',  ( 9.582915646760733708, 10.07448976417602893, 0.7998128361456462443 ) ) ;
#160071 = CARTESIAN_POINT ( 'NONE',  ( 0.9035134896902213830, 1.721610636892715984, 1.212602220121623775 ) ) ;
#160072 = AXIS2_PLACEMENT_3D ( 'NONE', #100926, #31689, #2335 ) ;
#160074 = CARTESIAN_POINT ( 'NONE',  ( 0.7499999999999885647, 0.5666666666666875241, -1.299038105676652899 ) ) ;
#160073 = CARTESIAN_POINT ( 'NONE',  ( -8.012344526598182026E-15, 9.796875000341399797, -1.575800808251669460 ) ) ;
#160075 = CARTESIAN_POINT ( 'NONE',  ( -4.285259070371116863, 7.157163461145040095, 1.199719254218452935 ) ) ;
#160076 = CARTESIAN_POINT ( 'NONE',  ( 6.468375372808552903, -1.978050569928070379, -0.3905794195708453542 ) ) ;
#160077 = VERTEX_POINT ( 'NONE', #146317 ) ;
#160078 = EDGE_CURVE ( 'NONE', #35104, #71781, #130126, .T. ) ;
#160079 = CARTESIAN_POINT ( 'NONE',  ( 10.42352117080803708, 11.05519620889787724, -0.7998128361456281477 ) ) ;
#160080 = CARTESIAN_POINT ( 'NONE',  ( 3.801501934187266230, -0.5436965770258190833, 1.789884385262895616 ) ) ;
#160081 = CARTESIAN_POINT ( 'NONE',  ( 4.715722526854881913, 0.4587184135333640111, -2.018627749927892179 ) ) ;
#160082 = CARTESIAN_POINT ( 'NONE',  ( -6.902509602688821744, 8.185920970292658083, -1.082531754730549967 ) ) ;
#160083 = DIRECTION ( 'NONE',  ( -3.330669073875478989E-16, 3.540251991789410786E-16, 1.000000000000000000 ) ) ;
#160084 = CARTESIAN_POINT ( 'NONE',  ( 8.751951852821344247, 10.16936423550178503, -1.199719254218446718 ) ) ;
#160085 = CARTESIAN_POINT ( 'NONE',  ( -1.530444406200916152, 8.694995975526813581, 2.517029436271791987 ) ) ;
#160086 = CARTESIAN_POINT ( 'NONE',  ( 7.842465510862060896, 8.114240948952696542, 0.000000000000000000 ) ) ;
#160087 = CARTESIAN_POINT ( 'NONE',  ( 5.081545378421249204, 4.913620246396115832, -0.1915759117748269125 ) ) ;
#160088 = CARTESIAN_POINT ( 'NONE',  ( 1.364683531249990311, 5.426041667008086655, 0.7879004041258500513 ) ) ;
#160089 = CARTESIAN_POINT ( 'NONE',  ( 3.560947883890089649, 1.548132398191165882, -1.204989647596923508 ) ) ;
#160090 = CARTESIAN_POINT ( 'NONE',  ( 1.300157425512000087, -1.823841169980220167, 0.8594962466553014435 ) ) ;
#160091 = ADVANCED_FACE ( 'NONE', ( #167864 ), #165169, .F. ) ;
#160092 = CARTESIAN_POINT ( 'NONE',  ( -0.3000000000000190292, 3.949999999999967315, 1.007084189318380618 ) ) ;
#160094 = CARTESIAN_POINT ( 'NONE',  ( 7.834948825496931057, -5.823938088759704534, 7.720982897393584565 ) ) ;
#160093 = CARTESIAN_POINT ( 'NONE',  ( 7.771848369131631351, 10.09024240211882351, -1.599625672291262513 ) ) ;
#160095 = CARTESIAN_POINT ( 'NONE',  ( 1.317418832401914930, -1.826178791559311509, 0.4043020138455517554 ) ) ;
#160096 = CARTESIAN_POINT ( 'NONE',  ( -1.201851678989727383E-14, 3.571875000341422357, 1.575800808251672791 ) ) ;
#160097 = CARTESIAN_POINT ( 'NONE',  ( 3.129155277828885140, 1.821763076032786977, 0.8570700399232934474 ) ) ;
#160099 = CARTESIAN_POINT ( 'NONE',  ( 1.968512934334982978, -2.077085554295199810, -0.4095441970272342136 ) ) ;
#160098 = CARTESIAN_POINT ( 'NONE',  ( -4.772106882330223954, 8.511282429453158827, -0.7216878364870267237 ) ) ;
#160100 = DIRECTION ( 'NONE',  ( 0.000000000000000000, 0.000000000000000000, -1.000000000000000000 ) ) ;
#160101 = CARTESIAN_POINT ( 'NONE',  ( 3.824723168590526523, -1.392635068473629500, 1.532133406949770960 ) ) ;
#160102 = CARTESIAN_POINT ( 'NONE',  ( 7.842465510862060896, 8.114240948952696542, 0.000000000000000000 ) ) ;
#160104 = CARTESIAN_POINT ( 'NONE',  ( 3.837121167867449945, 4.435395103055503441, 1.199719254218464037 ) ) ;
#160103 = CARTESIAN_POINT ( 'NONE',  ( -0.04130929284668418550, -1.869521504948624235, -0.9361258523304989421 ) ) ;
#160106 = ORIENTED_EDGE ( 'NONE', *, *, #68413, .T. ) ;
#160105 = CARTESIAN_POINT ( 'NONE',  ( 5.790036952090301448, -0.8187086143041850672, 1.631793460665122986 ) ) ;
#160107 = CARTESIAN_POINT ( 'NONE',  ( 7.228468454380276853, 11.58496363008569574, 1.040834085586084257E-14 ) ) ;
#160108 = FACE_OUTER_BOUND ( 'NONE', #205811, .T. ) ;
#160110 = VECTOR ( 'NONE', #79445, 1000.000000000000000 ) ;
#160109 = CARTESIAN_POINT ( 'NONE',  ( 10.32808049211214652, 11.37156981856230686, -7.280726186550563028 ) ) ;
#160111 = CARTESIAN_POINT ( 'NONE',  ( 5.983472182158235064, 2.041168445429199618, -0.8392293214988936212 ) ) ;
#160112 = CARTESIAN_POINT ( 'NONE',  ( 1.364683531250000748, 12.56770833367473372, -0.7879004041258355073 ) ) ;
#160113 = CARTESIAN_POINT ( 'NONE',  ( 4.652931681422667332, 0.3304644650514582116, 1.883354098946861344 ) ) ;
#160114 = CARTESIAN_POINT ( 'NONE',  ( -8.239604668803112375, 10.63595808506888396, -1.599625672291263179 ) ) ;
#160115 = CARTESIAN_POINT ( 'NONE',  ( 6.470265622219697477, 8.571729197388226140, -1.599625672291262513 ) ) ;
#160116 = CARTESIAN_POINT ( 'NONE',  ( 0.6801582343749952297, 2.255208333674735499, 1.178068619123839866 ) ) ;
#160117 = CARTESIAN_POINT ( 'NONE',  ( 3.009546912109283934, 6.454962464195385330, 0.000000000000000000 ) ) ;
#160118 = SURFACE_STYLE_USAGE ( .BOTH. , #127714 ) ;
#160119 = CARTESIAN_POINT ( 'NONE',  ( 4.660252114795294887, 6.460046772059735432, -1.599625672291256295 ) ) ;
#160120 = VERTEX_POINT ( 'NONE', #10669 ) ;
#160121 = CARTESIAN_POINT ( 'NONE',  ( 0.000000000000000000, -4.000000000000003553, 0.000000000000000000 ) ) ;
#160122 = FACE_OUTER_BOUND ( 'NONE', #201631, .T. ) ;
#160123 = CARTESIAN_POINT ( 'NONE',  ( 5.481239241674765950, 9.616805891921051952, -0.7998128361456481317 ) ) ;
#160124 = CARTESIAN_POINT ( 'NONE',  ( -0.4465194593918104249, 3.080450244942120719, -0.4155024747329819634 ) ) ;
#160125 = PRESENTATION_LAYER_ASSIGNMENT (  '', '', ( #21865 ) ) ;
#160126 = AXIS2_PLACEMENT_3D ( 'NONE', #90517, #57997, #213555 ) ;
#160127 = CARTESIAN_POINT ( 'NONE',  ( -6.081925898509194184, 7.037820769655190212, 1.000852813763454252 ) ) ;
#160128 = CARTESIAN_POINT ( 'NONE',  ( -5.070386261830872598, 8.859275038870594088, 0.7216878364870458196 ) ) ;
#160129 = CARTESIAN_POINT ( 'NONE',  ( 3.659811400685081040, 6.357198169852855685, -1.199719254218446718 ) ) ;
#160130 = CARTESIAN_POINT ( 'NONE',  ( 2.834760172256750810, -1.883157219239324887, -0.5764521555583942414 ) ) ;
#160131 = CARTESIAN_POINT ( 'NONE',  ( 3.480092364642515701, -2.014234743589532695, -0.09611699103692641910 ) ) ;
#160132 = CARTESIAN_POINT ( 'NONE',  ( -8.193204901359996128, 8.453160561208463264, 1.040834085586084257E-14 ) ) ;
#160133 = CARTESIAN_POINT ( 'NONE',  ( 6.554440917563797875, 6.611545590104705994, -0.7998128361456481317 ) ) ;
#160134 = CARTESIAN_POINT ( 'NONE',  ( 6.727182134110199385, 1.257034414284210921, 2.204727292504021108 ) ) ;
#160135 = CARTESIAN_POINT ( 'NONE',  ( 4.013774469618203611, -1.125877316280783358, -1.879984707117538845 ) ) ;
#160136 = LINE ( 'NONE', #161207, #36420 ) ;
#160137 = CARTESIAN_POINT ( 'NONE',  ( 1.659075543930859764, -1.650851203806924294, -0.9926060514057006845 ) ) ;
#160138 = CARTESIAN_POINT ( 'NONE',  ( -9.321394304595349567, 10.83371376257142416, 1.199719254218462483 ) ) ;
#160139 = CARTESIAN_POINT ( 'NONE',  ( -0.1296875068448125334, 2.048176110289974261, -2.243787855586779401 ) ) ;
#160140 = CARTESIAN_POINT ( 'NONE',  ( 0.1329588055935396196, 0.006246367379872731426, -1.846049620084761367 ) ) ;
#160141 = CARTESIAN_POINT ( 'NONE',  ( -10.39336823037077195, 4.932734307774878424, -5.330979603150785451 ) ) ;
#160143 = EDGE_CURVE ( 'NONE', #133382, #187426, #74629, .T. ) ;
#160142 = CARTESIAN_POINT ( 'NONE',  ( 8.945682426918439845, 9.331051007693339727, 1.040834085586084257E-14 ) ) ;
#160144 = VECTOR ( 'NONE', #185807, 1000.000000000000000 ) ;
#160145 = CARTESIAN_POINT ( 'NONE',  ( 6.257251587906815793, 7.258880593101466161, 1.199719254218462483 ) ) ;
#160146 = CARTESIAN_POINT ( 'NONE',  ( -6.958662999125652782, -8.148356111791692058, 6.505896022970778958 ) ) ;
#160147 = CARTESIAN_POINT ( 'NONE',  ( 5.316205630334249754, 7.295602216847000498, -1.443375672974078761 ) ) ;
#160148 = ORIENTED_EDGE ( 'NONE', *, *, #136490, .T. ) ;
#160150 = CARTESIAN_POINT ( 'NONE',  ( 2.244791168117025837, 1.953224514136771006, 0.4868699220301163089 ) ) ;
#160149 = CARTESIAN_POINT ( 'NONE',  ( 6.550350952284553330, -1.418464805562440922, 1.173678288350611609 ) ) ;
#160151 = CARTESIAN_POINT ( 'NONE',  ( 4.306267096541755990, -2.002170989124392175, 1.128539623919281754 ) ) ;
#160153 = CARTESIAN_POINT ( 'NONE',  ( 2.219380450391433168, 0.3239122733160957890, -1.832380290584040505 ) ) ;
#160152 = CARTESIAN_POINT ( 'NONE',  ( -0.1290005225502675879, 5.719648796287211567, -2.768066027128403217 ) ) ;
#160154 = CARTESIAN_POINT ( 'NONE',  ( 0.000000000000000000, -1.246874999522042948, -3.793834371823813001 ) ) ;
#160155 = CARTESIAN_POINT ( 'NONE',  ( -0.1290005225502675879, 2.860092606084875033, -2.662085506130333457 ) ) ;
#160156 = CARTESIAN_POINT ( 'NONE',  ( 5.836178160628028522, -1.067892152678026951, -1.586260290404594597 ) ) ;
#160157 = CARTESIAN_POINT ( 'NONE',  ( -7.182068686937172153, 9.402166106225269715, 1.599625672291283607 ) ) ;
#160158 = CARTESIAN_POINT ( 'NONE',  ( -6.143253000767895600, 6.339752387083549934, 0.000000000000000000 ) ) ;
#160160 = CARTESIAN_POINT ( 'NONE',  ( 3.537841792810627606, 0.8420186812403904764, -1.670516725672297031 ) ) ;
#160159 = CARTESIAN_POINT ( 'NONE',  ( 4.616787868375789472, -0.1008748965102136408, 2.088423895528898733 ) ) ;
#160161 = CARTESIAN_POINT ( 'NONE',  ( 6.643132081016117851, 8.773406732650713025, 1.443375672974076540 ) ) ;
#160162 = CARTESIAN_POINT ( 'NONE',  ( 0.3656762941044484627, -7.723177556210781169, -10.97096416026298904 ) ) ;
#160163 = CARTESIAN_POINT ( 'NONE',  ( 6.463511695382619493, 0.2867160277617316622, -1.700725516685620553 ) ) ;
#160164 = CARTESIAN_POINT ( 'NONE',  ( -4.889686956022917919, 8.856385215335397021, 1.214306433183764966E-14 ) ) ;
#160165 = CARTESIAN_POINT ( 'NONE',  ( 1.547078507373225165, -1.226440487959565173, 1.226290910655163380 ) ) ;
#160166 = CARTESIAN_POINT ( 'NONE',  ( 0.000000000000000000, 0.08000000000000020983, 0.000000000000000000 ) ) ;
#160167 = CARTESIAN_POINT ( 'NONE',  ( -1.451998047845039830, 7.315968950354585942, -4.301760722576429607 ) ) ;
#160169 = CARTESIAN_POINT ( 'NONE',  ( 6.209878556409044847, 0.6379485578581347571, -2.075210184031409888 ) ) ;
#160168 = B_SPLINE_CURVE_WITH_KNOTS ( 'NONE', 3,
 ( #93925, #159966, #11571, #143763, #56070, #122226, #105929, #171953, #23542, #89651, #155705 ),
 .UNSPECIFIED., .F., .F.,
 ( 4, 1, 1, 1, 1, 1, 1, 1, 4 ),
 ( 0.000000000000000000, 0.2254704865597413344, 0.3973194950497592193, 0.5246576192285303808, 0.6166070239209043846, 0.6823180413592140336, 0.7309932997181896042, 0.7717238569598857678, 1.000000000000000000 ),
 .UNSPECIFIED. ) ;
#160170 = CARTESIAN_POINT ( 'NONE',  ( 3.932112477472641920, 0.9751300899686901058, -1.543267412809447681 ) ) ;
#160171 = CARTESIAN_POINT ( 'NONE',  ( 1.920681792755132067, -1.391007931628859939, 1.383589105726056756 ) ) ;
#160172 = CARTESIAN_POINT ( 'NONE',  ( 0.07011551774125344971, -0.9937341303020963412, 1.869520526064169408 ) ) ;
#160173 = CARTESIAN_POINT ( 'NONE',  ( 0.000000000000000000, 3.599999999999999201, 0.000000000000000000 ) ) ;
#160174 = CARTESIAN_POINT ( 'NONE',  ( -0.7499999999999972244, 5.608333333333353821, -1.299038105676652011 ) ) ;
#160175 = CARTESIAN_POINT ( 'NONE',  ( 9.088043039861931405, 9.497138389460751284, 1.040834085586084257E-14 ) ) ;
#160176 = CARTESIAN_POINT ( 'NONE',  ( 2.684367718930933844, 1.136400967617630986, 1.790090880730066392 ) ) ;
#160177 = CARTESIAN_POINT ( 'NONE',  ( -4.961921032921567054, 4.891255414604337659, 0.7216878364870317197 ) ) ;
#160178 = CARTESIAN_POINT ( 'NONE',  ( 0.000000000000000000, 6.999999999999999112, -11.00000000000000000 ) ) ;
#160179 = CARTESIAN_POINT ( 'NONE',  ( -5.725072791067139732, 6.113630025739863250, -0.7036897515925732982 ) ) ;
#160180 = CARTESIAN_POINT ( 'NONE',  ( 0.9892257793299992219, 0.1485654903058269416, 2.064951490685583924 ) ) ;
#160182 = CARTESIAN_POINT ( 'NONE',  ( -1.500000000000015099, 14.51041666734946567, -0.8660254037844309360 ) ) ;
#160181 = CARTESIAN_POINT ( 'NONE',  ( -10.85972455493619471, 4.659241855712780378, 5.106971684771559161 ) ) ;
#160184 = ORIENTED_EDGE ( 'NONE', *, *, #66221, .F. ) ;
#160183 = CARTESIAN_POINT ( 'NONE',  ( 2.983289111093189394, -2.053184633062016484, -0.8481636011889515103 ) ) ;
#160185 = CARTESIAN_POINT ( 'NONE',  ( 0.5812297525147345212, -0.8198687466959112546, 2.147686052911641497 ) ) ;
#160187 = CARTESIAN_POINT ( 'NONE',  ( 5.155161738035724639, 1.717805270433828246, -1.141362358335789251 ) ) ;
#160186 = CARTESIAN_POINT ( 'NONE',  ( 3.063252641683779753, 5.661212951017999373, 1.199719254218450271 ) ) ;
#160189 = CARTESIAN_POINT ( 'NONE',  ( 3.475000000000000533, -1.254166666666665098, 2.006292185433948827 ) ) ;
#160188 = CARTESIAN_POINT ( 'NONE',  ( 5.180097208873055692, 8.201141289397330780, -1.199719254218450271 ) ) ;
#160190 = ADVANCED_FACE ( 'NONE', ( #192619 ), #10363, .T. ) ;
#160191 = CARTESIAN_POINT ( 'NONE',  ( 0.2333540202161506205, 0.2466631755442013352, -2.080888922837381916 ) ) ;
#160192 = CARTESIAN_POINT ( 'NONE',  ( 5.196754805642953556, 1.508532920973480795, 1.055450849767838317 ) ) ;
#160193 = CARTESIAN_POINT ( 'NONE',  ( 5.040934186182656873, 4.775511393501539636, 1.040834085586084257E-14 ) ) ;
#160194 = CARTESIAN_POINT ( 'NONE',  ( 3.117853853556023846, -0.8486709934477435491, -1.501428560464845630 ) ) ;
#160195 = CARTESIAN_POINT ( 'NONE',  ( 1.094935803221647186, 1.780670018850015079, 0.9462964651613046119 ) ) ;
#160196 = CARTESIAN_POINT ( 'NONE',  ( 3.305630555216050759, 1.456526447221625276, -1.778376517212407748 ) ) ;
#160197 = CARTESIAN_POINT ( 'NONE',  ( 2.319920442056855325, -2.194974118250800021, 0.5478587534586392138 ) ) ;
#160198 = CARTESIAN_POINT ( 'NONE',  ( 5.707678396406405064, -0.5131847548165735518, 2.042461488563215966 ) ) ;
#160199 = CARTESIAN_POINT ( 'NONE',  ( -6.617788377246193399, 8.814115421577600529, -1.443375672974066548 ) ) ;
#160200 = CARTESIAN_POINT ( 'NONE',  ( 4.182668740906975380, -0.1716826142807558186, -1.761352938113736277 ) ) ;
#160202 = EDGE_CURVE ( 'NONE', #12101, #20507, #24447, .T. ) ;
#160201 = CARTESIAN_POINT ( 'NONE',  ( 6.311484202361478779, 7.322151976631905868, -1.199719254218446718 ) ) ;
#160204 = CARTESIAN_POINT ( 'NONE',  ( 6.233931918547526152, 2.266764885754421144, 0.3408509611897111991 ) ) ;
#160203 = CARTESIAN_POINT ( 'NONE',  ( 4.624739795592929248, 6.488892076315451618, -1.443375672974068769 ) ) ;
#160205 = CARTESIAN_POINT ( 'NONE',  ( 4.892441406782115365, 1.528958278715689234, -1.025397978904031060 ) ) ;
#160206 = CARTESIAN_POINT ( 'NONE',  ( -5.623934791570306402, 5.455678766453782913, 0.7998128361456341429 ) ) ;
#160207 = UNCERTAINTY_MEASURE_WITH_UNIT (LENGTH_MEASURE( 1.000000000000000082E-05 ), #179115, 'distance_accuracy_value', 'NONE');
#160208 = CARTESIAN_POINT ( 'NONE',  ( 5.083944415000174466, 7.914723669933440675, -1.082531754730549078 ) ) ;
#160209 = CARTESIAN_POINT ( 'NONE',  ( -1.201851678989727383E-14, 3.087500000000026112, -1.732050807568863648 ) ) ;
#160210 = CARTESIAN_POINT ( 'NONE',  ( 4.207102436150745639, -0.3756362130699179014, 2.158856393654845274 ) ) ;
#160211 = CARTESIAN_POINT ( 'NONE',  ( -3.436101866059630527, 6.096203712789787232, 1.199719254218462483 ) ) ;
#160212 = DIRECTION ( 'NONE',  ( 0.000000000000000000, -1.000000000000000000, 0.000000000000000000 ) ) ;
#160213 = CYLINDRICAL_SURFACE ( 'NONE', #4030, 0.08000000000000020983 ) ;
#160214 = CARTESIAN_POINT ( 'NONE',  ( -1.201851678989727383E-14, 4.196875000341417028, -1.575800808251660134 ) ) ;
#160215 = CARTESIAN_POINT ( 'NONE',  ( 3.088414555603569145, -1.898068263532082245, -0.3288968790781700013 ) ) ;
#160216 = CARTESIAN_POINT ( 'NONE',  ( -0.6823417656250003738, 8.901041667008065872, 1.181850606188754593 ) ) ;
#160217 = CARTESIAN_POINT ( 'NONE',  ( -3.253593677599670109, 5.779314476299451719, 1.082531754730560403 ) ) ;
#160218 = CARTESIAN_POINT ( 'NONE',  ( -0.1224090711158704881, -1.988194106603015987, -0.9910323345065151779 ) ) ;
#160219 = VERTEX_POINT ( 'NONE', #109333 ) ;
#160222 = CIRCLE ( 'NONE', #125671, 3.000000000000010214 ) ;
#160221 = CARTESIAN_POINT ( 'NONE',  ( 4.248158675776232407, 7.140945339103782707, 1.189375853805716643 ) ) ;
#160220 = DIRECTION ( 'NONE',  ( 0.000000000000000000, 0.000000000000000000, 1.000000000000000000 ) ) ;
#160223 = CARTESIAN_POINT ( 'NONE',  ( 5.030238685870051185, 5.827365540725222282, -1.199719254218452047 ) ) ;
#160224 = FACE_OUTER_BOUND ( 'NONE', #181113, .T. ) ;
#160225 =( NAMED_UNIT ( * ) PLANE_ANGLE_UNIT ( ) SI_UNIT ( $, .RADIAN. ) );
#160226 = CARTESIAN_POINT ( 'NONE',  ( 0.4830727172305282480, 6.835855489795042317, -3.747807319729578701 ) ) ;
#160227 = CARTESIAN_POINT ( 'NONE',  ( -4.326460414921602826, 8.061637894134911164, 8.322892513849239118E-08 ) ) ;
#160228 = CARTESIAN_POINT ( 'NONE',  ( 0.1683002474503410839, -0.8351952195557799108, -1.773497582445908938 ) ) ;
#160229 = CARTESIAN_POINT ( 'NONE',  ( -1.364683531250012516, 1.092708333674754506, 0.7879004041258379498 ) ) ;
#160230 = CARTESIAN_POINT ( 'NONE',  ( 6.508665849870632236, 1.605377118863276387, -1.447859449074364591 ) ) ;
#160231 = CARTESIAN_POINT ( 'NONE',  ( 5.441838459065293065, 1.316327937319297758, 1.454900926449454124 ) ) ;
#160232 = CARTESIAN_POINT ( 'NONE',  ( -7.960608749518247151, 12.43912730774665576, 0.000000000000000000 ) ) ;
#160233 = CARTESIAN_POINT ( 'NONE',  ( -6.033015167956810920, 7.101234453113482559, -1.082531754730543083 ) ) ;
#160234 = CARTESIAN_POINT ( 'NONE',  ( 5.401312781148373432, 1.764888628567516049, 1.247983453017486699 ) ) ;
#160236 = ORIENTED_EDGE ( 'NONE', *, *, #3792, .F. ) ;
#160235 = CARTESIAN_POINT ( 'NONE',  ( -0.1106727585415863135, 6.947232144882324434, -2.598525652753637782 ) ) ;
#160237 = CARTESIAN_POINT ( 'NONE',  ( 1.364683531249988535, 4.113541667008088432, 0.7879004041258500513 ) ) ;
#160238 = CARTESIAN_POINT ( 'NONE',  ( 0.6494046996203367561, 0.5928216254872006319, -1.774177939146783345 ) ) ;
#160239 = CARTESIAN_POINT ( 'NONE',  ( 5.993412714446900047, 1.671717086469927560, 0.4595231857335341785 ) ) ;
#160241 = CARTESIAN_POINT ( 'NONE',  ( 3.351304529449970371, 0.5305821810032870234, -2.126252377916526992 ) ) ;
#160240 = CARTESIAN_POINT ( 'NONE',  ( 0.6801582343749970061, 0.8072916670080754198, -1.178068619123858962 ) ) ;
#160242 = CARTESIAN_POINT ( 'NONE',  ( 3.276728144386112263, -1.376063543960687641, 1.852258789692583507 ) ) ;
#160243 = CARTESIAN_POINT ( 'NONE',  ( 5.483688661837972766, 1.380929853543419128, 1.529855004671219820 ) ) ;
#160244 = CARTESIAN_POINT ( 'NONE',  ( 1.324054681829215818, 1.871493247920783753, 0.5181311518769672331 ) ) ;
#160245 = CARTESIAN_POINT ( 'NONE',  ( -6.683806541412780078, 6.900121841177441873, -0.7216878364870267237 ) ) ;
#160246 = CARTESIAN_POINT ( 'NONE',  ( -11.97929049433705373, 12.22000000000000064, 0.7046979865771783036 ) ) ;
#160247 = CARTESIAN_POINT ( 'NONE',  ( 5.010073305087408002, -0.7609581946756528437, 1.979555329295646260 ) ) ;
#160248 = CARTESIAN_POINT ( 'NONE',  ( 0.000000000000000000, 0.5000000000000004441, -3.475000000000000089 ) ) ;
#160249 = CARTESIAN_POINT ( 'NONE',  ( 2.531875153343257523, -1.674887184936912909, 1.122499117612890673 ) ) ;
#160250 = CARTESIAN_POINT ( 'NONE',  ( -6.575341312503472757, 7.733948288417905381, 1.082531754730549967 ) ) ;
#160251 = CARTESIAN_POINT ( 'NONE',  ( 6.194375513154499302, -2.195555142843173879, -0.2223249613259313806 ) ) ;
#160252 = CARTESIAN_POINT ( 'NONE',  ( 3.285556943750000070, -1.071874999522042016, 0.000000000000000000 ) ) ;
#160253 = CARTESIAN_POINT ( 'NONE',  ( -3.257807097882708725, -3.093939727723714839, -1.071007828276776319 ) ) ;
#160254 = FACE_OUTER_BOUND ( 'NONE', #136218, .T. ) ;
#160255 = CARTESIAN_POINT ( 'NONE',  ( -7.262327558775498737, 8.501745569106741840, 1.199719254218452047 ) ) ;
#160257 = CARTESIAN_POINT ( 'NONE',  ( 4.365362273920238678, 7.076377838673507448, 1.082531754730558626 ) ) ;
#160256 = CARTESIAN_POINT ( 'NONE',  ( -5.181409149560055383, 7.856748536063159705, 1.265847179423916335 ) ) ;
#160258 = CARTESIAN_POINT ( 'NONE',  ( -4.859018323670466266, 8.113919647779686883, 0.9376688295712337640 ) ) ;
#160259 = ORIENTED_EDGE ( 'NONE', *, *, #49979, .T. ) ;
#160260 = CARTESIAN_POINT ( 'NONE',  ( 3.924726224964281140, 1.956320258297845172, 0.6483119717206936583 ) ) ;
#160261 = CARTESIAN_POINT ( 'NONE',  ( 4.048877618987437366, 7.739821757498127397, -0.4883357188320930353 ) ) ;
#160262 = CARTESIAN_POINT ( 'NONE',  ( 0.2329586101569872392, 0.008238550247445528343, -1.845944905557160398 ) ) ;
#160263 = CARTESIAN_POINT ( 'NONE',  ( -3.906720819032141190, 7.709591388846142479, -0.7998128361456281477 ) ) ;
#160264 = CARTESIAN_POINT ( 'NONE',  ( -5.191846479390389568, 5.021852078902356631, 0.7998128361456281477 ) ) ;
#160265 = CARTESIAN_POINT ( 'NONE',  ( 4.582678730018482582, -1.317704446820912700, 1.530705718492784362 ) ) ;
#160266 = CARTESIAN_POINT ( 'NONE',  ( 1.499999999999987121, 1.045833333333352266, -0.8660254037844253849 ) ) ;
#160268 = CARTESIAN_POINT ( 'NONE',  ( 9.747949258545622442, 10.47495501116581984, 0.000000000000000000 ) ) ;
#160267 = CARTESIAN_POINT ( 'NONE',  ( -3.793249116773374396, 7.647484079536056356, 0.7998128361456352531 ) ) ;
#160269 = CARTESIAN_POINT ( 'NONE',  ( 6.982612806237943559, 8.105135347821125436, -1.199719254218446718 ) ) ;
#160270 = CARTESIAN_POINT ( 'NONE',  ( 3.133719265644947960, -1.383057153600345535, -1.528062560492246202 ) ) ;
#160271 = CARTESIAN_POINT ( 'NONE',  ( 2.936172824561167349, -1.650081981912490336, -1.158688413653415239 ) ) ;
#160272 = ORIENTED_EDGE ( 'NONE', *, *, #137765, .T. ) ;
#160273 = CARTESIAN_POINT ( 'NONE',  ( 1.878188943807069800, 3.299815425349211129, -0.3999999999999993006 ) ) ;
#160274 = CARTESIAN_POINT ( 'NONE',  ( 5.691725559638619814, 5.534767995866836543, 1.040834085586084257E-14 ) ) ;
#160275 = B_SPLINE_CURVE_WITH_KNOTS ( 'NONE', 3,
 ( #1740, #49461, #85151, #52652, #151236 ),
 .UNSPECIFIED., .F., .F.,
 ( 4, 1, 4 ),
 ( 0.001713136426838625295, 0.001716577612580663008, 0.001720018798322700722 ),
 .UNSPECIFIED. ) ;
#160277 = ORIENTED_EDGE ( 'NONE', *, *, #20664, .F. ) ;
#160276 = CARTESIAN_POINT ( 'NONE',  ( -0.5610452518370884212, 7.732119650022654334, -1.919700688223590079 ) ) ;
#160278 = CARTESIAN_POINT ( 'NONE',  ( 2.829453700430568652, -1.392333688140505510, 1.458332250898628057 ) ) ;
#160279 = CARTESIAN_POINT ( 'NONE',  ( 2.958754162918544761, 0.2696264243384552950, -1.821159755858774654 ) ) ;
#160280 = CARTESIAN_POINT ( 'NONE',  ( 1.155362744787872931, -1.816424715318950112, 1.423309470994944537 ) ) ;
#160281 = CARTESIAN_POINT ( 'NONE',  ( 5.910428620914669473, 5.860197910680708944, 0.000000000000000000 ) ) ;
#160282 = CARTESIAN_POINT ( 'NONE',  ( 2.477987356985793088, 1.327747062846416526, 1.705691702009938915 ) ) ;
#160283 = CARTESIAN_POINT ( 'NONE',  ( -5.900823170445743671, 7.907379670318584353, 1.599625672291269396 ) ) ;
#160284 = ORIENTED_EDGE ( 'NONE', *, *, #56195, .F. ) ;
#160285 = DIRECTION ( 'NONE',  ( -0.9632918427306580433, 0.000000000000000000, 0.2684563758389303945 ) ) ;
#160286 = CIRCLE ( 'NONE', #8135, 0.07999999999999998779 ) ;
#160287 = CARTESIAN_POINT ( 'NONE',  ( 1.604156678829884886, -0.6703249191640224813, -1.746612230856612769 ) ) ;
#160288 = AXIS2_PLACEMENT_3D ( 'NONE', #107855, #3843, #206338 ) ;
#160289 = CARTESIAN_POINT ( 'NONE',  ( 5.366080375918201639, 0.9711980517450971018, 1.715566965677978173 ) ) ;
#160291 = CARTESIAN_POINT ( 'NONE',  ( 8.771762197917315262, 10.29643932140079166, -1.082531754730543083 ) ) ;
#160290 = CARTESIAN_POINT ( 'NONE',  ( -1.364683531249997417, 4.009375000341424133, 1.214306433183764966E-14 ) ) ;
#160293 = CARTESIAN_POINT ( 'NONE',  ( 0.5927436934281338221, -2.190715567557582677, -0.2661302102612560505 ) ) ;
#160292 = CARTESIAN_POINT ( 'NONE',  ( -7.389357414647957256, 8.579670724299436557, 1.199719254218450271 ) ) ;
#160294 = CARTESIAN_POINT ( 'NONE',  ( 6.408651866624735405, 0.6456447432892989946, 1.967203394946090977 ) ) ;
#160295 = CARTESIAN_POINT ( 'NONE',  ( 6.819914962873951936, 7.915321197229798322, -1.199719254218446718 ) ) ;
#160296 = CARTESIAN_POINT ( 'NONE',  ( -4.726989112658928072, 8.666571064744069020, 1.040834085586084257E-14 ) ) ;
#160297 = CARTESIAN_POINT ( 'NONE',  ( 6.639320575229248789, 2.413637632230402286, 2.584074196137386092 ) ) ;
#160298 = CARTESIAN_POINT ( 'NONE',  ( 4.592626242060598329, -0.4308863251132522554, -1.923655822462609466 ) ) ;
#160299 = CARTESIAN_POINT ( 'NONE',  ( 0.05319811239242258627, 0.3688592364489845510, 2.088132107045739705 ) ) ;
#160300 = CARTESIAN_POINT ( 'NONE',  ( 1.499999999999989120, 0.3062500006828158816, 0.000000000000000000 ) ) ;
#160301 = CARTESIAN_POINT ( 'NONE',  ( 4.899205829341429563, 1.920759858200033587, -1.278847778945918279 ) ) ;
#160302 = CARTESIAN_POINT ( 'NONE',  ( 2.096602096640389767, 2.039512422605322950, 0.3069443246750125365 ) ) ;
#160303 = CARTESIAN_POINT ( 'NONE',  ( 7.212574532790092974, 9.437756259720353924, -1.443375672974057666 ) ) ;
#160305 = CARTESIAN_POINT ( 'NONE',  ( 4.694866332082116678, 8.699370830729650450, 0.7998128361456341429 ) ) ;
#160304 = VECTOR ( 'NONE', #182026, 1000.000000000000227 ) ;
#160306 = CARTESIAN_POINT ( 'NONE',  ( 5.910428620914669473, 5.860197910680708944, 0.000000000000000000 ) ) ;
#160307 = CARTESIAN_POINT ( 'NONE',  ( 1.364683531249988757, 2.196875000341415252, 1.214306433183764966E-14 ) ) ;
#160308 = CARTESIAN_POINT ( 'NONE',  ( -1.674002081864904623, 14.52982574599248977, 11.91747069027295858 ) ) ;
#160309 = CARTESIAN_POINT ( 'NONE',  ( 4.622967192135525316, 8.337286124226029216, -0.7216878364870207285 ) ) ;
#160310 = CARTESIAN_POINT ( 'NONE',  ( 4.141221389272289777, -0.2091070545618961274, -2.161069556037761519 ) ) ;
#160311 = CARTESIAN_POINT ( 'NONE',  ( -7.065207446497166366, 9.336104335703744539, 0.000000000000000000 ) ) ;
#160313 = CARTESIAN_POINT ( 'NONE',  ( 4.476008884455379366, -1.787108923542475525, -0.4427587100873929815 ) ) ;
#160312 = CARTESIAN_POINT ( 'NONE',  ( -2.480778921620681921, 5.838066475291996404, 1.040834085586084257E-14 ) ) ;
#160315 = CARTESIAN_POINT ( 'NONE',  ( 6.620655732516652847, 2.468432086671234149, 2.210906647470804565 ) ) ;
#160314 = CARTESIAN_POINT ( 'NONE',  ( 1.364683531249992088, 5.634375000341417916, 1.214306433183764966E-14 ) ) ;
#160316 = CARTESIAN_POINT ( 'NONE',  ( 5.337503337980974649, 0.8888059580158399475, -2.003405333693850654 ) ) ;
#160317 = DIRECTION ( 'NONE',  ( 0.000000000000000000, 0.000000000000000000, 1.000000000000000000 ) ) ;
#160318 = CARTESIAN_POINT ( 'NONE',  ( 6.280173827431851485, -1.216757814587710929, 1.907326054681435235 ) ) ;
#160319 = VERTEX_POINT ( 'NONE', #59435 ) ;
#160320 = CARTESIAN_POINT ( 'NONE',  ( -4.010472434439474654, 7.801430412234481082, -0.4134458547365611469 ) ) ;
#160321 = CARTESIAN_POINT ( 'NONE',  ( 11.48806469435255551, 11.33089772872448719, -3.468902948106704631 ) ) ;
#160322 = CARTESIAN_POINT ( 'NONE',  ( 5.260375520412221562, 7.786458765878076171, 1.288147692060326532 ) ) ;
#160323 = CARTESIAN_POINT ( 'NONE',  ( -4.624739795592943459, 6.488892076315448065, -1.443375672974066548 ) ) ;
#160324 = CARTESIAN_POINT ( 'NONE',  ( 3.119784744920330422, 6.653849612466795627, 0.7216878364870257245 ) ) ;
#160325 = CARTESIAN_POINT ( 'NONE',  ( 1.111743784240331712, -0.7909239834335696218, -1.583357840528883287 ) ) ;
#160326 = CARTESIAN_POINT ( 'NONE',  ( 4.916656812733911863, -0.6802563888389367985, -1.894789199515679146 ) ) ;
#160327 = CARTESIAN_POINT ( 'NONE',  ( 5.120175567455225618, 9.125288595339771547, -0.7998128361456281477 ) ) ;
#160328 = CARTESIAN_POINT ( 'NONE',  ( 3.926872384942071914, 1.999011803875171189, 0.6627620907858290389 ) ) ;
#160329 = CARTESIAN_POINT ( 'NONE',  ( 1.757307594529472272, 1.832486779838927937, -0.5580655975847663708 ) ) ;
#160330 = LINE ( 'NONE', #126850, #102113 ) ;
#160331 = CARTESIAN_POINT ( 'NONE',  ( 3.103910798422233608, 0.7114650421483189602, -1.836736179910645195 ) ) ;
#160332 = CARTESIAN_POINT ( 'NONE',  ( 5.308855472784884455, -0.4948685743355190070, -1.958072916474236314 ) ) ;
#160333 = CARTESIAN_POINT ( 'NONE',  ( 1.850267049257280139, 0.5840378008528935849, 1.777222254475477659 ) ) ;
#160336 = VERTEX_POINT ( 'NONE', #159073 ) ;
#160335 = CARTESIAN_POINT ( 'NONE',  ( 1.546972149855216472, 0.1906517044060058730, 1.902890584052991940 ) ) ;
#160334 = CARTESIAN_POINT ( 'NONE',  ( 5.232891500378062943, 0.1322050776780703540, 1.719872175869048947 ) ) ;
#160338 = CARTESIAN_POINT ( 'NONE',  ( 3.701012746850603996, 7.261672604726938651, 1.040834085586084257E-14 ) ) ;
#160337 = CARTESIAN_POINT ( 'NONE',  ( 1.049787907720298286, -1.741764784136769162, -1.355102641770723704 ) ) ;
#160339 = ADVANCED_FACE ( 'NONE', ( #176398 ), #76740, .T. ) ;
#160340 = CARTESIAN_POINT ( 'NONE',  ( -1.364683531250014514, 2.051041667008086655, -0.7879004041258289570 ) ) ;
#160341 = CARTESIAN_POINT ( 'NONE',  ( 9.250740883225924804, 9.686952540052077509, 1.040834085586084257E-14 ) ) ;
#160342 = CARTESIAN_POINT ( 'NONE',  ( 11.91826849282518630, 10.89999999999998082, 1.399999999999996581 ) ) ;
#160343 = SURFACE_STYLE_USAGE ( .BOTH. , #94302 ) ;
#160344 = CARTESIAN_POINT ( 'NONE',  ( 0.04629450404499204502, 2.597981984072172512, -2.080474185699523026 ) ) ;
#160345 = DIRECTION ( 'NONE',  ( 0.000000000000000000, 0.000000000000000000, -1.000000000000000000 ) ) ;
#160346 = ORIENTED_EDGE ( 'NONE', *, *, #55794, .F. ) ;
#160347 = CARTESIAN_POINT ( 'NONE',  ( 2.418496320782090869, 0.8830982243829659240, 1.872697815963566992 ) ) ;
#160348 = CARTESIAN_POINT ( 'NONE',  ( 1.499999999999989120, 1.775000000000019673, 0.000000000000000000 ) ) ;
#160349 = CARTESIAN_POINT ( 'NONE',  ( 5.341022448779654930, 8.318611059296550536, 1.199719254218462483 ) ) ;
#160350 = CARTESIAN_POINT ( 'NONE',  ( -6.093499974338126179, 9.196501505781426999, -1.199719254218440723 ) ) ;
#160351 = CARTESIAN_POINT ( 'NONE',  ( 3.054329744828568227, 6.785411478933790264, 0.000000000000000000 ) ) ;
#160352 = CARTESIAN_POINT ( 'NONE',  ( 6.111998723603361938, -0.7147493727725148238, 1.996541221815250733 ) ) ;
#160353 = CARTESIAN_POINT ( 'NONE',  ( 1.364683531249988535, 2.363541667008088432, 0.7879004041258500513 ) ) ;
#160354 = ORIENTED_EDGE ( 'NONE', *, *, #44751, .T. ) ;
#160356 = CARTESIAN_POINT ( 'NONE',  ( 4.207107738942202246, 3.802713871720993399, 1.214306433183764966E-14 ) ) ;
#160355 = CARTESIAN_POINT ( 'NONE',  ( -0.5000000000000056621, 3.172938907704293765, -0.4000000000000305533 ) ) ;
#160357 = CARTESIAN_POINT ( 'NONE',  ( 4.007185349139028574, 2.006139037694018690, 0.2004037502189442987 ) ) ;
#160358 = CARTESIAN_POINT ( 'NONE',  ( 4.399565145148922163, -1.877536364458038065, 0.3796658851462595408 ) ) ;
#160359 = SURFACE_STYLE_USAGE ( .BOTH. , #9832 ) ;
#160360 = CARTESIAN_POINT ( 'NONE',  ( 3.070069520051089906, -1.303570237086741024, 1.761582097007891923 ) ) ;
#160361 = CARTESIAN_POINT ( 'NONE',  ( 0.2335667940002476017, 0.2385907455819072931, -2.187945659632169804 ) ) ;
#160362 = CARTESIAN_POINT ( 'NONE',  ( -1.500000000000015099, 0.4104166673494891726, -0.8660254037844383745 ) ) ;
#160363 = CARTESIAN_POINT ( 'NONE',  ( 5.133069374350656133, 1.861756548879553996, 0.7665277172332859434 ) ) ;
#160364 = CARTESIAN_POINT ( 'NONE',  ( -6.073162743917628781, 9.172774736957510555, -1.199719254218440723 ) ) ;
#160366 = CARTESIAN_POINT ( 'NONE',  ( 6.310183273250552283, 1.218863855842572175, -1.731025912240143017 ) ) ;
#160365 = CARTESIAN_POINT ( 'NONE',  ( -3.850152436600983386, 4.554561266531622188, 1.082531754730560403 ) ) ;
#160367 = CARTESIAN_POINT ( 'NONE',  ( 0.6823417656249934904, 10.00520833367472839, 1.181850606188764807 ) ) ;
#160368 = B_SPLINE_CURVE_WITH_KNOTS ( 'NONE', 3,
 ( #160791, #133381, #184211, #167977, #51032, #197267, #144582, #49963 ),
 .UNSPECIFIED., .F., .F.,
 ( 4, 2, 2, 4 ),
 ( 6.599180864910166611E-16, 0.0002305131806121978120, 0.0004610263612237356702, 0.0009220527224468131212 ),
 .UNSPECIFIED. ) ;
#160370 = CARTESIAN_POINT ( 'NONE',  ( -7.632314129850253259, 7.869064337772231355, 0.7998128361456341429 ) ) ;
#160369 = CARTESIAN_POINT ( 'NONE',  ( 3.157844376090960026, 0.9421199074126384021, 1.866540799821286845 ) ) ;
#160372 = VERTEX_POINT ( 'NONE', #98337 ) ;
#160371 = CARTESIAN_POINT ( 'NONE',  ( 2.238867094643140376, -1.542287835237671212, 0.7722583484809567578 ) ) ;
#160373 = CARTESIAN_POINT ( 'NONE',  ( 5.097945154717048233, 1.425953928781589886, 1.569717048080176314 ) ) ;
#160374 = CARTESIAN_POINT ( 'NONE',  ( 6.471319392424407901, 6.444294134116939077, 0.7998128361456341429 ) ) ;
#160375 = CARTESIAN_POINT ( 'NONE',  ( 1.264911064067348656, 3.849999999999994316, 0.5000000000000064393 ) ) ;
#160376 = CARTESIAN_POINT ( 'NONE',  ( 7.565242077046510971, -6.863172033216027756, 7.985752187169479654 ) ) ;
#160377 = CARTESIAN_POINT ( 'NONE',  ( -7.487360338304412721, -6.465328379374280843, -7.487360338304378971 ) ) ;
#160378 = CARTESIAN_POINT ( 'NONE',  ( 7.332262146892202459, 7.448727347662698506, -0.7998128361456281477 ) ) ;
#160379 = ORIENTED_EDGE ( 'NONE', *, *, #23681, .T. ) ;
#160381 = CIRCLE ( 'NONE', #139678, 0.08000000000000001554 ) ;
#160380 = CARTESIAN_POINT ( 'NONE',  ( 0.5773502691896124084, -2.500000000000002220, -0.9999999999999991118 ) ) ;
#160382 = CARTESIAN_POINT ( 'NONE',  ( 1.172180985828397581, 0.7336035429467204771, 1.656470807091579900 ) ) ;
#160383 = CARTESIAN_POINT ( 'NONE',  ( -6.718228810771495141, 7.796687353110217877, 1.199719254218450271 ) ) ;
#160384 = ORIENTED_EDGE ( 'NONE', *, *, #178173, .F. ) ;
#160385 = CARTESIAN_POINT ( 'NONE',  ( 3.216308754939877446, 4.775446185561722956, -1.599625672291262513 ) ) ;
#160386 = ORIENTED_EDGE ( 'NONE', *, *, #138098, .T. ) ;
#160387 = CARTESIAN_POINT ( 'NONE',  ( 5.737035277238070385, 6.722237907313067140, -1.199719254218452047 ) ) ;
#160388 = CARTESIAN_POINT ( 'NONE',  ( 2.613665174717228368, -0.5667244042059360609, 1.720617414772870335 ) ) ;
#160389 = LINE ( 'NONE', #79128, #25383 ) ;
#160390 = CARTESIAN_POINT ( 'NONE',  ( 4.618273733618881494, 6.903169301580018846, 1.208453198238930382 ) ) ;
#160391 = CARTESIAN_POINT ( 'NONE',  ( 3.525696930263744200, 1.816150354290571034, -0.4055864600542318232 ) ) ;
#160392 = CARTESIAN_POINT ( 'NONE',  ( 1.634256478289298320, 0.6027960111968011514, 1.818337931642779903 ) ) ;
#160393 = CARTESIAN_POINT ( 'NONE',  ( 0.7447965706881398695, -1.568309060004613231, 0.9341869532639992535 ) ) ;
#160394 = DIRECTION ( 'NONE',  ( 0.000000000000000000, 0.000000000000000000, 1.000000000000000000 ) ) ;
#160395 = CARTESIAN_POINT ( 'NONE',  ( -0.2046361996433256059, 3.442961633857401171, 1.991136556534453206 ) ) ;
#160396 = VECTOR ( 'NONE', #195701, 1000.000000000000000 ) ;
#160397 = CARTESIAN_POINT ( 'NONE',  ( 5.370783296855561773, 7.572579728427998091, 1.242435897699250891 ) ) ;
#160398 =( NAMED_UNIT ( * ) SI_UNIT ( $, .STERADIAN. ) SOLID_ANGLE_UNIT ( ) );
#160399 = CARTESIAN_POINT ( 'NONE',  ( -3.090895834235680262, 5.589500325708124606, 1.082531754730560403 ) ) ;
#160400 = CARTESIAN_POINT ( 'NONE',  ( 6.805829924380097040, 10.88395931184472154, 0.7216878364870438212 ) ) ;
#160401 = CARTESIAN_POINT ( 'NONE',  ( 5.805506361076694155, -1.550124894993635261, -1.214668715896784379 ) ) ;
#160402 = CARTESIAN_POINT ( 'NONE',  ( -3.581325132304157943, 7.329963087663487364, -0.7998128361456281477 ) ) ;
#160403 = CARTESIAN_POINT ( 'NONE',  ( -11.89204169242383458, 9.799999999999998934, -0.8046421800350854747 ) ) ;
#160404 = CARTESIAN_POINT ( 'NONE',  ( 0.2696249905001372182, 1.205521239366886821, 1.707859383111657747 ) ) ;
#160405 = CARTESIAN_POINT ( 'NONE',  ( 6.662942426112080874, 9.860851032851066122, 1.199719254218460707 ) ) ;
#160406 = CARTESIAN_POINT ( 'NONE',  ( 4.875960570263176308, 1.108828003875685475, 1.575097709652195643 ) ) ;
#160407 = CARTESIAN_POINT ( 'NONE',  ( -6.338600509588822263, 7.353787668397130162, -1.199719254218446718 ) ) ;
#160408 = CARTESIAN_POINT ( 'NONE',  ( 1.623764174509664038, -1.011042645414115038, -1.519837739365454521 ) ) ;
#160409 = CARTESIAN_POINT ( 'NONE',  ( 2.508667999599442755, -0.8457060194008919618, -2.038605049697986615 ) ) ;
#160410 =( LENGTH_UNIT ( ) NAMED_UNIT ( * ) SI_UNIT ( .MILLI., .METRE. ) );
#160411 = CARTESIAN_POINT ( 'NONE',  ( 0.8538788329778913555, -0.7122206123622039087, 1.836445260119154543 ) ) ;
#160412 = CARTESIAN_POINT ( 'NONE',  ( 2.542442122522000414, -1.613304532933591995, 1.080848972723145618 ) ) ;
#160413 = ORIENTED_EDGE ( 'NONE', *, *, #165205, .T. ) ;
#160414 = CARTESIAN_POINT ( 'NONE',  ( 1.282577132041575529, -1.967586879516727061, 0.4389604359977539172 ) ) ;
#160416 = CARTESIAN_POINT ( 'NONE',  ( 5.067181549875774849, 1.617961714123143047, 0.9193176493522186021 ) ) ;
#160415 = CARTESIAN_POINT ( 'NONE',  ( -6.252245114557387851, 7.323316050852266557, -1.199719254218453823 ) ) ;
#160417 = CARTESIAN_POINT ( 'NONE',  ( 4.525389411911321602, 8.501647757197021704, -0.7998128361456381397 ) ) ;
#160418 = CARTESIAN_POINT ( 'NONE',  ( 8.500000000000000000, 6.200000000000038369, -2.900000000000000799 ) ) ;
#160419 = CARTESIAN_POINT ( 'NONE',  ( 9.049177462117294013, 12.64479190819049670, -1.199719254218446718 ) ) ;
#160420 = CARTESIAN_POINT ( 'NONE',  ( -4.446184310277715213, 7.274633231044262516, -1.199719254218452047 ) ) ;
#160421 = CARTESIAN_POINT ( 'NONE',  ( -6.261886844665283114, 8.398896966899865646, 1.599625672291269396 ) ) ;
#160422 = CARTESIAN_POINT ( 'NONE',  ( 1.716621854089026344, 2.046377219401524616, 0.7848826361863747714 ) ) ;
#160423 = CARTESIAN_POINT ( 'NONE',  ( 4.867013957625893283, 4.780530493426062399, 1.040834085586084257E-14 ) ) ;
#160424 = CARTESIAN_POINT ( 'NONE',  ( -10.59782195348455680, 12.30000000000000071, -3.302675849420335652 ) ) ;
#160425 = FACE_OUTER_BOUND ( 'NONE', #475, .T. ) ;
#160426 = CARTESIAN_POINT ( 'NONE',  ( 2.244514701088017539, 0.3993153960501935051, 1.781317584591130432 ) ) ;
#160427 = DIRECTION ( 'NONE',  ( 0.3281536732072464768, -0.000000000000000000, -0.9446243521954066358 ) ) ;
#160428 = CARTESIAN_POINT ( 'NONE',  ( -4.548924232584923288, 5.265832011892554121, -1.199719254218446718 ) ) ;
#160429 = CARTESIAN_POINT ( 'NONE',  ( -4.624683998644739447, 8.449116153850892985, -0.4091045222319161234 ) ) ;
#160430 = DIRECTION ( 'NONE',  ( 0.000000000000000000, 0.000000000000000000, 1.000000000000000000 ) ) ;
#160431 = CARTESIAN_POINT ( 'NONE',  ( 7.865701674222579598, 12.32840238656838139, -0.7998128361456352531 ) ) ;
#160432 = CARTESIAN_POINT ( 'NONE',  ( 1.418447215319606602, 1.294224929256732493, -1.427187236927564440 ) ) ;
#160433 = CARTESIAN_POINT ( 'NONE',  ( 5.928557400228100072, -1.247251702497784942, 1.514172074262534418 ) ) ;
#160434 = CARTESIAN_POINT ( 'NONE',  ( -5.716734326456539783, 9.821273814174633188, -0.7998128361456231517 ) ) ;
#160435 = CARTESIAN_POINT ( 'NONE',  ( 4.527533231959700366, 7.369540306339926516, 1.199719254218462483 ) ) ;
#160436 = CARTESIAN_POINT ( 'NONE',  ( 4.985950990042907094, -2.174969566330759996, -0.2684501861200879747 ) ) ;
#160437 = B_SPLINE_CURVE_WITH_KNOTS ( 'NONE', 3,
 ( #161967, #160890, #46089, #146799, #111135, #209606, #48229 ),
 .UNSPECIFIED., .F., .F.,
 ( 4, 3, 4 ),
 ( -2.180065393147345858E-06, 0.000000000000000000, 4.270488675890887276E-05 ),
 .UNSPECIFIED. ) ;
#160438 = AXIS2_PLACEMENT_3D ( 'NONE', #110951, #82638, #13376 ) ;
#160439 = CARTESIAN_POINT ( 'NONE',  ( -1.284279953904135407, 3.128360285806111474, -0.7749999999999892530 ) ) ;
#160440 = CARTESIAN_POINT ( 'NONE',  ( 3.801679563076823420, -1.564429233171928058, -1.355977067927462754 ) ) ;
#160441 = CARTESIAN_POINT ( 'NONE',  ( -0.6823417656250003738, 1.780208333674752952, -1.181850606188749264 ) ) ;
#160443 = VERTEX_POINT ( 'NONE', #30138 ) ;
#160442 = AXIS2_PLACEMENT_3D ( 'NONE', #153407, #119906, #52696 ) ;
#160444 = CARTESIAN_POINT ( 'NONE',  ( 3.938341551375645011, -1.911473949098478897, -1.276577049080502624 ) ) ;
#160446 = EDGE_LOOP ( 'NONE', ( #69305, #151321, #13033, #28395, #107869 ) ) ;
#160445 = CARTESIAN_POINT ( 'NONE',  ( 7.958272981541723468, 8.386999354661243800, 1.040834085586084257E-14 ) ) ;
#160448 = CARTESIAN_POINT ( 'NONE',  ( 3.285556943749998737, -0.6052083328553753416, -1.896917185911906500 ) ) ;
#160447 = CARTESIAN_POINT ( 'NONE',  ( 4.584065335196261692, 7.401807753487379848, 1.082531754730549078 ) ) ;
#160449 = CARTESIAN_POINT ( 'NONE',  ( -4.858757509019083543, 5.629766575900002401, -2.420000000000000373 ) ) ;
#160450 = CARTESIAN_POINT ( 'NONE',  ( -0.3000000000000155320, 3.999999999999955147, 1.007084189318345757 ) ) ;
#160451 = CARTESIAN_POINT ( 'NONE',  ( 3.521366475706534160, -1.157360712602263808, -1.559242563676524584 ) ) ;
#160452 = VERTEX_POINT ( 'NONE', #96226 ) ;
#160453 = CARTESIAN_POINT ( 'NONE',  ( -5.000000000000000888, 3.300000000000025135, -0.7749999999999935829 ) ) ;
#160454 = ORIENTED_EDGE ( 'NONE', *, *, #19832, .T. ) ;
#160455 = CARTESIAN_POINT ( 'NONE',  ( 5.203337695038355193, 1.683698669361912259, -0.9069238330124268499 ) ) ;
#160456 = CARTESIAN_POINT ( 'NONE',  ( 5.860297766850644408, 0.7031890092840873407, 1.575098903243739024 ) ) ;
#160457 = CARTESIAN_POINT ( 'NONE',  ( 4.557827498477605488, 1.164984774316142113, 1.645760986912048862 ) ) ;
#160458 = CARTESIAN_POINT ( 'NONE',  ( 3.538314903486612817, 7.071858454135611538, 1.040834085586084257E-14 ) ) ;
#160459 = CARTESIAN_POINT ( 'NONE',  ( 2.192262590105994668, -0.9421081357594159877, 1.995820444975453745 ) ) ;
#160461 = CARTESIAN_POINT ( 'NONE',  ( -4.990809943606294929, 4.995235487061662205, -0.7216878364870338292 ) ) ;
#160460 = CARTESIAN_POINT ( 'NONE',  ( -3.970504344535652486, 7.404204864921184459, -0.6292205879280321490 ) ) ;
#160463 = CARTESIAN_POINT ( 'NONE',  ( 0.4261447845913856614, 1.691672268694037307, 0.5201907349937917591 ) ) ;
#160462 = CARTESIAN_POINT ( 'NONE',  ( 1.781308773403101231, 1.442672104170627190, 1.513329462076596243 ) ) ;
#160464 = CARTESIAN_POINT ( 'NONE',  ( 5.467422714486909641, -1.967887220244109558, -0.4390321945699494632 ) ) ;
#160465 = EDGE_CURVE ( 'NONE', #123984, #57442, #31116, .T. ) ;
#160467 = CARTESIAN_POINT ( 'NONE',  ( 2.906493132324819761, 1.659771084382713369, -1.581246672503307638 ) ) ;
#160466 = CARTESIAN_POINT ( 'NONE',  ( 5.143339171537801846, 7.093924681584509173, 1.599625672291269396 ) ) ;
#160468 = CARTESIAN_POINT ( 'NONE',  ( 1.587455592251562297, -1.731706956562387711, -0.1728515053983879501 ) ) ;
#160469 = CARTESIAN_POINT ( 'NONE',  ( 2.971057270251746818, -1.603071526910588629, 1.388259434452358665 ) ) ;
#160470 = CARTESIAN_POINT ( 'NONE',  ( 0.000000000000000000, 0.000000000000000000, 0.000000000000000000 ) ) ;
#160471 = CARTESIAN_POINT ( 'NONE',  ( 1.036033436886945047, 1.672847207165208072, -0.4555716438836182602 ) ) ;
#160472 = CARTESIAN_POINT ( 'NONE',  ( 0.6801582343749952297, 1.088541667008086078, -1.178068619123883165 ) ) ;
#160473 = DIRECTION ( 'NONE',  ( 1.224646799147353207E-16, 0.000000000000000000, -1.000000000000000000 ) ) ;
#160474 = CARTESIAN_POINT ( 'NONE',  ( 1.856167715545921748, -0.7324389044234179691, 2.044012385327702575 ) ) ;
#160475 = CARTESIAN_POINT ( 'NONE',  ( 3.344935638061694139, -1.780668040901035143, -0.9463001528628791625 ) ) ;
#160476 = CARTESIAN_POINT ( 'NONE',  ( 3.750000000000002665, 2.137871159508210026E-13, 2.052068128417945836 ) ) ;
#160477 = CARTESIAN_POINT ( 'NONE',  ( -1.500000000000001332, 1.431250000682816825, 0.000000000000000000 ) ) ;
#160478 = CARTESIAN_POINT ( 'NONE',  ( 0.1121488755844394364, -0.8197171475488943537, -1.741376145853351431 ) ) ;
#160479 = CARTESIAN_POINT ( 'NONE',  ( 0.6823417656249969321, 12.77604166700806232, -1.181850606188757036 ) ) ;
#160480 = CARTESIAN_POINT ( 'NONE',  ( 3.674281580191523400, 2.204306621758029383, -0.2748671541705596799 ) ) ;
#160481 = ORIENTED_EDGE ( 'NONE', *, *, #121920, .T. ) ;
#160482 = CARTESIAN_POINT ( 'NONE',  ( 6.506163559800162588, -8.203199116536543656, 6.922777049148927553 ) ) ;
#160483 = CARTESIAN_POINT ( 'NONE',  ( -1.500000000000015099, -0.8708333333333129200, -0.8660254037844383745 ) ) ;
#160484 = CARTESIAN_POINT ( 'NONE',  ( 8.426556166093362776, 9.789735934319136135, -1.199719254218446718 ) ) ;
#160485 =( LENGTH_UNIT ( ) NAMED_UNIT ( * ) SI_UNIT ( .MILLI., .METRE. ) );
#160486 = CARTESIAN_POINT ( 'NONE',  ( 5.284588373313929388, 1.531378566088846371, -0.8270805780791794515 ) ) ;
#160487 = CARTESIAN_POINT ( 'NONE',  ( 5.019951445752288244, 1.940773837913706057, -0.2859759768028962146 ) ) ;
#160489 = CARTESIAN_POINT ( 'NONE',  ( -5.260200412422200600, 8.120355666925794580, -1.082531754730544860 ) ) ;
#160488 = CARTESIAN_POINT ( 'NONE',  ( 4.532503425670185493, 4.182342172903648070, 1.214306433183764966E-14 ) ) ;
#160490 = CARTESIAN_POINT ( 'NONE',  ( 0.000000000000000000, 12.30000000000000071, 0.000000000000000000 ) ) ;
#160491 = CARTESIAN_POINT ( 'NONE',  ( 5.184992917819648994, -0.2698046931138863846, -2.246192962944548732 ) ) ;
#160492 = CARTESIAN_POINT ( 'NONE',  ( 1.943872066224684669, 1.420748078972498440, 1.495595626624636409 ) ) ;
#160493 = CARTESIAN_POINT ( 'NONE',  ( -6.531277313481209212, 8.642909503859968368, 1.599625672291283607 ) ) ;
#160495 = EDGE_CURVE ( 'NONE', #12101, #110280, #22812, .T. ) ;
#160494 =( BOUNDED_CURVE ( )  B_SPLINE_CURVE ( 3, ( #154602, #106970, #44061, #125374 ),
 .UNSPECIFIED., .F., .T. ) 
 B_SPLINE_CURVE_WITH_KNOTS ( ( 4, 4 ),
 ( 0.5000000000000003331, 1.000000000000000000 ),
 .UNSPECIFIED. ) 
 CURVE ( )  GEOMETRIC_REPRESENTATION_ITEM ( )  RATIONAL_B_SPLINE_CURVE ( ( 0.9999999999999997780, 0.3333333333333334259, 0.3333333333333338699, 1.000000000000000222 ) ) 
 REPRESENTATION_ITEM ( '' )  );
#160496 = ORIENTED_EDGE ( 'NONE', *, *, #64003, .F. ) ;
#160497 = CARTESIAN_POINT ( 'NONE',  ( -1.500000000000015099, 0.9104166673494835660, -0.8660254037844313801 ) ) ;
#160498 = CARTESIAN_POINT ( 'NONE',  ( 3.883945074633635031, -0.9243716352356041721, 1.626130415258054018 ) ) ;
#160499 = CARTESIAN_POINT ( 'NONE',  ( 2.707300540323886562, 1.633622375412818073, 0.5822755513817943207 ) ) ;
#160500 = CARTESIAN_POINT ( 'NONE',  ( 0.1699995558098127968, 1.326729642492694872, 1.869266897796989291 ) ) ;
#160501 = CARTESIAN_POINT ( 'NONE',  ( 0.7278961316968115547, -2.094849050945537972, 0.6941159686642893734 ) ) ;
#160502 = CARTESIAN_POINT ( 'NONE',  ( 3.502937704049163159, 1.705309618848281472, -1.328393843302433153 ) ) ;
#160503 = CARTESIAN_POINT ( 'NONE',  ( 4.716706857919571227, -0.09384406936703558466, 1.939798966779549882 ) ) ;
#160505 = UNCERTAINTY_MEASURE_WITH_UNIT (LENGTH_MEASURE( 1.000000000000000082E-05 ), #102376, 'distance_accuracy_value', 'NONE');
#160504 = CARTESIAN_POINT ( 'NONE',  ( -9.499700864329909678, -7.154544010627095219, -0.07538891330675229208 ) ) ;
#160506 =( NAMED_UNIT ( * ) SI_UNIT ( $, .STERADIAN. ) SOLID_ANGLE_UNIT ( ) );
#160507 = CARTESIAN_POINT ( 'NONE',  ( -0.3978093821461001767, 3.011896635411785983, 0.3978093821460482182 ) ) ;
#160508 =( NAMED_UNIT ( * ) PLANE_ANGLE_UNIT ( ) SI_UNIT ( $, .RADIAN. ) );
#160509 = CARTESIAN_POINT ( 'NONE',  ( -5.608478439449225306, 5.609308656285654671, -0.4224404339892348093 ) ) ;
#160510 = CARTESIAN_POINT ( 'NONE',  ( 5.959611329766300258, -1.915599147091971544, -0.6298778581111733610 ) ) ;
#160511 = CARTESIAN_POINT ( 'NONE',  ( -8.805130697071332335, 12.36007068230351358, 1.199719254218462483 ) ) ;
#160512 = CARTESIAN_POINT ( 'NONE',  ( 7.741869408603235136, 8.990934717247309749, 1.199719254218462483 ) ) ;
#160513 = CARTESIAN_POINT ( 'NONE',  ( 2.632325991586431435, -0.3920720250259056017, -0.1636427795756393855 ) ) ;
#160514 = CARTESIAN_POINT ( 'NONE',  ( 2.912524513316586461, 1.322148455168963510, -1.259233298254287536 ) ) ;
#160515 = CARTESIAN_POINT ( 'NONE',  ( 2.221956617217385244, -2.140583525707707935, 0.5359638216213060691 ) ) ;
#160516 = EDGE_LOOP ( 'NONE', ( #144136, #177971, #5810, #127175 ) ) ;
#160517 = CARTESIAN_POINT ( 'NONE',  ( -5.614485009390564940, 5.722856397143323726, 0.000000000000000000 ) ) ;
#160518 = CARTESIAN_POINT ( 'NONE',  ( 3.285556943750000070, -2.471874999522040373, 0.000000000000000000 ) ) ;
#160519 = CARTESIAN_POINT ( 'NONE',  ( -6.482770005628665011, 10.71498210654212002, 0.7998128361456481317 ) ) ;
#160520 = CARTESIAN_POINT ( 'NONE',  ( 0.5979230068290807276, 1.359733756741304811, 1.493685216911154967 ) ) ;
#160521 = CARTESIAN_POINT ( 'NONE',  ( 1.436355765274465623, -1.180822252328097344, -1.761085815303937929 ) ) ;
#160522 = CARTESIAN_POINT ( 'NONE',  ( 6.238160076063574699, 6.450477308261794107, -0.7216878364870207285 ) ) ;
#160523 = CARTESIAN_POINT ( 'NONE',  ( -6.784929528996132220, 6.880448970109080520, 0.000000000000000000 ) ) ;
#160524 = CARTESIAN_POINT ( 'NONE',  ( 1.779899486625190264, -1.028416011161866983, -1.550745576289275895 ) ) ;
#160525 = CARTESIAN_POINT ( 'NONE',  ( 5.366329872910639232, 5.155139694684188534, 1.040834085586084257E-14 ) ) ;
#160526 = CARTESIAN_POINT ( 'NONE',  ( 0.2687375195599971400, -1.410744835756465365, 1.637978619736128127 ) ) ;
#160527 = CARTESIAN_POINT ( 'NONE',  ( 6.610000000000006537, 0.002781820520842553934, 2.000159646111852929 ) ) ;
#160528 = VERTEX_POINT ( 'NONE', #213128 ) ;
#160529 = ORIENTED_EDGE ( 'NONE', *, *, #91370, .T. ) ;
#160530 = CARTESIAN_POINT ( 'NONE',  ( -9.053093885623068715, 11.58502883802551153, -1.599625672291263179 ) ) ;
#160531 = CARTESIAN_POINT ( 'NONE',  ( 3.527797039230845311, -1.088449851438414218, -1.465592618984489670 ) ) ;
#160533 = CARTESIAN_POINT ( 'NONE',  ( -5.057943438340505082, 6.748278329294532085, -1.445135742742007068 ) ) ;
#160532 = CARTESIAN_POINT ( 'NONE',  ( -5.113360211009450040, 5.994616996712990975, -1.199719254218453823 ) ) ;
#160534 = CARTESIAN_POINT ( 'NONE',  ( 5.753927575595171540, 7.371122731025397279, 1.306365966420112601 ) ) ;
#160535 = CARTESIAN_POINT ( 'NONE',  ( 6.415388720371407949, 0.6297814698452592896, 1.915305867393565897 ) ) ;
#160536 = CARTESIAN_POINT ( 'NONE',  ( 5.894452933195245770, 1.502573388107550034, -1.063714819228026132 ) ) ;
#160537 = CARTESIAN_POINT ( 'NONE',  ( 0.07700591528353968596, 0.003617085621422307627, -1.910863332519038282 ) ) ;
#160538 = CARTESIAN_POINT ( 'NONE',  ( 4.108297157686680912, -2.301651690510425841, 0.1678553853470560464 ) ) ;
#160539 = CARTESIAN_POINT ( 'NONE',  ( 4.355912491740495440, 8.303924683664389406, 0.000000000000000000 ) ) ;
#160540 = CARTESIAN_POINT ( 'NONE',  ( 6.116527240895272222, 1.456737685447502262, -1.597155580871166602 ) ) ;
#160541 = CARTESIAN_POINT ( 'NONE',  ( 5.795220594837462436, 8.848508896363995291, -1.199719254218440723 ) ) ;
#160542 = CARTESIAN_POINT ( 'NONE',  ( 1.733828471206948496, 1.921180395534723528, 0.2831599317468564969 ) ) ;
#160543 = VERTEX_POINT ( 'NONE', #180645 ) ;
#160544 = CARTESIAN_POINT ( 'NONE',  ( 5.132278277959533064, 0.2326997901972542582, -2.286600633956968220 ) ) ;
#160545 = FACE_OUTER_BOUND ( 'NONE', #15855, .T. ) ;
#160546 = CARTESIAN_POINT ( 'NONE',  ( -5.029148636026397945, 4.832037928311032182, 0.7998128361456281477 ) ) ;
#160547 = CARTESIAN_POINT ( 'NONE',  ( 4.170664822833985319, -1.745344833062393075, -0.6735866001992969476 ) ) ;
#160548 = ORIENTED_EDGE ( 'NONE', *, *, #207277, .T. ) ;
#160551 = CARTESIAN_POINT ( 'NONE',  ( -3.935609729716867289, 7.813571461303467913, 0.7998128361456352531 ) ) ;
#160550 = CARTESIAN_POINT ( 'NONE',  ( 1.499999999999987121, 0.2854166673494805684, 0.8660254037844524744 ) ) ;
#160549 = CARTESIAN_POINT ( 'NONE',  ( 2.742330423940505302, 1.058908597569432120, -1.592262909973440888 ) ) ;
#160552 = CARTESIAN_POINT ( 'NONE',  ( 4.125739685719872263, -2.112183141943014153, 0.6395159525410462065 ) ) ;
#160553 = CARTESIAN_POINT ( 'NONE',  ( -4.083708824282378913, 7.596498746673441715, 0.5977277219625460880 ) ) ;
#160554 = CARTESIAN_POINT ( 'NONE',  ( 2.218730694130720771, 5.740269576461138890, 0.7998128361456462443 ) ) ;
#160555 = CARTESIAN_POINT ( 'NONE',  ( 5.519577934094851202, 8.493239118869080784, 1.082531754730547524 ) ) ;
#160556 = CARTESIAN_POINT ( 'NONE',  ( -6.577113915960841162, 7.806292669110006521, -1.082531754730549967 ) ) ;
#160557 = CARTESIAN_POINT ( 'NONE',  ( 1.563680990848853591, 1.942865793614118930, -0.3330471066002506642 ) ) ;
#160558 = CARTESIAN_POINT ( 'NONE',  ( 1.167484012262551607, -2.087313454887162578, -0.9842159052040798661 ) ) ;
#160559 = CARTESIAN_POINT ( 'NONE',  ( 2.594135478747404022, 0.9273930874063830432, -1.728848471177657942 ) ) ;
#160560 = CARTESIAN_POINT ( 'NONE',  ( -4.423703259808839938, 8.383013913077439483, 0.7998128361456350310 ) ) ;
#160561 = CARTESIAN_POINT ( 'NONE',  ( 5.541865367331380909, 1.381078337155069224, 1.532129260548445782 ) ) ;
#160562 = CARTESIAN_POINT ( 'NONE',  ( 4.528060117284229413, 7.266191989264828344, 1.082531754730558626 ) ) ;
#160563 = CARTESIAN_POINT ( 'NONE',  ( 6.554440917563797875, 6.611545590104705994, -0.7998128361456481317 ) ) ;
#160564 = ORIENTED_EDGE ( 'NONE', *, *, #144073, .T. ) ;
#160565 = CARTESIAN_POINT ( 'NONE',  ( -10.64723070543352712, 11.31619066596094392, 0.7998128361456462443 ) ) ;
#160566 = CARTESIAN_POINT ( 'NONE',  ( 6.758184431511291557, -6.900108348305955985, 6.825879202496260234 ) ) ;
#160567 = CARTESIAN_POINT ( 'NONE',  ( 10.01963921569910632, 11.64833282552586091, 1.199719254218450271 ) ) ;
#160568 = CARTESIAN_POINT ( 'NONE',  ( 2.553800759094803308, 1.675875371511101886, 1.380159786156359258 ) ) ;
#160569 = CARTESIAN_POINT ( 'NONE',  ( 6.215487077222150880, 6.216099443039444949, 0.000000000000000000 ) ) ;
#160570 = CYLINDRICAL_SURFACE ( 'NONE', #168852, 1.224999999999996980 ) ;
#160571 = LINE ( 'NONE', #129240, #139589 ) ;
#160572 = CARTESIAN_POINT ( 'NONE',  ( 2.407302635362520427, -0.4140892318466664612, 1.823965488845371574 ) ) ;
#160573 = CARTESIAN_POINT ( 'NONE',  ( 6.520800673124607982, 2.014292100380775885, 0.7847517145297827623 ) ) ;
#160575 = CARTESIAN_POINT ( 'NONE',  ( -8.002408263930261612, -6.836568542494980250, 7.346809171966449448 ) ) ;
#160574 = CARTESIAN_POINT ( 'NONE',  ( 7.720982897393566802, -5.907420853759296264, -7.834948825496929281 ) ) ;
#160576 = CARTESIAN_POINT ( 'NONE',  ( 1.364683531249986537, -0.3864583329919166199, 0.7879004041258500513 ) ) ;
#160577 =( NAMED_UNIT ( * ) PLANE_ANGLE_UNIT ( ) SI_UNIT ( $, .RADIAN. ) );
#160578 = CARTESIAN_POINT ( 'NONE',  ( 2.736851483355093873, 1.801321139115559244, 0.6423184003811268639 ) ) ;
#160579 =( BOUNDED_CURVE ( )  B_SPLINE_CURVE ( 2, ( #137484, #42121, #56216, #122380, #9589 ),
 .UNSPECIFIED., .F., .T. ) 
 B_SPLINE_CURVE_WITH_KNOTS ( ( 3, 2, 3 ),
 ( 0.2499999999999997502, 0.2541666666666666519, 0.2544499682697047849 ),
 .UNSPECIFIED. ) 
 CURVE ( )  GEOMETRIC_REPRESENTATION_ITEM ( )  RATIONAL_B_SPLINE_CURVE ( ( 1.000000000000007994, 0.8660254037844307140, 1.000000000000000000, 0.9908907477101788208, 0.9830202149929265776 ) ) 
 REPRESENTATION_ITEM ( '' )  );
#160580 = CARTESIAN_POINT ( 'NONE',  ( 4.100303288188038131, -0.5556836211836749806, -1.680424235071773742 ) ) ;
#160581 = CARTESIAN_POINT ( 'NONE',  ( 1.646971982979035909, 0.1886418863925183320, 1.902964618272011021 ) ) ;
#160582 = CARTESIAN_POINT ( 'NONE',  ( -6.064574784014443942, 5.969758757638621738, -0.7998128361456291469 ) ) ;
#160584 = CARTESIAN_POINT ( 'NONE',  ( -0.1884536309573183466, -1.180508991428173671, -1.509157985239983679 ) ) ;
#160583 = CARTESIAN_POINT ( 'NONE',  ( 0.000000000000000000, -1.500000000000001332, 0.000000000000000000 ) ) ;
#160585 = CARTESIAN_POINT ( 'NONE',  ( -1.500000000000013101, 0.1708333333333560411, 0.8660254037844403729 ) ) ;
#160586 = CARTESIAN_POINT ( 'NONE',  ( 0.3794556558127279988, -0.1030994254981997954, 2.067933115924729837 ) ) ;
#160587 = CARTESIAN_POINT ( 'NONE',  ( 0.7499999999999902300, 5.316666666666685082, -1.299038105676658228 ) ) ;
#160588 = LINE ( 'NONE', #94550, #189714 ) ;
#160589 = CARTESIAN_POINT ( 'NONE',  ( 5.383624799460786647, 1.257121276536907750, 1.385457850027263182 ) ) ;
#160590 = CARTESIAN_POINT ( 'NONE',  ( 2.262075381241589245, 0.7800679334904643270, 1.650788133108482825 ) ) ;
#160592 = CARTESIAN_POINT ( 'NONE',  ( 4.684024595049480766, 8.263433789595206136, 0.5754648794667740486 ) ) ;
#160591 = CARTESIAN_POINT ( 'NONE',  ( 4.899154391205060577, 1.836108854712194649, -1.224054507610386366 ) ) ;
#160593 = ADVANCED_FACE ( 'NONE', ( #13863 ), #65790, .T. ) ;
#160594 = CARTESIAN_POINT ( 'NONE',  ( 0.6823417656249882723, -0.6572916663252492686, 1.181850606188755259 ) ) ;
#160595 = CARTESIAN_POINT ( 'NONE',  ( 2.893094712532847890, 0.2500570216604477980, 2.047387263510790145 ) ) ;
#160597 = CARTESIAN_POINT ( 'NONE',  ( -7.828943636887387925, 11.22118577875556156, 1.199719254218453823 ) ) ;
#160596 = AXIS2_PLACEMENT_3D ( 'NONE', #31298, #208945, #178616 ) ;
#160598 = CARTESIAN_POINT ( 'NONE',  ( 1.387358672533417936, 7.315968950353815892, 4.254625267138360201 ) ) ;
#160599 = CARTESIAN_POINT ( 'NONE',  ( 9.134442807305049428, 11.67993591332117376, 1.599625672291281386 ) ) ;
#160600 = CARTESIAN_POINT ( 'NONE',  ( 1.369796495953883753, 3.411350084130203797, 0.2487645435796728144 ) ) ;
#160601 = DIRECTION ( 'NONE',  ( 0.000000000000000000, 0.000000000000000000, 1.000000000000000000 ) ) ;
#160602 = CARTESIAN_POINT ( 'NONE',  ( 6.505933609711257226, 8.683618192786854095, -1.599625672291281386 ) ) ;
#160603 = VERTEX_POINT ( 'NONE', #147104 ) ;
#160604 = CARTESIAN_POINT ( 'NONE',  ( 5.652806998763869828, -0.4994405740583847675, -2.009109930559597856 ) ) ;
#160606 = CARTESIAN_POINT ( 'NONE',  ( 0.6823417656249882723, 0.2385416670080825474, -1.181850606188749264 ) ) ;
#160605 = CIRCLE ( 'NONE', #94908, 11.49999999999998934 ) ;
#160607 = CARTESIAN_POINT ( 'NONE',  ( 3.145949958485740883, 0.7812230816454240889, -2.015650884352723882 ) ) ;
#160608 = CARTESIAN_POINT ( 'NONE',  ( -4.626128544448885549, 8.355821839108529048, -0.2988314032242797569 ) ) ;
#160609 = CARTESIAN_POINT ( 'NONE',  ( 3.211586479193883292, 1.593432852337670624, 1.240894322269629813 ) ) ;
#160610 = CARTESIAN_POINT ( 'NONE',  ( -3.701970883082888353, 7.364863713882347618, 2.499999999999998668 ) ) ;
#160611 = ADVANCED_FACE ( 'NONE', ( #79942 ), #179592, .F. ) ;
#160614 = CARTESIAN_POINT ( 'NONE',  ( 8.107412671292047790, 8.560995659369956101, 0.7216878364870458196 ) ) ;
#160613 = CARTESIAN_POINT ( 'NONE',  ( 3.475000000000000533, -1.195833333333332194, -2.006292185433951047 ) ) ;
#160612 = SURFACE_STYLE_USAGE ( .BOTH. , #27403 ) ;
#160615 = CARTESIAN_POINT ( 'NONE',  ( -2.984203208339354152, 6.495671153122273722, 0.000000000000000000 ) ) ;
#160616 = CARTESIAN_POINT ( 'NONE',  ( 1.094935803221647186, 1.780670018850015079, 0.9462964651613046119 ) ) ;
#160617 = CARTESIAN_POINT ( 'NONE',  ( 5.741772062182810998, 2.188963553168365994, 0.1087695542012837302 ) ) ;
#160618 = CARTESIAN_POINT ( 'NONE',  ( -1.201851678989727383E-14, 4.368750000682820378, -1.732050807568863648 ) ) ;
#160619 = CARTESIAN_POINT ( 'NONE',  ( 4.992401499097729456, -1.057410677138232780, 1.593263788312593743 ) ) ;
#160620 = CARTESIAN_POINT ( 'NONE',  ( -5.088387723830502196, 4.830873854090670605, -0.7998128361456221525 ) ) ;
#160621 = CARTESIAN_POINT ( 'NONE',  ( 6.765155463094759014, 7.955398130774449683, 1.082531754730558626 ) ) ;
#160623 = CARTESIAN_POINT ( 'NONE',  ( 3.497672881252233967, -1.986097994744703721, 0.3474890017408845955 ) ) ;
#160622 = CARTESIAN_POINT ( 'NONE',  ( -9.666600336419303829, 11.34041714965307968, 1.082531754730558626 ) ) ;
#160624 = CARTESIAN_POINT ( 'NONE',  ( -1.364683531250014514, 13.90104166700806765, -0.7879004041258335089 ) ) ;
#160625 = CARTESIAN_POINT ( 'NONE',  ( -3.169574050544739841, 6.919863168935977527, -0.7998128361456481317 ) ) ;
#160626 = CARTESIAN_POINT ( 'NONE',  ( 5.157137038817142916, -1.458691705945897032, -0.9200343150467110709 ) ) ;
#160627 = CARTESIAN_POINT ( 'NONE',  ( 6.658989722967328717, 7.797851427330578566, 1.199719254218452935 ) ) ;
#160628 = CARTESIAN_POINT ( 'NONE',  ( 9.490344339885973923, 12.09515436799890331, -1.443375672974057666 ) ) ;
#160629 = DIRECTION ( 'NONE',  ( 0.000000000000000000, 0.000000000000000000, 1.000000000000000000 ) ) ;
#160630 = CYLINDRICAL_SURFACE ( 'NONE', #133826, 1.250000000000000000 ) ;
#160631 = CARTESIAN_POINT ( 'NONE',  ( 0.6200890622066607127, 2.048230590617374336, -0.3001980380039070972 ) ) ;
#160632 = CARTESIAN_POINT ( 'NONE',  ( 6.865700769154306826, -0.4580177224273937475, 2.026514595051785772 ) ) ;
#160633 = ORIENTED_EDGE ( 'NONE', *, *, #150631, .T. ) ;
#160634 = CARTESIAN_POINT ( 'NONE',  ( 5.813115421323210796, 1.476946679544950847, -1.048544953227096288 ) ) ;
#160635 = CARTESIAN_POINT ( 'NONE',  ( 6.527324610336440180, 6.579909898339485252, 0.7998128361456331437 ) ) ;
#160637 = EDGE_CURVE ( 'NONE', #119366, #12329, #169462, .T. ) ;
#160636 = CARTESIAN_POINT ( 'NONE',  ( 1.500000000000053291, 7.750000000000000000, 15.74999999999999289 ) ) ;
#160638 = CARTESIAN_POINT ( 'NONE',  ( 6.217428747564047065, 1.510149904227086504, 1.000116013982331076 ) ) ;
#160639 = CARTESIAN_POINT ( 'NONE',  ( 5.031484404002878996, 7.923796667095108326, 1.082531754730548412 ) ) ;
#160640 = CARTESIAN_POINT ( 'NONE',  ( 10.87278331243690133, 9.634830980282087509, 5.090122543959602730 ) ) ;
#160641 = CARTESIAN_POINT ( 'NONE',  ( 3.486445073788289051, -0.4274320362823453290, -2.149191018322317515 ) ) ;
#160642 = VERTEX_POINT ( 'NONE', #148163 ) ;
#160644 = CARTESIAN_POINT ( 'NONE',  ( 9.413438726589914651, 9.876766690643398405, 0.000000000000000000 ) ) ;
#160643 = CARTESIAN_POINT ( 'NONE',  ( 0.4144086874100678664, 0.7473079093508437909, 1.814158889769983185 ) ) ;
#160645 = CARTESIAN_POINT ( 'NONE',  ( 5.483970141128155618, -1.915793143390194242, 0.004843307671191510178 ) ) ;
#160646 = DIRECTION ( 'NONE',  ( 0.000000000000000000, 0.000000000000000000, -1.000000000000000000 ) ) ;
#160647 = CARTESIAN_POINT ( 'NONE',  ( -6.220586654761008027, 6.942393398233093649, 0.8502372543972673835 ) ) ;
#160648 = AXIS2_PLACEMENT_3D ( 'NONE', #201534, #98743, #67265 ) ;
#160649 = EDGE_CURVE ( 'NONE', #12172, #10803, #199000, .T. ) ;
#160650 = CYLINDRICAL_SURFACE ( 'NONE', #101834, 0.3999999999999996891 ) ;
#160651 = CARTESIAN_POINT ( 'NONE',  ( -1.402160292154681736E-14, 0.4468750003414233563, -1.575800808251665908 ) ) ;
#160653 = ORIENTED_EDGE ( 'NONE', *, *, #103129, .T. ) ;
#160652 = CARTESIAN_POINT ( 'NONE',  ( 4.528060117284229413, 7.266191989264828344, 1.082531754730558626 ) ) ;
#160654 = CARTESIAN_POINT ( 'NONE',  ( -8.188761592974040937, 11.53701037756964887, -1.082531754730543971 ) ) ;
#160655 = CARTESIAN_POINT ( 'NONE',  ( 2.008865009297224447, 1.601992838228694316, -1.451600824242594845 ) ) ;
#160656 = ADVANCED_FACE ( 'NONE', ( #146046 ), #54480, .F. ) ;
#160657 = CARTESIAN_POINT ( 'NONE',  ( -3.526002468005825286, 6.271364091718859335, -1.199719254218450271 ) ) ;
#160658 = COLOUR_RGB ( '', 0.08235294, 0.09019608, 0.10196078) ;
#160659 = CARTESIAN_POINT ( 'NONE',  ( 5.872089928494542477, 9.864872326636710653, 0.000000000000000000 ) ) ;
#160660 = CARTESIAN_POINT ( 'NONE',  ( 2.362075219488588562, 0.7782009281872975803, 1.651537983114875763 ) ) ;
#160661 = CARTESIAN_POINT ( 'NONE',  ( -2.819205876637805641, 5.376491725131008259, -1.199719254218446718 ) ) ;
#160662 = CARTESIAN_POINT ( 'NONE',  ( 5.051681782491273864, 0.5714109786712183725, -1.733901259708306331 ) ) ;
#160663 = CARTESIAN_POINT ( 'NONE',  ( 13.00188123086410563, 6.790293321084564404, 2.180131930379270333 ) ) ;
#160664 = CARTESIAN_POINT ( 'NONE',  ( 3.058751851047710080, 0.4689117840017149041, 1.853869267190631831 ) ) ;
#160665 = ORIENTED_EDGE ( 'NONE', *, *, #124222, .T. ) ;
#160666 = CARTESIAN_POINT ( 'NONE',  ( 3.965261034597372891, 1.688065314258681893, 1.014448032605998584 ) ) ;
#160667 = ORIENTED_EDGE ( 'NONE', *, *, #132306, .F. ) ;
#160668 = CARTESIAN_POINT ( 'NONE',  ( 6.409718653046240000, -0.9196952807892575521, -1.710506293091022201 ) ) ;
#160669 = EDGE_LOOP ( 'NONE', ( #199102, #183274, #56915, #22505 ) ) ;
#160670 = CARTESIAN_POINT ( 'NONE',  ( -4.776215253764153346, 8.794277906025310898, -0.7998128361456362523 ) ) ;
#160672 = CARTESIAN_POINT ( 'NONE',  ( 5.976833544478475702, -1.498421880457675215, 1.500811427713820478 ) ) ;
#160671 = CARTESIAN_POINT ( 'NONE',  ( -3.461074353238556167, 7.259946855412102273, 0.000000000000000000 ) ) ;
#160673 = CARTESIAN_POINT ( 'NONE',  ( 5.980555156959511898, 9.991415093179179863, -0.7216878364870458196 ) ) ;
#160674 = CARTESIAN_POINT ( 'NONE',  ( 3.563058999304801411, -1.561743426874351970, 1.103242700682869781 ) ) ;
#160675 = CARTESIAN_POINT ( 'NONE',  ( 4.470816497852414528, 7.277750640693428252, -1.251308411505752671 ) ) ;
#160676 = CARTESIAN_POINT ( 'NONE',  ( -9.597801448743025432, -7.025535116234744137, 0.01424860406304543671 ) ) ;
#160677 = CARTESIAN_POINT ( 'NONE',  ( 3.902768115887398803, 5.646591783325653147, -1.599625672291269396 ) ) ;
#160678 = PRODUCT_DEFINITION ( 'UNKNOWN', '', #118085, #72461 ) ;
#160679 = CARTESIAN_POINT ( 'NONE',  ( 4.881498389339896882, 0.1952109149471596417, -2.003590356478464507 ) ) ;
#160680 = PLANE ( 'NONE',  #23872 ) ;
#160681 = CARTESIAN_POINT ( 'NONE',  ( 5.602125774977974260, -1.825872481414937853, 0.004271240736861136277 ) ) ;
#160682 = CARTESIAN_POINT ( 'NONE',  ( 0.9595327444568906294, 1.691550050060253829, 1.193477315110213599 ) ) ;
#160683 = CARTESIAN_POINT ( 'NONE',  ( -6.534666852106790103, 10.56760239419251590, 0.7216878364870458196 ) ) ;
#160684 = CARTESIAN_POINT ( 'NONE',  ( -6.419388467533182485, 6.810688026658763938, -0.4840902626340077841 ) ) ;
#160685 = FACE_OUTER_BOUND ( 'NONE', #25321, .T. ) ;
#160686 = CARTESIAN_POINT ( 'NONE',  ( 0.000000000000000000, -2.646874999522041083, -3.793834371823813445 ) ) ;
#160687 = CARTESIAN_POINT ( 'NONE',  ( 7.450369105909416589, 8.650851030771185890, -1.199719254218441611 ) ) ;
#160688 = DIRECTION ( 'NONE',  ( 0.000000000000000000, 0.000000000000000000, 1.000000000000000000 ) ) ;
#160689 = CARTESIAN_POINT ( 'NONE',  ( 0.2333690889706682703, 0.003390530909083006028, -2.053566628440507635 ) ) ;
#160690 = CARTESIAN_POINT ( 'NONE',  ( -1.364683531250010295, 11.69270833367473017, 0.7879004041258445001 ) ) ;
#160691 = CARTESIAN_POINT ( 'NONE',  ( -3.588104209110990706, 7.337872010604796991, 1.040834085586084257E-14 ) ) ;
#160693 = CARTESIAN_POINT ( 'NONE',  ( -3.973948422136981407, 5.729635473950147606, -1.443375672974066548 ) ) ;
#160692 = PLANE ( 'NONE',  #27692 ) ;
#160694 = CARTESIAN_POINT ( 'NONE',  ( 3.937908632975633871, -1.444535402496229137, -0.9590898762639500363 ) ) ;
#160695 = CARTESIAN_POINT ( 'NONE',  ( -4.120788623549732854, 6.895004929861607401, -1.199719254218452047 ) ) ;
#160696 = CARTESIAN_POINT ( 'NONE',  ( 1.323191598296684646, -1.869966582492128548, -0.8887066864657000576 ) ) ;
#160697 = CARTESIAN_POINT ( 'NONE',  ( 2.829822700998831486, 0.7593016614581545864, -1.976571788296621834 ) ) ;
#160698 = CARTESIAN_POINT ( 'NONE',  ( 3.520313441042647540, 7.258782781191745137, 0.7998128361456321445 ) ) ;
#160699 = CARTESIAN_POINT ( 'NONE',  ( 8.372323551638698902, 9.726464550788689323, 1.199719254218462483 ) ) ;
#160700 = DIRECTION ( 'NONE',  ( 5.551115123125765446E-17, 0.000000000000000000, -1.000000000000000000 ) ) ;
#160701 = CARTESIAN_POINT ( 'NONE',  ( 0.9538786243144499188, -0.7140540310214549269, 1.835613268467409576 ) ) ;
#160702 = CARTESIAN_POINT ( 'NONE',  ( 4.075236096247129680, 7.726954018008360237, 0.5961105570580684798 ) ) ;
#160703 = CARTESIAN_POINT ( 'NONE',  ( 5.856759171423504107, 5.935233242856626568, -0.7216878364870257245 ) ) ;
#160705 = PLANE ( 'NONE',  #94759 ) ;
#160704 = CARTESIAN_POINT ( 'NONE',  ( 1.737499999999999378, -1.516666666666666163, -3.009438278150925683 ) ) ;
#160706 = CARTESIAN_POINT ( 'NONE',  ( 3.029517917392979598, -1.539792254791607862, -1.698243321706040421 ) ) ;
#160707 = CARTESIAN_POINT ( 'NONE',  ( 1.242498012622397674, 0.3540479964400863877, 1.790853789395550955 ) ) ;
#160708 = CARTESIAN_POINT ( 'NONE',  ( 3.041163856788456687, 0.05134138945498378792, 1.911883771832747048 ) ) ;
#160709 = CARTESIAN_POINT ( 'NONE',  ( 7.042534447655770080, 7.180988041878682004, -0.7998128361456341429 ) ) ;
#160710 = CARTESIAN_POINT ( 'NONE',  ( 5.626270559546810546, 8.547437505237857280, 1.082531754730558626 ) ) ;
#160711 = CARTESIAN_POINT ( 'NONE',  ( -9.318531651294266638, 9.766041769465124034, -0.7998128361456291469 ) ) ;
#160712 = CARTESIAN_POINT ( 'NONE',  ( 1.898691433116481031, -1.975183796067316866, -0.3886032139628642912 ) ) ;
#160713 = CARTESIAN_POINT ( 'NONE',  ( 1.727322521004183598, 0.1496332796787832875, -1.956138870750294023 ) ) ;
#160714 = CARTESIAN_POINT ( 'NONE',  ( -9.158696461231359720, 10.64389961198009615, 1.199719254218462483 ) ) ;
#160715 = CARTESIAN_POINT ( 'NONE',  ( -6.906989191158078079, 10.14557225873805812, -1.199719254218440723 ) ) ;
#160716 = CARTESIAN_POINT ( 'NONE',  ( -11.41381675112453387, 10.19999999999999929, -3.704697986577184299 ) ) ;
#160718 = CARTESIAN_POINT ( 'NONE',  ( 3.063107849133941851, 0.2611542325122416797, -1.750338901227658894 ) ) ;
#160717 = CARTESIAN_POINT ( 'NONE',  ( 5.332010518800971433, 2.059573894497103819, 0.3580650863252275440 ) ) ;
#160719 = CARTESIAN_POINT ( 'NONE',  ( -8.065673738755203104, 15.99999998465560758, 8.613976760013509093 ) ) ;
#160720 = EDGE_CURVE ( 'NONE', #512, #198714, #105561, .T. ) ;
#160722 = CARTESIAN_POINT ( 'NONE',  ( 0.04132284026489921325, -1.696808583893465894, -1.386471574116483696 ) ) ;
#160721 = CARTESIAN_POINT ( 'NONE',  ( 1.608462485350597770, 8.735270501766754236, -2.463594439587629914 ) ) ;
#160723 = CARTESIAN_POINT ( 'NONE',  ( 4.400191647014492169, 1.342938829013840207, -1.106906270395467295 ) ) ;
#160724 = CARTESIAN_POINT ( 'NONE',  ( 9.738834413317897898, 10.25639499182604730, 0.000000000000000000 ) ) ;
#160725 = DIRECTION ( 'NONE',  ( 0.000000000000000000, 0.000000000000000000, 1.000000000000000000 ) ) ;
#160726 = CARTESIAN_POINT ( 'NONE',  ( 4.727759377455642564, -1.549208768551156190, -0.7787371415562751586 ) ) ;
#160727 = CARTESIAN_POINT ( 'NONE',  ( 4.229095133649480864, -2.024433085375398900, -0.7850780064641171840 ) ) ;
#160728 = CARTESIAN_POINT ( 'NONE',  ( 2.510230996824538430, 6.080353262937265413, 0.000000000000000000 ) ) ;
#160729 = CARTESIAN_POINT ( 'NONE',  ( 6.385953923436008317, -2.015982004707029596, 0.05432014494890363698 ) ) ;
#160730 = CARTESIAN_POINT ( 'NONE',  ( 6.156250000000002665, -1.895863743163982207, 0.7852924748303072855 ) ) ;
#160731 = CARTESIAN_POINT ( 'NONE',  ( 4.161989969715272686, 4.726297878971393196, 2.500000000000011102 ) ) ;
#160732 = CARTESIAN_POINT ( 'NONE',  ( 2.819263867200746176, -0.1907306445340165024, 1.916936124417574661 ) ) ;
#160733 = CARTESIAN_POINT ( 'NONE',  ( 0.7500000000000006661, 9.947916667349469222, -1.299038105676657340 ) ) ;
#160734 = CARTESIAN_POINT ( 'NONE',  ( 0.03034698492793227315, -2.177136498186870384, 0.4399771670399817425 ) ) ;
#160735 = VERTEX_POINT ( 'NONE', #23188 ) ;
#160736 = CARTESIAN_POINT ( 'NONE',  ( 6.983263157960372780, 7.052928845687945980, 2.444341994195888379 ) ) ;
#160737 = CARTESIAN_POINT ( 'NONE',  ( 1.499999999999989120, 3.504166666666683749, 0.8660254037844524744 ) ) ;
#160738 = CARTESIAN_POINT ( 'NONE',  ( 4.937140493670735708, 8.911747675924535983, -0.7998128361456281477 ) ) ;
#160739 = CARTESIAN_POINT ( 'NONE',  ( 2.262617597476920039, 2.220861250988148683, 0.05131716197829398751 ) ) ;
#160740 = CARTESIAN_POINT ( 'NONE',  ( 6.127922243696800386, 10.09306701771420656, -0.7216878364870267237 ) ) ;
#160741 = CARTESIAN_POINT ( 'NONE',  ( -10.43941509239824228, 11.28166515066052966, 1.040834085586084257E-14 ) ) ;
#160742 = CIRCLE ( 'NONE', #5003, 10.99999999999999112 ) ;
#160743 = CARTESIAN_POINT ( 'NONE',  ( 2.891631901464575272, 6.595597328342462262, 0.000000000000000000 ) ) ;
#160744 = CARTESIAN_POINT ( 'NONE',  ( 0.2291389764034670318, 2.011204493129043591, 0.1455304468792120720 ) ) ;
#160746 = CARTESIAN_POINT ( 'NONE',  ( 5.125460521936802571, 0.2056810312900352600, -2.052415479088207650 ) ) ;
#160745 = CARTESIAN_POINT ( 'NONE',  ( 9.399880572976245574, 9.860948844760784482, 0.7998128361456462443 ) ) ;
#160747 = CARTESIAN_POINT ( 'NONE',  ( -4.253507506385335368, 5.985511395581417204, 1.599625672291267398 ) ) ;
#160748 = AXIS2_PLACEMENT_3D ( 'NONE', #171051, #36781, #173214 ) ;
#160749 = CARTESIAN_POINT ( 'NONE',  ( -1.500000000000011324, 4.910416667349486453, -0.8660254037844313801 ) ) ;
#160750 = CARTESIAN_POINT ( 'NONE',  ( 1.364683531249986537, 0.9052083336747533959, -0.7879004041258239610 ) ) ;
#160751 = CARTESIAN_POINT ( 'NONE',  ( 6.889956934492897034, -0.7990643998789861424, 1.689675875712663755 ) ) ;
#160752 = CARTESIAN_POINT ( 'NONE',  ( 6.135404405475363809, 0.5537102809010217008, 1.643457313873160741 ) ) ;
#160753 = CARTESIAN_POINT ( 'NONE',  ( 5.653775904655955920, 0.7130309894091393375, 1.587888939141286038 ) ) ;
#160754 = CARTESIAN_POINT ( 'NONE',  ( 2.894357049080374278, -0.6678387144627718763, -2.192917219349885816 ) ) ;
#160755 = CARTESIAN_POINT ( 'NONE',  ( -1.364683531250000748, -0.9906249996585805295, 0.000000000000000000 ) ) ;
#160756 = CARTESIAN_POINT ( 'NONE',  ( 2.290725937607818175, 1.422998120520948984, 1.168276728405498455 ) ) ;
#160757 = EDGE_CURVE ( 'NONE', #80954, #110599, #114196, .T. ) ;
#160758 = CARTESIAN_POINT ( 'NONE',  ( -0.4123176713736765309, 3.999999999999973799, 0.8977835139437544409 ) ) ;
#160759 =( NAMED_UNIT ( * ) PLANE_ANGLE_UNIT ( ) SI_UNIT ( $, .RADIAN. ) );
#160760 = CARTESIAN_POINT ( 'NONE',  ( 2.115964440355810439, -0.8579360106165806465, -1.611413330227830176 ) ) ;
#160761 = CARTESIAN_POINT ( 'NONE',  ( 2.197888892816081796, 1.802417619043535701, 0.9041091288993635677 ) ) ;
#160762 = CARTESIAN_POINT ( 'NONE',  ( -2.765500147063310266, 6.170241238308400433, 1.040834085586084257E-14 ) ) ;
#160763 = CARTESIAN_POINT ( 'NONE',  ( 6.861939425476737853, 15.00000000000000000, -9.452896198007838535 ) ) ;
#160764 = CARTESIAN_POINT ( 'NONE',  ( 4.155375932019107488, -1.749630165425161143, -1.171798067238625229 ) ) ;
#160765 = CARTESIAN_POINT ( 'NONE',  ( -5.442708600882160574, 8.437244903416123876, -1.199719254218446718 ) ) ;
#160766 = CARTESIAN_POINT ( 'NONE',  ( 6.743451644395038080, 14.99925532292382790, 9.536680772710601772 ) ) ;
#160767 =( BOUNDED_CURVE ( )  B_SPLINE_CURVE ( 2, ( #70597, #38135, #154021, #5588, #71667, #203799, #55445 ),
 .UNSPECIFIED., .F., .T. ) 
 B_SPLINE_CURVE_WITH_KNOTS ( ( 3, 2, 2, 3 ),
 ( 0.3423693953400485657, 0.3452380952380952328, 0.3511904761904761640, 0.3540591760885228867 ),
 .UNSPECIFIED. ) 
 CURVE ( )  GEOMETRIC_REPRESENTATION_ITEM ( )  RATIONAL_B_SPLINE_CURVE ( ( 0.9331000818465633451, 0.9354320710352566071, 1.000000000000000000, 0.8660254037844387076, 1.000000000000000000, 0.9354320710352559409, 0.9331000818465633451 ) ) 
 REPRESENTATION_ITEM ( '' )  );
#160768 = AXIS2_PLACEMENT_3D ( 'NONE', #193979, #191838, #9899 ) ;
#160769 = CARTESIAN_POINT ( 'NONE',  ( 2.752462066230080495, -2.064650614848703825, -0.1547973748374023295 ) ) ;
#160770 = CARTESIAN_POINT ( 'NONE',  ( 3.897079088924235712, 6.634010472798538949, 1.199719254218462483 ) ) ;
#160771 = CARTESIAN_POINT ( 'NONE',  ( -3.956095110007852622E-14, -1.015624999658570893, 1.570758158831770279 ) ) ;
#160773 = B_SPLINE_CURVE_WITH_KNOTS ( 'NONE', 3,
 ( #210190, #80201, #93288, #179847, #191804, #61828 ),
 .UNSPECIFIED., .F., .F.,
 ( 4, 2, 4 ),
 ( 0.000000000000000000, 0.0003767643964918267023, 0.0007535287929836531878 ),
 .UNSPECIFIED. ) ;
#160772 = CARTESIAN_POINT ( 'NONE',  ( 4.881546266219149999, 0.2071824046101199135, -2.110321684233848583 ) ) ;
#160774 = CARTESIAN_POINT ( 'NONE',  ( 6.586557105272873969, -1.791547847876047594, -0.3505316570680468979 ) ) ;
#160775 = VERTEX_POINT ( 'NONE', #11221 ) ;
#160776 = CARTESIAN_POINT ( 'NONE',  ( -4.796552484184649856, 8.818004674849227342, -0.7998128361456362523 ) ) ;
#160777 = CARTESIAN_POINT ( 'NONE',  ( 9.398826802771546696, 11.98838390803207865, -1.599625672291262513 ) ) ;
#160778 = CARTESIAN_POINT ( 'NONE',  ( 6.251718229232841928, 8.387033582228703210, -1.443375672974078761 ) ) ;
#160779 = CARTESIAN_POINT ( 'NONE',  ( 1.737500000000001155, -1.239583332377419689, 3.009438278150922130 ) ) ;
#160780 = CARTESIAN_POINT ( 'NONE',  ( -6.067437437315529536, 7.037430750744921859, 1.199719254218450271 ) ) ;
#160781 = CARTESIAN_POINT ( 'NONE',  ( 6.486587849989844834, -1.303813291173651301, 1.673118453357678392 ) ) ;
#160782 = CARTESIAN_POINT ( 'NONE',  ( 1.465998146299499094, 2.074868464730471374, -0.3595401751291906756 ) ) ;
#160783 = CARTESIAN_POINT ( 'NONE',  ( -5.842637852846353397, 5.781108681267656202, 0.7998128361456281477 ) ) ;
#160784 = CARTESIAN_POINT ( 'NONE',  ( 10.06423010004587759, 10.63602329300870153, 0.000000000000000000 ) ) ;
#160785 = CARTESIAN_POINT ( 'NONE',  ( 4.768306509995578146, -0.7929947328253506011, -1.683642203456004127 ) ) ;
#160786 = CARTESIAN_POINT ( 'NONE',  ( 8.749089199520284410, 9.101692242395490240, 0.7998128361456481317 ) ) ;
#160787 = CARTESIAN_POINT ( 'NONE',  ( 4.883397849413137592, 4.931525130979966143, -0.7509430347461319988 ) ) ;
#160788 = ORIENTED_EDGE ( 'NONE', *, *, #162297, .T. ) ;
#160789 = CARTESIAN_POINT ( 'NONE',  ( -7.485510208520816278, 8.866088343763324886, 1.082531754730549078 ) ) ;
#160790 = CARTESIAN_POINT ( 'NONE',  ( -2.656508033273816238, 5.186677574539687363, -1.199719254218446718 ) ) ;
#160791 = CARTESIAN_POINT ( 'NONE',  ( -7.346809171966454777, -6.836568542494980250, -8.002408263930250953 ) ) ;
#160792 = CYLINDRICAL_SURFACE ( 'NONE', #213042, 1.500000000000000222 ) ;
#160794 = CARTESIAN_POINT ( 'NONE',  ( 2.207404936347991065, -1.573848641742966459, -1.171066219227391070 ) ) ;
#160793 = CARTESIAN_POINT ( 'NONE',  ( -8.206763054973658100, 8.468978407091068306, 0.7998128361456602331 ) ) ;
#160795 = CARTESIAN_POINT ( 'NONE',  ( 1.446389902895691693, 2.159248346720197276, 0.1057134262518744372 ) ) ;
#160796 = AXIS2_PLACEMENT_3D ( 'NONE', #167542, #5006, #17000 ) ;
#160798 = CARTESIAN_POINT ( 'NONE',  ( -6.103605818514504122, 6.017332118737867219, 0.3415998263276952551 ) ) ;
#160797 = CARTESIAN_POINT ( 'NONE',  ( -6.017840079619296567, 8.114175741012878973, -1.599625672291271394 ) ) ;
#160799 = CARTESIAN_POINT ( 'NONE',  ( 0.6823417656249899377, 1.092708333674752286, 1.181850606188755259 ) ) ;
#160800 = CARTESIAN_POINT ( 'NONE',  ( 3.233448856393176474, -1.601016440221241455, -0.6660543662743572124 ) ) ;
#160801 = CARTESIAN_POINT ( 'NONE',  ( 1.868729199028572596, 1.665863247900209121, -0.5035742270650641617 ) ) ;
#160802 = CARTESIAN_POINT ( 'NONE',  ( 7.836249599018724865, 9.205007956019091608, -1.082531754730537976 ) ) ;
#160803 = CARTESIAN_POINT ( 'NONE',  ( -12.76460961864369814, 7.407083900356914441, 2.164514475593080078 ) ) ;
#160804 = EDGE_CURVE ( 'NONE', #96867, #92970, #59985, .T. ) ;
#160805 = CARTESIAN_POINT ( 'NONE',  ( 0.8607036144342284922, -0.7282710370301350711, 1.880145570116364073 ) ) ;
#160806 = CARTESIAN_POINT ( 'NONE',  ( 6.925078400183590333, 2.001873123210990535, 2.545813127278444998 ) ) ;
#160807 = CARTESIAN_POINT ( 'NONE',  ( -4.122561227007127016, 6.967349310553715647, 1.199719254218452935 ) ) ;
#160808 = CARTESIAN_POINT ( 'NONE',  ( 1.621884544099384096, -1.093522035911981050, -1.640203223306810232 ) ) ;
#160810 = CARTESIAN_POINT ( 'NONE',  ( -6.455090533882213322, 6.703562842383589349, -0.7216878364870338292 ) ) ;
#160809 = CARTESIAN_POINT ( 'NONE',  ( 5.695548698317931091, 1.764485844685494742, -0.7379451211212140205 ) ) ;
#160811 = CARTESIAN_POINT ( 'NONE',  ( -5.709392084686210289, 8.714688961225625974, 1.082531754730550855 ) ) ;
#160812 = CARTESIAN_POINT ( 'NONE',  ( 4.552505719138623341, 8.533283448962240669, 0.7998128361456341429 ) ) ;
#160813 = AXIS2_PLACEMENT_3D ( 'NONE', #147117, #111470, #12810 ) ;
#160814 = CARTESIAN_POINT ( 'NONE',  ( -7.442499979258930587, 7.647614495415686164, -0.7998128361456362523 ) ) ;
#160815 = CARTESIAN_POINT ( 'NONE',  ( 1.453777360798803819, -1.464386276593489189, -1.391179603160071387 ) ) ;
#160816 = CARTESIAN_POINT ( 'NONE',  ( 4.032480619008128819, 1.237564890788948269, -1.947499633988438061 ) ) ;
#160817 = CARTESIAN_POINT ( 'NONE',  ( 6.338335788673861160, -1.050647824335379399, 1.656640365463659670 ) ) ;
#160818 = CARTESIAN_POINT ( 'NONE',  ( 3.151168776707893748, 1.684956273983062580, -1.004420888743910334 ) ) ;
#160819 = CARTESIAN_POINT ( 'NONE',  ( 8.934986926605834157, 10.38290515491702770, -1.199719254218446718 ) ) ;
#160820 = CARTESIAN_POINT ( 'NONE',  ( -9.508802380631136586, 15.10175073245280686, 7.212919681869107258 ) ) ;
#160821 = ORIENTED_EDGE ( 'NONE', *, *, #40961, .T. ) ;
#160822 = CARTESIAN_POINT ( 'NONE',  ( 1.007203092032255665, -0.04580389244966718426, 2.116997601370627091 ) ) ;
#160824 = CARTESIAN_POINT ( 'NONE',  ( -6.995117189646935962, 10.24838825697502109, 1.199719254218453823 ) ) ;
#160823 = CARTESIAN_POINT ( 'NONE',  ( -4.243865776277440993, 4.909930479533815451, -1.199719254218446718 ) ) ;
#160825 = CARTESIAN_POINT ( 'NONE',  ( 2.185277780439310202, -0.7877041259056734024, 1.664256631099890971 ) ) ;
#160826 = ORIENTED_EDGE ( 'NONE', *, *, #101740, .F. ) ;
#160827 = CARTESIAN_POINT ( 'NONE',  ( 11.27149238125475428, 8.841068552745543485, 4.121733248070676758 ) ) ;
#160828 = CARTESIAN_POINT ( 'NONE',  ( 3.445663904809421307, -1.957918079443463855, 0.8150281543025169606 ) ) ;
#160829 = CARTESIAN_POINT ( 'NONE',  ( 1.499999999999989120, 5.035416667349487341, 0.8660254037844524744 ) ) ;
#160830 = CARTESIAN_POINT ( 'NONE',  ( 7.456094412511537151, 10.78619501698377370, 1.199719254218460707 ) ) ;
#160832 = PRESENTATION_STYLE_ASSIGNMENT (( #62261 ) ) ;
#160831 = B_SPLINE_CURVE_WITH_KNOTS ( 'NONE', 3,
 ( #47713, #45576, #11977, #144175 ),
 .UNSPECIFIED., .F., .F.,
 ( 4, 4 ),
 ( 6.656384948891156620E-05, 9.470887020559977376E-05 ),
 .UNSPECIFIED. ) ;
#160833 = CARTESIAN_POINT ( 'NONE',  ( 3.761055697714862589, -1.815786459315921642, -0.9745866149870155981 ) ) ;
#160835 = CARTESIAN_POINT ( 'NONE',  ( 0.2746299231596514012, 1.718356743839201561, -0.6618312839273902126 ) ) ;
#160834 = CARTESIAN_POINT ( 'NONE',  ( -9.027031348600448979, 9.425958082989001952, 1.040834085586084257E-14 ) ) ;
#160836 = CARTESIAN_POINT ( 'NONE',  ( -1.364683531250010295, 3.780208333674750953, 0.7879004041258379498 ) ) ;
#160837 =( NAMED_UNIT ( * ) PLANE_ANGLE_UNIT ( ) SI_UNIT ( $, .RADIAN. ) );
#160838 = CARTESIAN_POINT ( 'NONE',  ( 1.430949710260827068, 3.674736480791771509, 0.4689103363400765612 ) ) ;
#160839 = CARTESIAN_POINT ( 'NONE',  ( -0.01666059994226073634, -0.1612322585618740090, -2.171656592459796808 ) ) ;
#160840 = CARTESIAN_POINT ( 'NONE',  ( 3.023041696300738934, 2.129209760986842781, 0.7651156340112361676 ) ) ;
#160841 = CARTESIAN_POINT ( 'NONE',  ( -8.595506201384022660, 11.05117653974661529, 1.443375672974064550 ) ) ;
#160842 = CARTESIAN_POINT ( 'NONE',  ( 2.636723998446516948, 1.707110652976281839, 0.6067464242315090406 ) ) ;
#160843 = EDGE_CURVE ( 'NONE', #201330, #183276, #30706, .T. ) ;
#160844 = CARTESIAN_POINT ( 'NONE',  ( 2.905391412282500863, -1.844872930762898600, 0.5157873856561823178 ) ) ;
#160845 = CARTESIAN_POINT ( 'NONE',  ( 4.334477209444560053, -1.194628513295314942, 1.690740121169509447 ) ) ;
#160846 = CARTESIAN_POINT ( 'NONE',  ( -1.201851678989727383E-14, 3.509375000341421469, -1.575800808251660134 ) ) ;
#160847 = CARTESIAN_POINT ( 'NONE',  ( 1.586731204520151151, -0.2873679327500404668, -1.950290023627434755 ) ) ;
#160848 = CARTESIAN_POINT ( 'NONE',  ( 0.3934162593667543950, 1.425226140442600098, 1.296210752655905463 ) ) ;
#160849 = CARTESIAN_POINT ( 'NONE',  ( 2.694054421766533203, -1.865511834602461949, -0.1395888279770511053 ) ) ;
#160851 = CARTESIAN_POINT ( 'NONE',  ( 4.641544345285703699, 8.432478572106539616, -0.4375188090333537727 ) ) ;
#160850 = CARTESIAN_POINT ( 'NONE',  ( 2.174872218848258765, -1.417835807431093276, 1.820694940605925849 ) ) ;
#160853 = ADVANCED_FACE ( 'NONE', ( #29633 ), #105755, .T. ) ;
#160852 = CARTESIAN_POINT ( 'NONE',  ( 2.664321193032999524, -0.7092454343347885937, -1.720814620647417303 ) ) ;
#160854 = CARTESIAN_POINT ( 'NONE',  ( -1.364683531249997417, 2.759375000341422801, 1.214306433183764966E-14 ) ) ;
#160855 = CARTESIAN_POINT ( 'NONE',  ( 6.127400154304522673, 0.1556050751826357770, -2.056880999590751991 ) ) ;
#160856 = CARTESIAN_POINT ( 'NONE',  ( -3.899941742225307539, 7.701682465904834629, 0.7998128361456341429 ) ) ;
#160857 = CARTESIAN_POINT ( 'NONE',  ( 8.125414133291656071, 8.374071331795406081, -0.7998128361456291469 ) ) ;
#160858 = CARTESIAN_POINT ( 'NONE',  ( -1.499630086250555605, 3.250805626717326202, 0.09116236908480998546 ) ) ;
#160859 = B_SPLINE_CURVE_WITH_KNOTS ( 'NONE', 3,
 ( #203133, #54775, #104604, #205268, #120922, #38527, #22238, #55839 ),
 .UNSPECIFIED., .F., .F.,
 ( 4, 2, 2, 4 ),
 ( 4.412020206058498508E-14, 0.0006900569950749766085, 0.001035085492590404922, 0.001380113990105833128 ),
 .UNSPECIFIED. ) ;
#160860 = CARTESIAN_POINT ( 'NONE',  ( 6.387733883603046614, 1.449543625446013673, 1.527951702703828074 ) ) ;
#160861 = CARTESIAN_POINT ( 'NONE',  ( -1.364683531250012516, 3.801041667008087099, -0.7879004041258300672 ) ) ;
#160862 = CARTESIAN_POINT ( 'NONE',  ( 6.538358481810655043, 2.137031053877674225, 0.3242996077847115632 ) ) ;
#160863 = CARTESIAN_POINT ( 'NONE',  ( 6.164714676696682716, 0.6357101859572679148, 1.917071687811313652 ) ) ;
#160864 = CARTESIAN_POINT ( 'NONE',  ( 0.6823417656249882723, -0.6572916663252492686, 1.181850606188755259 ) ) ;
#160865 = CARTESIAN_POINT ( 'NONE',  ( -5.436456409399874623, 5.444880020495701523, 0.000000000000000000 ) ) ;
#160866 = ADVANCED_FACE ( 'NONE', ( #26411 ), #76612, .F. ) ;
#160869 = CARTESIAN_POINT ( 'NONE',  ( 3.389175213736285386, 6.897862149426897460, 0.7216878364870317197 ) ) ;
#160868 = CARTESIAN_POINT ( 'NONE',  ( -1.642778471875000035, -0.8677083328553769626, -2.845375778867859751 ) ) ;
#160867 = CARTESIAN_POINT ( 'NONE',  ( 6.444921918449731280, 8.612437886315108315, 1.599625672291268286 ) ) ;
#160870 = CARTESIAN_POINT ( 'NONE',  ( -5.652823702255029836, 5.559658838911111900, -0.7998128361456362523 ) ) ;
#160871 = CARTESIAN_POINT ( 'NONE',  ( 4.891814693739657827, -2.006371927678828104, 0.2024599332275459629 ) ) ;
#160872 = CARTESIAN_POINT ( 'NONE',  ( -7.015454420067433361, 10.27211502579893754, 1.199719254218453823 ) ) ;
#160874 = CARTESIAN_POINT ( 'NONE',  ( -6.034787771414192648, 9.094317262408276648, 1.082531754730549967 ) ) ;
#160873 = CARTESIAN_POINT ( 'NONE',  ( -9.490344339885977476, 11.13478515369756217, -1.082531754730539753 ) ) ;
#160875 = CARTESIAN_POINT ( 'NONE',  ( -1.364683531249997417, 4.759375000341424133, 1.214306433183764966E-14 ) ) ;
#160877 = CARTESIAN_POINT ( 'NONE',  ( 0.6823417656249934904, 8.942708333674733723, 1.181850606188764807 ) ) ;
#160876 = CARTESIAN_POINT ( 'NONE',  ( 6.579002408576895000, -0.1006694238701970334, -2.159482418181729813 ) ) ;
#160878 = CARTESIAN_POINT ( 'NONE',  ( 10.10343170206398966, 2.974000657017692006, -5.833219012919978574 ) ) ;
#160879 = CARTESIAN_POINT ( 'NONE',  ( -11.94589778161906857, 8.080793008161904822, -0.5292555138636146905 ) ) ;
#160881 = CARTESIAN_POINT ( 'NONE',  ( 6.485953897545715385, -2.015913262743720402, 0.05231248585663844652 ) ) ;
#160880 = CARTESIAN_POINT ( 'NONE',  ( -7.497295758232736418, 7.849192594134070333, -0.7216878364870267237 ) ) ;
#160882 = CARTESIAN_POINT ( 'NONE',  ( -1.364683531250014514, -0.9072916663252470482, 0.7879004041258379498 ) ) ;
#160883 = CARTESIAN_POINT ( 'NONE',  ( -1.499999999999997780, 4.900000000000022560, 1.214306433183764966E-14 ) ) ;
#160884 = CARTESIAN_POINT ( 'NONE',  ( 1.840065157383737438, 1.705764225012149859, 0.2551292777918309773 ) ) ;
#160885 = CARTESIAN_POINT ( 'NONE',  ( 8.167861197590044142, 8.493869250135347215, 0.000000000000000000 ) ) ;
#160886 = CARTESIAN_POINT ( 'NONE',  ( 6.364626766972446781, 6.390095747748157251, 0.7998128361456352531 ) ) ;
#160887 = CARTESIAN_POINT ( 'NONE',  ( 0.4458543674108841337, 2.831572362596164627, -1.950633739370720487 ) ) ;
#160888 = CARTESIAN_POINT ( 'NONE',  ( 0.9656335942268097217, 0.8653965441102560163, 1.543625204253181948 ) ) ;
#160889 = CARTESIAN_POINT ( 'NONE',  ( 1.014315213425314166, -2.013265974724808061, 0.002173784167216683862 ) ) ;
#160890 = CARTESIAN_POINT ( 'NONE',  ( -0.3776192402222604549, 3.049641483663570352, -0.4287046358292799231 ) ) ;
#160891 = CARTESIAN_POINT ( 'NONE',  ( 3.258999418838660400, -1.672185875938383859, 1.440126295696932068 ) ) ;
#160892 = CARTESIAN_POINT ( 'NONE',  ( 5.084931552659712750, 2.075598280349931546, 0.6366630897998347693 ) ) ;
#160893 = EDGE_LOOP ( 'NONE', ( #141051, #182875, #45729, #189295, #9748, #66108 ) ) ;
#160894 = CARTESIAN_POINT ( 'NONE',  ( 4.598150373690133463, 5.393538853173795111, -1.199719254218452047 ) ) ;
#160895 = CARTESIAN_POINT ( 'NONE',  ( 8.771762197917315262, 10.29643932140079166, -1.082531754730543083 ) ) ;
#160897 = CARTESIAN_POINT ( 'NONE',  ( 2.829704019156009220, 0.7231233381281774175, -1.882481713119791067 ) ) ;
#160896 = CARTESIAN_POINT ( 'NONE',  ( 3.598385148150527346, -1.043669326629501848, 1.845773325594574077 ) ) ;
#160899 = ORIENTED_EDGE ( 'NONE', *, *, #28879, .F. ) ;
#160898 = CARTESIAN_POINT ( 'NONE',  ( 3.709066938097814514, 1.527391393591450486, -0.9738182928965555263 ) ) ;
#160900 = CARTESIAN_POINT ( 'NONE',  ( 4.701645408888975197, 8.707279753670952971, 0.000000000000000000 ) ) ;
#160901 = ORIENTED_EDGE ( 'NONE', *, *, #181856, .T. ) ;
#160902 = CARTESIAN_POINT ( 'NONE',  ( 0.3384655940862451029, 0.3152513238553408814, 1.843739016257638141 ) ) ;
#160903 = CARTESIAN_POINT ( 'NONE',  ( 6.419949431270806528, 7.448694743692793274, 1.199719254218462483 ) ) ;
#160905 = CARTESIAN_POINT ( 'NONE',  ( 1.358442855636652791, -1.820242846481026078, -0.5975442777857197241 ) ) ;
#160904 = CARTESIAN_POINT ( 'NONE',  ( -5.037017762676898158, 5.835274463666530131, -1.199719254218446718 ) ) ;
#160906 = CARTESIAN_POINT ( 'NONE',  ( 1.499999999999989120, 3.525000000000021227, 1.214306433183764966E-14 ) ) ;
#160907 = CARTESIAN_POINT ( 'NONE',  ( 5.015243055491540147, 4.745538407695236494, 0.3158334299713649318 ) ) ;
#160908 = CIRCLE ( 'NONE', #84681, 0.07999999999999990452 ) ;
#160909 = EDGE_CURVE ( 'NONE', #181560, #102463, #9127, .T. ) ;
#160910 = CARTESIAN_POINT ( 'NONE',  ( -1.364683531250000748, 1.571875000341421691, 0.000000000000000000 ) ) ;
#160911 = DIRECTION ( 'NONE',  ( 0.000000000000000000, 1.000000000000000000, 0.000000000000000000 ) ) ;
#160912 = CARTESIAN_POINT ( 'NONE',  ( -9.657485491635913633, 10.16148791653038330, 1.040834085586084257E-14 ) ) ;
#160913 = VERTEX_POINT ( 'NONE', #76236 ) ;
#160914 = CARTESIAN_POINT ( 'NONE',  ( 5.383715653711652394, 1.448795075966866852, 1.604530791579752425 ) ) ;
#160915 = ADVANCED_FACE ( 'NONE', ( #211554 ), #160692, .F. ) ;
#160916 = CARTESIAN_POINT ( 'NONE',  ( -4.489158259900630554, 8.251452046610447510, 0.000000000000000000 ) ) ;
#160917 = CARTESIAN_POINT ( 'NONE',  ( -7.099629715411508890, 8.311931418515415615, 1.199719254218452047 ) ) ;
#160918 = CARTESIAN_POINT ( 'NONE',  ( 3.181995841446764839, 2.068044944583770306, -0.4684364081647199307 ) ) ;
#160920 = CARTESIAN_POINT ( 'NONE',  ( -11.47191357686926771, 5.776505007901941546, -5.393588192467421827 ) ) ;
#160919 = CARTESIAN_POINT ( 'NONE',  ( -0.1296875068448159474, 0.7431874094961619104, -1.910093690679348200 ) ) ;
#160921 = CARTESIAN_POINT ( 'NONE',  ( 4.499269426148129192, 1.581550893178500727, 1.176622024725955784 ) ) ;
#160922 = CARTESIAN_POINT ( 'NONE',  ( 0.03540237040386850359, -0.09474447662855033092, 2.011072404829179483 ) ) ;
#160923 = ORIENTED_EDGE ( 'NONE', *, *, #159645, .F. ) ;
#160924 = CARTESIAN_POINT ( 'NONE',  ( 5.594942764039734229, 1.868482245966827326, 0.9958698414167986845 ) ) ;
#160925 = CARTESIAN_POINT ( 'NONE',  ( 0.9067890187421032699, 0.5993529260880943177, 1.981728858978973218 ) ) ;
#160926 = CARTESIAN_POINT ( 'NONE',  ( 2.343606807962240524, 1.941525774309307284, 0.04751797161560606525 ) ) ;
#160927 = ORIENTED_EDGE ( 'NONE', *, *, #163868, .F. ) ;
#160928 = CARTESIAN_POINT ( 'NONE',  ( 2.290224193653310536, 5.542776064365107835, 0.4201001246203844297 ) ) ;
#160929 = CARTESIAN_POINT ( 'NONE',  ( 5.528692779322568640, 9.672168352510192690, 0.7998128361456341429 ) ) ;
#160931 = CARTESIAN_POINT ( 'NONE',  ( 5.982172092127724383, 8.002286745614243912, -1.599625672291262513 ) ) ;
#160930 = CARTESIAN_POINT ( 'NONE',  ( 2.642619598058312036, -1.737709898662170183, 1.162055570667380300 ) ) ;
#160932 = CARTESIAN_POINT ( 'NONE',  ( 4.299344108864946890, 6.109263775132799168, -1.443375672974068769 ) ) ;
#160934 = ORIENTED_EDGE ( 'NONE', *, *, #186980, .T. ) ;
#160933 = CARTESIAN_POINT ( 'NONE',  ( -0.05833479489262324152, -1.112358503097829576, -1.430056051773327841 ) ) ;
#160935 = CARTESIAN_POINT ( 'NONE',  ( 4.143358556170802842, -1.920740624720223666, 1.086653567583625746 ) ) ;
#160936 = DIRECTION ( 'NONE',  ( 0.000000000000000000, -1.000000000000000000, 0.000000000000000000 ) ) ;
#160937 = CARTESIAN_POINT ( 'NONE',  ( 3.487540646120320442, 1.995909124301387116, -0.9416478298167814120 ) ) ;
#160938 = CARTESIAN_POINT ( 'NONE',  ( 7.771848369131631351, 10.09024240211882351, -1.599625672291262513 ) ) ;
#160939 = FILL_AREA_STYLE ('',( #112252 ) ) ;
#160940 = CARTESIAN_POINT ( 'NONE',  ( 1.242663310189826564, 1.843194135250892707, 0.5091577964371830634 ) ) ;
#160941 = CARTESIAN_POINT ( 'NONE',  ( 9.748476143425788720, 11.33197590787365172, -1.199719254218440723 ) ) ;
#160942 = CARTESIAN_POINT ( 'NONE',  ( 5.512195382060368409, 2.068158883198469855, -0.09793725168850964113 ) ) ;
#160944 = CARTESIAN_POINT ( 'NONE',  ( 2.694378501574711926, -2.155843008138720762, -0.1600555415394027403 ) ) ;
#160943 = CARTESIAN_POINT ( 'NONE',  ( 5.342823980928593564, 4.390142039796938178, 2.499999999999998668 ) ) ;
#160945 = CARTESIAN_POINT ( 'NONE',  ( 5.003566749295822014, -2.181051155298455058, 0.2145382695054529609 ) ) ;
#160946 = ORIENTED_EDGE ( 'NONE', *, *, #121379, .F. ) ;
#160947 = CARTESIAN_POINT ( 'NONE',  ( 10.72180055030867329, 11.40318881831530540, 0.7998128361456341429 ) ) ;
#160948 = FILL_AREA_STYLE_COLOUR ( '', #128729 ) ;
#160949 = CARTESIAN_POINT ( 'NONE',  ( -9.333041836230016486, 15.44694763438214125, 7.472413793098208856 ) ) ;
#160950 = CARTESIAN_POINT ( 'NONE',  ( 4.552505719138623341, 8.533283448962240669, 0.7998128361456341429 ) ) ;
#160951 = CARTESIAN_POINT ( 'NONE',  ( -3.644109427023046521, 7.473487774827342278, 0.000000000000000000 ) ) ;
#160952 = CARTESIAN_POINT ( 'NONE',  ( 0.2291389764034670318, 2.011204493129043591, 0.1455304468792120720 ) ) ;
#160954 = CARTESIAN_POINT ( 'NONE',  ( -7.863365906246054138, 11.15738207638699464, -1.082531754730543971 ) ) ;
#160953 = COLOUR_RGB ( '', 0.09019608, 0.27058824, 0.51372549) ;
#160955 = CARTESIAN_POINT ( 'NONE',  ( 4.064412189046650248, 7.963840997188264659, 0.7998128361456271485 ) ) ;
#160956 = CARTESIAN_POINT ( 'NONE',  ( 5.120015143727554729, 2.048507142264085701, -0.2983452141967629645 ) ) ;
#160957 = CARTESIAN_POINT ( 'NONE',  ( 3.018101299323606046, -0.9500872288037317537, -1.675862364343786215 ) ) ;
#160958 = CARTESIAN_POINT ( 'NONE',  ( -0.1058464554703278104, -0.8645191204341062807, -1.819937883007181512 ) ) ;
#160959 = CARTESIAN_POINT ( 'NONE',  ( 4.299907273828439180, 8.168308919441841454, 1.040834085586084257E-14 ) ) ;
#160960 = CARTESIAN_POINT ( 'NONE',  ( 9.476364159883866378, 3.602179703620744800, 7.289721612074727908 ) ) ;
#160961 = CARTESIAN_POINT ( 'NONE',  ( 3.731269929808676000, 0.05278475387572807015, -1.968924232409387409 ) ) ;
#160962 = CARTESIAN_POINT ( 'NONE',  ( 0.4456111923471539615, 0.6836232613432814409, -2.082162021007263331 ) ) ;
#160963 = CARTESIAN_POINT ( 'NONE',  ( 4.160648861918358143, -1.351394993475165673, 1.227733137840483879 ) ) ;
#160964 = AXIS2_PLACEMENT_3D ( 'NONE', #133574, #199580, #193468 ) ;
#160965 = CARTESIAN_POINT ( 'NONE',  ( 7.214347136247488912, 7.589362211809770997, -0.7216878364870317197 ) ) ;
#160966 = CARTESIAN_POINT ( 'NONE',  ( 3.172244755473273781, 6.644776614786712443, 0.000000000000000000 ) ) ;
#160967 = CARTESIAN_POINT ( 'NONE',  ( -7.767895665986912057, 8.027242796598338614, -0.7998128361456362523 ) ) ;
#160968 = CARTESIAN_POINT ( 'NONE',  ( 5.716698046817569434, 6.698511138489155137, -1.199719254218452047 ) ) ;
#160969 = EDGE_LOOP ( 'NONE', ( #26236, #77156, #85669, #201069 ) ) ;
#160971 = CARTESIAN_POINT ( 'NONE',  ( 5.590095194574172588, 1.202541018705102660, 1.614423701025817115 ) ) ;
#160970 = CARTESIAN_POINT ( 'NONE',  ( 1.909461114401575843, -0.8690924446688346183, -1.623246667998109682 ) ) ;
#160972 = CARTESIAN_POINT ( 'NONE',  ( 0.4393512522801552023, 1.325809523182071237, 1.877307722886724317 ) ) ;
#160973 = CARTESIAN_POINT ( 'NONE',  ( 5.453941704850034711, -0.7095916301838971485, 1.829088932523432964 ) ) ;
#160974 = CARTESIAN_POINT ( 'NONE',  ( -6.073162743917628781, 9.172774736957510555, -1.199719254218440723 ) ) ;
#160975 = DIRECTION ( 'NONE',  ( -0.000000000000000000, -1.000000000000000000, -0.000000000000000000 ) ) ;
#160976 = CARTESIAN_POINT ( 'NONE',  ( -4.485049888022365927, 4.126979712314507331, 0.7998128361456341429 ) ) ;
#160977 = CARTESIAN_POINT ( 'NONE',  ( -7.725699985795401403, -5.832912386296871254, 7.725699985795430713 ) ) ;
#160978 = CARTESIAN_POINT ( 'NONE',  ( -3.786470039966538970, 7.639575156594750283, 0.000000000000000000 ) ) ;
#160980 = CARTESIAN_POINT ( 'NONE',  ( 0.1802491246630563426, -1.813337052076903877, -0.4591185353455888296 ) ) ;
#160979 = CARTESIAN_POINT ( 'NONE',  ( 1.505537475160537264, -2.074567991729712180, 0.2591490344204059881 ) ) ;
#160981 = CARTESIAN_POINT ( 'NONE',  ( -8.081892667527538876, -5.166862915010145052, 7.462104991928527831 ) ) ;
#160982 = CARTESIAN_POINT ( 'NONE',  ( -0.1104750535120043037, 1.338503269012698116, -2.356272470560859755 ) ) ;
#160983 = CARTESIAN_POINT ( 'NONE',  ( 0.5029371931441508625, -1.732330776274123796, 0.1679752909130062255 ) ) ;
#160984 = CARTESIAN_POINT ( 'NONE',  ( 4.801558957534076022, 8.753569217098425170, 0.7998128361456462443 ) ) ;
#160985 = DIRECTION ( 'NONE',  ( 5.551115123125764829E-17, 0.000000000000000000, -1.000000000000000000 ) ) ;
#160986 = CARTESIAN_POINT ( 'NONE',  ( 1.787319861506628804, 1.187891131197996497, 1.250883549239764081 ) ) ;
#160987 = CARTESIAN_POINT ( 'NONE',  ( 1.488088480104592826, -2.181432686776756391, -0.2102995727721947705 ) ) ;
#160988 = CARTESIAN_POINT ( 'NONE',  ( 3.668774463136436736, -1.482526648764719734, 1.634931011441637771 ) ) ;
#160989 = CARTESIAN_POINT ( 'NONE',  ( -10.39336823037077195, 4.932734307774878424, -5.330979603150785451 ) ) ;
#160990 = CARTESIAN_POINT ( 'NONE',  ( 1.587047119190465594, 2.091647000433814352, 0.5815059253076891865 ) ) ;
#160991 = CARTESIAN_POINT ( 'NONE',  ( 1.031563979315492485, -1.156294252604734396, -1.412831148817683680 ) ) ;
#160992 = CARTESIAN_POINT ( 'NONE',  ( 2.905574018005254722, -2.039320757748352086, 0.5691538075108558692 ) ) ;
#160993 = CARTESIAN_POINT ( 'NONE',  ( 6.539320575229256249, 2.979067782826943844, 2.350490835693248126 ) ) ;
#160994 = ORIENTED_EDGE ( 'NONE', *, *, #158806, .T. ) ;
#160996 = CARTESIAN_POINT ( 'NONE',  ( 1.364683531249986537, -0.03229166632525094088, -0.7879004041258309554 ) ) ;
#160995 = CARTESIAN_POINT ( 'NONE',  ( 3.527152830493656577, -2.117552691746289018, 0.8784855890422419433 ) ) ;
#160997 = CARTESIAN_POINT ( 'NONE',  ( -3.838364070418780027, 7.492192144726518954, 0.0001517565043702621237 ) ) ;
#160998 = CARTESIAN_POINT ( 'NONE',  ( 4.216749469050096621, 4.878294787768598262, -1.199719254218452047 ) ) ;
#160999 = CARTESIAN_POINT ( 'NONE',  ( 6.006509256357773552, -2.210310773855695743, -0.2204792344780072411 ) ) ;
#161000 = CARTESIAN_POINT ( 'NONE',  ( -5.694061328059534688, 8.626526735169329996, 1.082531754730548412 ) ) ;
#161001 = CARTESIAN_POINT ( 'NONE',  ( 5.531363484695522637, 5.555604941673978558, -0.7216878364870207285 ) ) ;
#161002 = CARTESIAN_POINT ( 'NONE',  ( -6.521108698048767138, 10.55178454779148289, -0.7216878364870267237 ) ) ;
#161003 = CARTESIAN_POINT ( 'NONE',  ( 5.750066545971570520, 5.881034856487848295, -0.7216878364870458196 ) ) ;
#161004 = ORIENTED_EDGE ( 'NONE', *, *, #153202, .F. ) ;
#161005 = CARTESIAN_POINT ( 'NONE',  ( 4.272111401563948085, 1.799923229630392640, -0.9091438646662284295 ) ) ;
#161007 = CARTESIAN_POINT ( 'NONE',  ( 1.780209297579591565, -1.142364670758776013, -1.717135550327288485 ) ) ;
#161006 = CARTESIAN_POINT ( 'NONE',  ( 5.829115978871627135, 8.888053511070525659, 1.199719254218462483 ) ) ;
#161008 = FACE_BOUND ( 'NONE', #40080, .T. ) ;
#161009 = CARTESIAN_POINT ( 'NONE',  ( 3.729901657090938460, 7.365652676665848553, 0.7216878364870257245 ) ) ;
#161010 = CARTESIAN_POINT ( 'NONE',  ( -6.493979434129342643, -7.868711957284892478, -6.493979434129312445 ) ) ;
#161011 = CARTESIAN_POINT ( 'NONE',  ( -0.6823417656249969321, 4.717708333674755394, -1.181850606188749264 ) ) ;
#161012 = CARTESIAN_POINT ( 'NONE',  ( 5.261759291836726860, 1.077959533075742993, 1.907929976554381124 ) ) ;
#161013 = CARTESIAN_POINT ( 'NONE',  ( 1.881482635453747720, -0.5404922439061732309, -1.942541187959702764 ) ) ;
#161014 = CARTESIAN_POINT ( 'NONE',  ( 2.489598673502769977, -1.836455140896048999, -0.1334285330320400531 ) ) ;
#161015 = CARTESIAN_POINT ( 'NONE',  ( 5.133733721068893807, 9.141106441222381918, 1.040834085586084257E-14 ) ) ;
#161016 = SURFACE_SIDE_STYLE ('',( #128604 ) ) ;
#161017 = CARTESIAN_POINT ( 'NONE',  ( 5.332948099851452461, 0.1360325894329272867, 1.820554394434070744 ) ) ;
#161018 = CARTESIAN_POINT ( 'NONE',  ( 5.836564609439236939, 0.5826586670559866787, -1.930416874340326938 ) ) ;
#161019 = CARTESIAN_POINT ( 'NONE',  ( -7.877450944739929461, 9.149113176073413456, 1.199719254218462483 ) ) ;
#161021 = CARTESIAN_POINT ( 'NONE',  ( -6.493429226302317225, 6.540365283632955773, 0.7998128361456341429 ) ) ;
#161020 = CARTESIAN_POINT ( 'NONE',  ( 5.471622919743277969, 2.182126815565027300, -0.5975609995224858695 ) ) ;
#161022 = CARTESIAN_POINT ( 'NONE',  ( 0.2234445423696731770, -0.1008541980360810469, 2.103780803345968398 ) ) ;
#161023 = CARTESIAN_POINT ( 'NONE',  ( -5.887983850084758330, 10.09134126839936840, 0.7998128361456291469 ) ) ;
#161024 = CARTESIAN_POINT ( 'NONE',  ( 7.242026607993941489, 11.60078147596829901, 0.7998128361456462443 ) ) ;
#161025 = CARTESIAN_POINT ( 'NONE',  ( -3.054546515950523400, 6.451825606165701998, 0.6676900015689657408 ) ) ;
#161026 = DIRECTION ( 'NONE',  ( 0.03900831951378930240, 0.000000000000000000, 0.9992388858569857257 ) ) ;
#161027 = MANIFOLD_SOLID_BREP ( 'Sweep1[8]', #70675 ) ;
#161028 = CARTESIAN_POINT ( 'NONE',  ( -6.418895661066105873, 9.576129806964074120, -1.199719254218440723 ) ) ;
#161029 = DIRECTION ( 'NONE',  ( 0.000000000000000000, 1.000000000000000000, 0.000000000000000000 ) ) ;
#161030 = CARTESIAN_POINT ( 'NONE',  ( 7.795575137733369075, 9.157554417852841411, -1.082531754730537976 ) ) ;
#161031 = CARTESIAN_POINT ( 'NONE',  ( 3.998507505471064594, 7.829874410826325182, -0.01819030738507872169 ) ) ;
#161032 = CARTESIAN_POINT ( 'NONE',  ( -9.544576954340667996, 11.19805653722800365, 1.082531754730558626 ) ) ;
#161034 = CARTESIAN_POINT ( 'NONE',  ( 3.111816671419795011, 1.753586859115576324, 1.363618078755132634 ) ) ;
#161033 = CARTESIAN_POINT ( 'NONE',  ( 1.353939357992512305, -1.539690173578952770, -1.458446627980537480 ) ) ;
#161035 = DIRECTION ( 'NONE',  ( 0.000000000000000000, 0.000000000000000000, -1.000000000000000000 ) ) ;
#161036 = CARTESIAN_POINT ( 'NONE',  ( -6.180537922983287302, 8.303989891604203422, -1.599625672291271394 ) ) ;
#161037 = CARTESIAN_POINT ( 'NONE',  ( 6.636879889089462026, 7.701780277814560982, -1.199719254218446718 ) ) ;
#161038 = CARTESIAN_POINT ( 'NONE',  ( 3.842202535371820993, -0.9690557767615382012, 1.705768119890891610 ) ) ;
#161039 = CARTESIAN_POINT ( 'NONE',  ( 9.240045382913317340, 10.73880668727576015, -1.199719254218446718 ) ) ;
#161040 = CARTESIAN_POINT ( 'NONE',  ( -5.171837412746745244, 6.485142596490002909, 1.193510785747232905 ) ) ;
#161041 = CARTESIAN_POINT ( 'NONE',  ( 2.496672843210871129, 6.064535417054653266, -0.7998128361456291469 ) ) ;
#161042 = CARTESIAN_POINT ( 'NONE',  ( -4.285785955695645910, 7.053815144069948140, 1.082531754730549967 ) ) ;
#161044 = ORIENTED_EDGE ( 'NONE', *, *, #118594, .T. ) ;
#161043 = CARTESIAN_POINT ( 'NONE',  ( -5.910991785878165317, 8.879612269291090598, -1.082531754730538864 ) ) ;
#161045 = CARTESIAN_POINT ( 'NONE',  ( 2.391022662813433453, -2.030629854096975606, -0.6112283555373964061 ) ) ;
#161046 = CARTESIAN_POINT ( 'NONE',  ( -5.906512197408906317, 6.919960980845699439, -1.199719254218453823 ) ) ;
#161047 = CARTESIAN_POINT ( 'NONE',  ( 4.118171802502921253, -1.108985364570359566, -1.855417305202881506 ) ) ;
#161048 = CARTESIAN_POINT ( 'NONE',  ( 3.948646536499214932, -1.533023199436277961, -1.019512891124202403 ) ) ;
#161049 = CARTESIAN_POINT ( 'NONE',  ( -4.980508561475621043, 6.629897003107849685, 1.243112925831350246 ) ) ;
#161050 = CARTESIAN_POINT ( 'NONE',  ( -1.402160292154681736E-14, 0.009375000341421267647, -1.575800808251665908 ) ) ;
#161051 = CARTESIAN_POINT ( 'NONE',  ( 5.226372699876832506, 0.1332071266631333351, 1.735289576922446786 ) ) ;
#161053 = ADVANCED_FACE ( 'NONE', ( #168156 ), #187305, .T. ) ;
#161052 = CARTESIAN_POINT ( 'NONE',  ( 6.727182134110222478, 3.706444386917655986, 2.325533714637216143 ) ) ;
#161054 = CARTESIAN_POINT ( 'NONE',  ( 3.687454593236936251, 7.245854758844324728, -0.7216878364870267237 ) ) ;
#161055 = CARTESIAN_POINT ( 'NONE',  ( 5.314433026432511475, 5.302519407033794430, 1.040834085586084257E-14 ) ) ;
#161056 = CARTESIAN_POINT ( 'NONE',  ( 3.450221060135277629, 2.161883445724331665, 0.001893877739161941697 ) ) ;
#161057 = EDGE_CURVE ( 'NONE', #210172, #118273, #42951, .T. ) ;
#161058 = CIRCLE ( 'NONE', #95370, 0.07999999999999993228 ) ;
#161059 = CARTESIAN_POINT ( 'NONE',  ( 5.923203835008548523, 0.8145033986626595279, 1.844426808122232142 ) ) ;
#161060 = CARTESIAN_POINT ( 'NONE',  ( -9.612367721964613310, 11.27714576612263997, -1.082531754730537976 ) ) ;
#161061 = CARTESIAN_POINT ( 'NONE',  ( 2.922914210685311431, 2.035003303901411265, 0.7295308445595325431 ) ) ;
#161062 = CARTESIAN_POINT ( 'NONE',  ( 4.200430055897656167, -0.6152532741215356316, -1.872979577440760046 ) ) ;
#161063 = AXIS2_PLACEMENT_3D ( 'NONE', #175339, #8544, #73547 ) ;
#161064 = SURFACE_STYLE_USAGE ( .BOTH. , #10525 ) ;
#161065 = CARTESIAN_POINT ( 'NONE',  ( 5.073749223668181152, -1.075672608635285687, 1.616763269924810231 ) ) ;
#161068 = ORIENTED_EDGE ( 'NONE', *, *, #130606, .F. ) ;
#161067 = CARTESIAN_POINT ( 'NONE',  ( 1.500000000000035971, 6.999999999999999112, 9.886859966642587594 ) ) ;
#161066 = CARTESIAN_POINT ( 'NONE',  ( -8.853111119599343937, 10.39134639669645566, 1.082531754730558626 ) ) ;
#161069 = CARTESIAN_POINT ( 'NONE',  ( -7.065734331377342414, 8.272386803808890576, -1.199719254218452047 ) ) ;
#161070 = CARTESIAN_POINT ( 'NONE',  ( -11.92619526913699879, 12.69999999999998153, 1.328859060402684644 ) ) ;
#161072 = ORIENTED_EDGE ( 'NONE', *, *, #57679, .T. ) ;
#161071 = CARTESIAN_POINT ( 'NONE',  ( -4.655245641445871385, 6.524482229810530498, 1.599625672291263179 ) ) ;
#161073 = CARTESIAN_POINT ( 'NONE',  ( -8.392133896734675247, 10.81390885098904420, 1.443375672974064550 ) ) ;
#161074 = CARTESIAN_POINT ( 'NONE',  ( 0.6400319944965120467, -1.562016764346199960, -1.559085968200937256 ) ) ;
#161075 = CARTESIAN_POINT ( 'NONE',  ( -3.285556943749998737, -1.130208332855377140, 1.896917185911908499 ) ) ;
#161076 = CARTESIAN_POINT ( 'NONE',  ( 6.297705697576845729, -1.418553083497756884, -1.355282376159852475 ) ) ;
#161077 = CARTESIAN_POINT ( 'NONE',  ( -1.201851678989727383E-14, 5.009375000341421469, -1.575800808251660134 ) ) ;
#161078 = CARTESIAN_POINT ( 'NONE',  ( -0.7499999999999972244, 4.639583334016150751, -1.299038105676652899 ) ) ;
#161079 = CARTESIAN_POINT ( 'NONE',  ( 5.777328231396808178, 6.232550548966264259, -0.9930585829777474061 ) ) ;
#161080 = CARTESIAN_POINT ( 'NONE',  ( 0.07479286986305544449, 6.948552162806721277, -2.450557996216149892 ) ) ;
#161081 = CARTESIAN_POINT ( 'NONE',  ( 5.015489797737916255, -0.9877249803392705862, -1.553577481828890106 ) ) ;
#161082 = ORIENTED_EDGE ( 'NONE', *, *, #65049, .F. ) ;
#161083 = CARTESIAN_POINT ( 'NONE',  ( 0.6801582343749744686, -0.2760416663252704406, 1.178068619123780802 ) ) ;
#161084 = CARTESIAN_POINT ( 'NONE',  ( -6.808165692356648258, 11.09461040772476714, 0.7998128361456481317 ) ) ;
#161085 = CARTESIAN_POINT ( 'NONE',  ( 0.3094237646162965594, 2.106443173867519437E-14, 1.330970632288056787 ) ) ;
#161086 = CARTESIAN_POINT ( 'NONE',  ( 5.836213162209912930, -1.179542664122106510, -1.762073437084572314 ) ) ;
#161087 = CARTESIAN_POINT ( 'NONE',  ( 1.255262969126037241E-15, 2.999999999999999112, -10.25000000000000000 ) ) ;
#161088 = CARTESIAN_POINT ( 'NONE',  ( 5.983225862332436584, 5.874851682342960402, 0.7998128361456341429 ) ) ;
#161089 = CARTESIAN_POINT ( 'NONE',  ( 0.1806374041631699234, -1.998871265498179506, -0.5013196448642556202 ) ) ;
#161090 = EDGE_CURVE ( 'NONE', #57811, #103946, #114351, .T. ) ;
#161093 = CARTESIAN_POINT ( 'NONE',  ( 3.632213977189250098, 0.2737156317273430894, 1.820677940640710979 ) ) ;
#161092 = CARTESIAN_POINT ( 'NONE',  ( 2.172091045797384989, -0.8737597001905510474, -1.643165899227620796 ) ) ;
#161091 = DIRECTION ( 'NONE',  ( -0.5254827454987585078, 0.7071067811865536790, -0.4731467892558060551 ) ) ;
#161094 = CARTESIAN_POINT ( 'NONE',  ( 8.796542737168120851, 9.157054702984622097, -0.7998128361456211532 ) ) ;
#161095 = PLANE ( 'NONE',  #214094 ) ;
#161096 = CARTESIAN_POINT ( 'NONE',  ( -6.957269102468015554, 8.145844036748005834, 1.199719254218452047 ) ) ;
#161098 = EDGE_LOOP ( 'NONE', ( #77797, #191973, #159895, #6816 ) ) ;
#161097 = CARTESIAN_POINT ( 'NONE',  ( 6.610000000000012754, 2.967812824040618302, 2.453181572820533951 ) ) ;
#161099 = AXIS2_PLACEMENT_3D ( 'NONE', #148896, #468, #132679 ) ;
#161100 = CARTESIAN_POINT ( 'NONE',  ( 3.844505992619148937, 2.196175933995975438, 0.2170506636963928093 ) ) ;
#161101 = CARTESIAN_POINT ( 'NONE',  ( 5.659536867407776839, 0.4493550105662181271, -2.217189852095033942 ) ) ;
#161102 = CARTESIAN_POINT ( 'NONE',  ( -6.453317930424837812, 7.591587675992828466, 1.082531754730549967 ) ) ;
#161103 = CARTESIAN_POINT ( 'NONE',  ( 5.343967111402722736, -1.155686419774919704, -1.395051459885946699 ) ) ;
#161104 = CARTESIAN_POINT ( 'NONE',  ( 6.087116770962817114, 1.596809997336025022, 1.058066368194489959 ) ) ;
#161105 = CARTESIAN_POINT ( 'NONE',  ( 3.939566984407675498, 8.987080315575580514, 0.7749999999999996891 ) ) ;
#161106 = CARTESIAN_POINT ( 'NONE',  ( 6.508674657442179878, 1.384610780642284711, -1.258058027910214927 ) ) ;
#161107 = CARTESIAN_POINT ( 'NONE',  ( 5.479139036522528983, -1.730609802697373079, -0.8137914003483390779 ) ) ;
#161108 = CARTESIAN_POINT ( 'NONE',  ( -0.004084902416449302624, 15.44286970158244721, 11.94689474181819122 ) ) ;
#161109 = CARTESIAN_POINT ( 'NONE',  ( 5.893352214189693683, 1.342564598491655437, 1.153274331617970550 ) ) ;
#161110 = AXIS2_PLACEMENT_3D ( 'NONE', #184085, #168907, #103925 ) ;
#161111 = CARTESIAN_POINT ( 'NONE',  ( 1.833220611596135363, -1.622487599052296670, -1.197302888167578683 ) ) ;
#161113 = CARTESIAN_POINT ( 'NONE',  ( 3.211649026191341072, -0.4105298382788050704, 2.065488094592916823 ) ) ;
#161112 = CARTESIAN_POINT ( 'NONE',  ( -9.854078719034067291, 10.39084668182823634, 0.7998128361456462443 ) ) ;
#161114 = CARTESIAN_POINT ( 'NONE',  ( 9.596473800374404561, 10.09030761005864285, 0.000000000000000000 ) ) ;
#161116 = CARTESIAN_POINT ( 'NONE',  ( -7.980945979938748103, 12.46285407657057220, 0.000000000000000000 ) ) ;
#161115 = CARTESIAN_POINT ( 'NONE',  ( 1.499999999999987121, 0.2541666666666844154, 0.8660254037844524744 ) ) ;
#161117 = CARTESIAN_POINT ( 'NONE',  ( -1.115562610750309283E-14, 8.562500000000000000, 1.500000000000001554 ) ) ;
#161118 = CARTESIAN_POINT ( 'NONE',  ( 2.654562054903885304, 2.005031730908119147, 0.2428967267811207309 ) ) ;
#161119 = CARTESIAN_POINT ( 'NONE',  ( -0.6823417656249969321, 3.467708333674754506, -1.181850606188749264 ) ) ;
#161120 = CARTESIAN_POINT ( 'NONE',  ( 2.347533153460546806, 5.890539112345938300, 0.000000000000000000 ) ) ;
#161121 = EDGE_CURVE ( 'NONE', #10691, #75117, #38207, .T. ) ;
#161122 = CARTESIAN_POINT ( 'NONE',  ( 3.093221446634909721, 1.855696356685032633, -1.108285163885482039 ) ) ;
#161123 = CARTESIAN_POINT ( 'NONE',  ( 5.989670002187236442, 10.20997511251894529, -0.7998128361456481317 ) ) ;
#161124 = CARTESIAN_POINT ( 'NONE',  ( 1.499999999999990896, 4.525000000000021672, 1.214306433183764966E-14 ) ) ;
#161126 = DIRECTION ( 'NONE',  ( 0.000000000000000000, 1.000000000000000000, 0.000000000000000000 ) ) ;
#161125 = CARTESIAN_POINT ( 'NONE',  ( 7.856023664475727308, 8.130058794835305136, -0.7998128361456341429 ) ) ;
#161127 = CARTESIAN_POINT ( 'NONE',  ( 7.741342523278686549, 11.97539067722642869, 0.7216878364870438212 ) ) ;
#161129 = CARTESIAN_POINT ( 'NONE',  ( 7.219375133607416117, 15.46908217912056038, -9.592069343535143844 ) ) ;
#161128 = CARTESIAN_POINT ( 'NONE',  ( 1.311231623020674419, -1.711955697424736744, 1.335301017299495685 ) ) ;
#161130 = CARTESIAN_POINT ( 'NONE',  ( -6.616015773788831211, 7.781401826584148473, 1.082531754730549967 ) ) ;
#161131 = CARTESIAN_POINT ( 'NONE',  ( -1.364683531250012516, 1.280208333674755172, 0.7879004041258379498 ) ) ;
#161132 = CARTESIAN_POINT ( 'NONE',  ( 2.384552795368581890, -0.3778730364575392797, -2.158588602542845347 ) ) ;
#161133 = CARTESIAN_POINT ( 'NONE',  ( 6.883263157960330503, 7.629137130509037412, 2.553810918356711479 ) ) ;
#161134 = CARTESIAN_POINT ( 'NONE',  ( 2.887862062735581326, 1.599188571496454658, 1.600737006856695288 ) ) ;
#161135 = CARTESIAN_POINT ( 'NONE',  ( -8.206763054973658100, 8.468978407091068306, 0.7998128361456602331 ) ) ;
#161136 = CARTESIAN_POINT ( 'NONE',  ( -2.751941993449643409, 6.154423392425789174, 0.7216878364870317197 ) ) ;
#161137 = CARTESIAN_POINT ( 'NONE',  ( -1.364683531250012516, 3.092708333674755838, 0.7879004041258379498 ) ) ;
#161138 = CARTESIAN_POINT ( 'NONE',  ( 4.876420697298537554, 8.045338245374718866, 0.9427337716215690167 ) ) ;
#161139 = CARTESIAN_POINT ( 'NONE',  ( 0.7500000000000006661, 12.58333333333333570, 1.299038105676657340 ) ) ;
#161140 = CARTESIAN_POINT ( 'NONE',  ( 6.536439455564164724, 7.758839131980592718, 1.082531754730549967 ) ) ;
#161141 = EDGE_CURVE ( 'NONE', #117162, #167392, #149998, .T. ) ;
#161142 = CARTESIAN_POINT ( 'NONE',  ( 4.006921011573481906, 1.516870794648169873, 0.9113941657561406284 ) ) ;
#161143 = CARTESIAN_POINT ( 'NONE',  ( 7.723341061279088038, 12.16231500480096983, -0.7998128361456291469 ) ) ;
#161144 = CARTESIAN_POINT ( 'NONE',  ( 0.7628874492277806230, -1.525271245827728661, 1.452362197770618923 ) ) ;
#161145 = CARTESIAN_POINT ( 'NONE',  ( -1.364683531250014514, 9.088541667008060543, -0.7879004041258335089 ) ) ;
#161146 = CARTESIAN_POINT ( 'NONE',  ( -4.960304097753355457, 6.880383762169266504, 1.599625672291263179 ) ) ;
#161147 = CARTESIAN_POINT ( 'NONE',  ( 6.239861269555550649, 2.010826412442122013, -0.1511553674920090573 ) ) ;
#161148 = ORIENTED_EDGE ( 'NONE', *, *, #95435, .F. ) ;
#161149 = CARTESIAN_POINT ( 'NONE',  ( 9.398826802771546696, 11.98838390803207865, -1.599625672291262513 ) ) ;
#161150 = CARTESIAN_POINT ( 'NONE',  ( 3.274138816734498025, -1.115311402298941656, 1.501645261301733481 ) ) ;
#161151 = CARTESIAN_POINT ( 'NONE',  ( 3.133707330959301096, 1.967300496787489639, -0.6450458050009516553 ) ) ;
#161152 = CARTESIAN_POINT ( 'NONE',  ( -5.112833325684904118, 8.979072956692109031, -0.7216878364870338292 ) ) ;
#161153 = CARTESIAN_POINT ( 'NONE',  ( -0.4339420102923736700, 3.713490786104575392, -0.4852232617283411265 ) ) ;
#161154 = CARTESIAN_POINT ( 'NONE',  ( 9.725276259704228821, 10.24057714594344048, 0.7998128361456462443 ) ) ;
#161155 = CARTESIAN_POINT ( 'NONE',  ( -9.707245187965476418, 5.109025436760802563, -6.475459982491707400 ) ) ;
#161156 = PLANE ( 'NONE',  #204357 ) ;
#161157 = CARTESIAN_POINT ( 'NONE',  ( 6.508665849870631348, 1.605377118863276165, -1.447859449074364591 ) ) ;
#161158 = EDGE_CURVE ( 'NONE', #172377, #86628, #10407, .T. ) ;
#161159 = CARTESIAN_POINT ( 'NONE',  ( -1.364683531250010295, 5.092708333674757171, 0.7879004041258379498 ) ) ;
#161160 = CARTESIAN_POINT ( 'NONE',  ( 2.629291921057617554, 0.09916324773191761976, -1.959495597191794225 ) ) ;
#161161 = ADVANCED_FACE ( 'NONE', ( #76480 ), #94895, .F. ) ;
#161162 = CARTESIAN_POINT ( 'NONE',  ( 0.9837497097957871306, 1.861730512597782550, 0.7742002051285418185 ) ) ;
#161163 = CARTESIAN_POINT ( 'NONE',  ( -3.471769853551161411, 6.208092708188416076, 1.199719254218452935 ) ) ;
#161165 = CARTESIAN_POINT ( 'NONE',  ( -11.44791656467458374, 12.29999999999998650, 3.303228920649577294 ) ) ;
#161164 = CARTESIAN_POINT ( 'NONE',  ( 7.072549687823125097, 11.40305840243567381, -0.7998128361456291469 ) ) ;
#161166 = CARTESIAN_POINT ( 'NONE',  ( 1.036156370570060270, 1.841834720703208639, 0.3256331921374157057 ) ) ;
#161167 = CARTESIAN_POINT ( 'NONE',  ( -0.6823417656249969321, 3.717708333674754506, -1.181850606188749264 ) ) ;
#161168 = CARTESIAN_POINT ( 'NONE',  ( 3.234638274129162827, 1.273785088661258058, -1.559031609643942717 ) ) ;
#161170 = CARTESIAN_POINT ( 'NONE',  ( 1.915762678288157383, -1.385565726045881130, -1.600959455242874974 ) ) ;
#161169 = CARTESIAN_POINT ( 'NONE',  ( -6.399085315970151733, 7.528316292462387871, -1.082531754730544860 ) ) ;
#161171 = FACE_OUTER_BOUND ( 'NONE', #57544, .T. ) ;
#161172 = CARTESIAN_POINT ( 'NONE',  ( 4.229010956685672618, -1.930657356216297860, -0.7480826485904977785 ) ) ;
#161173 = CARTESIAN_POINT ( 'NONE',  ( 2.925527285498711549, 6.635141943048991742, 0.7998128361456281477 ) ) ;
#161175 = CARTESIAN_POINT ( 'NONE',  ( 2.544126380858701797, 6.119897877643793116, 0.7998128361456462443 ) ) ;
#161174 = CARTESIAN_POINT ( 'NONE',  ( 0.3454080995960371325, 0.6521308015206389586, -1.986527616087286452 ) ) ;
#161177 = ORIENTED_EDGE ( 'NONE', *, *, #31468, .F. ) ;
#161176 = CARTESIAN_POINT ( 'NONE',  ( 4.963791182761823961, 1.805510465697376610, -0.2690417022049585438 ) ) ;
#161178 = CARTESIAN_POINT ( 'NONE',  ( 7.540305987494599016, 11.94877408538573427, -0.7998128361456291469 ) ) ;
#161179 = CARTESIAN_POINT ( 'NONE',  ( 4.905525160107046645, 6.476373528817812364, -2.499999999999995115 ) ) ;
#161180 = CARTESIAN_POINT ( 'NONE',  ( 10.90672086898367077, 10.32844188227105953, 5.068303158999801994 ) ) ;
#161181 = CARTESIAN_POINT ( 'NONE',  ( 6.774453055690137226, -1.363307072557031985, 1.735998097611628710 ) ) ;
#161183 =( BOUNDED_SURFACE ( )  B_SPLINE_SURFACE ( 3, 2, ( 
 ( #106601, #172629, #153163 ),
 ( #4738, #136927, #22057 ),
 ( #88167, #144431, #127155 ),
 ( #190977, #49808, #44775 ) ),
 .UNSPECIFIED., .F., .F., .F. ) 
 B_SPLINE_SURFACE_WITH_KNOTS ( ( 4, 4 ),
 ( 3, 3 ),
 ( 4.082329036714114956, 4.712388980384689674 ),
 ( 0.000000000000000000, 1.000000000000000000 ),
 .UNSPECIFIED. ) 
 GEOMETRIC_REPRESENTATION_ITEM ( )  RATIONAL_B_SPLINE_SURFACE ( (
 ( 1.000000000000000000, 0.8226529996940207257, 1.000000000000000000),
 ( 1.000000000000000000, 0.7917671131328134493, 1.000000000000000000),
 ( 1.000000000000000000, 0.7517196685946749835, 1.000000000000000000),
 ( 1.000000000000000000, 0.7071067811865544561, 1.000000000000000000) ) ) 
 REPRESENTATION_ITEM ( '' )  SURFACE ( )  );
#161182 = CARTESIAN_POINT ( 'NONE',  ( -8.012344526598182026E-15, 12.35937500034139624, -1.575800808251669460 ) ) ;
#161184 = CARTESIAN_POINT ( 'NONE',  ( 4.916621234345090130, -0.6478637630910142331, -1.799314785492410529 ) ) ;
#161185 = CARTESIAN_POINT ( 'NONE',  ( -3.755772246185468788, 4.340488027759846545, -1.199719254218452047 ) ) ;
#161186 = CARTESIAN_POINT ( 'NONE',  ( 6.226218857173709154, 8.287007971501239467, 1.599625672291281386 ) ) ;
#161187 = CARTESIAN_POINT ( 'NONE',  ( 0.6801582343749952297, 1.088541667008086078, -1.178068619123883165 ) ) ;
#161188 = FILL_AREA_STYLE_COLOUR ( '', #144728 ) ;
#161189 = CARTESIAN_POINT ( 'NONE',  ( 5.281064527722868718, 6.119995689553514140, 1.199719254218462483 ) ) ;
#161190 = ORIENTED_EDGE ( 'NONE', *, *, #142193, .T. ) ;
#161191 = CARTESIAN_POINT ( 'NONE',  ( -8.086512275908061653, 8.398962174839683215, 0.000000000000000000 ) ) ;
#161192 = CARTESIAN_POINT ( 'NONE',  ( 4.815616550699190590, -1.834762568278673900, 0.3632225495420540184 ) ) ;
#161193 = CARTESIAN_POINT ( 'NONE',  ( 10.99976498415366954, -5.359187537802506895, -0.08336379702153423610 ) ) ;
#161194 = CARTESIAN_POINT ( 'NONE',  ( 7.042534447655770080, 7.180988041878682004, -0.7998128361456341429 ) ) ;
#161195 = VECTOR ( 'NONE', #84887, 1000.000000000000000 ) ;
#161196 = DIRECTION ( 'NONE',  ( 0.000000000000000000, 0.7996470168499970610, 0.6004703560067728985 ) ) ;
#161197 = CARTESIAN_POINT ( 'NONE',  ( -5.955741603288206676, 7.127506980570093020, 1.099513196254948699 ) ) ;
#161198 = CARTESIAN_POINT ( 'NONE',  ( -6.588899466561478846, 6.789396920517583922, 0.7216878364870317197 ) ) ;
#161199 = CIRCLE ( 'NONE', #53902, 2.021340551328831392 ) ;
#161200 = CARTESIAN_POINT ( 'NONE',  ( 4.253507506385319381, 5.985511395581417204, 1.599625672291267398 ) ) ;
#161201 = CARTESIAN_POINT ( 'NONE',  ( 1.780066195911081284, -1.089727156841081346, -1.640273131265007844 ) ) ;
#161202 = CARTESIAN_POINT ( 'NONE',  ( 3.726185550002871771, 2.006962945745351945, 0.1948219989877792990 ) ) ;
#161203 = CARTESIAN_POINT ( 'NONE',  ( -7.507464373665155399, 9.781794407407920389, 1.599625672291295375 ) ) ;
#161204 = CARTESIAN_POINT ( 'NONE',  ( 5.890091390494168522, 5.836471141856793388, 0.000000000000000000 ) ) ;
#161205 = FACE_OUTER_BOUND ( 'NONE', #56684, .T. ) ;
#161206 = CARTESIAN_POINT ( 'NONE',  ( 3.908297495596550597, 1.550167135825938569, -1.549264980215167231 ) ) ;
#161207 = CARTESIAN_POINT ( 'NONE',  ( 0.000000000000000000, 9.999999999999998224, -2.000000000000000000 ) ) ;
#161208 = CARTESIAN_POINT ( 'NONE',  ( 2.555585810550043302, 0.5154765373659023764, -1.856070933656640332 ) ) ;
#161209 = CARTESIAN_POINT ( 'NONE',  ( -10.13488352141530768, 11.78278451552804817, 1.199719254218462483 ) ) ;
#161210 = CARTESIAN_POINT ( 'NONE',  ( 0.1331565106231571705, 6.948071080078889850, -2.540993614958915181 ) ) ;
#161211 = CARTESIAN_POINT ( 'NONE',  ( 3.607878275012313285, 6.262922849939428716, 1.082531754730549078 ) ) ;
#161212 = CARTESIAN_POINT ( 'NONE',  ( 7.422199028477372451, 10.74665040227725044, -1.199719254218441611 ) ) ;
#161213 = CARTESIAN_POINT ( 'NONE',  ( 5.286789834324991055, 8.255339675766103724, -1.199719254218452935 ) ) ;
#161214 = CARTESIAN_POINT ( 'NONE',  ( 2.205172540517054802, 5.724451730578533848, 1.040834085586084257E-14 ) ) ;
#161215 = CARTESIAN_POINT ( 'NONE',  ( 4.068855497876973537, 7.761098824249525130, -0.7216878364870338292 ) ) ;
#161216 = ORIENTED_EDGE ( 'NONE', *, *, #171344, .F. ) ;
#161218 = CARTESIAN_POINT ( 'NONE',  ( 1.893228294049788207, -0.1010902060475794423, -2.010683160356161014 ) ) ;
#161217 = CARTESIAN_POINT ( 'NONE',  ( 4.950658015114751009, -1.558304906039936988, -0.9804572199803849308 ) ) ;
#161219 = CARTESIAN_POINT ( 'NONE',  ( 4.815913765717094286, -1.849969270989433534, 1.363755144342413850 ) ) ;
#161221 = CARTESIAN_POINT ( 'NONE',  ( 1.990827601993300666, 0.1760917813397035736, 1.852568099299256366 ) ) ;
#161220 = CARTESIAN_POINT ( 'NONE',  ( -0.1290005225502433017, 7.629137130509076492, -2.773995091683974401 ) ) ;
#161222 = CARTESIAN_POINT ( 'NONE',  ( 1.001543065824772753E-15, -2.121874999522043836, 3.793834371823811669 ) ) ;
#161223 =( NAMED_UNIT ( * ) PLANE_ANGLE_UNIT ( ) SI_UNIT ( $, .RADIAN. ) );
#161224 = CARTESIAN_POINT ( 'NONE',  ( 5.976807594091997800, -1.347613670528555740, 1.357171208065083512 ) ) ;
#161225 = CARTESIAN_POINT ( 'NONE',  ( -7.832860060393135093, 10.16142270859057462, 1.599625672291295375 ) ) ;
#161226 = CARTESIAN_POINT ( 'NONE',  ( -5.994113311017573054, 6.165756082374834079, 0.7216878364870257245 ) ) ;
#161228 = CARTESIAN_POINT ( 'NONE',  ( 2.992876365407059147, 1.605230647100181596, -0.9602576221170722182 ) ) ;
#161227 = CARTESIAN_POINT ( 'NONE',  ( 4.405862271158119903, -0.8954353465763136288, -1.889446048457727789 ) ) ;
#161229 = CARTESIAN_POINT ( 'NONE',  ( 7.632877294813741109, 8.007371053478589573, 1.040834085586084257E-14 ) ) ;
#161230 = DIRECTION ( 'NONE',  ( 5.551115123125765446E-17, 0.000000000000000000, -1.000000000000000000 ) ) ;
#161231 = DIRECTION ( 'NONE',  ( -5.578564026256490882E-16, -1.000000000000000000, -9.066213480720158442E-32 ) ) ;
#161232 = CARTESIAN_POINT ( 'NONE',  ( 4.793404903408416295, 1.281069664470562142, 1.155212482600373125 ) ) ;
#161233 = CARTESIAN_POINT ( 'NONE',  ( -5.388475986427523345, 8.373973519885682393, 1.199719254218452047 ) ) ;
#161234 = CARTESIAN_POINT ( 'NONE',  ( -15.75000000000000000, 13.40000000000000036, -1.100000000000002087 ) ) ;
#161235 = LINE ( 'NONE', #61595, #43251 ) ;
#161237 = ADVANCED_FACE ( 'NONE', ( #13611 ), #12539, .F. ) ;
#161236 = CARTESIAN_POINT ( 'NONE',  ( 6.262907710099243630, -0.1037740067610822270, -2.014008436551452785 ) ) ;
#161238 = VECTOR ( 'NONE', #193929, 1000.000000000000000 ) ;
#161239 = CARTESIAN_POINT ( 'NONE',  ( 6.385609454247954453, -2.047150228866960298, 0.7234482234039444348 ) ) ;
#161240 = CARTESIAN_POINT ( 'NONE',  ( 4.863791234866603475, 1.805334366393744450, -0.2710410529033688842 ) ) ;
#161241 = CARTESIAN_POINT ( 'NONE',  ( 1.323018481131872370, -1.771187822987334570, -0.8437873667686208723 ) ) ;
#161242 = CARTESIAN_POINT ( 'NONE',  ( 0.4568545718052554050, -1.995212666551810399, -0.7087754862673681933 ) ) ;
#161243 = CARTESIAN_POINT ( 'NONE',  ( -0.6823417656250212460, 3.363541667008085323, 1.181850606188767472 ) ) ;
#161244 = CARTESIAN_POINT ( 'NONE',  ( 10.12536109763334125, -7.563986176625362212, -0.4645846211130729708 ) ) ;
#161245 = CARTESIAN_POINT ( 'NONE',  ( 8.158255747121103241, 10.54105100977322174, 1.599625672291281386 ) ) ;
#161246 = AXIS2_PLACEMENT_3D ( 'NONE', #188477, #120358, #186336 ) ;
#161247 = CARTESIAN_POINT ( 'NONE',  ( 2.244932509249154329, 2.057497683098849617, 0.5125483897536405875 ) ) ;
#161248 = CARTESIAN_POINT ( 'NONE',  ( -4.012850279964973232, 4.744375417122949301, 1.082531754730560403 ) ) ;
#161249 = CARTESIAN_POINT ( 'NONE',  ( 3.913815762669449416, 7.330443837381343641, -0.8582294057540799104 ) ) ;
#161250 = CARTESIAN_POINT ( 'NONE',  ( -3.904385050611244079, 7.498940292447679568, 1.040834085586084257E-14 ) ) ;
#161251 = CARTESIAN_POINT ( 'NONE',  ( 0.7255434793691470929, 0.2065170452952343472, -2.059959488672699290 ) ) ;
#161253 = CARTESIAN_POINT ( 'NONE',  ( 0.7500000000000006661, 14.19791666734946567, -1.299038105676657340 ) ) ;
#161252 = CARTESIAN_POINT ( 'NONE',  ( 6.883263157960364254, 3.685033293952295175, 2.667793810733168236 ) ) ;
#161255 = ORIENTED_EDGE ( 'NONE', *, *, #203422, .T. ) ;
#161254 = CARTESIAN_POINT ( 'NONE',  ( 2.297798353768167434, 2.029563722251678026, -0.9032078376340900716 ) ) ;
#161256 = CARTESIAN_POINT ( 'NONE',  ( 0.3175262209036809891, 1.174723722100686762, -1.975753589677962552 ) ) ;
#161258 = CARTESIAN_POINT ( 'NONE',  ( 6.086800983681886379, 1.986285820840045124, 0.5554444937589071429 ) ) ;
#161257 = CARTESIAN_POINT ( 'NONE',  ( 3.277320446201373638, 4.846626492033466072, 1.599625672291267398 ) ) ;
#161260 = CARTESIAN_POINT ( 'NONE',  ( 0.000000000000000000, -1.137499999999999067, -4.012584370867899430 ) ) ;
#161259 = CARTESIAN_POINT ( 'NONE',  ( 5.367048706163317640, 7.354919138647580290, -1.599625672291281386 ) ) ;
#161261 = CARTESIAN_POINT ( 'NONE',  ( 4.877901405866606588, 8.912911750144889567, 0.7998128361456341429 ) ) ;
#161262 = CARTESIAN_POINT ( 'NONE',  ( 0.1333542156527295908, 5.722835866173135777, -2.639957043922738666 ) ) ;
#161263 = CARTESIAN_POINT ( 'NONE',  ( 6.040549724581927293, -1.551790349881351450, 0.9907606852931831742 ) ) ;
#161264 = VECTOR ( 'NONE', #73336, 1000.000000000000000 ) ;
#161265 = CARTESIAN_POINT ( 'NONE',  ( 2.706824224222692088, 6.309712028235118453, 0.7998128361456362523 ) ) ;
#161266 = DIRECTION ( 'NONE',  ( 1.000000000000000000, 0.000000000000000000, 0.000000000000000000 ) ) ;
#161267 = CARTESIAN_POINT ( 'NONE',  ( 3.258550815082728036, -1.306766610546957530, 1.125807055032159054 ) ) ;
#161268 = CARTESIAN_POINT ( 'NONE',  ( 1.692592581891849912, 1.490968054865527082, -1.357870634957742961 ) ) ;
#161269 = CARTESIAN_POINT ( 'NONE',  ( 2.795839995030196423, 1.662961046791612940, -1.587192879829945946 ) ) ;
#161270 = CARTESIAN_POINT ( 'NONE',  ( -1.364683531249997417, 3.321875000341423245, 1.214306433183764966E-14 ) ) ;
#161271 = CARTESIAN_POINT ( 'NONE',  ( 2.355063576532693936, -1.750152493129919717, 1.433722681173225100 ) ) ;
#161272 = CARTESIAN_POINT ( 'NONE',  ( 4.406922956430887162, 1.628233754946675882, -1.335794222675233511 ) ) ;
#161273 = CARTESIAN_POINT ( 'NONE',  ( -7.485510208520816278, 8.866088343763324886, 1.082531754730549078 ) ) ;
#161274 = CARTESIAN_POINT ( 'NONE',  ( 3.725649928583890436, -1.052200936647734286, -1.422817597083583241 ) ) ;
#161275 = CARTESIAN_POINT ( 'NONE',  ( 6.471319392424407901, 6.444294134116939077, 0.7998128361456341429 ) ) ;
#161277 = CARTESIAN_POINT ( 'NONE',  ( 5.935170609274059039, -1.657740282732190096, -1.583558971889464706 ) ) ;
#161276 = CARTESIAN_POINT ( 'NONE',  ( 6.016786309414542622, 10.24161080428416426, 0.7998128361456341429 ) ) ;
#161278 = CARTESIAN_POINT ( 'NONE',  ( 4.927609005033061429, 0.9437523325564222132, -1.580719041474540010 ) ) ;
#161279 = CARTESIAN_POINT ( 'NONE',  ( -3.913499895838973508, 7.717500311787445000, 1.040834085586084257E-14 ) ) ;
#161280 = CARTESIAN_POINT ( 'NONE',  ( 5.382223794500827552, 7.302347065049529462, -1.443375672974051449 ) ) ;
#161281 = CARTESIAN_POINT ( 'NONE',  ( 0.7499999999999902300, 2.983333333333351600, 1.299038105676669330 ) ) ;
#161282 = EDGE_CURVE ( 'NONE', #191009, #58680, #79642, .T. ) ;
#161283 = CARTESIAN_POINT ( 'NONE',  ( 4.734432829848630675, 0.3728853646711489112, 2.159338447334692823 ) ) ;
#161284 = CARTESIAN_POINT ( 'NONE',  ( -5.271422797614987665, 5.044414773505913274, -0.7998128361456221525 ) ) ;
#161285 = CARTESIAN_POINT ( 'NONE',  ( 0.5601741628961998121, 7.746630099212591603, -1.919951735362950052 ) ) ;
#161286 = CARTESIAN_POINT ( 'NONE',  ( 5.413285142218079216, 7.534467834982624623, -1.255836820238024121 ) ) ;
#161287 = CARTESIAN_POINT ( 'NONE',  ( -1.201851678989727383E-14, 4.696875000341419693, -1.575800808251660134 ) ) ;
#161288 = CARTESIAN_POINT ( 'NONE',  ( 3.176308805823165660, -1.146983237646619580, 1.547710939905672989 ) ) ;
#161289 = CARTESIAN_POINT ( 'NONE',  ( -1.364683531250010295, 8.630208333674731946, 0.7879004041258445001 ) ) ;
#161290 = CARTESIAN_POINT ( 'NONE',  ( -4.989037340148921196, 5.883260320670900434, 1.082531754730560403 ) ) ;
#161291 = CARTESIAN_POINT ( 'NONE',  ( 0.4400545237335662940, -2.106857831338632359, 0.7043091553551988904 ) ) ;
#161292 = CARTESIAN_POINT ( 'NONE',  ( -6.305950844131887223, 6.529566537674873494, 0.000000000000000000 ) ) ;
#161293 = ORIENTED_EDGE ( 'NONE', *, *, #22449, .F. ) ;
#161295 = CARTESIAN_POINT ( 'NONE',  ( 3.847109862837356786, 4.045599327266925727, -0.8077998227820462063 ) ) ;
#161294 = CARTESIAN_POINT ( 'NONE',  ( -5.817857314039913241, 5.960124085900898372, 0.000000000000000000 ) ) ;
#161296 = CARTESIAN_POINT ( 'NONE',  ( 4.599240423533799138, 6.388866465587984322, 1.599625672291267398 ) ) ;
#161297 =( LENGTH_UNIT ( ) NAMED_UNIT ( * ) SI_UNIT ( .MILLI., .METRE. ) );
#161298 = CARTESIAN_POINT ( 'NONE',  ( -2.370002892456521959, 0.1903694832692625627, -0.4477549104883318254 ) ) ;
#161299 = CARTESIAN_POINT ( 'NONE',  ( 11.43209210103587914, 13.65596075983914659, 3.649125173352119944 ) ) ;
#161300 = CARTESIAN_POINT ( 'NONE',  ( -0.6823417656250212460, 3.613541667008085767, 1.181850606188767472 ) ) ;
#161301 = CARTESIAN_POINT ( 'NONE',  ( 2.278492620635372390, 1.590801041788017178, -0.7064735415249421280 ) ) ;
#161302 = CARTESIAN_POINT ( 'NONE',  ( 11.55950211276791251, 9.719999999999982876, 3.221476510067110777 ) ) ;
#161304 = EDGE_CURVE ( 'NONE', #77529, #157380, #99681, .T. ) ;
#161303 = CARTESIAN_POINT ( 'NONE',  ( 0.6780837441340243910, -1.046368970337024473, -1.659334490400856676 ) ) ;
#161305 = CARTESIAN_POINT ( 'NONE',  ( 1.364683531249988757, 1.196875000341421469, 0.000000000000000000 ) ) ;
#161306 = DIRECTION ( 'NONE',  ( -0.000000000000000000, -1.000000000000000000, -0.000000000000000000 ) ) ;
#161307 = CARTESIAN_POINT ( 'NONE',  ( 6.702040708066513197, -2.161345696851162845, 0.04751196314212167288 ) ) ;
#161308 = CARTESIAN_POINT ( 'NONE',  ( -9.459838494033043332, 12.05956421450382088, 1.599625672291281386 ) ) ;
#161309 = CARTESIAN_POINT ( 'NONE',  ( -5.694061327615147050, 9.586895948952255608, 0.000000000000000000 ) ) ;
#161310 = CARTESIAN_POINT ( 'NONE',  ( 5.823154874416164084, -0.05760400987671504547, 2.161107263091876618 ) ) ;
#161311 = ORIENTED_EDGE ( 'NONE', *, *, #160720, .F. ) ;
#161312 = CARTESIAN_POINT ( 'NONE',  ( -0.6823417656250212460, 4.551041667008086655, 1.181850606188767472 ) ) ;
#161313 = CARTESIAN_POINT ( 'NONE',  ( 6.591095686763909001, 1.716256228956919871, -0.9697327587238188107 ) ) ;
#161314 = CARTESIAN_POINT ( 'NONE',  ( 6.380242484794338864, -0.2077342984398328762, 1.721287130621736772 ) ) ;
#161316 = CARTESIAN_POINT ( 'NONE',  ( 3.404031855413204966, -0.8899279105200922357, -2.002928011436304612 ) ) ;
#161315 = CARTESIAN_POINT ( 'NONE',  ( 1.360316468749973584, 0.7864583336747016373, -0.7853790794159161148 ) ) ;
#161317 = CARTESIAN_POINT ( 'NONE',  ( 2.802171680323842118, -0.7245931359087741663, 2.190924829087222303 ) ) ;
#161318 = CARTESIAN_POINT ( 'NONE',  ( 6.134070664438048048, 1.019536383099900245, -1.790854842558225801 ) ) ;
#161319 = CARTESIAN_POINT ( 'NONE',  ( 1.165847801482827517, -1.232189268765693235, 1.500965459471349961 ) ) ;
#161320 = CARTESIAN_POINT ( 'NONE',  ( -4.894130264408858899, 8.653643041878236630, -0.7216878364870207285 ) ) ;
#161321 = PRODUCT_DEFINITION_SHAPE ( 'NONE', 'NONE',  #214424 ) ;
#161322 = CARTESIAN_POINT ( 'NONE',  ( 2.032879073410320814E-16, -7.630846356335640124, -9.566809970447321732 ) ) ;
#161323 = CARTESIAN_POINT ( 'NONE',  ( -9.497986837693062512, 14.58017599252426066, 7.334206418178426112 ) ) ;
#161324 = CARTESIAN_POINT ( 'NONE',  ( 3.586284538990120119, 1.181046903802231984, 1.761068336431830472 ) ) ;
#161325 = LINE ( 'NONE', #160248, #1653 ) ;
#161326 = CARTESIAN_POINT ( 'NONE',  ( 2.637342451166882373, 0.6819965276749391236, 1.897697610567940174 ) ) ;
#161327 = CARTESIAN_POINT ( 'NONE',  ( -4.568734577680875653, 8.274014740695587733, -0.7216878364870257245 ) ) ;
#161328 = CARTESIAN_POINT ( 'NONE',  ( 5.719807747550186505, -2.154180246964752410, 0.4782370604126117142 ) ) ;
#161329 = CARTESIAN_POINT ( 'NONE',  ( -3.285556943749998737, -0.8677083328553740760, 1.896917185911908499 ) ) ;
#161330 = CARTESIAN_POINT ( 'NONE',  ( -2.886704779471910953, -3.062285525734984137, 1.909201817158099335 ) ) ;
#161331 = CARTESIAN_POINT ( 'NONE',  ( 11.97929049433705373, 12.22000000000000064, -0.7046979865771834106 ) ) ;
#161332 = CARTESIAN_POINT ( 'NONE',  ( -6.064239847062411926, 10.29697326487330500, 0.000000000000000000 ) ) ;
#161335 = AXIS2_PLACEMENT_3D ( 'NONE', #14612, #93776, #193380 ) ;
#161334 = DIRECTION ( 'NONE',  ( 0.9999580691339164940, 0.000000000000000000, -0.009157509157509348754 ) ) ;
#161333 = CARTESIAN_POINT ( 'NONE',  ( -5.739830873228516595, 7.379802178037835780, 1.322642659050039970 ) ) ;
#161336 = CARTESIAN_POINT ( 'NONE',  ( 1.551702917632593826, 8.754377144105253805, -2.473499015030054871 ) ) ;
#161337 = EDGE_LOOP ( 'NONE', ( #180916, #99028, #124264, #100953 ) ) ;
#161338 = CARTESIAN_POINT ( 'NONE',  ( 4.592684518728709975, -0.4495978358524716501, -2.011083796685923630 ) ) ;
#161339 = CARTESIAN_POINT ( 'NONE',  ( -6.685579144870156476, 9.853573864773576219, 1.082531754730549967 ) ) ;
#161340 = UNCERTAINTY_MEASURE_WITH_UNIT (LENGTH_MEASURE( 1.000000000000000082E-05 ), #71720, 'distance_accuracy_value', 'NONE');
#161341 = CARTESIAN_POINT ( 'NONE',  ( -1.115562610750309283E-14, 10.84375000068279604, 1.500000000000001554 ) ) ;
#161342 = CARTESIAN_POINT ( 'NONE',  ( -5.525111292768871252, 6.404716915440499037, -1.199719254218446718 ) ) ;
#161343 = CARTESIAN_POINT ( 'NONE',  ( -4.620413885680726196, 7.122912077659854013, 1.384570422981110216 ) ) ;
#161344 = CARTESIAN_POINT ( 'NONE',  ( 3.738929604108613969, 1.918458267904774806, 0.6316034170958833016 ) ) ;
#161345 = CARTESIAN_POINT ( 'NONE',  ( -1.500000000000013101, 1.129166666666688634, -0.8660254037844313801 ) ) ;
#161347 = CARTESIAN_POINT ( 'NONE',  ( 7.917598520700710019, 12.18102267421877727, -0.7216878364870328300 ) ) ;
#161346 = CARTESIAN_POINT ( 'NONE',  ( -3.871735385154307263, 6.674719161725423788, -1.199719254218450271 ) ) ;
#161348 = CARTESIAN_POINT ( 'NONE',  ( 5.472687561410540802, 9.536552588287639409, 0.7998128361456462443 ) ) ;
#161349 = CARTESIAN_POINT ( 'NONE',  ( 2.623961231070126132, -1.185536401616044566, -1.685555923420704039 ) ) ;
#161350 = CARTESIAN_POINT ( 'NONE',  ( 2.619767714365705658, 0.2496074646863334634, 2.000857082853441327 ) ) ;
#161351 = EDGE_LOOP ( 'NONE', ( #175279, #97977, #201005, #1554, #174041, #33826, #200573, #205357 ) ) ;
#161352 = CARTESIAN_POINT ( 'NONE',  ( -6.473746350531913940, 6.725327903095910109, 0.2421321588450163209 ) ) ;
#161353 = CARTESIAN_POINT ( 'NONE',  ( 4.599240423533799138, 6.388866465587984322, 1.599625672291267398 ) ) ;
#161355 = ORIENTED_EDGE ( 'NONE', *, *, #56757, .F. ) ;
#161354 = CARTESIAN_POINT ( 'NONE',  ( -0.007473969438128235526, 8.279395425053861501, -1.999986034896453768 ) ) ;
#161356 = CARTESIAN_POINT ( 'NONE',  ( 2.653672528425448540, -0.3418824089525332455, -1.986742401007553172 ) ) ;
#161357 = CARTESIAN_POINT ( 'NONE',  ( 2.976309490518674217, -0.1360139883382974202, -1.836174483004118674 ) ) ;
#161358 = CARTESIAN_POINT ( 'NONE',  ( 6.393228082638676923, 1.922373441260841087, -1.083778638264052852 ) ) ;
#161359 = CARTESIAN_POINT ( 'NONE',  ( 5.845500506147374153, 6.848780674373954547, 1.199719254218453823 ) ) ;
#161360 = CARTESIAN_POINT ( 'NONE',  ( 2.390102426918311540, -0.9266024157483061519, 1.953076554623616401 ) ) ;
#161361 = CARTESIAN_POINT ( 'NONE',  ( -4.500943810056945438, 5.313817868896925312, 1.082531754730560403 ) ) ;
#161362 = CARTESIAN_POINT ( 'NONE',  ( 4.188735998470741073, 1.634407174013367214, -1.345997343221926545 ) ) ;
#161363 = CARTESIAN_POINT ( 'NONE',  ( 2.583761237542493205, 1.502156065388253081, -1.739619357585840520 ) ) ;
#161364 = VERTEX_POINT ( 'NONE', #65539 ) ;
#161365 = AXIS2_PLACEMENT_3D ( 'NONE', #8752, #5519, #171251 ) ;
#161366 = CARTESIAN_POINT ( 'NONE',  ( -11.94105721237523099, 12.69999999999999929, 1.187919463087248273 ) ) ;
#161367 = CARTESIAN_POINT ( 'NONE',  ( 1.656895194024514906, -1.602792776363659133, -0.9643473572949823325 ) ) ;
#161368 = CARTESIAN_POINT ( 'NONE',  ( 6.104366069677094053, -0.7090783117675543146, -1.839710284007533225 ) ) ;
#161369 = CIRCLE ( 'NONE', #81735, 0.09999999999999982514 ) ;
#161371 = CARTESIAN_POINT ( 'NONE',  ( 8.798878505144646311, 11.28844422746735532, -1.443375672974052559 ) ) ;
#161370 = CARTESIAN_POINT ( 'NONE',  ( -1.364683531250012516, 3.530208333674758059, 0.7879004041258379498 ) ) ;
#161373 = CARTESIAN_POINT ( 'NONE',  ( 0.3642759247451561322, 2.182245240920151375, -0.3280614795862640820 ) ) ;
#161372 = CARTESIAN_POINT ( 'NONE',  ( -7.063961727919978451, 8.200042423116789436, 1.199719254218450271 ) ) ;
#161374 = CARTESIAN_POINT ( 'NONE',  ( 6.320769956279724155, -1.466918727022302971, 1.461273828345016845 ) ) ;
#161375 = CARTESIAN_POINT ( 'NONE',  ( 6.114890974963323345, 7.092793211334054604, 1.199719254218462483 ) ) ;
#161376 = CARTESIAN_POINT ( 'NONE',  ( -5.551173829791513192, 8.563787670477010394, 1.199719254218452047 ) ) ;
#161377 = CARTESIAN_POINT ( 'NONE',  ( 6.539320575229297106, 0.5644099559201658511, 2.255290358406045303 ) ) ;
#161378 = CARTESIAN_POINT ( 'NONE',  ( 5.453970954872065846, 1.969229766360120149, -0.09616449669870225092 ) ) ;
#161379 = CARTESIAN_POINT ( 'NONE',  ( -0.1401555495076401980, -1.643345231473653190, -1.339971704266910812 ) ) ;
#161380 = CARTESIAN_POINT ( 'NONE',  ( 1.499999999999987121, 0.8270833340161471980, -0.8660254037844253849 ) ) ;
#161381 = CARTESIAN_POINT ( 'NONE',  ( 4.248838534556359292, 0.6131519058680062750, 2.224680453567278171 ) ) ;
#161382 = CARTESIAN_POINT ( 'NONE',  ( 2.043871907009750633, 1.419221230981766668, 1.496905473486829230 ) ) ;
#161383 = CARTESIAN_POINT ( 'NONE',  ( 7.944714827928056167, 8.371181508778631652, 0.7216878364870458196 ) ) ;
#161384 = EDGE_CURVE ( 'NONE', #154266, #19980, #197299, .T. ) ;
#161385 = CARTESIAN_POINT ( 'NONE',  ( 4.193214648376505593, 8.114110533073061404, 0.000000000000000000 ) ) ;
#161386 = CARTESIAN_POINT ( 'NONE',  ( 3.088225128862704949, 6.824956093640315302, 0.7998128361456281477 ) ) ;
#161387 =( BOUNDED_CURVE ( )  B_SPLINE_CURVE ( 2, ( #62804, #158201, #76917, #143043, #92147, #44452, #176571, #93211, #178710 ),
 .UNSPECIFIED., .F., .T. ) 
 B_SPLINE_CURVE_WITH_KNOTS ( ( 3, 2, 2, 2, 3 ),
 ( 0.6406250000000002220, 0.6458333333333333703, 0.6562500000000000000, 0.6666666666666666297, 0.6718749999999998890 ),
 .UNSPECIFIED. ) 
 CURVE ( )  GEOMETRIC_REPRESENTATION_ITEM ( )  RATIONAL_B_SPLINE_CURVE ( ( 0.9330127018922194093, 0.9330127018922221849, 1.000000000000000000, 0.8660254037844387076, 1.000000000000000000, 0.8660254037844387076, 1.000000000000000000, 0.9330127018922207416, 0.9330127018922192983 ) ) 
 REPRESENTATION_ITEM ( '' )  );
#161388 = CARTESIAN_POINT ( 'NONE',  ( -1.364683531250000748, 2.071875000341422357, 1.214306433183764966E-14 ) ) ;
#161389 = CARTESIAN_POINT ( 'NONE',  ( 4.065465959251388206, 5.836405933916976707, -1.599625672291269396 ) ) ;
#161390 = CARTESIAN_POINT ( 'NONE',  ( 5.300874872818830852, 7.207439989753867238, 1.443375672974062551 ) ) ;
#161391 = CARTESIAN_POINT ( 'NONE',  ( 4.352125359537689420, -0.8347222424532302343, 2.004499096949263759 ) ) ;
#161393 = CARTESIAN_POINT ( 'NONE',  ( 4.106863108761789505, -0.3106082297497716471, 1.814695527881895476 ) ) ;
#161392 = CARTESIAN_POINT ( 'NONE',  ( -3.090895834235680262, 5.589500325708124606, 1.082531754730560403 ) ) ;
#161395 = CARTESIAN_POINT ( 'NONE',  ( 6.620655732516649294, 4.703748234811334861, 2.289014941052476715 ) ) ;
#161394 = CARTESIAN_POINT ( 'NONE',  ( -1.001543065824772872E-14, 5.571875000341416140, 1.575800808251672791 ) ) ;
#161396 = CARTESIAN_POINT ( 'NONE',  ( 5.653911837654605144, 0.8871495062587383407, 2.004161502255866090 ) ) ;
#161397 = CARTESIAN_POINT ( 'NONE',  ( 6.776370306708061619, -7.161464053357560644, 6.781144757626056396 ) ) ;
#161398 = CARTESIAN_POINT ( 'NONE',  ( 5.823173511171203742, -0.06224829877122214916, 2.261828766561886361 ) ) ;
#161399 = ORIENTED_EDGE ( 'NONE', *, *, #122422, .T. ) ;
#161400 = CARTESIAN_POINT ( 'NONE',  ( -3.985535776513723150, 7.835598525918981316, 0.2247789072947203870 ) ) ;
#161401 = CARTESIAN_POINT ( 'NONE',  ( 5.214490215732396017, 7.828485850976955263, 1.269369371331245500 ) ) ;
#161402 = CARTESIAN_POINT ( 'NONE',  ( -4.733205024502264102, 7.575804057677677505, 1.082531754730549967 ) ) ;
#161403 = CARTESIAN_POINT ( 'NONE',  ( 5.072158865288245444, 5.090142562357324429, 0.7216878364870338292 ) ) ;
#161404 = CARTESIAN_POINT ( 'NONE',  ( 0.7953275966026486232, -0.6425790844533132429, 1.649264876520744272 ) ) ;
#161405 = CARTESIAN_POINT ( 'NONE',  ( 5.338544149128367167, 1.197215095128815632, -1.618272059301849586 ) ) ;
#161406 = CARTESIAN_POINT ( 'NONE',  ( 7.142447996300871793, 7.227277505306155092, 0.7998128361456341429 ) ) ;
#161407 = CARTESIAN_POINT ( 'NONE',  ( 4.032330418399681093, 1.128390736420165519, -1.777953997047557744 ) ) ;
#161408 = CARTESIAN_POINT ( 'NONE',  ( 1.862754361789496160, -0.09592165986596230820, -1.913344494172765753 ) ) ;
#161409 = CARTESIAN_POINT ( 'NONE',  ( 3.684065054611349144, 5.321161868511784299, -1.599625672291262513 ) ) ;
#161410 = CARTESIAN_POINT ( 'NONE',  ( 2.717198260794476017, -1.712298780928861008, -0.9731099088599747260 ) ) ;
#161411 = CARTESIAN_POINT ( 'NONE',  ( 4.992447118679333329, -1.118567257517719460, 1.681552772592603384 ) ) ;
#161412 = CARTESIAN_POINT ( 'NONE',  ( 1.129532124359374334, -1.183843481993757774, -1.448407549327054955 ) ) ;
#161415 = ORIENTED_EDGE ( 'NONE', *, *, #62562, .T. ) ;
#161414 = CARTESIAN_POINT ( 'NONE',  ( 1.072351618572921605, 0.7776387867773439933, 1.747342548420704800 ) ) ;
#161413 = CARTESIAN_POINT ( 'NONE',  ( 5.443894040360703457, 0.6935754108010495633, -1.579493244201269908 ) ) ;
#161417 = CARTESIAN_POINT ( 'NONE',  ( 3.551873057100283226, 6.127307085716883428, 1.082531754730558626 ) ) ;
#161416 = CARTESIAN_POINT ( 'NONE',  ( 1.418904949497600487, 1.480075412272121582, -1.637148382315711359 ) ) ;
#161418 = CIRCLE ( 'NONE', #189074, 0.08000000000000041800 ) ;
#161419 = CARTESIAN_POINT ( 'NONE',  ( 0.6823417656249882723, 2.238541667008084435, -1.181850606188749264 ) ) ;
#161420 = CARTESIAN_POINT ( 'NONE',  ( 7.391166297744269365, 11.77477778067701664, 1.040834085586084257E-14 ) ) ;
#161421 = CARTESIAN_POINT ( 'NONE',  ( 11.41381675112453031, 12.69999999999999929, -3.704697986577182078 ) ) ;
#161422 =( NAMED_UNIT ( * ) PLANE_ANGLE_UNIT ( ) SI_UNIT ( $, .RADIAN. ) );
#161423 = DIRECTION ( 'NONE',  ( 0.000000000000000000, -1.000000000000000000, 0.000000000000000000 ) ) ;
#161424 = CARTESIAN_POINT ( 'NONE',  ( 6.332887962430945983, -1.963924782908726296, -0.6550794379977520343 ) ) ;
#161425 = CARTESIAN_POINT ( 'NONE',  ( 0.9595327444568906294, 1.691550050060253829, 1.193477315110213599 ) ) ;
#161426 = CARTESIAN_POINT ( 'NONE',  ( -1.500000000000013101, 2.129166666666693519, -0.8660254037844313801 ) ) ;
#161427 = CARTESIAN_POINT ( 'NONE',  ( 6.471319392424407901, 6.444294134116939077, 0.7998128361456341429 ) ) ;
#161428 = CARTESIAN_POINT ( 'NONE',  ( -8.389798128758148010, 8.682519326506312751, 0.7998128361456462443 ) ) ;
#161429 = CARTESIAN_POINT ( 'NONE',  ( 6.052789233858158369, 6.026285292448116948, 0.000000000000000000 ) ) ;
#161430 = CARTESIAN_POINT ( 'NONE',  ( 5.110073233524446756, -0.7627883623938614965, 1.978724553277847464 ) ) ;
#161431 = CARTESIAN_POINT ( 'NONE',  ( -2.788906526875773208E-15, 10.46875000068279604, -1.499999999999998446 ) ) ;
#161432 = EDGE_CURVE ( 'NONE', #105963, #82863, #32012, .T. ) ;
#161433 = CARTESIAN_POINT ( 'NONE',  ( 1.364683531249988757, 2.134375000341422357, 1.214306433183764966E-14 ) ) ;
#161434 = AXIS2_PLACEMENT_3D ( 'NONE', #67205, #177000, #199346 ) ;
#161435 = CARTESIAN_POINT ( 'NONE',  ( 1.499999999999989120, 3.275000000000020783, 1.214306433183764966E-14 ) ) ;
#161437 = CARTESIAN_POINT ( 'NONE',  ( 3.708318708537623021, 4.285125567170706695, -1.199719254218446718 ) ) ;
#161436 = CARTESIAN_POINT ( 'NONE',  ( 1.474414414893455261, 7.826756755319739689, 10.64843978026285320 ) ) ;
#161438 = CARTESIAN_POINT ( 'NONE',  ( 3.884138610457484653, -0.1511163893381066714, 2.010518618204664154 ) ) ;
#161439 = CARTESIAN_POINT ( 'NONE',  ( 5.155460239800898847, 1.844409812803897264, -0.5174689040137578910 ) ) ;
#161440 =( LENGTH_UNIT ( ) NAMED_UNIT ( * ) SI_UNIT ( .MILLI., .METRE. ) );
#161441 = CARTESIAN_POINT ( 'NONE',  ( 2.314256413632868714, 1.428969747754246233, -1.661726224907192684 ) ) ;
#161442 = FACE_OUTER_BOUND ( 'NONE', #150346, .T. ) ;
#161443 = CARTESIAN_POINT ( 'NONE',  ( 0.7499999999999885647, 0.2645833340161538039, 1.299038105676657340 ) ) ;
#161444 = CARTESIAN_POINT ( 'NONE',  ( 5.097907127711155617, 1.355137859109056819, 1.488956579698009763 ) ) ;
#161445 = CARTESIAN_POINT ( 'NONE',  ( -6.287230548435221777, 8.358188277972981695, -1.599625672291263179 ) ) ;
#161446 = ADVANCED_FACE ( 'NONE', ( #181441 ), #50385, .F. ) ;
#161448 = CARTESIAN_POINT ( 'NONE',  ( 5.888306048034124274, -0.7624388358357903073, -1.975341773770035614 ) ) ;
#161447 = CARTESIAN_POINT ( 'NONE',  ( -3.795919822146289313, 5.451659097302528068, -1.443375672974053447 ) ) ;
#161449 = SURFACE_SIDE_STYLE ('',( #199229 ) ) ;
#161451 = CARTESIAN_POINT ( 'NONE',  ( -5.420227550413282636, 9.545625585449309725, 0.7998128361456291469 ) ) ;
#161450 = CARTESIAN_POINT ( 'NONE',  ( 3.052369502041663019, -1.581437162565798804, 1.367655637459828544 ) ) ;
#161453 = ORIENTED_EDGE ( 'NONE', *, *, #47479, .T. ) ;
#161452 = CARTESIAN_POINT ( 'NONE',  ( 1.377515174558477273, 1.023066641755419282, 1.388426169202553018 ) ) ;
#161454 = CARTESIAN_POINT ( 'NONE',  ( 5.467072749063267345, -1.670387955228332277, 1.306269166133758208 ) ) ;
#161455 = CARTESIAN_POINT ( 'NONE',  ( 6.257251587906815793, 7.258880593101466161, 1.199719254218462483 ) ) ;
#161456 = FILL_AREA_STYLE_COLOUR ( '', #175175 ) ;
#161457 = CARTESIAN_POINT ( 'NONE',  ( 1.224999999999958789, 0.8541666666667161456, 0.7072540797572558491 ) ) ;
#161458 = CARTESIAN_POINT ( 'NONE',  ( -7.253312916980337199, -6.796015482748900105, -7.253312916980295455 ) ) ;
#161459 = CARTESIAN_POINT ( 'NONE',  ( 5.795220594837462436, 8.848508896363995291, -1.199719254218440723 ) ) ;
#161460 = ORIENTED_EDGE ( 'NONE', *, *, #14059, .T. ) ;
#161461 = CARTESIAN_POINT ( 'NONE',  ( -11.84103413958613160, 13.61004478473142676, -1.443924719788764799 ) ) ;
#161463 = CARTESIAN_POINT ( 'NONE',  ( 1.963241191952873388, -1.455257657876586341, -1.078514734469406600 ) ) ;
#161462 = CARTESIAN_POINT ( 'NONE',  ( 4.179656494762836516, 8.098292687190454586, -0.7998128361456362523 ) ) ;
#161464 = CARTESIAN_POINT ( 'NONE',  ( -7.393273838153706201, 7.519907654134449615, 0.7998128361456341429 ) ) ;
#161465 = EDGE_LOOP ( 'NONE', ( #52215, #76987, #128520, #49289, #25878 ) ) ;
#161466 = CARTESIAN_POINT ( 'NONE',  ( 2.869522067586683711, 6.499526178826442013, 0.7998128361456362523 ) ) ;
#161467 = ORIENTED_EDGE ( 'NONE', *, *, #68466, .F. ) ;
#161468 = CARTESIAN_POINT ( 'NONE',  ( 6.225128807330042591, 7.291680359087043151, -1.199719254218452047 ) ) ;
#161469 = CARTESIAN_POINT ( 'NONE',  ( 2.350024359177401490, 0.8526225883829393615, -1.598239438867412820 ) ) ;
#161470 = CARTESIAN_POINT ( 'NONE',  ( 6.539320575229228716, 1.281788455817688188, 2.013036689384885225 ) ) ;
#161471 = CARTESIAN_POINT ( 'NONE',  ( -3.104453987849326690, 4.644948957289396496, 1.040834085586084257E-14 ) ) ;
#161472 = CARTESIAN_POINT ( 'NONE',  ( 4.078835981324096416, 7.487686104445945290, 0.5747339805607706298 ) ) ;
#161473 = ORIENTED_EDGE ( 'NONE', *, *, #162808, .T. ) ;
#161474 = EDGE_CURVE ( 'NONE', #12264, #67678, #147900, .T. ) ;
#161475 = CARTESIAN_POINT ( 'NONE',  ( 3.754231824312683763, -1.858861104869345082, -0.09317703841194531489 ) ) ;
#161476 = CARTESIAN_POINT ( 'NONE',  ( 1.071739250477701466, -0.8599075215434035524, 1.711803488807943197 ) ) ;
#161477 = CARTESIAN_POINT ( 'NONE',  ( 6.071306304379397112, 0.1413743337459697769, -1.921272325444240980 ) ) ;
#161478 = CARTESIAN_POINT ( 'NONE',  ( 1.364643601765283432, 4.015812731716659201, 0.6238217115099053967 ) ) ;
#161479 = CARTESIAN_POINT ( 'NONE',  ( -3.059665831784952651E-14, 3.479999999999999538, 2.000000000000000000 ) ) ;
#161480 = EDGE_CURVE ( 'NONE', #99811, #193311, #186930, .T. ) ;
#161481 = CARTESIAN_POINT ( 'NONE',  ( 0.6124999999999776179, 1.479166667349464337, -1.060881119635962211 ) ) ;
#161482 = DIRECTION ( 'NONE',  ( -5.176899690512889973E-31, 0.6004703560067813362, 0.7996470168499908437 ) ) ;
#161483 = FACE_OUTER_BOUND ( 'NONE', #41063, .T. ) ;
#161484 = CARTESIAN_POINT ( 'NONE',  ( 6.968527767744093993, 10.11340424813470662, 1.082531754730558626 ) ) ;
#161485 = CARTESIAN_POINT ( 'NONE',  ( 5.910992199152527604, -1.554775717584104378, 1.208803697826433599 ) ) ;
#161486 = CARTESIAN_POINT ( 'NONE',  ( -4.928552533767591726, 5.708731696605642725, 1.199719254218462483 ) ) ;
#161487 = CARTESIAN_POINT ( 'NONE',  ( 4.997242633387394051, 4.932463948481133897, -0.4367601086738909233 ) ) ;
#161488 = CARTESIAN_POINT ( 'NONE',  ( 0.3399330434069799400, 2.085199349320911555, 0.1515528320938461238 ) ) ;
#161489 = CARTESIAN_POINT ( 'NONE',  ( 5.790048612033079856, -0.8660258810785811390, 1.720834695440204509 ) ) ;
#161490 = CARTESIAN_POINT ( 'NONE',  ( -5.696397096036042385, 9.797547045350714967, -0.7998128361456231517 ) ) ;
#161491 = CARTESIAN_POINT ( 'NONE',  ( 1.149113351018778539, -1.436424422225426767, -1.126575773451453433 ) ) ;
#161492 = CARTESIAN_POINT ( 'NONE',  ( 1.770444396619451632, 1.136427050704125419, 1.891651738277564831 ) ) ;
#161493 = DIRECTION ( 'NONE',  ( 1.000000000000000000, 0.000000000000000000, 0.000000000000000000 ) ) ;
#161494 = CARTESIAN_POINT ( 'NONE',  ( 0.1231139863388103495, 1.664874722635242277, 0.9407772870168448209 ) ) ;
#161495 = ORIENTED_EDGE ( 'NONE', *, *, #17156, .T. ) ;
#161496 = CARTESIAN_POINT ( 'NONE',  ( 0.9593497616274889728, 1.608103478905052119, 1.136861374779022604 ) ) ;
#161497 = CARTESIAN_POINT ( 'NONE',  ( 1.294366139777222369, 1.586748096885544745, -1.119478687268110173 ) ) ;
#161498 = VECTOR ( 'NONE', #42641, 1000.000000000000114 ) ;
#161499 = CARTESIAN_POINT ( 'NONE',  ( 0.3333609138582178111, -1.319029705771988858, 1.524807370920200356 ) ) ;
#161501 = CARTESIAN_POINT ( 'NONE',  ( 5.049569799528213387, 1.377159375265882391, 1.251766951177714526 ) ) ;
#161500 = CARTESIAN_POINT ( 'NONE',  ( -5.498713818794216834, 8.572860667638675380, -1.199719254218452047 ) ) ;
#161502 = CARTESIAN_POINT ( 'NONE',  ( 5.037736595929563244, 8.035053907629919223, -1.199719254218452047 ) ) ;
#161503 = CARTESIAN_POINT ( 'NONE',  ( -2.723004532691724489, 3.009022671084740974, 2.500000000000000444 ) ) ;
#161504 = DIRECTION ( 'NONE',  ( -0.000000000000000000, -1.000000000000000000, -0.000000000000000000 ) ) ;
#161505 = CARTESIAN_POINT ( 'NONE',  ( -6.254388934605767503, 6.191208599995166040, 0.7998128361456341429 ) ) ;
#161506 = CARTESIAN_POINT ( 'NONE',  ( -5.749539660647037032, 8.865490816466966351, 1.199719254218454489 ) ) ;
#161507 = CARTESIAN_POINT ( 'NONE',  ( 1.523247060345904291, -2.062048068855956373, 0.7425582295156886170 ) ) ;
#161508 = CARTESIAN_POINT ( 'NONE',  ( 3.877268743828270470, 5.546566172598190292, 1.443375672974062551 ) ) ;
#161509 = CARTESIAN_POINT ( 'NONE',  ( 7.095713291905693332, 9.371694488680407886, 1.599625672291268286 ) ) ;
#161510 = DIRECTION ( 'NONE',  ( 0.000000000000000000, 1.000000000000000000, 0.000000000000000000 ) ) ;
#161511 = CARTESIAN_POINT ( 'NONE',  ( 1.576486190600217663, -1.733098801405801304, -0.5742540608338757568 ) ) ;
#161512 = CARTESIAN_POINT ( 'NONE',  ( 0.4867935908802952238, 7.427453578140642776, 4.536604770850393820 ) ) ;
#161513 = CARTESIAN_POINT ( 'NONE',  ( -4.090809663021341969, 5.795697244990093644, 1.599625672291267398 ) ) ;
#161514 = CARTESIAN_POINT ( 'NONE',  ( -6.423891471114925977, 6.884501071190606503, -0.7550301924055674574 ) ) ;
#161515 = CARTESIAN_POINT ( 'NONE',  ( 6.509000000000034092, 7.052765612591089806, 2.598154238703707541 ) ) ;
#161516 = CARTESIAN_POINT ( 'NONE',  ( 10.37606763316019531, 10.99983374830873650, 0.7998128361456462443 ) ) ;
#161517 = CARTESIAN_POINT ( 'NONE',  ( 0.7680398806059639538, 0.9487340639210088966, 1.676631345724951982 ) ) ;
#161518 = CARTESIAN_POINT ( 'NONE',  ( 5.260583753728677259, -0.6573284944802314511, -1.848511375219172415 ) ) ;
#161519 = CARTESIAN_POINT ( 'NONE',  ( -6.353967546298838087, 10.56471257065732416, 0.000000000000000000 ) ) ;
#161520 = CARTESIAN_POINT ( 'NONE',  ( 5.443762371086860341, 6.309809840144842141, 1.199719254218462483 ) ) ;
#161521 = CARTESIAN_POINT ( 'NONE',  ( 4.669572502782517454, 1.262004115398765780, 1.791526714441132873 ) ) ;
#161522 = CIRCLE ( 'NONE', #68077, 0.1999999999999998723 ) ;
#161523 = CARTESIAN_POINT ( 'NONE',  ( 3.847109862837357230, 4.045599327266925727, -0.8077998227820462063 ) ) ;
#161524 = CARTESIAN_POINT ( 'NONE',  ( 3.889561532384704368, -1.914723906051108537, 0.7877538119766481772 ) ) ;
#161526 = CARTESIAN_POINT ( 'NONE',  ( 1.364683531249986537, 0.9260416670080896528, 0.7879004041258500513 ) ) ;
#161525 = CARTESIAN_POINT ( 'NONE',  ( 8.730309718301390021, 13.52954257607862942, 8.166533740197252200 ) ) ;
#161527 = ORIENTED_EDGE ( 'NONE', *, *, #12290, .F. ) ;
#161528 = CARTESIAN_POINT ( 'NONE',  ( 4.008600857689972763, -2.199693827605917917, 0.6672659128543911855 ) ) ;
#161530 = ORIENTED_EDGE ( 'NONE', *, *, #121592, .T. ) ;
#161529 = CARTESIAN_POINT ( 'NONE',  ( 7.998947442382716488, 9.394822106610419610, -1.082531754730543083 ) ) ;
#161531 = CARTESIAN_POINT ( 'NONE',  ( 6.699137298928158124, 6.988284068270579574, 0.7216878364870328300 ) ) ;
#161532 = CARTESIAN_POINT ( 'NONE',  ( -7.524604700374180055, -5.166862990899345753, -8.024185963717888725 ) ) ;
#161533 = CARTESIAN_POINT ( 'NONE',  ( 4.312401332534675724, 1.776009277829879718, 0.7858599780834804038 ) ) ;
#161534 = ORIENTED_EDGE ( 'NONE', *, *, #188635, .T. ) ;
#161535 = CARTESIAN_POINT ( 'NONE',  ( 5.680503174445848735, 5.729601246382692636, 1.040834085586084257E-14 ) ) ;
#161536 = ORIENTED_EDGE ( 'NONE', *, *, #31789, .T. ) ;
#161537 = CARTESIAN_POINT ( 'NONE',  ( 5.133030909251353968, 1.769313487831367659, 0.7262901588861517821 ) ) ;
#161538 =( NAMED_UNIT ( * ) PLANE_ANGLE_UNIT ( ) SI_UNIT ( $, .RADIAN. ) );
#161539 = CARTESIAN_POINT ( 'NONE',  ( 6.774431772926147843, -1.055741295204252195, 1.364281925921766447 ) ) ;
#161540 = CARTESIAN_POINT ( 'NONE',  ( 4.206267736153862735, 1.236801365491456028, -1.592660703826812352 ) ) ;
#161541 = CARTESIAN_POINT ( 'NONE',  ( 11.52460864928264783, 12.21999999999998110, 3.346683403123522638 ) ) ;
#161542 = CARTESIAN_POINT ( 'NONE',  ( 1.295869073816724226, 1.673045085319382119, 1.439284050222865652 ) ) ;
#161544 = CARTESIAN_POINT ( 'NONE',  ( -5.343321937561608337, 5.406499480009534508, 0.7216878364870257245 ) ) ;
#161543 = CARTESIAN_POINT ( 'NONE',  ( -9.642873567817536795, 12.27310513391906532, 1.599625672291281386 ) ) ;
#161546 = CARTESIAN_POINT ( 'NONE',  ( 6.450471989241519211, 0.5578098333037047052, 1.679625245746432016 ) ) ;
#161545 = CARTESIAN_POINT ( 'NONE',  ( 1.341864181646670540, 2.088322648670298598, 0.1009416716012418447 ) ) ;
#161547 = CARTESIAN_POINT ( 'NONE',  ( 5.678361341766085424, 1.528739221709461082, 1.314999087022615587 ) ) ;
#161549 = CARTESIAN_POINT ( 'NONE',  ( 2.572590238467100665, -2.194022629849821104, -0.6638836622538509813 ) ) ;
#161548 = CARTESIAN_POINT ( 'NONE',  ( 5.737035277238070385, 6.722237907313067140, -1.199719254218452047 ) ) ;
#161550 = CARTESIAN_POINT ( 'NONE',  ( 0.7963321702096434196, 1.420339700582837539, 1.005379078535458159 ) ) ;
#161551 = DIRECTION ( 'NONE',  ( 5.578564026256504688E-16, 1.000000000000000000, 9.066213480720158442E-32 ) ) ;
#161552 = CARTESIAN_POINT ( 'NONE',  ( 0.9832555119714074809, 1.599142458273569600, 0.6705785602827417646 ) ) ;
#161553 = CARTESIAN_POINT ( 'NONE',  ( 1.360316468749971364, 0.04687500034143698979, -3.469446951953614189E-14 ) ) ;
#161554 = CARTESIAN_POINT ( 'NONE',  ( -0.4254946254914159787, 3.044090126848159716, 0.4192457809233481880 ) ) ;
#161555 = CARTESIAN_POINT ( 'NONE',  ( 1.803425971091272340, -1.834736872252432649, 1.160642024321426380 ) ) ;
#161556 = CARTESIAN_POINT ( 'NONE',  ( 2.747280062631300535, 0.2910806042949847239, -1.995268371848608835 ) ) ;
#161558 = CIRCLE ( 'NONE', #67955, 0.07999999999999998779 ) ;
#161557 = CARTESIAN_POINT ( 'NONE',  ( 4.812500000000003553, 1.451031289061308183, 1.451031289060921159 ) ) ;
#161559 = CARTESIAN_POINT ( 'NONE',  ( 1.499999999999987121, 1.035416667349484232, 0.8660254037844524744 ) ) ;
#161560 = CARTESIAN_POINT ( 'NONE',  ( 6.111935756226617222, -1.911612718183410387, 0.2385651428990897549 ) ) ;
#161561 = CARTESIAN_POINT ( 'NONE',  ( 1.364683531249997417, 12.98437500034139980, 2.602085213965210642E-15 ) ) ;
#161562 = CARTESIAN_POINT ( 'NONE',  ( 3.375417215397161552, -1.960608319544883793, -1.044296844735680185 ) ) ;
#161563 = EDGE_LOOP ( 'NONE', ( #99870, #102102, #19502, #153193 ) ) ;
#161564 = PLANE ( 'NONE',  #22158 ) ;
#161565 = SURFACE_STYLE_USAGE ( .BOTH. , #31559 ) ;
#161566 = CARTESIAN_POINT ( 'NONE',  ( 7.727257484784855635, 11.10255193463598111, -1.199719254218446718 ) ) ;
#161567 = CARTESIAN_POINT ( 'NONE',  ( 1.364683531249986981, -1.115624999658580752, 0.000000000000000000 ) ) ;
#161568 = CARTESIAN_POINT ( 'NONE',  ( 5.952664183270127474, -1.497414089959566930, -0.8868285315999470120 ) ) ;
#161571 = EDGE_CURVE ( 'NONE', #22501, #136572, #19476, .T. ) ;
#161570 = CARTESIAN_POINT ( 'NONE',  ( 3.894932841003693191, 0.2855096342280309396, 1.940843471192068792 ) ) ;
#161569 = PRESENTATION_LAYER_ASSIGNMENT (  '', '', ( #64742 ) ) ;
#161573 = CARTESIAN_POINT ( 'NONE',  ( -5.748293942514172805, 8.689798118699771479, -1.082531754730538864 ) ) ;
#161572 = CARTESIAN_POINT ( 'NONE',  ( 4.383363735919856730, 4.008345868194933104, -0.7998128361456211532 ) ) ;
#161574 = CARTESIAN_POINT ( 'NONE',  ( -1.318127287744123688, 4.161901352009867772, 0.3960634941688782606 ) ) ;
#161575 = CARTESIAN_POINT ( 'NONE',  ( 4.200629628819559258, -0.7044727654359562719, -2.150022973637927048 ) ) ;
#161576 = CARTESIAN_POINT ( 'NONE',  ( 1.732955346664406537, -1.957976925384408817, -0.6489628464096306448 ) ) ;
#161577 = CARTESIAN_POINT ( 'NONE',  ( -7.206322340863467346, 8.366129804884193888, 1.199719254218450271 ) ) ;
#161578 = CARTESIAN_POINT ( 'NONE',  ( 2.061739773175938595, 0.3863463398323406794, -2.229145236428681454 ) ) ;
#161579 = ORIENTED_EDGE ( 'NONE', *, *, #114249, .F. ) ;
#161580 = CARTESIAN_POINT ( 'NONE',  ( -0.7500000000000215383, 1.722916667349486008, 1.299038105676659116 ) ) ;
#161581 = CARTESIAN_POINT ( 'NONE',  ( 3.743291833738107144, -1.414529149469236691, -1.224010458943748603 ) ) ;
#161582 = CARTESIAN_POINT ( 'NONE',  ( 2.267823513004694647, 1.585025364652093760, -0.7039959249812016706 ) ) ;
#161583 = CARTESIAN_POINT ( 'NONE',  ( 6.462441986028243157, -2.002789442531027309, -0.8901952361822995652 ) ) ;
#161584 = CARTESIAN_POINT ( 'NONE',  ( 0.3939699847536023980, 1.636818068892214040, 1.480257586202008646 ) ) ;
#161585 = CARTESIAN_POINT ( 'NONE',  ( 4.083022661009271914, -0.2092679848491978134, -2.151539631373246220 ) ) ;
#161586 = CARTESIAN_POINT ( 'NONE',  ( 5.068278781427039803, -1.829183178514147690, -0.6524800764661740082 ) ) ;
#161587 = COLOUR_RGB ( '', 0.08235294, 0.09019608, 0.10196078) ;
#161588 = CARTESIAN_POINT ( 'NONE',  ( -2.290964770585000920, 5.616616632417037458, -0.7216878364870257245 ) ) ;
#161589 = CARTESIAN_POINT ( 'NONE',  ( 6.872336254976083580, -1.150436037642876608, 1.475500831757702747 ) ) ;
#161590 = CARTESIAN_POINT ( 'NONE',  ( 4.067670533747345551, 7.502496534258641603, 0.5382987142239087364 ) ) ;
#161591 = FACE_OUTER_BOUND ( 'NONE', #79267, .T. ) ;
#161592 = EDGE_CURVE ( 'NONE', #95302, #126635, #654, .T. ) ;
#161593 = CARTESIAN_POINT ( 'NONE',  ( -0.6801582343750004478, 2.598958333674746157, -1.178068619123848526 ) ) ;
#161594 = CARTESIAN_POINT ( 'NONE',  ( 5.238907797441370029, 2.013986022392059816, -0.1017483359899013229 ) ) ;
#161595 = CARTESIAN_POINT ( 'NONE',  ( -8.319899820280397762, 12.85830022363583147, -0.7998128361456281477 ) ) ;
#161596 = CARTESIAN_POINT ( 'NONE',  ( 7.446452682403650769, 9.710614100936176385, -1.599625672291262513 ) ) ;
#161597 = CARTESIAN_POINT ( 'NONE',  ( 3.902768115887398803, 5.646591783325653147, -1.599625672291269396 ) ) ;
#161598 = CARTESIAN_POINT ( 'NONE',  ( 2.701551412915685457, -0.5726843992823158480, 1.733614832724015731 ) ) ;
#161599 = CARTESIAN_POINT ( 'NONE',  ( 1.923171073188837843, 2.059116738528983692, 0.7940920450543451636 ) ) ;
#161600 = EDGE_LOOP ( 'NONE', ( #99205, #6592, #9476, #82280 ) ) ;
#161601 = CARTESIAN_POINT ( 'NONE',  ( -5.329763783503577379, 6.351050847909847086, 1.082531754730549078 ) ) ;
#161602 = UNCERTAINTY_MEASURE_WITH_UNIT (LENGTH_MEASURE( 1.000000000000000082E-05 ), #201277, 'distance_accuracy_value', 'NONE');
#161603 = CARTESIAN_POINT ( 'NONE',  ( -3.285556943749998737, -4.017708332855375986, 1.896917185911908499 ) ) ;
#161604 = CARTESIAN_POINT ( 'NONE',  ( -7.914208982075130905, 10.25632978388623684, -1.599625672291263179 ) ) ;
#161605 = CARTESIAN_POINT ( 'NONE',  ( 1.265885189609064376, 0.5823756177252036315, -1.934031124627869414 ) ) ;
#161606 = CARTESIAN_POINT ( 'NONE',  ( 1.576976220782677185, -1.497206391897941913, 1.501870991332490135 ) ) ;
#161607 = CARTESIAN_POINT ( 'NONE',  ( -4.610654757099099221, 7.536791762327691657, 1.199719254218452935 ) ) ;
#161608 = CARTESIAN_POINT ( 'NONE',  ( 1.604125426503384411, 1.858527726531463697, 0.09786615749988146484 ) ) ;
#161609 = CARTESIAN_POINT ( 'NONE',  ( 4.325214697959421706, 5.004837554829479451, 1.199719254218462483 ) ) ;
#161610 = CARTESIAN_POINT ( 'NONE',  ( 6.614142728931415860, -0.9689641062460941923, -1.818880834187324824 ) ) ;
#161611 = CARTESIAN_POINT ( 'NONE',  ( 6.451795992440088057, -1.844709169062180409, -0.8146298745319994206 ) ) ;
#161612 = VERTEX_POINT ( 'NONE', #1596 ) ;
#161613 = EDGE_LOOP ( 'NONE', ( #180528, #83258, #91703, #36212 ) ) ;
#161614 = CARTESIAN_POINT ( 'NONE',  ( -10.32183501870554387, 10.93656236477829502, 0.7998128361456462443 ) ) ;
#161615 = CARTESIAN_POINT ( 'NONE',  ( 4.019992336727182369, -0.9402185374879183932, -1.564826772493657536 ) ) ;
#161617 = CARTESIAN_POINT ( 'NONE',  ( -5.927203485463973465, 6.129067544638190590, -0.8144944673919730649 ) ) ;
#161616 = CARTESIAN_POINT ( 'NONE',  ( -5.842637852846353397, 5.781108681267656202, 0.7998128361456281477 ) ) ;
#161618 = CARTESIAN_POINT ( 'NONE',  ( 6.548892101489681927, 6.803534504848940401, 0.4251794856353352525 ) ) ;
#161619 = CARTESIAN_POINT ( 'NONE',  ( 6.432970213454214381, 1.034009579150240610, 1.730599625746793935 ) ) ;
#161620 = CARTESIAN_POINT ( 'NONE',  ( 5.472543265827003012, -0.04911201564661467345, -1.840652735559132669 ) ) ;
#161621 = CARTESIAN_POINT ( 'NONE',  ( 0.07680821025393690105, 0.005952109439256307241, -1.810863387344714193 ) ) ;
#161622 = CARTESIAN_POINT ( 'NONE',  ( 3.510674805948321264, -0.9346715503392712954, -2.110115307156499753 ) ) ;
#161623 = CARTESIAN_POINT ( 'NONE',  ( 6.313256805818848960, 7.394496357324014113, 1.199719254218452047 ) ) ;
#161624 = CARTESIAN_POINT ( 'NONE',  ( 5.800121417639972243, -2.161773191644947634, -0.006422599366645573467 ) ) ;
#161625 = CARTESIAN_POINT ( 'NONE',  ( 7.091078035147269532, 8.231678114882006625, 1.199719254218462483 ) ) ;
#161626 = CARTESIAN_POINT ( 'NONE',  ( 1.153739077726954498, 0.7885942357991974072, 1.774928408438203098 ) ) ;
#161627 = ORIENTED_EDGE ( 'NONE', *, *, #189888, .T. ) ;
#161628 = CARTESIAN_POINT ( 'NONE',  ( 4.183220704542046420, -1.177475575078859027, -1.973740397952013836 ) ) ;
#161629 = CARTESIAN_POINT ( 'NONE',  ( -2.788906526875773208E-15, 9.187500000000001776, -1.499999999999998446 ) ) ;
#161630 = CARTESIAN_POINT ( 'NONE',  ( -6.237633190739009237, 9.434933268240943249, 1.199719254218452047 ) ) ;
#161631 = CARTESIAN_POINT ( 'NONE',  ( 4.680451076648031616, -1.814532364864028136, -0.4542276060127621862 ) ) ;
#161632 = ORIENTED_EDGE ( 'NONE', *, *, #90176, .T. ) ;
#161635 = CARTESIAN_POINT ( 'NONE',  ( -5.529746549527323474, 7.544733289238903851, -1.599625672291271394 ) ) ;
#161634 = CARTESIAN_POINT ( 'NONE',  ( 1.499999999999987121, 0.03541666734948738238, 0.8660254037844524744 ) ) ;
#161633 = CARTESIAN_POINT ( 'NONE',  ( 2.162237915172473546, 1.912057200688283665, 0.04323261116381121871 ) ) ;
#161636 = CARTESIAN_POINT ( 'NONE',  ( 4.266400587755204477, 1.039063272370500668, 1.946970035688735390 ) ) ;
#161637 = CARTESIAN_POINT ( 'NONE',  ( 6.983263157960410972, 2.978556228996271482, 2.299637001123565838 ) ) ;
#161638 = CARTESIAN_POINT ( 'NONE',  ( 4.054051625686104998, 4.688480637177271149, -1.199719254218446718 ) ) ;
#161639 = CARTESIAN_POINT ( 'NONE',  ( 5.329763783503544516, 9.232158490813878515, -0.7216878364870458196 ) ) ;
#161640 = CARTESIAN_POINT ( 'NONE',  ( -3.918470089549458635, 4.530302178351167441, -1.199719254218452047 ) ) ;
#161641 = CARTESIAN_POINT ( 'NONE',  ( -5.221298554594238084, 8.145246509451649075, 1.082531754730549967 ) ) ;
#161642 = CARTESIAN_POINT ( 'NONE',  ( 2.073447407941295673, 1.887670557785134928, -0.5683696268203948243 ) ) ;
#161643 = CARTESIAN_POINT ( 'NONE',  ( 0.9038794553481295235, 1.888499008566895787, 1.325839279686758632 ) ) ;
#161644 = CARTESIAN_POINT ( 'NONE',  ( 2.752341281506097470, -1.956419249932477955, -0.1471676765215298721 ) ) ;
#161645 = LINE ( 'NONE', #108675, #19745 ) ;
#161646 = CARTESIAN_POINT ( 'NONE',  ( 5.471554536677815328, -0.3081364425130261320, 2.039334399838355960 ) ) ;
#161647 = CARTESIAN_POINT ( 'NONE',  ( 5.829642864196171281, 5.903597551091405826, 0.7216878364870317197 ) ) ;
#161648 = CARTESIAN_POINT ( 'NONE',  ( 4.878955176071345434, 6.785476686873604280, -1.599625672291269396 ) ) ;
#161649 = ORIENTED_EDGE ( 'NONE', *, *, #17750, .T. ) ;
#161650 = CARTESIAN_POINT ( 'NONE',  ( 1.364683531249990311, 5.676041667008088432, 0.7879004041258500513 ) ) ;
#161651 = CYLINDRICAL_SURFACE ( 'NONE', #93841, 9.999999999999998224 ) ;
#161652 = CARTESIAN_POINT ( 'NONE',  ( 3.836594282542920009, 4.538743420130594508, 1.082531754730560403 ) ) ;
#161654 = MECHANICAL_DESIGN_GEOMETRIC_PRESENTATION_REPRESENTATION (  '', ( #71617 ), #5884 ) ;
#161653 = CARTESIAN_POINT ( 'NONE',  ( 0.7960475122521799562, -1.534068779871503363, -1.536527999751842621 ) ) ;
#161655 = CARTESIAN_POINT ( 'NONE',  ( 4.355912491740495440, 8.303924683664389406, 0.000000000000000000 ) ) ;
#161656 = DIRECTION ( 'NONE',  ( -0.6507913734559658270, -0.7592566023652989049, 0.000000000000000000 ) ) ;
#161657 = CARTESIAN_POINT ( 'NONE',  ( -9.702943487419032564, 4.518467169708416442, -7.062559895321285808 ) ) ;
#161658 = CARTESIAN_POINT ( 'NONE',  ( 2.196370303256788503, -0.4943915968025693330, -1.803980227719769847 ) ) ;
#161659 = CARTESIAN_POINT ( 'NONE',  ( 0.3861014259941424887, -0.9735654513510684227, 1.816333823429964411 ) ) ;
#161661 = CARTESIAN_POINT ( 'NONE',  ( 6.727182134110231360, 2.105158487175392334, 2.022197281440795358 ) ) ;
#161660 = DIRECTION ( 'NONE',  ( 0.000000000000000000, -1.000000000000000000, 0.000000000000000000 ) ) ;
#161662 = CARTESIAN_POINT ( 'NONE',  ( -1.364683531250014514, -0.2197916663252438285, 0.7879004041258379498 ) ) ;
#161663 = CARTESIAN_POINT ( 'NONE',  ( 2.807167725247063483, 1.639017566557477990, -0.9848878580655600068 ) ) ;
#161664 = B_SPLINE_CURVE_WITH_KNOTS ( 'NONE', 3,
 ( #118822, #72125, #184809, #151276, #36438, #204246 ),
 .UNSPECIFIED., .F., .F.,
 ( 4, 2, 4 ),
 ( 0.000000000000000000, 0.0003767643964918265939, 0.0007535287929836531878 ),
 .UNSPECIFIED. ) ;
#161665 = CARTESIAN_POINT ( 'NONE',  ( 3.871743310845751296, 0.9831255770079703193, 1.471438590500689925 ) ) ;
#161666 = CARTESIAN_POINT ( 'NONE',  ( 1.805181101471531546, 1.663141274854248230, -0.9436981260437929953 ) ) ;
#161667 = CARTESIAN_POINT ( 'NONE',  ( -4.934277840369690971, 7.844075682818238526, -1.199719254218452047 ) ) ;
#161669 = CARTESIAN_POINT ( 'NONE',  ( 5.378507874412199463, -0.4701315380702688618, -1.856876755957288516 ) ) ;
#161668 = FILL_AREA_STYLE_COLOUR ( '', #42288 ) ;
#161670 = CARTESIAN_POINT ( 'NONE',  ( -1.500000000000001332, -1.099999999999976108, 0.000000000000000000 ) ) ;
#161671 = CARTESIAN_POINT ( 'NONE',  ( 6.250452387334210158, -1.959941389959872549, -0.1944618805250642457 ) ) ;
#161672 = CARTESIAN_POINT ( 'NONE',  ( 1.499999999999990896, 5.275000000000022560, 1.214306433183764966E-14 ) ) ;
#161673 = CARTESIAN_POINT ( 'NONE',  ( 2.004293344102888508, -0.9022931611136343344, 1.919180038594799687 ) ) ;
#161674 = CARTESIAN_POINT ( 'NONE',  ( 4.873830839387755631, 1.077430855447782942, 1.529020332772989210 ) ) ;
#161676 = ORIENTED_EDGE ( 'NONE', *, *, #166530, .F. ) ;
#161675 = CARTESIAN_POINT ( 'NONE',  ( 1.207329354700342305, -0.4456725867950651621, 1.770335049871730071 ) ) ;
#161678 = CARTESIAN_POINT ( 'NONE',  ( 4.594924845400013780, 8.373833185659544043, 0.04553248676899754321 ) ) ;
#161677 = CARTESIAN_POINT ( 'NONE',  ( 4.301547675229603129, 1.771612934706376707, 1.315755017190944676 ) ) ;
#161679 = CARTESIAN_POINT ( 'NONE',  ( 0.6823417656249864960, -1.073958332991911568, -1.181850606188749264 ) ) ;
#161680 = CARTESIAN_POINT ( 'NONE',  ( 1.398963405728241183, 0.4003750237208941742, 2.023287731994154015 ) ) ;
#161681 = CARTESIAN_POINT ( 'NONE',  ( 6.972971076130050072, 7.029554431773520129, 1.040834085586084257E-14 ) ) ;
#161682 = CARTESIAN_POINT ( 'NONE',  ( -6.842061076390810292, 11.13415502243129218, 0.000000000000000000 ) ) ;
#161683 = CARTESIAN_POINT ( 'NONE',  ( 1.500000000000035971, 8.500000000000000000, 9.886859966642587594 ) ) ;
#161684 = CARTESIAN_POINT ( 'NONE',  ( 1.352846302990980076, 3.447904424298776416, 0.3040853380226353764 ) ) ;
#161685 = PRESENTATION_STYLE_ASSIGNMENT (( #130317 ) ) ;
#161686 = CARTESIAN_POINT ( 'NONE',  ( 5.006703865196457492, 9.063181286029688977, 0.000000000000000000 ) ) ;
#161687 = CIRCLE ( 'NONE', #2526, 0.4999999999999995559 ) ;
#161688 = ORIENTED_EDGE ( 'NONE', *, *, #146265, .T. ) ;
#161689 = CARTESIAN_POINT ( 'NONE',  ( 4.598136200040512378, 0.8882050449813773119, -1.870312673664726644 ) ) ;
#161690 = CARTESIAN_POINT ( 'NONE',  ( -1.364683531250000748, -0.6781249996585803075, 0.000000000000000000 ) ) ;
#161691 = CARTESIAN_POINT ( 'NONE',  ( 2.179201376995115513, -0.1036959380565916772, -2.159207860300814463 ) ) ;
#161692 = CARTESIAN_POINT ( 'NONE',  ( -4.789308618567226006, 8.160042084799258078, 0.7984581689710170682 ) ) ;
#161693 = CARTESIAN_POINT ( 'NONE',  ( 2.719404001658455527, 1.707403962800517316, 1.078498517531191858 ) ) ;
#161694 = CARTESIAN_POINT ( 'NONE',  ( 6.620655732516615544, 2.958939621373418483, 2.526443930770333246 ) ) ;
#161695 = EDGE_CURVE ( 'NONE', #135683, #42950, #131685, .T. ) ;
#161696 = ORIENTED_EDGE ( 'NONE', *, *, #110826, .T. ) ;
#161698 = CARTESIAN_POINT ( 'NONE',  ( 8.120970824905713314, 8.576813505252564696, 1.040834085586084257E-14 ) ) ;
#161697 = CARTESIAN_POINT ( 'NONE',  ( -3.475000000000000533, -2.100000000000000977, 0.000000000000000000 ) ) ;
#161699 = CARTESIAN_POINT ( 'NONE',  ( -4.299344108864961989, 6.109263775132799168, -1.443375672974066548 ) ) ;
#161700 = CARTESIAN_POINT ( 'NONE',  ( 1.604704241733472037, 1.883313803065278513, 0.7212895827233902768 ) ) ;
#161701 = CARTESIAN_POINT ( 'NONE',  ( 5.706613541269077494, 1.932210019790636224, 1.034112652976440394 ) ) ;
#161702 = CARTESIAN_POINT ( 'NONE',  ( 1.499999999999991118, 5.285416667349480235, 0.8660254037844524744 ) ) ;
#161703 = CARTESIAN_POINT ( 'NONE',  ( 4.359561026920276916, -1.481784043772149451, -1.208992945495937610 ) ) ;
#161704 = CARTESIAN_POINT ( 'NONE',  ( -2.916975605234527702, 6.554888639415577423, 1.040834085586084257E-14 ) ) ;
#161705 = EDGE_CURVE ( 'NONE', #31992, #93052, #202837, .T. ) ;
#161706 = CARTESIAN_POINT ( 'NONE',  ( 5.626270559546804328, 9.507806719539201978, 0.7216878364870438212 ) ) ;
#161708 = CARTESIAN_POINT ( 'NONE',  ( 2.161732667986946410, 1.242745142284812365, 1.587824664567152766 ) ) ;
#161707 = CARTESIAN_POINT ( 'NONE',  ( -8.636180661780658241, 12.05899929117736846, -1.082531754730543083 ) ) ;
#161709 = CARTESIAN_POINT ( 'NONE',  ( 0.6823417656249934904, 14.25520833367473195, 1.181850606188764807 ) ) ;
#161710 = CARTESIAN_POINT ( 'NONE',  ( -4.842197138736131556, 5.678260079060780008, 1.199719254218452935 ) ) ;
#161711 = CARTESIAN_POINT ( 'NONE',  ( 5.174679765213248572, -1.625057609515182078, -0.5782863776828560676 ) ) ;
#161712 = CARTESIAN_POINT ( 'NONE',  ( -0.1399997263889559695, 7.629137130509076492, -2.600276787041354343 ) ) ;
#161713 = CARTESIAN_POINT ( 'NONE',  ( 10.05978679165993839, 10.83876546646586014, 0.7216878364870438212 ) ) ;
#161714 = DIRECTION ( 'NONE',  ( 0.000000000000000000, -0.000000000000000000, 1.000000000000000000 ) ) ;
#161715 = CARTESIAN_POINT ( 'NONE',  ( 3.571683402196252910, 6.254382171615883834, 1.199719254218462483 ) ) ;
#161716 = CARTESIAN_POINT ( 'NONE',  ( -2.482948226198895103, 5.072301959192136778, 2.500000000000011102 ) ) ;
#161717 = CARTESIAN_POINT ( 'NONE',  ( 0.8485890540621650047, -2.054197865963180547, -0.2570499307305574299 ) ) ;
#161718 = VERTEX_POINT ( 'NONE', #36246 ) ;
#161719 = CARTESIAN_POINT ( 'NONE',  ( 5.004484103855499910, -1.798449698946352537, -0.2161431223286890690 ) ) ;
#161720 = CARTESIAN_POINT ( 'NONE',  ( 5.716698046817569434, 6.698511138489155137, -1.199719254218452047 ) ) ;
#161721 = CYLINDRICAL_SURFACE ( 'NONE', #69963, 0.07999999999999993228 ) ;
#161722 = CARTESIAN_POINT ( 'NONE',  ( 6.445981706654077215, -1.189238676736432465, -1.366527308926633211 ) ) ;
#161723 = CARTESIAN_POINT ( 'NONE',  ( 6.197485614778188712, 6.403023770095574108, -0.7216878364870458196 ) ) ;
#161724 = CARTESIAN_POINT ( 'NONE',  ( 10.42279406580779444, 10.52049161362584684, -5.955436901484764789 ) ) ;
#161725 = CARTESIAN_POINT ( 'NONE',  ( 3.345827479060593301, 2.191629467292684819, -0.0001215010576177677764 ) ) ;
#161726 = VERTEX_POINT ( 'NONE', #148952 ) ;
#161727 = COLOUR_RGB ( '', 0.66274510, 0.83137255, 0.94901961) ;
#161729 = CARTESIAN_POINT ( 'NONE',  ( 8.432281472695482449, 11.92507992053172572, 1.199719254218450271 ) ) ;
#161728 = CARTESIAN_POINT ( 'NONE',  ( 0.1858947801188018389, -1.204007190563995078, -1.549573762531175625 ) ) ;
#161730 = CARTESIAN_POINT ( 'NONE',  ( 4.446842608676645270, -1.712983832262956696, -0.8575701973691277624 ) ) ;
#161731 = CARTESIAN_POINT ( 'NONE',  ( -1.445103857048104512, 8.688264192037886247, 2.625611233228265284 ) ) ;
#161732 = EDGE_CURVE ( 'NONE', #73245, #108056, #49332, .T. ) ;
#161733 = CARTESIAN_POINT ( 'NONE',  ( 0.6823417656249864960, -0.8239583329919114574, -1.181850606188749264 ) ) ;
#161735 = VERTEX_POINT ( 'NONE', #523 ) ;
#161734 = CARTESIAN_POINT ( 'NONE',  ( 5.856759171423504107, 5.935233242856626568, -0.7216878364870257245 ) ) ;
#161736 = CARTESIAN_POINT ( 'NONE',  ( -8.351459436338037889, 10.76645531385962862, -1.443375672974059665 ) ) ;
#161737 = CARTESIAN_POINT ( 'NONE',  ( 1.657319961134783748, -1.854130675604428902, -1.111159678259740602 ) ) ;
#161738 = CARTESIAN_POINT ( 'NONE',  ( -5.632486471834530661, 5.535932070087196344, -0.7998128361456362523 ) ) ;
#161739 = CARTESIAN_POINT ( 'NONE',  ( 4.878955176071345434, 6.785476686873604280, -1.599625672291269396 ) ) ;
#161740 = CARTESIAN_POINT ( 'NONE',  ( 2.028078973712159172, 1.053637016394028292, -1.490636434207486261 ) ) ;
#161741 = CARTESIAN_POINT ( 'NONE',  ( -5.088387723830502196, 4.830873854090670605, -0.7998128361456221525 ) ) ;
#161742 = CARTESIAN_POINT ( 'NONE',  ( 5.139593076133684768, -1.292025762983130877, -1.289991942498528443 ) ) ;
#161743 = CARTESIAN_POINT ( 'NONE',  ( 10.88220342306020072, 9.708224249340068113, -7.303426440398375519 ) ) ;
#161744 = CARTESIAN_POINT ( 'NONE',  ( 2.935702856749936362, -1.841876368404654629, 0.5141854427313449216 ) ) ;
#161745 = VERTEX_POINT ( 'NONE', #19995 ) ;
#161746 = CARTESIAN_POINT ( 'NONE',  ( 3.332427603156477680, -1.175354876789212799, 1.580226413267592500 ) ) ;
#161747 = EDGE_LOOP ( 'NONE', ( #7149, #110890, #146985, #122007 ) ) ;
#161748 = CARTESIAN_POINT ( 'NONE',  ( 5.548367435846999207, -1.528527190574509032, 1.197884188273186323 ) ) ;
#161749 = ORIENTED_EDGE ( 'NONE', *, *, #107203, .F. ) ;
#161750 = CARTESIAN_POINT ( 'NONE',  ( -6.261886844665283114, 8.398896966899865646, 1.599625672291269396 ) ) ;
#161752 = CARTESIAN_POINT ( 'NONE',  ( 4.939744792934912532, -2.012803497507458683, 0.6676120485993168874 ) ) ;
#161751 = CARTESIAN_POINT ( 'NONE',  ( 5.020262018810099924, 9.078999131912302900, 0.7998128361456331437 ) ) ;
#161753 = CARTESIAN_POINT ( 'NONE',  ( 6.875393295461478260, 8.154285278527437342, -1.082531754730548412 ) ) ;
#161755 = ORIENTED_EDGE ( 'NONE', *, *, #200438, .F. ) ;
#161754 = CARTESIAN_POINT ( 'NONE',  ( 2.930216680654484041, -0.9444820207657660394, -1.662695861641521278 ) ) ;
#161756 = CARTESIAN_POINT ( 'NONE',  ( 4.707942587747941943, 7.051207734045064512, -1.383178547476830111 ) ) ;
#161757 = CARTESIAN_POINT ( 'NONE',  ( -9.605899910213580029, -6.890735599539922873, 0.05097232478521593335 ) ) ;
#161758 = CARTESIAN_POINT ( 'NONE',  ( 4.065465959251388206, 5.836405933916976707, -1.599625672291269396 ) ) ;
#161759 = CARTESIAN_POINT ( 'NONE',  ( 5.338544149128367167, 1.197215095128815632, -1.618272059301849586 ) ) ;
#161760 = CARTESIAN_POINT ( 'NONE',  ( 11.78331023100045627, 12.30000000000000071, -1.800000000000001155 ) ) ;
#161761 = CARTESIAN_POINT ( 'NONE',  ( 6.094357461763901362, -1.817385979143220309, -0.1739998769475574192 ) ) ;
#161762 = CARTESIAN_POINT ( 'NONE',  ( 0.7485892145711987578, -2.054541080789675789, -0.2550698046258002005 ) ) ;
#161763 = CARTESIAN_POINT ( 'NONE',  ( -6.887178846062105286, 10.97886638714038554, -0.7216878364870267237 ) ) ;
#161764 = CARTESIAN_POINT ( 'NONE',  ( -5.947459870766462764, 7.133493745255431229, -1.104964307564069603 ) ) ;
#161765 = CARTESIAN_POINT ( 'NONE',  ( -0.4500000000000339839, 3.999999999999980904, -0.8338124244296073462 ) ) ;
#161766 = EDGE_CURVE ( 'NONE', #205644, #88486, #196640, .T. ) ;
#161767 = CARTESIAN_POINT ( 'NONE',  ( 6.819227946136852125, -0.1326586024288610444, 1.840611662119538749 ) ) ;
#161768 = CARTESIAN_POINT ( 'NONE',  ( 7.772902139336337335, 7.962807338847539107, 0.7998128361456341429 ) ) ;
#161769 = CARTESIAN_POINT ( 'NONE',  ( 0.000000000000000000, -3.517800438942085606, 0.000000000000000000 ) ) ;
#161770 = CARTESIAN_POINT ( 'NONE',  ( 1.364683531249997417, 10.79687500034139802, 2.602085213965210642E-15 ) ) ;
#161771 = CARTESIAN_POINT ( 'NONE',  ( -5.596818484342970912, 5.424043074688562172, -0.7998128361456221525 ) ) ;
#161772 = CARTESIAN_POINT ( 'NONE',  ( -7.014364370223741929, 9.276787413384745662, -1.599625672291271394 ) ) ;
#161773 = CARTESIAN_POINT ( 'NONE',  ( 3.375360373764887179, -0.3420621250952958214, -1.699858368971490563 ) ) ;
#161774 = CARTESIAN_POINT ( 'NONE',  ( -5.603597561149804562, 5.431951997629870910, 0.7998128361456341429 ) ) ;
#161775 = CARTESIAN_POINT ( 'NONE',  ( 1.850524992189076290, -2.059912964915584954, -0.2069831422613493399 ) ) ;
#161776 =( BOUNDED_CURVE ( )  B_SPLINE_CURVE ( 3, ( #127561, #193529, #28904, #80851 ),
 .UNSPECIFIED., .F., .T. ) 
 B_SPLINE_CURVE_WITH_KNOTS ( ( 4, 4 ),
 ( 4.712388980384627502, 6.283185307179586232 ),
 .UNSPECIFIED. ) 
 CURVE ( )  GEOMETRIC_REPRESENTATION_ITEM ( )  RATIONAL_B_SPLINE_CURVE ( ( 1.000000000000000000, 0.8047378541243503935, 0.8047378541243503935, 1.000000000000000000 ) ) 
 REPRESENTATION_ITEM ( '' )  );
#161777 = CARTESIAN_POINT ( 'NONE',  ( 2.197004041102487371, 1.892657838527435299, 0.9490559450526787622 ) ) ;
#161778 = CARTESIAN_POINT ( 'NONE',  ( 3.493197133815315603, 7.227147089426516402, -0.7998128361456291469 ) ) ;
#161779 = CARTESIAN_POINT ( 'NONE',  ( 7.076466111328892694, 10.34329533227067799, -1.199719254218441611 ) ) ;
#161780 = CARTESIAN_POINT ( 'NONE',  ( 0.3776192402222143807, 3.049641483663593888, 0.4287046358292035952 ) ) ;
#161781 = CARTESIAN_POINT ( 'NONE',  ( 0.5671661303022774714, 1.710823773062917219, 0.9755123711343968163 ) ) ;
#161782 = CARTESIAN_POINT ( 'NONE',  ( 4.602920755658417740, 7.148668813305413039, 1.337190490212318839 ) ) ;
#161783 = CARTESIAN_POINT ( 'NONE',  ( 4.528060117284232966, 6.305822774963486310, 1.443375672974062551 ) ) ;
#161785 = CARTESIAN_POINT ( 'NONE',  ( -1.420000000000001039, 7.140846818246206595, -4.154462424328208670 ) ) ;
#161784 = CARTESIAN_POINT ( 'NONE',  ( -3.474999999999998312, -2.770833333333333037, 2.006292185433951047 ) ) ;
#161786 = CARTESIAN_POINT ( 'NONE',  ( 2.344040366607359704, 2.291775683190785173, 0.05432913299479279201 ) ) ;
#161787 = CARTESIAN_POINT ( 'NONE',  ( 0.4338677482375961070, 0.9413943332680120291, -1.564114433284753636 ) ) ;
#161788 = CARTESIAN_POINT ( 'NONE',  ( 3.287273477832891366, 0.04233216220104508987, -1.912079899511004433 ) ) ;
#161789 = CARTESIAN_POINT ( 'NONE',  ( 6.313256805818848960, 7.394496357324014113, 1.199719254218452047 ) ) ;
#161790 = CARTESIAN_POINT ( 'NONE',  ( 7.741342523278707866, 8.133913820021057006, 0.7216878364870458196 ) ) ;
#161791 = CARTESIAN_POINT ( 'NONE',  ( 1.494390954318410625, -1.073482900754536784, 1.702939308294330489 ) ) ;
#161792 = CARTESIAN_POINT ( 'NONE',  ( 1.586688997538304058, 1.889165970957426444, 0.5283831072378852856 ) ) ;
#161793 = CARTESIAN_POINT ( 'NONE',  ( -8.513630394377489807, 12.01998699582738972, -1.199719254218446718 ) ) ;
#161794 = CARTESIAN_POINT ( 'NONE',  ( -5.716734326456539783, 9.821273814174633188, -0.7998128361456231517 ) ) ;
#161795 = CARTESIAN_POINT ( 'NONE',  ( -11.51804212353614609, 7.080072447566390537, 3.210211610704029717 ) ) ;
#161797 = CARTESIAN_POINT ( 'NONE',  ( 3.467426238747231881, 1.726840169280913662, -0.3869839817904097701 ) ) ;
#161796 = CARTESIAN_POINT ( 'NONE',  ( 4.980460981504991835, -0.2552229379441274815, -2.074931007936396288 ) ) ;
#161798 = CARTESIAN_POINT ( 'NONE',  ( -1.225000000000038058, 0.08333333401614038960, 0.7072540797572558491 ) ) ;
#161800 = CARTESIAN_POINT ( 'NONE',  ( 0.1467655724766807612, -1.757430454515636509, 1.308964887167405111 ) ) ;
#161799 = CARTESIAN_POINT ( 'NONE',  ( 0.3000000000000016542, 4.000000000000003553, -1.007084189318387502 ) ) ;
#161801 = CARTESIAN_POINT ( 'NONE',  ( 4.101278252482940978, -1.735469017763660027, 0.1308211784099410635 ) ) ;
#161802 = CARTESIAN_POINT ( 'NONE',  ( 9.348510611822643313, 10.86534945433664134, 1.199719254218453823 ) ) ;
#161803 = CARTESIAN_POINT ( 'NONE',  ( 3.094081423030320933E-15, 0.7598076211376182387, 11.09999999999961062 ) ) ;
#161804 = CARTESIAN_POINT ( 'NONE',  ( 4.815645707022956579, -1.391897370064384631, 1.033600972745553070 ) ) ;
#161805 = CARTESIAN_POINT ( 'NONE',  ( 5.178266966923749770, -1.157238278732542369, -1.836894593069735793 ) ) ;
#161806 = CARTESIAN_POINT ( 'NONE',  ( 3.871016551901614200, 4.474939717762034697, -1.199719254218446718 ) ) ;
#161807 = CARTESIAN_POINT ( 'NONE',  ( 5.999232488047272049, -0.2420365156972601739, 2.001857322483958423 ) ) ;
#161808 = CARTESIAN_POINT ( 'NONE',  ( 5.781250000000004441, 0.7852924748302878566, 1.895863743163952453 ) ) ;
#161809 = AXIS2_PLACEMENT_3D ( 'NONE', #135651, #103143, #134608 ) ;
#161810 = CARTESIAN_POINT ( 'NONE',  ( -1.500000000000011324, 5.160416667349487341, -0.8660254037844313801 ) ) ;
#161811 = CARTESIAN_POINT ( 'NONE',  ( 3.399358865922623263, 1.517880436307640579, 1.186064745714454638 ) ) ;
#161812 = CARTESIAN_POINT ( 'NONE',  ( -0.7500000000000179856, 10.32291666734946922, 1.299038105676658228 ) ) ;
#161813 = CARTESIAN_POINT ( 'NONE',  ( -0.004779673669230537214, -2.156333359934967220, -0.5329991086745686779 ) ) ;
#161814 = EDGE_LOOP ( 'NONE', ( #9694, #44240, #3624, #87917 ) ) ;
#161815 = CARTESIAN_POINT ( 'NONE',  ( 6.983263157960371892, 7.629137130509070275, 2.546189081643289942 ) ) ;
#161816 = CARTESIAN_POINT ( 'NONE',  ( -0.7500000000000215383, 2.441666666666689078, 1.299038105676671107 ) ) ;
#161817 = CARTESIAN_POINT ( 'NONE',  ( 6.634017235788401301, 6.634108284708264414, 0.7998128361456341429 ) ) ;
#161818 = B_SPLINE_CURVE_WITH_KNOTS ( 'NONE', 3,
 ( #30939, #114374, #195561, #176119, #31993, #111174, #113312, #95948, #27719, #162003, #194482, #177175, #193419, #98074, #213897 ),
 .UNSPECIFIED., .F., .F.,
 ( 4, 1, 2, 2, 2, 2, 2, 4 ),
 ( 0.6950735642280609916, 0.6991140303181444526, 0.7011342633631861831, 0.7031544964082280247, 0.7112354285883952798, 0.7193163607685624239, 0.7273972929487294570, 0.7597210216693985885 ),
 .UNSPECIFIED. ) ;
#161819 = CARTESIAN_POINT ( 'NONE',  ( 2.561440534034305827, -1.845267710029829145, 1.236318238231758571 ) ) ;
#161821 = EDGE_CURVE ( 'NONE', #45616, #72859, #13900, .T. ) ;
#161820 = CARTESIAN_POINT ( 'NONE',  ( 6.443807124430430910, 1.351966286592180211, 1.421895456074427688 ) ) ;
#161822 = CARTESIAN_POINT ( 'NONE',  ( 6.304178240674458422, 10.29869901418813782, 1.040834085586084257E-14 ) ) ;
#161823 = CARTESIAN_POINT ( 'NONE',  ( -9.232739420781982176, 12.75498451001223010, 1.082531754730558626 ) ) ;
#161824 = CARTESIAN_POINT ( 'NONE',  ( 5.388439706788500594, 5.251210844200210559, 0.7998128361456352531 ) ) ;
#161826 = VECTOR ( 'NONE', #24258, 1000.000000000000000 ) ;
#161825 = AXIS2_PLACEMENT_3D ( 'NONE', #88219, #188909, #153216 ) ;
#161827 = CARTESIAN_POINT ( 'NONE',  ( -4.556949027968976829, 5.449433633119473264, 1.082531754730549078 ) ) ;
#161829 = CARTESIAN_POINT ( 'NONE',  ( 5.635237469726069648, -0.04712981909091130961, -2.062292871413499373 ) ) ;
#161828 = CARTESIAN_POINT ( 'NONE',  ( 8.218213668177886788, 12.73966637951625813, 0.7998128361456462443 ) ) ;
#161830 = CARTESIAN_POINT ( 'NONE',  ( -3.144601563365788444, 5.756120026313656268, -1.199719254218452935 ) ) ;
#161831 = CARTESIAN_POINT ( 'NONE',  ( 1.499999999999989120, 4.785416667349486453, 0.8660254037844524744 ) ) ;
#161832 = CARTESIAN_POINT ( 'NONE',  ( 1.364683531249988757, 0.3843750003414206362, 0.000000000000000000 ) ) ;
#161833 = CARTESIAN_POINT ( 'NONE',  ( 0.6316679966703161453, 0.9168908782757211329, -1.513568585016269452 ) ) ;
#161834 = CARTESIAN_POINT ( 'NONE',  ( 6.346334349054894908, 0.2861236430486256421, -1.710204530248355059 ) ) ;
#161835 = CARTESIAN_POINT ( 'NONE',  ( 5.267066465580821699, 1.675244640197434798, -0.4716337365339871579 ) ) ;
#161836 = CARTESIAN_POINT ( 'NONE',  ( 4.792970997630896512, 5.550553237779539018, 1.199719254218464037 ) ) ;
#161837 = CARTESIAN_POINT ( 'NONE',  ( 3.281108521976669135, 2.071599159226782838, -0.9818635949487266590 ) ) ;
#161838 = CARTESIAN_POINT ( 'NONE',  ( 1.364683531249992088, 5.446875000341417916, 1.214306433183764966E-14 ) ) ;
#161839 = CARTESIAN_POINT ( 'NONE',  ( 0.7437973067255730930, 0.5320827018340993364, 1.762565881533173950 ) ) ;
#161840 = CARTESIAN_POINT ( 'NONE',  ( 5.708314589969347708, 6.277192745311285016, 1.110195795946368635 ) ) ;
#161841 = CARTESIAN_POINT ( 'NONE',  ( -10.96648295346442126, 6.136757939018690600, -4.903056198141964472 ) ) ;
#161842 = CARTESIAN_POINT ( 'NONE',  ( 2.203868028057700990, -1.825262823911228072, 0.04193083753635528516 ) ) ;
#161843 = CARTESIAN_POINT ( 'NONE',  ( 2.953750172290268150, -1.864168560446223033, -0.7691209412190866956 ) ) ;
#161844 = CARTESIAN_POINT ( 'NONE',  ( 0.6740948890744530297, -1.214310170130480593, 1.824057261183717582 ) ) ;
#161845 = CARTESIAN_POINT ( 'NONE',  ( 9.177312029184088615, 14.07967752687478757, -6.957318393903204168 ) ) ;
#161846 = CARTESIAN_POINT ( 'NONE',  ( 4.577239374156605756, 0.002566705667105330900, -2.106147099847696325 ) ) ;
#161847 = CARTESIAN_POINT ( 'NONE',  ( -6.958359152311683893, 9.141171649162195934, -1.599625672291263179 ) ) ;
#161848 = CARTESIAN_POINT ( 'NONE',  ( 7.441609955141260002, 14.00158514652465591, 10.27059997516222190 ) ) ;
#161849 = CARTESIAN_POINT ( 'NONE',  ( 1.082579992370054311, 1.234693400583252609, -1.661741702728709802 ) ) ;
#161850 = CARTESIAN_POINT ( 'NONE',  ( 5.626797444871351139, 6.523350759560078593, 1.199719254218462483 ) ) ;
#161851 = CARTESIAN_POINT ( 'NONE',  ( 1.360316468749969809, -0.6822916663252893699, -0.7853790794159082322 ) ) ;
#161852 = CARTESIAN_POINT ( 'NONE',  ( 4.916704032076687270, -0.7149955815140829340, -1.996424279390257572 ) ) ;
#161853 = CARTESIAN_POINT ( 'NONE',  ( 0.1879448220486016896, -0.9096115147686645308, 1.698232400582524670 ) ) ;
#161854 = ORIENTED_EDGE ( 'NONE', *, *, #185415, .F. ) ;
#161855 = CARTESIAN_POINT ( 'NONE',  ( -6.629010762438975135, 6.698543742459062145, -0.7998128361456362523 ) ) ;
#161856 = CARTESIAN_POINT ( 'NONE',  ( -11.33772463945036968, 10.90000000000000036, -3.600000000000002309 ) ) ;
#161857 = CARTESIAN_POINT ( 'NONE',  ( 5.682275777458841048, 8.683053269460405232, 1.082531754730547524 ) ) ;
#161858 = CARTESIAN_POINT ( 'NONE',  ( -1.737499999999997824, -1.997916665710752770, 3.009438278150925683 ) ) ;
#161859 = CARTESIAN_POINT ( 'NONE',  ( -5.311043488251275591, 7.219303374425030562, -1.599625672291256295 ) ) ;
#161860 = CARTESIAN_POINT ( 'NONE',  ( 6.258074605086497932, 0.8102346573028992305, -1.959903593942226685 ) ) ;
#161861 = CARTESIAN_POINT ( 'NONE',  ( 1.641775563537830829, -1.524941811188656127, -1.452692102197229884 ) ) ;
#161862 = CARTESIAN_POINT ( 'NONE',  ( -4.847922445338252118, 7.813604065273374921, -1.199719254218453823 ) ) ;
#161863 = CARTESIAN_POINT ( 'NONE',  ( 8.028399517586572998, 12.51821653715971472, -0.7998128361456352531 ) ) ;
#161864 = CARTESIAN_POINT ( 'NONE',  ( 5.225394145299861570, 0.1845887361094991075, -1.851793659149820082 ) ) ;
#161865 = CARTESIAN_POINT ( 'NONE',  ( 7.727257484784855635, 11.10255193463598111, -1.199719254218446718 ) ) ;
#161866 = CARTESIAN_POINT ( 'NONE',  ( -10.28478851095648849, 4.808147343396361961, -6.103030503883996261 ) ) ;
#161867 = CARTESIAN_POINT ( 'NONE',  ( -5.469788628470539926, 5.346117919495872783, -0.7998128361456362523 ) ) ;
#161869 = CARTESIAN_POINT ( 'NONE',  ( -8.459924665247381625, 11.85336729522185806, 1.082531754730560403 ) ) ;
#161868 = AXIS2_PLACEMENT_3D ( 'NONE', #172000, #24658, #126529 ) ;
#161870 =( BOUNDED_SURFACE ( )  B_SPLINE_SURFACE ( 1, 2, ( 
 ( #9031, #76165, #122888, #74040, #141216, #107671, #140130, #173699, #93510, #75105, #207226, #58850, #108738, #159551, #125006, #190963, #158492, #10091, #142270, #208281, #77225, #203997, #55646, #121802, #39401, #96721, #144419, #143344, #127140, #211484, #16475, #197372, #49014, #193112, #30636, #195261, #145489, #63120, #210421, #13297, #209338, #130336, #114085, #45825, #110869, #46895, #111946, #129285, #31699, #62063, #94577, #81503, #128218, #95654, #44761, #176874, #177948, #115133, #29562, #194180, #161704, #79370, #113010, #28486, #179019, #160620, #196325, #162770, #14348, #164881, #80438, #78293, #12221, #146537, #212556, #64195, #47969, #180076, #97774, #163834, #15413, #60987, #147582, #213600, #65226, #131376, #181128, #32749, #98831, #70544, #119394, #169140, #66278, #52200, #69485, #51136, #148642, #67343, #133488, #150783, #199491, #1285, #83622, #134550, #37002, #20735, #135593, #208, #198427, #103084, #50073, #86830, #2346, #149704, #18616, #152894, #100935, #17533, #117258, #200553, #84696, #104157, #82555, #33808, #68422, #185382, #183257, #34861, #202688, #170205, #184312, #118326, #35936, #4473, #102015, #168084, #19684, #132426, #151842, #120476, #167022, #85762, #3419, #201614, #53263, #116194, #136663, #54337, #186449, #38085, #182181, #99887, #165949, #87898, #155035, #40222, #203751, #59660, #92200, #191779, #153971, #57536, #56466, #106333, #171274, #91119, #204815, #138795, #157178, #41306, #43435, #72700, #188590, #139871, #55395, #172354, #156108, #123694, #108485, #22867, #122628, #173438, #25017, #6620, #208032, #205902, #74855, #8772, #140957, #206968, #88982, #58598, #137731, #158250, #121550, #187521, #23944, #90048, #7692, #73775, #189655, #124753, #190713, #42374, #174509, #107414, #75914, #26085, #9838, #142017, #39152, #125817, #109559, #21789, #5538, #71619, #105233, #210157, #211227, #193919, #176618, #192842, #212289, #11967, #147323, #163572, #47704, #44501, #112749, #197115, #178761, #161445, #213350, #76966, #64973, #10891, #143093, #78040, #14081, #95394, #48754, #162510, #94323, #175563, #63922, #131127, #81241, #144164, #27154, #61798, #93258, #28230, #113818, #129015, #160364, #179818, #159292, #127967, #126884, #110618, #45565, #111682, #79103, #177689, #209085, #60721, #29300, #13026, #130077, #145221, #62853, #194992, #46626, #30373, #96460, #80171, #146277, #196072, #31437, #97516, #15155, #68156, #150522, #167820, #185113, #198171, #148386, #165689, #132165, #49804, #18355, #152633, #99623, #84433, #149439, #34612, #134290, #115930, #114867, #98563, #182995, #202421, #168880, #20484, #164624, #2083, #166760, #116995, #100682, #181920, #199226, #180868, #101753, #85498, #17278, #82293, #200295, #83354, #51948, #3152, #33550, #66016, #52997, #1021, #67086, #16209, #214387, #133220, #86570, #50873, #118070, #184057, #35675, #19420, #151585, #69223, #135342, #201356, #119133, #36739, #136405, #102825, #4220, #70289, #32489, #23688, #22611, #189397, #55140, #88719, #121286, #5280, #54076, #72431, #93799, #71357, #6362, #138533, #204556, #187261, #45046, #159839, #143636, #37819, #89798, #41039, #154778, #120211, #38888, #104973, #122368, #171014, #56204, #188324, #106072, #11439, #209630, #110093, #186186, #169944, #77515, #21530, #61271, #39964, #172095, #155843, #127433, #7429, #203487, #73510, #87640, #139613, #205635, #57273, #193403, #123435, #176103, #27703, #111159, #177158, #28777, #94859, #160912, #12507, #78579, #144701, #103897, #153711, #137473, #132701, #112228, #95933, #195546, #80727, #196607, #163054, #48247, #181409, #213883, #33035, #16758, #130615, #50352, #491, #47182, #131652, #161989, #164114, #113296, #63407, #182464, #197655, #128499, #30925, #31982, #14633, #211769, #13579, #99113, #179304, #34093, #198707, #82841, #79652, #147867, #17818, #65505, #97001, #129559, #145768, #146818, #148917, #212837, #64474, #194468, #46110, #114361, #116472, #180356, #98060, #15699, #81784, #49301, #178236, #115417, #165163, #66559, #100164, #166228, #83902, #210712, #62340, #29851, #119677, #3691, #134823, #103366, #18891, #200828, #84975, #35144 ),
 ( #52479, #149992, #2629, #68701, #168365, #118607, #184595, #151066, #152120, #70829, #202972, #169428, #133769, #51423, #136946, #117544, #54613, #19961, #36213, #102292, #120761, #53545, #69768, #21011, #186739, #167304, #183538, #86045, #101220, #135874, #201893, #22072, #185663, #37293, #87110, #153180, #4754, #38361, #1563, #199777, #104439, #67625, #170488, #88184, #154256, #5829, #181054, #131306, #197297, #196249, #213527, #195185, #116112, #99810, #31624, #96638, #32671, #83546, #97698, #47893, #80359, #146457, #67272, #114005, #81425, #112932, #178945, #163757, #34789, #15336, #180000, #147506, #65150, #48938, #30559, #115057, #212472, #182102, #98750, #164807, #150707, #16400, #64116, #162692, #66202, #82478, #148567, #49992, #130258, #134, #132347, #198352, #129208, #33733, #165875, #17461, #149627, #1209, #133410, #199416, #117184, #51060, #183185, #14266, #100864, #166949, #18541, #46818, #84618, #2269, #136588, #119317, #201540, #69411, #120398, #22789, #154960, #55324, #200481, #184237, #88907, #35861, #6545, #202609, #135519, #4400, #72623, #86754, #3342, #36926, #186373, #70472, #89975, #68345, #19611, #54261, #105160, #53189, #185303, #188514, #156026, #170130, #38008, #21714, #104080, #101940, #168005, #40144, #103009, #87826, #39074, #71545, #171199, #138722, #153896, #122553, #204740, #169065, #203675, #85684, #5465, #20662, #152824, #106257, #121475, #52127, #137656, #187446, #56389, #172282, #151771, #23868, #134479, #118256, #210079, #94244, #91041, #159212, #29222, #58519, #205825, #74773, #140876, #193837, #57456, #189580, #124674, #60643, #141942, #95312, #209006, #206888, #7615, #44420, #45486, #127886, #190631, #111602, #108404, #177610, #8691, #160283, #175484, #42292, #11885, #73699, #174427, #173357, #157101, #26003, #77961, #109476, #59578, #75834, #123617, #76888, #139796, #92113, #93179, #10813, #143008, #192761, #41228, #126805, #61718, #110538, #176538, #28149, #144082, #207954, #107333, #158168, #9760, #24938, #125734, #191696, #43355, #27072, #168543, #89447, #20140, #3871, #56929, #69944, #189059, #170672, #103549, #38547, #123102, #120945, #37471, #71010, #6015, #104625, #124156, #102477, #53729, #22260, #139261, #169609, #4934, #8170, #190118, #204206, #88369, #55859, #154435, #136056, #202069, #74254, #21191, #122015, #138196, #155499, #172828, #185839, #119861, #186917, #87294, #137123, #72084, #187983, #86227, #152298, #153363, #39609, #205291, #203152, #54796, #140348, #105712, #171740, #23337, #7082, #73154, #40696, #106799, #206367, #24399, #90512, #156577, #57993, #112155, #125212, #75313, #92658, #59055, #191174, #159761, #79576, #26550, #11361, #76372, #176029, #209551, #42841, #41772, #25486, #110016, #129489, #95857, #161913, #91592, #143557, #93722, #43902, #27622, #108948, #126282, #107884, #28700, #12425, #158700, #9241, #77440, #210637, #10299, #174968, #207436, #142479, #194391, #208487, #60123, #157644, #141429, #192240, #13503, #61195, #127354, #193323, #44971, #111079, #177083, #94785, #160834, #78505, #144623, #62264, #63329, #128424, #46034, #178158, #29773, #145695, #211693, #173912, #196533, #164045, #48175, #146743, #195471, #213808, #17739, #212762, #147791, #65429, #131579, #114288, #183464, #83827, #67553, #179223, #165093, #182387, #15620, #47103, #180286, #31909, #49224, #97986, #81710, #197581, #16684, #150989, #113218, #34017, #30848, #96926, #149920, #162977, #133697, #115344, #181335, #32962, #1488, #99037, #82768, #199702, #130541, #148842, #132627, #198632, #415, #167229, #66486, #100091, #50280, #116399, #166152, #51348, #117472, #14555, #35071, #80653, #64397, #101141, #18815, #84902, #2554, #68629, #105453, #137938, #171489, #155248, #54540, #188807, #139013, #185591, #55606, #85974, #88112, #37220, #201824, #106544, #121762, #52410, #169355, #170412, #153109, #135800, #152049, #23080, #103294, #172570, #122845, #6829, #3618, #71828, #156323, #20941, #118536, #53469, #119606, #24152, #184519, #102223, #87037, #187728, #120687, #7905, #39357, #4683, #134751, #89196, #90255, #40443, #70757, #200760, #136870, #36140, #202895 ) ),
 .UNSPECIFIED., .F., .F., .T. ) 
 B_SPLINE_SURFACE_WITH_KNOTS ( ( 2, 2 ),
 ( 3, 2, 2, 2, 2, 2, 2, 2, 2, 2, 2, 2, 2, 2, 2, 2, 2, 2, 2, 2, 2, 2, 2, 2, 2, 2, 2, 2, 2, 2, 2, 2, 2, 2, 2, 2, 2, 2, 2, 2, 2, 2, 2, 2, 2, 2, 2, 2, 2, 2, 2, 2, 2, 2, 2, 2, 2, 2, 2, 2, 2, 2, 2, 2, 2, 2, 2, 2, 2, 2, 2, 2, 2, 2, 2, 2, 2, 2, 2, 2, 2, 2, 2, 2, 2, 2, 2, 2, 2, 2, 2, 2, 2, 2, 2, 2, 2, 2, 2, 2, 2, 2, 2, 2, 2, 2, 2, 2, 2, 2, 2, 2, 2, 2, 2, 2, 2, 2, 2, 2, 2, 2, 2, 2, 2, 2, 2, 2, 2, 2, 2, 2, 2, 2, 2, 2, 2, 2, 2, 2, 2, 2, 2, 2, 2, 2, 2, 2, 2, 2, 2, 2, 2, 2, 2, 2, 2, 2, 2, 2, 2, 2, 2, 2, 2, 2, 2, 2, 2, 2, 2, 2, 2, 2, 2, 2, 2, 2, 2, 2, 2, 2, 2, 2, 2, 2, 2, 2, 2, 2, 2, 2, 2, 2, 2, 2, 2, 2, 2, 2, 2, 2, 2, 2, 2, 2, 2, 2, 2, 2, 2, 2, 2, 2, 2, 2, 2, 2, 2, 2, 2, 2, 2, 2, 2, 2, 2, 2, 2, 2, 2, 2, 2, 2, 2, 2, 2, 2, 2, 2, 3 ),
 ( 0.000000000000000000, 1.000000000000000000 ),
 ( 0.000000000000000000, 0.004166666666666666609, 0.008333333333333333218, 0.01250000000000000069, 0.01666666666666666644, 0.02083333333333333218, 0.02500000000000000139, 0.02916666666666666713, 0.03333333333333333287, 0.03749999999999999861, 0.04166666666666666435, 0.04583333333333333010, 0.05000000000000000278, 0.05416666666666666852, 0.05833333333333333426, 0.06250000000000000000, 0.06666666666666666574, 0.07083333333333333148, 0.07499999999999999722, 0.07916666666666666297, 0.08333333333333332871, 0.08749999999999999445, 0.09166666666666666019, 0.09583333333333333981, 0.1000000000000000056, 0.1041666666666666713, 0.1083333333333333370, 0.1125000000000000028, 0.1166666666666666685, 0.1208333333333333343, 0.1250000000000000000, 0.1291666666666666796, 0.1333333333333333315, 0.1375000000000000111, 0.1416666666666666630, 0.1458333333333333426, 0.1499999999999999944, 0.1541666666666666741, 0.1583333333333333259, 0.1625000000000000056, 0.1666666666666666574, 0.1708333333333333370, 0.1749999999999999889, 0.1791666666666666685, 0.1833333333333333204, 0.1875000000000000000, 0.1916666666666666796, 0.1958333333333333315, 0.2000000000000000111, 0.2041666666666666630, 0.2083333333333333426, 0.2124999999999999944, 0.2166666666666666741, 0.2208333333333333259, 0.2250000000000000056, 0.2291666666666666574, 0.2333333333333333370, 0.2374999999999999889, 0.2416666666666666685, 0.2458333333333333204, 0.2500000000000000000, 0.2541666666666666519, 0.2583333333333333592, 0.2625000000000000111, 0.2666666666666666630, 0.2708333333333333148, 0.2750000000000000222, 0.2791666666666666741, 0.2833333333333333259, 0.2874999999999999778, 0.2916666666666666852, 0.2958333333333333370, 0.2999999999999999889, 0.3041666666666666408, 0.3083333333333333481, 0.3125000000000000000, 0.3166666666666666519, 0.3208333333333333592, 0.3250000000000000111, 0.3291666666666666630, 0.3333333333333333148, 0.3375000000000000222, 0.3416666666666666741, 0.3458333333333333259, 0.3499999999999999778, 0.3541666666666666852, 0.3583333333333333370, 0.3624999999999999889, 0.3666666666666666408, 0.3708333333333333481, 0.3750000000000000000, 0.3791666666666666519, 0.3833333333333333592, 0.3875000000000000111, 0.3916666666666666630, 0.3958333333333333148, 0.4000000000000000222, 0.4041666666666666741, 0.4083333333333333259, 0.4124999999999999778, 0.4166666666666666852, 0.4208333333333333370, 0.4249999999999999889, 0.4291666666666666408, 0.4333333333333333481, 0.4375000000000000000, 0.4416666666666666519, 0.4458333333333333592, 0.4500000000000000111, 0.4541666666666666630, 0.4583333333333333148, 0.4625000000000000222, 0.4666666666666666741, 0.4708333333333333259, 0.4749999999999999778, 0.4791666666666666852, 0.4833333333333333370, 0.4874999999999999889, 0.4916666666666666408, 0.4958333333333333481, 0.5000000000000000000, 0.5041666666666666519, 0.5083333333333333037, 0.5124999999999999556, 0.5166666666666667185, 0.5208333333333333703, 0.5250000000000000222, 0.5291666666666666741, 0.5333333333333333259, 0.5374999999999999778, 0.5416666666666666297, 0.5458333333333332815, 0.5500000000000000444, 0.5541666666666666963, 0.5583333333333333481, 0.5625000000000000000, 0.5666666666666666519, 0.5708333333333333037, 0.5749999999999999556, 0.5791666666666667185, 0.5833333333333333703, 0.5875000000000000222, 0.5916666666666666741, 0.5958333333333333259, 0.5999999999999999778, 0.6041666666666666297, 0.6083333333333332815, 0.6125000000000000444, 0.6166666666666666963, 0.6208333333333333481, 0.6250000000000000000, 0.6291666666666666519, 0.6333333333333333037, 0.6374999999999999556, 0.6416666666666667185, 0.6458333333333333703, 0.6500000000000000222, 0.6541666666666666741, 0.6583333333333333259, 0.6624999999999999778, 0.6666666666666666297, 0.6708333333333332815, 0.6750000000000000444, 0.6791666666666666963, 0.6833333333333333481, 0.6875000000000000000, 0.6916666666666666519, 0.6958333333333333037, 0.6999999999999999556, 0.7041666666666667185, 0.7083333333333333703, 0.7125000000000000222, 0.7166666666666666741, 0.7208333333333333259, 0.7249999999999999778, 0.7291666666666666297, 0.7333333333333332815, 0.7375000000000000444, 0.7416666666666666963, 0.7458333333333333481, 0.7500000000000000000, 0.7541666666666666519, 0.7583333333333333037, 0.7624999999999999556, 0.7666666666666667185, 0.7708333333333333703, 0.7750000000000000222, 0.7791666666666666741, 0.7833333333333333259, 0.7874999999999999778, 0.7916666666666666297, 0.7958333333333332815, 0.8000000000000000444, 0.8041666666666666963, 0.8083333333333333481, 0.8125000000000000000, 0.8166666666666666519, 0.8208333333333333037, 0.8249999999999999556, 0.8291666666666667185, 0.8333333333333333703, 0.8375000000000000222, 0.8416666666666666741, 0.8458333333333333259, 0.8499999999999999778, 0.8541666666666666297, 0.8583333333333332815, 0.8625000000000000444, 0.8666666666666666963, 0.8708333333333333481, 0.8750000000000000000, 0.8791666666666666519, 0.8833333333333333037, 0.8874999999999999556, 0.8916666666666667185, 0.8958333333333333703, 0.9000000000000000222, 0.9041666666666666741, 0.9083333333333333259, 0.9124999999999999778, 0.9166666666666666297, 0.9208333333333332815, 0.9250000000000000444, 0.9291666666666666963, 0.9333333333333333481, 0.9375000000000000000, 0.9416666666666666519, 0.9458333333333333037, 0.9499999999999999556, 0.9541666666666667185, 0.9583333333333333703, 0.9625000000000000222, 0.9666666666666666741, 0.9708333333333333259, 0.9749999999999999778, 0.9791666666666666297, 0.9833333333333332815, 0.9875000000000000444, 0.9916666666666666963, 0.9958333333333333481, 1.000000000000000000 ),
 .UNSPECIFIED. ) 
 GEOMETRIC_REPRESENTATION_ITEM ( )  RATIONAL_B_SPLINE_SURFACE ( (
 ( 1.000000000000000000, 0.8660254037844387076, 1.000000000000000000, 0.8660254037844387076, 1.000000000000000000, 0.8660254037844387076, 1.000000000000000000, 0.8660254037844387076, 1.000000000000000000, 0.8660254037844387076, 1.000000000000000000, 0.8660254037844387076, 1.000000000000000000, 0.8660254037844387076, 1.000000000000000000, 0.8660254037844387076, 1.000000000000000000, 0.8660254037844387076, 1.000000000000000000, 0.8660254037844387076, 1.000000000000000000, 0.8660254037844387076, 1.000000000000000000, 0.8660254037844387076, 1.000000000000000000, 0.8660254037844387076, 1.000000000000000000, 0.8660254037844387076, 1.000000000000000000, 0.8660254037844387076, 1.000000000000000000, 0.8660254037844387076, 1.000000000000000000, 0.8660254037844387076, 1.000000000000000000, 0.8660254037844387076, 1.000000000000000000, 0.8660254037844387076, 1.000000000000000000, 0.8660254037844387076, 1.000000000000000000, 0.8660254037844387076, 1.000000000000000000, 0.8660254037844387076, 1.000000000000000000, 0.8660254037844387076, 1.000000000000000000, 0.8660254037844387076, 1.000000000000000000, 0.8660254037844387076, 1.000000000000000000, 0.8660254037844387076, 1.000000000000000000, 0.8660254037844387076, 1.000000000000000000, 0.8660254037844387076, 1.000000000000000000, 0.8660254037844387076, 1.000000000000000000, 0.8660254037844387076, 1.000000000000000000, 0.8660254037844387076, 1.000000000000000000, 0.8660254037844387076, 1.000000000000000000, 0.8660254037844387076, 1.000000000000000000, 0.8660254037844387076, 1.000000000000000000, 0.8660254037844387076, 1.000000000000000000, 0.8660254037844387076, 1.000000000000000000, 0.8660254037844387076, 1.000000000000000000, 0.8660254037844387076, 1.000000000000000000, 0.8660254037844387076, 1.000000000000000000, 0.8660254037844387076, 1.000000000000000000, 0.8660254037844387076, 1.000000000000000000, 0.8660254037844387076, 1.000000000000000000, 0.8660254037844387076, 1.000000000000000000, 0.8660254037844387076, 1.000000000000000000, 0.8660254037844387076, 1.000000000000000000, 0.8660254037844387076, 1.000000000000000000, 0.8660254037844387076, 1.000000000000000000, 0.8660254037844387076, 1.000000000000000000, 0.8660254037844387076, 1.000000000000000000, 0.8660254037844387076, 1.000000000000000000, 0.8660254037844387076, 1.000000000000000000, 0.8660254037844387076, 1.000000000000000000, 0.8660254037844387076, 1.000000000000000000, 0.8660254037844387076, 1.000000000000000000, 0.8660254037844387076, 1.000000000000000000, 0.8660254037844387076, 1.000000000000000000, 0.8660254037844387076, 1.000000000000000000, 0.8660254037844387076, 1.000000000000000000, 0.8660254037844387076, 1.000000000000000000, 0.8660254037844387076, 1.000000000000000000, 0.8660254037844387076, 1.000000000000000000, 0.8660254037844387076, 1.000000000000000000, 0.8660254037844387076, 1.000000000000000000, 0.8660254037844387076, 1.000000000000000000, 0.8660254037844387076, 1.000000000000000000, 0.8660254037844387076, 1.000000000000000000, 0.8660254037844387076, 1.000000000000000000, 0.8660254037844387076, 1.000000000000000000, 0.8660254037844387076, 1.000000000000000000, 0.8660254037844387076, 1.000000000000000000, 0.8660254037844387076, 1.000000000000000000, 0.8660254037844387076, 1.000000000000000000, 0.8660254037844387076, 1.000000000000000000, 0.8660254037844387076, 1.000000000000000000, 0.8660254037844387076, 1.000000000000000000, 0.8660254037844387076, 1.000000000000000000, 0.8660254037844387076, 1.000000000000000000, 0.8660254037844387076, 1.000000000000000000, 0.8660254037844387076, 1.000000000000000000, 0.8660254037844387076, 1.000000000000000000, 0.8660254037844387076, 1.000000000000000000, 0.8660254037844387076, 1.000000000000000000, 0.8660254037844387076, 1.000000000000000000, 0.8660254037844387076, 1.000000000000000000, 0.8660254037844387076, 1.000000000000000000, 0.8660254037844387076, 1.000000000000000000, 0.8660254037844387076, 1.000000000000000000, 0.8660254037844387076, 1.000000000000000000, 0.8660254037844387076, 1.000000000000000000, 0.8660254037844387076, 1.000000000000000000, 0.8660254037844387076, 1.000000000000000000, 0.8660254037844387076, 1.000000000000000000, 0.8660254037844387076, 1.000000000000000000, 0.8660254037844387076, 1.000000000000000000, 0.8660254037844387076, 1.000000000000000000, 0.8660254037844387076, 1.000000000000000000, 0.8660254037844387076, 1.000000000000000000, 0.8660254037844387076, 1.000000000000000000, 0.8660254037844387076, 1.000000000000000000, 0.8660254037844387076, 1.000000000000000000, 0.8660254037844387076, 1.000000000000000000, 0.8660254037844387076, 1.000000000000000000, 0.8660254037844387076, 1.000000000000000000, 0.8660254037844387076, 1.000000000000000000, 0.8660254037844387076, 1.000000000000000000, 0.8660254037844387076, 1.000000000000000000, 0.8660254037844387076, 1.000000000000000000, 0.8660254037844387076, 1.000000000000000000, 0.8660254037844387076, 1.000000000000000000, 0.8660254037844387076, 1.000000000000000000, 0.8660254037844387076, 1.000000000000000000, 0.8660254037844387076, 1.000000000000000000, 0.8660254037844387076, 1.000000000000000000, 0.8660254037844387076, 1.000000000000000000, 0.8660254037844387076, 1.000000000000000000, 0.8660254037844387076, 1.000000000000000000, 0.8660254037844387076, 1.000000000000000000, 0.8660254037844387076, 1.000000000000000000, 0.8660254037844387076, 1.000000000000000000, 0.8660254037844387076, 1.000000000000000000, 0.8660254037844387076, 1.000000000000000000, 0.8660254037844387076, 1.000000000000000000, 0.8660254037844387076, 1.000000000000000000, 0.8660254037844387076, 1.000000000000000000, 0.8660254037844387076, 1.000000000000000000, 0.8660254037844387076, 1.000000000000000000, 0.8660254037844387076, 1.000000000000000000, 0.8660254037844387076, 1.000000000000000000, 0.8660254037844387076, 1.000000000000000000, 0.8660254037844387076, 1.000000000000000000, 0.8660254037844387076, 1.000000000000000000, 0.8660254037844387076, 1.000000000000000000, 0.8660254037844387076, 1.000000000000000000, 0.8660254037844387076, 1.000000000000000000, 0.8660254037844387076, 1.000000000000000000, 0.8660254037844387076, 1.000000000000000000, 0.8660254037844387076, 1.000000000000000000, 0.8660254037844387076, 1.000000000000000000, 0.8660254037844387076, 1.000000000000000000, 0.8660254037844387076, 1.000000000000000000, 0.8660254037844387076, 1.000000000000000000, 0.8660254037844387076, 1.000000000000000000, 0.8660254037844387076, 1.000000000000000000, 0.8660254037844387076, 1.000000000000000000, 0.8660254037844387076, 1.000000000000000000, 0.8660254037844387076, 1.000000000000000000, 0.8660254037844387076, 1.000000000000000000, 0.8660254037844387076, 1.000000000000000000, 0.8660254037844387076, 1.000000000000000000, 0.8660254037844387076, 1.000000000000000000, 0.8660254037844387076, 1.000000000000000000, 0.8660254037844387076, 1.000000000000000000, 0.8660254037844387076, 1.000000000000000000, 0.8660254037844387076, 1.000000000000000000, 0.8660254037844387076, 1.000000000000000000, 0.8660254037844387076, 1.000000000000000000, 0.8660254037844387076, 1.000000000000000000, 0.8660254037844387076, 1.000000000000000000, 0.8660254037844387076, 1.000000000000000000, 0.8660254037844387076, 1.000000000000000000, 0.8660254037844387076, 1.000000000000000000, 0.8660254037844387076, 1.000000000000000000, 0.8660254037844387076, 1.000000000000000000, 0.8660254037844387076, 1.000000000000000000, 0.8660254037844387076, 1.000000000000000000, 0.8660254037844387076, 1.000000000000000000, 0.8660254037844387076, 1.000000000000000000, 0.8660254037844387076, 1.000000000000000000, 0.8660254037844387076, 1.000000000000000000, 0.8660254037844387076, 1.000000000000000000, 0.8660254037844387076, 1.000000000000000000, 0.8660254037844387076, 1.000000000000000000, 0.8660254037844387076, 1.000000000000000000, 0.8660254037844387076, 1.000000000000000000, 0.8660254037844387076, 1.000000000000000000, 0.8660254037844387076, 1.000000000000000000, 0.8660254037844387076, 1.000000000000000000, 0.8660254037844387076, 1.000000000000000000, 0.8660254037844387076, 1.000000000000000000, 0.8660254037844387076, 1.000000000000000000, 0.8660254037844387076, 1.000000000000000000, 0.8660254037844387076, 1.000000000000000000, 0.8660254037844387076, 1.000000000000000000, 0.8660254037844387076, 1.000000000000000000, 0.8660254037844387076, 1.000000000000000000, 0.8660254037844387076, 1.000000000000000000, 0.8660254037844387076, 1.000000000000000000, 0.8660254037844387076, 1.000000000000000000, 0.8660254037844387076, 1.000000000000000000, 0.8660254037844387076, 1.000000000000000000, 0.8660254037844387076, 1.000000000000000000, 0.8660254037844387076, 1.000000000000000000, 0.8660254037844387076, 1.000000000000000000, 0.8660254037844387076, 1.000000000000000000, 0.8660254037844387076, 1.000000000000000000, 0.8660254037844387076, 1.000000000000000000, 0.8660254037844387076, 1.000000000000000000, 0.8660254037844387076, 1.000000000000000000, 0.8660254037844387076, 1.000000000000000000, 0.8660254037844387076, 1.000000000000000000, 0.8660254037844387076, 1.000000000000000000, 0.8660254037844387076, 1.000000000000000000, 0.8660254037844387076, 1.000000000000000000, 0.8660254037844387076, 1.000000000000000000, 0.8660254037844387076, 1.000000000000000000, 0.8660254037844387076, 1.000000000000000000, 0.8660254037844387076, 1.000000000000000000, 0.8660254037844387076, 1.000000000000000000, 0.8660254037844387076, 1.000000000000000000, 0.8660254037844387076, 1.000000000000000000, 0.8660254037844387076, 1.000000000000000000, 0.8660254037844387076, 1.000000000000000000, 0.8660254037844387076, 1.000000000000000000, 0.8660254037844387076, 1.000000000000000000, 0.8660254037844387076, 1.000000000000000000, 0.8660254037844387076, 1.000000000000000000, 0.8660254037844387076, 1.000000000000000000, 0.8660254037844387076, 1.000000000000000000, 0.8660254037844387076, 1.000000000000000000, 0.8660254037844387076, 1.000000000000000000, 0.8660254037844387076, 1.000000000000000000, 0.8660254037844387076, 1.000000000000000000, 0.8660254037844387076, 1.000000000000000000, 0.8660254037844387076, 1.000000000000000000, 0.8660254037844387076, 1.000000000000000000, 0.8660254037844387076, 1.000000000000000000, 0.8660254037844387076, 1.000000000000000000, 0.8660254037844387076, 1.000000000000000000, 0.8660254037844387076, 1.000000000000000000, 0.8660254037844387076, 1.000000000000000000, 0.8660254037844387076, 1.000000000000000000, 0.8660254037844387076, 1.000000000000000000, 0.8660254037844387076, 1.000000000000000000, 0.8660254037844387076, 1.000000000000000000, 0.8660254037844387076, 1.000000000000000000, 0.8660254037844387076, 1.000000000000000000, 0.8660254037844387076, 1.000000000000000000, 0.8660254037844387076, 1.000000000000000000, 0.8660254037844387076, 1.000000000000000000, 0.8660254037844387076, 1.000000000000000000),
 ( 1.000000000000000000, 0.8660254037844387076, 1.000000000000000000, 0.8660254037844387076, 1.000000000000000000, 0.8660254037844387076, 1.000000000000000000, 0.8660254037844387076, 1.000000000000000000, 0.8660254037844387076, 1.000000000000000000, 0.8660254037844387076, 1.000000000000000000, 0.8660254037844387076, 1.000000000000000000, 0.8660254037844387076, 1.000000000000000000, 0.8660254037844387076, 1.000000000000000000, 0.8660254037844387076, 1.000000000000000000, 0.8660254037844387076, 1.000000000000000000, 0.8660254037844387076, 1.000000000000000000, 0.8660254037844387076, 1.000000000000000000, 0.8660254037844387076, 1.000000000000000000, 0.8660254037844387076, 1.000000000000000000, 0.8660254037844387076, 1.000000000000000000, 0.8660254037844387076, 1.000000000000000000, 0.8660254037844387076, 1.000000000000000000, 0.8660254037844387076, 1.000000000000000000, 0.8660254037844387076, 1.000000000000000000, 0.8660254037844387076, 1.000000000000000000, 0.8660254037844387076, 1.000000000000000000, 0.8660254037844387076, 1.000000000000000000, 0.8660254037844387076, 1.000000000000000000, 0.8660254037844387076, 1.000000000000000000, 0.8660254037844387076, 1.000000000000000000, 0.8660254037844387076, 1.000000000000000000, 0.8660254037844387076, 1.000000000000000000, 0.8660254037844387076, 1.000000000000000000, 0.8660254037844387076, 1.000000000000000000, 0.8660254037844387076, 1.000000000000000000, 0.8660254037844387076, 1.000000000000000000, 0.8660254037844387076, 1.000000000000000000, 0.8660254037844387076, 1.000000000000000000, 0.8660254037844387076, 1.000000000000000000, 0.8660254037844387076, 1.000000000000000000, 0.8660254037844387076, 1.000000000000000000, 0.8660254037844387076, 1.000000000000000000, 0.8660254037844387076, 1.000000000000000000, 0.8660254037844387076, 1.000000000000000000, 0.8660254037844387076, 1.000000000000000000, 0.8660254037844387076, 1.000000000000000000, 0.8660254037844387076, 1.000000000000000000, 0.8660254037844387076, 1.000000000000000000, 0.8660254037844387076, 1.000000000000000000, 0.8660254037844387076, 1.000000000000000000, 0.8660254037844387076, 1.000000000000000000, 0.8660254037844387076, 1.000000000000000000, 0.8660254037844387076, 1.000000000000000000, 0.8660254037844387076, 1.000000000000000000, 0.8660254037844387076, 1.000000000000000000, 0.8660254037844387076, 1.000000000000000000, 0.8660254037844387076, 1.000000000000000000, 0.8660254037844387076, 1.000000000000000000, 0.8660254037844387076, 1.000000000000000000, 0.8660254037844387076, 1.000000000000000000, 0.8660254037844387076, 1.000000000000000000, 0.8660254037844387076, 1.000000000000000000, 0.8660254037844387076, 1.000000000000000000, 0.8660254037844387076, 1.000000000000000000, 0.8660254037844387076, 1.000000000000000000, 0.8660254037844387076, 1.000000000000000000, 0.8660254037844387076, 1.000000000000000000, 0.8660254037844387076, 1.000000000000000000, 0.8660254037844387076, 1.000000000000000000, 0.8660254037844387076, 1.000000000000000000, 0.8660254037844387076, 1.000000000000000000, 0.8660254037844387076, 1.000000000000000000, 0.8660254037844387076, 1.000000000000000000, 0.8660254037844387076, 1.000000000000000000, 0.8660254037844387076, 1.000000000000000000, 0.8660254037844387076, 1.000000000000000000, 0.8660254037844387076, 1.000000000000000000, 0.8660254037844387076, 1.000000000000000000, 0.8660254037844387076, 1.000000000000000000, 0.8660254037844387076, 1.000000000000000000, 0.8660254037844387076, 1.000000000000000000, 0.8660254037844387076, 1.000000000000000000, 0.8660254037844387076, 1.000000000000000000, 0.8660254037844387076, 1.000000000000000000, 0.8660254037844387076, 1.000000000000000000, 0.8660254037844387076, 1.000000000000000000, 0.8660254037844387076, 1.000000000000000000, 0.8660254037844387076, 1.000000000000000000, 0.8660254037844387076, 1.000000000000000000, 0.8660254037844387076, 1.000000000000000000, 0.8660254037844387076, 1.000000000000000000, 0.8660254037844387076, 1.000000000000000000, 0.8660254037844387076, 1.000000000000000000, 0.8660254037844387076, 1.000000000000000000, 0.8660254037844387076, 1.000000000000000000, 0.8660254037844387076, 1.000000000000000000, 0.8660254037844387076, 1.000000000000000000, 0.8660254037844387076, 1.000000000000000000, 0.8660254037844387076, 1.000000000000000000, 0.8660254037844387076, 1.000000000000000000, 0.8660254037844387076, 1.000000000000000000, 0.8660254037844387076, 1.000000000000000000, 0.8660254037844387076, 1.000000000000000000, 0.8660254037844387076, 1.000000000000000000, 0.8660254037844387076, 1.000000000000000000, 0.8660254037844387076, 1.000000000000000000, 0.8660254037844387076, 1.000000000000000000, 0.8660254037844387076, 1.000000000000000000, 0.8660254037844387076, 1.000000000000000000, 0.8660254037844387076, 1.000000000000000000, 0.8660254037844387076, 1.000000000000000000, 0.8660254037844387076, 1.000000000000000000, 0.8660254037844387076, 1.000000000000000000, 0.8660254037844387076, 1.000000000000000000, 0.8660254037844387076, 1.000000000000000000, 0.8660254037844387076, 1.000000000000000000, 0.8660254037844387076, 1.000000000000000000, 0.8660254037844387076, 1.000000000000000000, 0.8660254037844387076, 1.000000000000000000, 0.8660254037844387076, 1.000000000000000000, 0.8660254037844387076, 1.000000000000000000, 0.8660254037844387076, 1.000000000000000000, 0.8660254037844387076, 1.000000000000000000, 0.8660254037844387076, 1.000000000000000000, 0.8660254037844387076, 1.000000000000000000, 0.8660254037844387076, 1.000000000000000000, 0.8660254037844387076, 1.000000000000000000, 0.8660254037844387076, 1.000000000000000000, 0.8660254037844387076, 1.000000000000000000, 0.8660254037844387076, 1.000000000000000000, 0.8660254037844387076, 1.000000000000000000, 0.8660254037844387076, 1.000000000000000000, 0.8660254037844387076, 1.000000000000000000, 0.8660254037844387076, 1.000000000000000000, 0.8660254037844387076, 1.000000000000000000, 0.8660254037844387076, 1.000000000000000000, 0.8660254037844387076, 1.000000000000000000, 0.8660254037844387076, 1.000000000000000000, 0.8660254037844387076, 1.000000000000000000, 0.8660254037844387076, 1.000000000000000000, 0.8660254037844387076, 1.000000000000000000, 0.8660254037844387076, 1.000000000000000000, 0.8660254037844387076, 1.000000000000000000, 0.8660254037844387076, 1.000000000000000000, 0.8660254037844387076, 1.000000000000000000, 0.8660254037844387076, 1.000000000000000000, 0.8660254037844387076, 1.000000000000000000, 0.8660254037844387076, 1.000000000000000000, 0.8660254037844387076, 1.000000000000000000, 0.8660254037844387076, 1.000000000000000000, 0.8660254037844387076, 1.000000000000000000, 0.8660254037844387076, 1.000000000000000000, 0.8660254037844387076, 1.000000000000000000, 0.8660254037844387076, 1.000000000000000000, 0.8660254037844387076, 1.000000000000000000, 0.8660254037844387076, 1.000000000000000000, 0.8660254037844387076, 1.000000000000000000, 0.8660254037844387076, 1.000000000000000000, 0.8660254037844387076, 1.000000000000000000, 0.8660254037844387076, 1.000000000000000000, 0.8660254037844387076, 1.000000000000000000, 0.8660254037844387076, 1.000000000000000000, 0.8660254037844387076, 1.000000000000000000, 0.8660254037844387076, 1.000000000000000000, 0.8660254037844387076, 1.000000000000000000, 0.8660254037844387076, 1.000000000000000000, 0.8660254037844387076, 1.000000000000000000, 0.8660254037844387076, 1.000000000000000000, 0.8660254037844387076, 1.000000000000000000, 0.8660254037844387076, 1.000000000000000000, 0.8660254037844387076, 1.000000000000000000, 0.8660254037844387076, 1.000000000000000000, 0.8660254037844387076, 1.000000000000000000, 0.8660254037844387076, 1.000000000000000000, 0.8660254037844387076, 1.000000000000000000, 0.8660254037844387076, 1.000000000000000000, 0.8660254037844387076, 1.000000000000000000, 0.8660254037844387076, 1.000000000000000000, 0.8660254037844387076, 1.000000000000000000, 0.8660254037844387076, 1.000000000000000000, 0.8660254037844387076, 1.000000000000000000, 0.8660254037844387076, 1.000000000000000000, 0.8660254037844387076, 1.000000000000000000, 0.8660254037844387076, 1.000000000000000000, 0.8660254037844387076, 1.000000000000000000, 0.8660254037844387076, 1.000000000000000000, 0.8660254037844387076, 1.000000000000000000, 0.8660254037844387076, 1.000000000000000000, 0.8660254037844387076, 1.000000000000000000, 0.8660254037844387076, 1.000000000000000000, 0.8660254037844387076, 1.000000000000000000, 0.8660254037844387076, 1.000000000000000000, 0.8660254037844387076, 1.000000000000000000, 0.8660254037844387076, 1.000000000000000000, 0.8660254037844387076, 1.000000000000000000, 0.8660254037844387076, 1.000000000000000000, 0.8660254037844387076, 1.000000000000000000, 0.8660254037844387076, 1.000000000000000000, 0.8660254037844387076, 1.000000000000000000, 0.8660254037844387076, 1.000000000000000000, 0.8660254037844387076, 1.000000000000000000, 0.8660254037844387076, 1.000000000000000000, 0.8660254037844387076, 1.000000000000000000, 0.8660254037844387076, 1.000000000000000000, 0.8660254037844387076, 1.000000000000000000, 0.8660254037844387076, 1.000000000000000000, 0.8660254037844387076, 1.000000000000000000, 0.8660254037844387076, 1.000000000000000000, 0.8660254037844387076, 1.000000000000000000, 0.8660254037844387076, 1.000000000000000000, 0.8660254037844387076, 1.000000000000000000, 0.8660254037844387076, 1.000000000000000000, 0.8660254037844387076, 1.000000000000000000, 0.8660254037844387076, 1.000000000000000000, 0.8660254037844387076, 1.000000000000000000, 0.8660254037844387076, 1.000000000000000000, 0.8660254037844387076, 1.000000000000000000, 0.8660254037844387076, 1.000000000000000000, 0.8660254037844387076, 1.000000000000000000, 0.8660254037844387076, 1.000000000000000000, 0.8660254037844387076, 1.000000000000000000, 0.8660254037844387076, 1.000000000000000000, 0.8660254037844387076, 1.000000000000000000, 0.8660254037844387076, 1.000000000000000000, 0.8660254037844387076, 1.000000000000000000, 0.8660254037844387076, 1.000000000000000000, 0.8660254037844387076, 1.000000000000000000, 0.8660254037844387076, 1.000000000000000000, 0.8660254037844387076, 1.000000000000000000, 0.8660254037844387076, 1.000000000000000000, 0.8660254037844387076, 1.000000000000000000, 0.8660254037844387076, 1.000000000000000000, 0.8660254037844387076, 1.000000000000000000, 0.8660254037844387076, 1.000000000000000000, 0.8660254037844387076, 1.000000000000000000, 0.8660254037844387076, 1.000000000000000000, 0.8660254037844387076, 1.000000000000000000, 0.8660254037844387076, 1.000000000000000000, 0.8660254037844387076, 1.000000000000000000, 0.8660254037844387076, 1.000000000000000000, 0.8660254037844387076, 1.000000000000000000, 0.8660254037844387076, 1.000000000000000000, 0.8660254037844387076, 1.000000000000000000, 0.8660254037844387076, 1.000000000000000000) ) ) 
 REPRESENTATION_ITEM ( '' )  SURFACE ( )  );
#161872 = CARTESIAN_POINT ( 'NONE',  ( 1.996468121258226924, 1.940055844723225009, 0.2909814450420752929 ) ) ;
#161871 = CARTESIAN_POINT ( 'NONE',  ( -8.179646747746328828, 8.437342715325849341, -0.7998128361456291469 ) ) ;
#161873 = CARTESIAN_POINT ( 'NONE',  ( 0.9190830904215805397, 1.997680973563022544, 0.8264451868333838602 ) ) ;
#161874 = CARTESIAN_POINT ( 'NONE',  ( 3.292204118033771110, -0.8216723425069611952, -1.841733987974409237 ) ) ;
#161876 = CARTESIAN_POINT ( 'NONE',  ( -6.082978790695654503, 6.030206930409384825, -0.4315292173028318912 ) ) ;
#161875 = CARTESIAN_POINT ( 'NONE',  ( -4.749098946536820520, 8.762642214260091933, 0.7998128361456281477 ) ) ;
#161877 = CARTESIAN_POINT ( 'NONE',  ( 0.6823417656249882723, 0.9260416670080831025, -1.181850606188749264 ) ) ;
#161878 = CARTESIAN_POINT ( 'NONE',  ( 3.374086008222790589, -0.3405263371191130095, 1.699849027820112823 ) ) ;
#161879 = CARTESIAN_POINT ( 'NONE',  ( 2.237881400472482962, 0.3803048411740033719, 1.698081864755231374 ) ) ;
#161880 = CARTESIAN_POINT ( 'NONE',  ( 6.155038550924133212, 10.12470270947942730, 0.7216878364870438212 ) ) ;
#161881 = CARTESIAN_POINT ( 'NONE',  ( -11.50450067106337571, 6.429220943216678030, -3.050492100467481205 ) ) ;
#161882 = CARTESIAN_POINT ( 'NONE',  ( 3.093097461593071973, 1.769307450888421673, -1.056303779743078985 ) ) ;
#161883 = CARTESIAN_POINT ( 'NONE',  ( 1.159529582462547781, -0.4871260124716703110, -1.956262300040665814 ) ) ;
#161884 = CARTESIAN_POINT ( 'NONE',  ( 6.925078400183550364, -0.007619068086212391067, 2.144148427808051594 ) ) ;
#161885 = CARTESIAN_POINT ( 'NONE',  ( -4.285259070371116863, 7.157163461145040095, 1.199719254218452935 ) ) ;
#161886 = CARTESIAN_POINT ( 'NONE',  ( 1.463681139585114588, 1.942636298559533792, -0.3350429378523085977 ) ) ;
#161887 = ADVANCED_FACE ( 'NONE', ( #140196 ), #69799, .F. ) ;
#161889 = CARTESIAN_POINT ( 'NONE',  ( -5.478903473698255588, 7.485416367438324059, -1.443375672974066548 ) ) ;
#161888 = CARTESIAN_POINT ( 'NONE',  ( 6.205323455156911194, 1.660478276859885582, -0.9486371710855368011 ) ) ;
#161890 = CARTESIAN_POINT ( 'NONE',  ( -5.736508391913536897, 9.706693867292189637, 0.7216878364870267237 ) ) ;
#161891 = CARTESIAN_POINT ( 'NONE',  ( 7.537407054554579489, 7.758339416593960536, 0.000000000000000000 ) ) ;
#161892 = CARTESIAN_POINT ( 'NONE',  ( -5.759181390754928742, 9.941071732514568993, 0.000000000000000000 ) ) ;
#161893 = CARTESIAN_POINT ( 'NONE',  ( 1.524088222275731486, -2.004166515738073695, 0.2493262195080257204 ) ) ;
#161894 = CYLINDRICAL_SURFACE ( 'NONE', #170331, 1.224999999999996980 ) ;
#161895 = CARTESIAN_POINT ( 'NONE',  ( 4.401628477801726724, 1.850755835686506590, 1.378093606121533199 ) ) ;
#161896 = CARTESIAN_POINT ( 'NONE',  ( 6.443807124430430910, 1.351966286592180211, 1.421895456074427688 ) ) ;
#161897 = CARTESIAN_POINT ( 'NONE',  ( 2.272246806564695021, -0.9202570425024100276, -1.732484491337261456 ) ) ;
#161898 = CARTESIAN_POINT ( 'NONE',  ( 9.398826802771546696, 11.98838390803207865, -1.599625672291262513 ) ) ;
#161899 = CARTESIAN_POINT ( 'NONE',  ( 0.03578008775950020093, -1.617816776142148250, 1.203357013023528932 ) ) ;
#161900 = ORIENTED_EDGE ( 'NONE', *, *, #55350, .T. ) ;
#161901 = CARTESIAN_POINT ( 'NONE',  ( 1.358780451569325365, -2.012465911620679115, -0.6584304486853159721 ) ) ;
#161903 = CARTESIAN_POINT ( 'NONE',  ( -8.206763054973658100, 8.468978407091068306, 0.7998128361456602331 ) ) ;
#161902 = CARTESIAN_POINT ( 'NONE',  ( -4.623494077460110319, 5.352830164246910272, 1.199719254218462483 ) ) ;
#161904 = CARTESIAN_POINT ( 'NONE',  ( 1.446930991382020748, 0.5358794165791405106, -1.761430032344503349 ) ) ;
#161905 = ORIENTED_EDGE ( 'NONE', *, *, #14538, .T. ) ;
#161906 = CARTESIAN_POINT ( 'NONE',  ( 4.241221290925122567, -0.2070989531138747453, -2.161143177887809852 ) ) ;
#161907 = CARTESIAN_POINT ( 'NONE',  ( 11.97450891632845327, 7.629227029099267199, 0.8948425641056547697 ) ) ;
#161908 = CARTESIAN_POINT ( 'NONE',  ( 3.322626870553476941, -0.8629183168706102691, -1.937285153019531414 ) ) ;
#161909 = CARTESIAN_POINT ( 'NONE',  ( 1.499999999999989120, 3.785416667349481123, 0.8660254037844524744 ) ) ;
#161910 = CARTESIAN_POINT ( 'NONE',  ( 7.391166297744269365, 11.77477778067701664, 1.040834085586084257E-14 ) ) ;
#161911 = CIRCLE ( 'NONE', #78839, 10.99999999999719513 ) ;
#161912 = CARTESIAN_POINT ( 'NONE',  ( 3.585278813505449858, 1.864625933638365485, -0.8777486340088790362 ) ) ;
#161914 = CARTESIAN_POINT ( 'NONE',  ( 0.2922019606856861018, 1.531309713818730822, -1.022077305420886040 ) ) ;
#161913 = CARTESIAN_POINT ( 'NONE',  ( -7.527801604085656351, 9.805521176231838609, 1.599625672291295375 ) ) ;
#161915 = CARTESIAN_POINT ( 'NONE',  ( 1.364683531249988535, 3.155208333674756283, -0.7879004041258239610 ) ) ;
#161916 = CARTESIAN_POINT ( 'NONE',  ( -1.737499999999997824, -2.741666666666666696, 3.009438278150925683 ) ) ;
#161917 = CARTESIAN_POINT ( 'NONE',  ( 1.465205965978033875, 4.370509616058218860, 0.3306380942217546082 ) ) ;
#161918 = CARTESIAN_POINT ( 'NONE',  ( 0.2236267563471248943, -0.1037379595543522215, 2.204571545119632603 ) ) ;
#161919 = CARTESIAN_POINT ( 'NONE',  ( 2.319920442056855325, -2.194974118250800021, 0.5478587534586392138 ) ) ;
#161920 = CARTESIAN_POINT ( 'NONE',  ( -8.188761592974033832, 12.49737959187099179, -0.7216878364870267237 ) ) ;
#161921 = CARTESIAN_POINT ( 'NONE',  ( 2.566445574732978407, 0.6140501124722294035, 1.704450811836472734 ) ) ;
#161922 = CARTESIAN_POINT ( 'NONE',  ( 2.026450851813020648, 0.4238854151232730461, 1.868046764376835922 ) ) ;
#161923 = CIRCLE ( 'NONE', #182610, 1.868950538045371035 ) ;
#161924 = CARTESIAN_POINT ( 'NONE',  ( 3.631357695093720750, 0.05367941694835526995, -2.069842578854002468 ) ) ;
#161925 = CARTESIAN_POINT ( 'NONE',  ( -1.201851678989727383E-14, 3.259375000341420581, -1.575800808251660134 ) ) ;
#161926 = CARTESIAN_POINT ( 'NONE',  ( 1.692193703850993103, -1.961769708113933808, -0.1953840112930530781 ) ) ;
#161927 = CARTESIAN_POINT ( 'NONE',  ( 6.147092719882727430, -1.626042154682215468, 1.032876571686857536 ) ) ;
#161928 = CARTESIAN_POINT ( 'NONE',  ( 3.063207453921251489, 0.2760179531714930246, -1.850060308400132358 ) ) ;
#161930 = CARTESIAN_POINT ( 'NONE',  ( 4.681345713234763117, 8.384430392927429310, -0.5894114041281351968 ) ) ;
#161929 = CARTESIAN_POINT ( 'NONE',  ( 1.489377799468382113, -0.3424701664414407931, -2.282033458877083199 ) ) ;
#161931 = CARTESIAN_POINT ( 'NONE',  ( 2.453354322281832811, 1.436274109216955752, 1.183453651933939588 ) ) ;
#161932 = CARTESIAN_POINT ( 'NONE',  ( 1.364683531249988535, 3.405208333674749621, -0.7879004041258239610 ) ) ;
#161933 = CARTESIAN_POINT ( 'NONE',  ( 5.213357787468869020, -1.740689653174596563, -1.106377904087485486 ) ) ;
#161934 = CARTESIAN_POINT ( 'NONE',  ( -4.900382456335551140, 7.804531068111707270, 1.199719254218464037 ) ) ;
#161935 = CARTESIAN_POINT ( 'NONE',  ( 6.089583550832340819, 10.25626457594641749, 1.040834085586084257E-14 ) ) ;
#161936 = FACE_OUTER_BOUND ( 'NONE', #50614, .T. ) ;
#161937 = CARTESIAN_POINT ( 'NONE',  ( 5.877981411467888329, 1.251756350581848309, 1.693418440539447234 ) ) ;
#161938 = CARTESIAN_POINT ( 'NONE',  ( -1.364683531250012516, 2.842708333674754506, 0.7879004041258379498 ) ) ;
#161939 = CARTESIAN_POINT ( 'NONE',  ( 5.887991582945823588, -0.9777203880148609416, 1.927937229880334113 ) ) ;
#161940 = B_SPLINE_CURVE_WITH_KNOTS ( 'NONE', 3,
 ( #201055, #19117, #185881, #20180 ),
 .UNSPECIFIED., .F., .F.,
 ( 4, 4 ),
 ( 0.003649387816030439866, 0.004429296091066699421 ),
 .UNSPECIFIED. ) ;
#161941 = CARTESIAN_POINT ( 'NONE',  ( 6.129558478109055741, -0.2449627755865962375, 2.004677898944156489 ) ) ;
#161942 = CARTESIAN_POINT ( 'NONE',  ( -0.6823417656250246877, -0.6989583329919113464, 1.181850606188755259 ) ) ;
#161943 = CARTESIAN_POINT ( 'NONE',  ( -4.094199201646926412, 7.720390135322642067, 0.7216878364870317197 ) ) ;
#161946 = CARTESIAN_POINT ( 'NONE',  ( 4.039966587192250103, 7.657118751792200584, 0.7216878364870298324 ) ) ;
#161945 = CARTESIAN_POINT ( 'NONE',  ( 1.642778471875000035, -0.2260416661887081069, -2.845375778867859751 ) ) ;
#161944 = CARTESIAN_POINT ( 'NONE',  ( 7.049313524462606395, 7.188896964819984525, 0.000000000000000000 ) ) ;
#161947 = CARTESIAN_POINT ( 'NONE',  ( -4.899292406491858820, 6.809203455697518947, -1.599625672291271394 ) ) ;
#161948 = CARTESIAN_POINT ( 'NONE',  ( 4.522672878804367969, 0.3494810548456111499, 1.985869246038343583 ) ) ;
#161949 = CARTESIAN_POINT ( 'NONE',  ( -6.367525699912501835, 10.58053041653993098, -0.7998128361456291469 ) ) ;
#161951 = CARTESIAN_POINT ( 'NONE',  ( -6.577113915960836721, 8.766661883411348555, -1.443375672974066548 ) ) ;
#161950 = CARTESIAN_POINT ( 'NONE',  ( -7.998947442382709383, 12.27592974951444660, 0.7216878364870478180 ) ) ;
#161952 = CARTESIAN_POINT ( 'NONE',  ( -1.001543065824772872E-14, 5.071875000341421469, 1.575800808251672791 ) ) ;
#161954 = CARTESIAN_POINT ( 'NONE',  ( 0.6823417656249934904, 8.692708333674733723, 1.181850606188764807 ) ) ;
#161953 = CARTESIAN_POINT ( 'NONE',  ( 6.420800710400103917, 2.015122584031241004, 0.7829223626853940576 ) ) ;
#161955 = CARTESIAN_POINT ( 'NONE',  ( -11.77541522617479508, 7.697538928213582210, 2.075964864015985345 ) ) ;
#161956 = EDGE_CURVE ( 'NONE', #115502, #199511, #128140, .T. ) ;
#161958 = CARTESIAN_POINT ( 'NONE',  ( 0.3861688966736884776, -0.6463253627202453222, -1.803393044390422029 ) ) ;
#161957 = CARTESIAN_POINT ( 'NONE',  ( -7.009202228140755331, 8.240119356661432803, -1.082531754730543083 ) ) ;
#161959 = CARTESIAN_POINT ( 'NONE',  ( 0.6823417656249882723, -0.3447916663252489911, 1.181850606188755259 ) ) ;
#161960 = CARTESIAN_POINT ( 'NONE',  ( 1.453258822912409043, 0.5037300415833938505, -1.649688963556243282 ) ) ;
#161961 = CARTESIAN_POINT ( 'NONE',  ( 3.901714345682657292, 7.774026846596938434, 0.7998128361456271485 ) ) ;
#161963 = CARTESIAN_POINT ( 'NONE',  ( 5.020262018810099924, 9.078999131912302900, 0.7998128361456331437 ) ) ;
#161962 = CARTESIAN_POINT ( 'NONE',  ( 8.120970824905713314, 8.576813505252564696, 1.040834085586084257E-14 ) ) ;
#161964 = CARTESIAN_POINT ( 'NONE',  ( -10.66277494340078746, 5.899681303200420501, -5.512943113908496784 ) ) ;
#161965 = CARTESIAN_POINT ( 'NONE',  ( 6.766881895623299670, -1.710433013466134744, -0.7576501205904457859 ) ) ;
#161966 = CARTESIAN_POINT ( 'NONE',  ( 0.5748582965167781111, -1.456639466575420538, 1.389732462146851200 ) ) ;
#161967 = CARTESIAN_POINT ( 'NONE',  ( -0.3769810270651957618, 3.049942316455299451, -0.4288785890453079008 ) ) ;
#161968 = CARTESIAN_POINT ( 'NONE',  ( 3.364504783244476993, 0.9904720576699842516, 1.972067388187691339 ) ) ;
#161969 = CIRCLE ( 'NONE', #89453, 1.000000000000000000 ) ;
#161970 = CARTESIAN_POINT ( 'NONE',  ( 5.770445249457275771, -0.9694031614774318850, -1.942678356158732855 ) ) ;
#161971 = ORIENTED_EDGE ( 'NONE', *, *, #9881, .F. ) ;
#161972 = CARTESIAN_POINT ( 'NONE',  ( -3.895595285070177383, 2.800000000000024691, -0.7749999999999944711 ) ) ;
#161973 = CARTESIAN_POINT ( 'NONE',  ( 8.202319746143333035, 12.51319743723517952, -0.7216878364870328300 ) ) ;
#161975 = CARTESIAN_POINT ( 'NONE',  ( 2.337517745082304810, 0.5350678814987767096, -1.944078148028174136 ) ) ;
#161974 = CARTESIAN_POINT ( 'NONE',  ( 3.264422710156249963, 2.120667954687505574, -0.001943060928578931989 ) ) ;
#161977 = EDGE_LOOP ( 'NONE', ( #95316, #16847, #110882, #59527, #188500, #202593 ) ) ;
#161976 = CARTESIAN_POINT ( 'NONE',  ( 1.775370306292364031, 0.3070917902865456517, -1.785173024263370101 ) ) ;
#161978 = CARTESIAN_POINT ( 'NONE',  ( 6.821687566331318564, 7.987665577921906568, 1.199719254218452935 ) ) ;
#161979 = ORIENTED_EDGE ( 'NONE', *, *, #3283, .F. ) ;
#161980 = CARTESIAN_POINT ( 'NONE',  ( 6.148786358997489820, 7.132337826040578754, -1.199719254218446718 ) ) ;
#161982 = CARTESIAN_POINT ( 'NONE',  ( 0.9189787140968961321, -1.730522700298501304, 0.8221016984403562988 ) ) ;
#161981 = CARTESIAN_POINT ( 'NONE',  ( -4.874319919312905647, 5.645460313075203018, -1.199719254218446718 ) ) ;
#161983 = VECTOR ( 'NONE', #139821, 1000.000000000000227 ) ;
#161984 = CARTESIAN_POINT ( 'NONE',  ( -2.680951471028987232, 0.4698187958462037295, -0.1032074697909404620 ) ) ;
#161985 = CARTESIAN_POINT ( 'NONE',  ( -1.734723475976807094E-15, -9.900000000000005684, -10.91970695577494332 ) ) ;
#161986 = CARTESIAN_POINT ( 'NONE',  ( 6.792271770322100721, 7.026664608238323950, -0.7216878364870257245 ) ) ;
#161987 = CARTESIAN_POINT ( 'NONE',  ( -1.364683531250012516, 0.8427083336747532849, 0.7879004041258379498 ) ) ;
#161988 = CARTESIAN_POINT ( 'NONE',  ( 10.62873463776380056, 9.799999999999998934, -3.200000000000001510 ) ) ;
#161989 = CARTESIAN_POINT ( 'NONE',  ( -9.982881178363895103, 10.54111621771303753, 1.040834085586084257E-14 ) ) ;
#161990 = CARTESIAN_POINT ( 'NONE',  ( 5.770447993230207295, -1.374857387916775364, 1.668144713590607120 ) ) ;
#161991 = CARTESIAN_POINT ( 'NONE',  ( -3.987506576194992824, 7.666191748953863794, 0.7216878364870338292 ) ) ;
#161992 = CARTESIAN_POINT ( 'NONE',  ( 5.750066545971570520, 5.881034856487848295, -0.7216878364870458196 ) ) ;
#161993 = CARTESIAN_POINT ( 'NONE',  ( 2.531617689938488791, -0.2033970545941807817, 2.110794199748195599 ) ) ;
#161995 = CARTESIAN_POINT ( 'NONE',  ( -12.40359606095370992, 6.583381993447835256, -3.463844519762692364 ) ) ;
#161994 = CARTESIAN_POINT ( 'NONE',  ( -0.02988540731099428513, 6.948706544289728448, -2.321349141872154132 ) ) ;
#161996 = CARTESIAN_POINT ( 'NONE',  ( 3.760970446608974171, -1.736958583363076736, -0.9323722252271587907 ) ) ;
#161997 = CARTESIAN_POINT ( 'NONE',  ( 5.238497809344139000, 1.134185964801931679, -1.539638564045166857 ) ) ;
#161998 = VERTEX_POINT ( 'NONE', #153214 ) ;
#161999 = CARTESIAN_POINT ( 'NONE',  ( -2.020417662918760016, 3.956598013261175772, 11.36521191596583336 ) ) ;
#162000 = CARTESIAN_POINT ( 'NONE',  ( 0.3970419974134197783, 0.3524218036512065111, 2.039982198586967943 ) ) ;
#162001 = CARTESIAN_POINT ( 'NONE',  ( 2.853385946047338084, 1.932536089888321040, -0.1910151464093560736 ) ) ;
#162002 = VERTEX_POINT ( 'NONE', #70862 ) ;
#162003 = CARTESIAN_POINT ( 'NONE',  ( -4.308392981759444851, 7.251705977524093072, -0.9751457471971426427 ) ) ;
#162005 = CARTESIAN_POINT ( 'NONE',  ( 6.502017186205484300, 9.743381262951846367, -1.199719254218452047 ) ) ;
#162004 = CARTESIAN_POINT ( 'NONE',  ( -6.617788377246193399, 8.814115421577600529, -1.443375672974066548 ) ) ;
#162007 = CARTESIAN_POINT ( 'NONE',  ( 7.169564303528210836, 7.258913197071374945, -0.7998128361456281477 ) ) ;
#162006 = CARTESIAN_POINT ( 'NONE',  ( 2.115285117227220901, -2.027561382914280674, 0.5091250600777631474 ) ) ;
#162008 = CARTESIAN_POINT ( 'NONE',  ( 5.221298554594243413, 5.264138866547622975, -0.7216878364870458196 ) ) ;
#162010 = ORIENTED_EDGE ( 'NONE', *, *, #141317, .F. ) ;
#162009 = CARTESIAN_POINT ( 'NONE',  ( -0.02317427319796245069, -1.617030479356797334, -0.8165419217573687272 ) ) ;
#162011 = CARTESIAN_POINT ( 'NONE',  ( 3.932405576212230525, 1.181341412803040614, -1.863887651898883613 ) ) ;
#162012 = CARTESIAN_POINT ( 'NONE',  ( 3.065657736429776570, 0.3252250816505456998, -2.182562984848686938 ) ) ;
#162013 = CARTESIAN_POINT ( 'NONE',  ( 8.178592977541601527, 10.56477777859713463, 1.599625672291281386 ) ) ;
#162014 = CARTESIAN_POINT ( 'NONE',  ( -11.87815913191726480, 12.29692179368583282, 1.708869976696563819 ) ) ;
#162015 = CARTESIAN_POINT ( 'NONE',  ( 1.348149404638066873, 0.9416913409402676294, -1.664245089135652389 ) ) ;
#162016 = CARTESIAN_POINT ( 'NONE',  ( 11.33772465723203915, 13.50868300734825844, -3.600000000000076472 ) ) ;
#162017 = CARTESIAN_POINT ( 'NONE',  ( 4.176279081494421952, -1.061646348645030713, -1.777293304589353085 ) ) ;
#162019 = CARTESIAN_POINT ( 'NONE',  ( 3.028364643526501698, 1.202066397148596977, -1.796461956351296019 ) ) ;
#162018 = CARTESIAN_POINT ( 'NONE',  ( -0.7499999999999972244, 3.858333333333359594, -1.299038105676652011 ) ) ;
#162020 = CARTESIAN_POINT ( 'NONE',  ( 4.950807510372833065, -1.851323926424643274, -1.172527737679923465 ) ) ;
#162021 = CARTESIAN_POINT ( 'NONE',  ( 10.73535870392234237, 11.41900666419791399, 0.000000000000000000 ) ) ;
#162022 = DIRECTION ( 'NONE',  ( 5.551115123125764213E-17, 0.000000000000000000, -1.000000000000000000 ) ) ;
#162023 = CARTESIAN_POINT ( 'NONE',  ( -0.4942839625836717987, 7.528790859548558423, 2.012357903315129537 ) ) ;
#162024 = CARTESIAN_POINT ( 'NONE',  ( 6.235824307642648279, 6.239826211863360506, 0.000000000000000000 ) ) ;
#162025 = CARTESIAN_POINT ( 'NONE',  ( 1.001543065824772753E-15, -2.209374999522042859, 3.793834371823810780 ) ) ;
#162026 = CARTESIAN_POINT ( 'NONE',  ( -5.438755897737433287, 6.374245297895642537, -1.199719254218453823 ) ) ;
#162027 = CARTESIAN_POINT ( 'NONE',  ( 0.6861729220449981348, 1.650083401500940239, 1.158686392676591570 ) ) ;
#162028 = CARTESIAN_POINT ( 'NONE',  ( -8.839552966430012759, 10.37552855133225904, -1.082531754730543971 ) ) ;
#162029 = CARTESIAN_POINT ( 'NONE',  ( 4.996967907133109676, 0.3485794866864948549, 2.040532872733556768 ) ) ;
#162030 = CARTESIAN_POINT ( 'NONE',  ( 3.510301166856438115, -0.7815644168660453861, -1.761018089871415393 ) ) ;
#162031 = CARTESIAN_POINT ( 'NONE',  ( 5.554358401905552967, -1.342484540487314026, 1.637217851860258699 ) ) ;
#162032 = CARTESIAN_POINT ( 'NONE',  ( 6.634017235788401301, 6.634108284708264414, 0.7998128361456341429 ) ) ;
#162033 = CARTESIAN_POINT ( 'NONE',  ( 9.601932014265653237, 4.115787152683171080, 7.121345992675207626 ) ) ;
#162034 = CARTESIAN_POINT ( 'NONE',  ( 4.258625426654465862, -0.6138343748593175775, -1.871441549783653180 ) ) ;
#162035 = CARTESIAN_POINT ( 'NONE',  ( 6.369073578265099123, 2.195482680428318290, -0.6590174882785122534 ) ) ;
#162036 = CARTESIAN_POINT ( 'NONE',  ( 3.738726038629454074, 0.2694068579384527595, 1.805578518607708016 ) ) ;
#162037 = CARTESIAN_POINT ( 'NONE',  ( 7.675324359112103423, 8.127168971818530707, 0.7216878364870267237 ) ) ;
#162038 = CARTESIAN_POINT ( 'NONE',  ( 5.192409643909512873, 6.120528008391641350, -1.082531754730549078 ) ) ;
#162039 = CARTESIAN_POINT ( 'NONE',  ( -6.526270840131767059, 8.707344961610770540, -1.599625672291271394 ) ) ;
#162040 = CARTESIAN_POINT ( 'NONE',  ( 6.313256805818848960, 7.394496357324014113, 1.199719254218452047 ) ) ;
#162041 =( BOUNDED_CURVE ( )  B_SPLINE_CURVE ( 2, ( #102510, #168572, #205326, #126044, #159528 ),
 .UNSPECIFIED., .F., .T. ) 
 B_SPLINE_CURVE_WITH_KNOTS ( ( 3, 2, 3 ),
 ( 0.7343749999999997780, 0.7395833333333319271, 0.7499999999999956701 ),
 .UNSPECIFIED. ) 
 CURVE ( )  GEOMETRIC_REPRESENTATION_ITEM ( )  RATIONAL_B_SPLINE_CURVE ( ( 0.9330127018922194093, 0.9330127018922165227, 1.000000000000000000, 0.8660254037844944408, 0.9999999999999442668 ) ) 
 REPRESENTATION_ITEM ( '' )  );
#162042 = ORIENTED_EDGE ( 'NONE', *, *, #103885, .F. ) ;
#162044 = CARTESIAN_POINT ( 'NONE',  ( 5.396744779746093457, -1.965104602953187563, -0.4368240711251635822 ) ) ;
#162043 = CARTESIAN_POINT ( 'NONE',  ( 1.417261839328866513, -1.023339270300478221, -1.530466495063505628 ) ) ;
#162045 = CARTESIAN_POINT ( 'NONE',  ( 5.854147224351119227, 0.1731004610599009841, -2.292201554650086237 ) ) ;
#162046 = CARTESIAN_POINT ( 'NONE',  ( 5.612146373276853950, 1.959670608579218376, -0.09257137562097839112 ) ) ;
#162047 = CARTESIAN_POINT ( 'NONE',  ( -7.206322340863467346, 8.366129804884193888, 1.199719254218450271 ) ) ;
#162048 = CARTESIAN_POINT ( 'NONE',  ( -4.948889764188092677, 5.732458465429559169, 1.199719254218462483 ) ) ;
#162049 = DIRECTION ( 'NONE',  ( 5.551115123125765446E-17, 0.000000000000000000, -1.000000000000000000 ) ) ;
#162050 = CARTESIAN_POINT ( 'NONE',  ( -5.743814354044916470, 6.730146830254374990, -1.199719254218453823 ) ) ;
#162052 = CARTESIAN_POINT ( 'NONE',  ( 6.315310819269446263, -0.2119676446582714757, 1.757049200028695690 ) ) ;
#162051 = CARTESIAN_POINT ( 'NONE',  ( 1.523107970189445215, -1.967458627398379623, 0.7076814851830464104 ) ) ;
#162053 = CARTESIAN_POINT ( 'NONE',  ( 0.3562281372918948974, 7.169715878026163836, -1.968597608854716574 ) ) ;
#162054 = CARTESIAN_POINT ( 'NONE',  ( -0.1106727585416201337, 1.364743060583981649, -2.259751816641343058 ) ) ;
#162055 = CARTESIAN_POINT ( 'NONE',  ( 0.7842107965865081631, 1.535900883440274090, -0.8186502264825399333 ) ) ;
#162056 = AXIS2_PLACEMENT_3D ( 'NONE', #166437, #84115, #162190 ) ;
#162057 = CARTESIAN_POINT ( 'NONE',  ( 4.774442650306744085, 8.721933525333202653, -0.7998128361456281477 ) ) ;
#162059 = CARTESIAN_POINT ( 'NONE',  ( 1.518728846951481470, 8.688592980705456270, 2.528358009378040450 ) ) ;
#162058 = CARTESIAN_POINT ( 'NONE',  ( 0.005768037945334394262, 14.55305234682519533, 11.95586101163397963 ) ) ;
#162060 = CARTESIAN_POINT ( 'NONE',  ( 1.664246808422519486, -1.221613929703774915, 1.218001262086549907 ) ) ;
#162061 = CARTESIAN_POINT ( 'NONE',  ( 1.962683346935737205, -2.005255389829229351, -0.8846387633431598285 ) ) ;
#162062 = CARTESIAN_POINT ( 'NONE',  ( 4.617920694193921705, -2.164688156338661962, 0.4286357439418769788 ) ) ;
#162063 = LINE ( 'NONE', #13652, #63953 ) ;
#162064 = CARTESIAN_POINT ( 'NONE',  ( 1.639757756142570244, 2.007014814066264474, -0.8283606533975582664 ) ) ;
#162065 = CARTESIAN_POINT ( 'NONE',  ( 0.5041868517345666767, -0.6120625888205477594, -1.720162557568189809 ) ) ;
#162066 = CARTESIAN_POINT ( 'NONE',  ( 3.819616621146375568, -1.462967937902563964, -1.530840818714680029 ) ) ;
#162067 = CARTESIAN_POINT ( 'NONE',  ( 3.497640442201256139, 7.024404915969360452, 1.040834085586084257E-14 ) ) ;
#162068 = ORIENTED_EDGE ( 'NONE', *, *, #198514, .F. ) ;
#162069 = CIRCLE ( 'NONE', #44573, 0.08000000000000025147 ) ;
#162071 = CARTESIAN_POINT ( 'NONE',  ( 1.364683531249988757, -0.05312499965857975237, 0.000000000000000000 ) ) ;
#162070 = CARTESIAN_POINT ( 'NONE',  ( 3.158078472442786833, 1.032628797542353816, 2.046708512074166819 ) ) ;
#162072 = CARTESIAN_POINT ( 'NONE',  ( 4.761938266897790761, 6.578680616179308771, 1.599625672291267398 ) ) ;
#162073 = CARTESIAN_POINT ( 'NONE',  ( 5.602238577124374785, -1.000643217919431116, 1.983199510308247815 ) ) ;
#162074 = CARTESIAN_POINT ( 'NONE',  ( -6.182154858151506893, 9.195969186943299789, 1.082531754730548412 ) ) ;
#162075 = ADVANCED_FACE ( 'NONE', ( #136977 ), #201925, .F. ) ;
#162076 = CARTESIAN_POINT ( 'NONE',  ( 4.528060117284229413, 7.266191989264828344, 1.082531754730558626 ) ) ;
#162077 = CARTESIAN_POINT ( 'NONE',  ( -5.870317324592805086, 9.792527945426188651, -0.7216878364870197293 ) ) ;
#162078 = CARTESIAN_POINT ( 'NONE',  ( 4.204437034013637664, 6.958908068774287692, -1.082531754730548412 ) ) ;
#162079 = VERTEX_POINT ( 'NONE', #90361 ) ;
#162080 = CARTESIAN_POINT ( 'NONE',  ( 3.744767666119628746, 2.000857235306313875, -0.2496062519145719194 ) ) ;
#162082 = CARTESIAN_POINT ( 'NONE',  ( 2.606363979242664719, 2.062007909489747881, 0.05513178878350195877 ) ) ;
#162081 = CARTESIAN_POINT ( 'NONE',  ( 5.286789834324991055, 8.255339675766103724, -1.199719254218452935 ) ) ;
#162083 = DIRECTION ( 'NONE',  ( -0.000000000000000000, -1.000000000000000000, -0.000000000000000000 ) ) ;
#162084 = CARTESIAN_POINT ( 'NONE',  ( 6.021229617800532452, 6.197391773621639288, 0.000000000000000000 ) ) ;
#162085 = ORIENTED_EDGE ( 'NONE', *, *, #60288, .T. ) ;
#162086 = FACE_OUTER_BOUND ( 'NONE', #211310, .T. ) ;
#162087 = CARTESIAN_POINT ( 'NONE',  ( 1.364683531249990311, 4.384375000341417028, 1.214306433183764966E-14 ) ) ;
#162088 = CARTESIAN_POINT ( 'NONE',  ( 5.472676780243426187, -0.05103125619924236966, -2.191024458042860168 ) ) ;
#162089 = CARTESIAN_POINT ( 'NONE',  ( 2.901017702322743919, -0.9963018188003970321, -1.753030416019534021 ) ) ;
#162090 = CARTESIAN_POINT ( 'NONE',  ( 1.663359199420410883, 0.9473472845980964729, 1.578708189602283873 ) ) ;
#162091 = EDGE_CURVE ( 'NONE', #96092, #96576, #177177, .T. ) ;
#162092 = CARTESIAN_POINT ( 'NONE',  ( 6.584456157731144899, 10.83361595066169514, -0.7998128361456291469 ) ) ;
#162093 =( NAMED_UNIT ( * ) SI_UNIT ( $, .STERADIAN. ) SOLID_ANGLE_UNIT ( ) );
#162094 = CARTESIAN_POINT ( 'NONE',  ( 5.807590115592688562, -0.4411735188285180187, 1.771332044933016547 ) ) ;
#162095 = CARTESIAN_POINT ( 'NONE',  ( 5.713517581197447015, 1.944070655204039433, 0.5350908816983344085 ) ) ;
#162096 = CARTESIAN_POINT ( 'NONE',  ( -7.178152263431422320, 10.46192917639026554, 1.199719254218453823 ) ) ;
#162098 = CARTESIAN_POINT ( 'NONE',  ( -6.119526231721793330, 8.232809585132461194, 1.599625672291263179 ) ) ;
#162097 = CARTESIAN_POINT ( 'NONE',  ( 5.331070463540595661, 0.1608317336210095816, 2.256856606938316023 ) ) ;
#162099 = CARTESIAN_POINT ( 'NONE',  ( 0.9968619785027620361, -0.5136065205212798634, -2.042351051948914531 ) ) ;
#162100 = CARTESIAN_POINT ( 'NONE',  ( -5.399890319992785237, 9.521898816625391504, 0.7998128361456291469 ) ) ;
#162101 = CARTESIAN_POINT ( 'NONE',  ( 9.836604141914616406, 11.43479190611061647, 1.199719254218452047 ) ) ;
#162102 = CARTESIAN_POINT ( 'NONE',  ( 1.360316468749964480, 2.796875000341370043, -3.989863994746656317E-14 ) ) ;
#162103 = DIRECTION ( 'NONE',  ( -7.901936524335548973E-16, -1.000000000000000000, 2.815447810940011413E-16 ) ) ;
#162104 = MANIFOLD_SOLID_BREP ( 'Sweep1[12]', #1556 ) ;
#162105 = CARTESIAN_POINT ( 'NONE',  ( -6.516665389662827934, 10.75452672124865217, 0.000000000000000000 ) ) ;
#162106 = CARTESIAN_POINT ( 'NONE',  ( 7.635176783151273128, 8.936736330878529699, 1.199719254218452935 ) ) ;
#162107 = CARTESIAN_POINT ( 'NONE',  ( 5.144285979226959959, 6.473071224410549718, -1.197504025336363576 ) ) ;
#162108 = CARTESIAN_POINT ( 'NONE',  ( -8.324343129110692630, 12.65555805069709550, 0.7216878364870338292 ) ) ;
#162109 = CARTESIAN_POINT ( 'NONE',  ( 2.531719857061366152, -0.2131849592692437734, 2.211133432850121761 ) ) ;
#162110 = DIRECTION ( 'NONE',  ( 1.276756478318932585E-15, -1.000000000000000000, 1.665334536937738262E-16 ) ) ;
#162111 = CARTESIAN_POINT ( 'NONE',  ( -6.771371375382467583, 6.864631124226471037, -0.7998128361456362523 ) ) ;
#162112 = CARTESIAN_POINT ( 'NONE',  ( 6.474182045725470402, 7.511966127223233869, -1.199719254218446718 ) ) ;
#162113 = CARTESIAN_POINT ( 'NONE',  ( 3.262109210011232108, -1.959739898415867154, 0.09363895518171151677 ) ) ;
#162114 = CARTESIAN_POINT ( 'NONE',  ( 5.341022448779654930, 8.318611059296550536, 1.199719254218462483 ) ) ;
#162115 = CARTESIAN_POINT ( 'NONE',  ( -4.183520347117292815, 7.398805986154902037, 0.7851016128354749712 ) ) ;
#162116 = CARTESIAN_POINT ( 'NONE',  ( 2.510230996824538430, 6.080353262937265413, 0.000000000000000000 ) ) ;
#162117 = CARTESIAN_POINT ( 'NONE',  ( -4.909461021924285795, 6.821066840368686712, 1.443375672974058777 ) ) ;
#162118 = CARTESIAN_POINT ( 'NONE',  ( -7.565086526745425033, 7.928281824065535055, 0.7216878364870317197 ) ) ;
#162120 = CARTESIAN_POINT ( 'NONE',  ( 2.039458538997685366, 0.004855507148140979744, 2.120778211687989856 ) ) ;
#162119 = COLOUR_RGB ( '', 0.09019608, 0.27058824, 0.51372549) ;
#162121 = CARTESIAN_POINT ( 'NONE',  ( -3.935609729716867289, 7.813571461303467913, 0.7998128361456352531 ) ) ;
#162122 = CARTESIAN_POINT ( 'NONE',  ( 4.487301133948972343, 1.932317252032596633, -0.9692046190768679459 ) ) ;
#162123 = CARTESIAN_POINT ( 'NONE',  ( 3.175182228840720544, 1.170341537027960843, 1.421418621496411294 ) ) ;
#162124 = CARTESIAN_POINT ( 'NONE',  ( -4.397013243575890407, 7.155424720373004810, 1.066431095959238462 ) ) ;
#162125 = EDGE_CURVE ( 'NONE', #8852, #38245, #76232, .T. ) ;
#162126 = CARTESIAN_POINT ( 'NONE',  ( 0.6823417656249864960, -0.5114583329919111243, -1.181850606188749264 ) ) ;
#162127 = CARTESIAN_POINT ( 'NONE',  ( 5.525286087770139964, -1.108758243214434724, -1.341423578285575235 ) ) ;
#162128 = DIRECTION ( 'NONE',  ( -0.000000000000000000, -1.000000000000000000, -0.000000000000000000 ) ) ;
#162129 = CARTESIAN_POINT ( 'NONE',  ( 5.016153647376217606, 4.954526798134778254, 0.7216878364870317197 ) ) ;
#162130 = CARTESIAN_POINT ( 'NONE',  ( -0.4350533259329449343, -9.438199013093624856, 9.251577493846887990 ) ) ;
#162131 = CARTESIAN_POINT ( 'NONE',  ( 2.993221558690632556, 1.854768100113469265, -1.110066390340218367 ) ) ;
#162132 = CARTESIAN_POINT ( 'NONE',  ( 4.218124927476913477, -1.674631575811252215, -1.122325875776951420 ) ) ;
#162133 = CARTESIAN_POINT ( 'NONE',  ( -9.463228032214294316, 10.14278024711257764, 1.040834085586084257E-14 ) ) ;
#162134 = AXIS2_PLACEMENT_3D ( 'NONE', #124572, #10715, #141845 ) ;
#162135 = CARTESIAN_POINT ( 'NONE',  ( 2.395597313961893349, 1.670541196947441520, 1.371929806955954012 ) ) ;
#162136 = CARTESIAN_POINT ( 'NONE',  ( 2.759003776822867238, -1.713332664616385781, -0.9749793123631170788 ) ) ;
#162137 = ADVANCED_FACE ( 'NONE', ( #26406 ), #117744, .T. ) ;
#162138 = CARTESIAN_POINT ( 'NONE',  ( 6.509000000000013664, 7.052434016701248254, 2.698154332336550887 ) ) ;
#162139 = CARTESIAN_POINT ( 'NONE',  ( 4.810071659083087425, 1.336522264689719686, -1.409242981738271894 ) ) ;
#162142 = VERTEX_POINT ( 'NONE', #77298 ) ;
#162141 = DIRECTION ( 'NONE',  ( 5.551115123125766062E-17, 0.000000000000000000, -1.000000000000000000 ) ) ;
#162140 = CARTESIAN_POINT ( 'NONE',  ( -9.124274191872640216, 10.70770331434866485, -1.082531754730537976 ) ) ;
#162144 = ADVANCED_FACE ( 'NONE', ( #95715 ), #124726, .T. ) ;
#162143 = CARTESIAN_POINT ( 'NONE',  ( -5.112833325684928987, 5.137596099486740897, -0.7216878364870338292 ) ) ;
#162145 = DIRECTION ( 'NONE',  ( 1.084202172485362439E-14, -1.000000000000000000, 3.260636891504970529E-14 ) ) ;
#162147 = ORIENTED_EDGE ( 'NONE', *, *, #161592, .T. ) ;
#162146 = CARTESIAN_POINT ( 'NONE',  ( -4.899292406491858820, 6.809203455697518947, -1.599625672291271394 ) ) ;
#162148 = CARTESIAN_POINT ( 'NONE',  ( -9.625925875578284163, 10.33259439770390564, 1.040834085586084257E-14 ) ) ;
#162149 = CARTESIAN_POINT ( 'NONE',  ( 0.9739772326014315418, 2.126351460888118883, -0.5901193814053447007 ) ) ;
#162150 = CARTESIAN_POINT ( 'NONE',  ( -3.285556943750000514, -1.888541666188711110, -1.896917185911906500 ) ) ;
#162151 = CARTESIAN_POINT ( 'NONE',  ( 5.067221110791254368, 1.704927679941736329, 0.9703409489375602881 ) ) ;
#162152 = FACE_OUTER_BOUND ( 'NONE', #73796, .T. ) ;
#162153 = CARTESIAN_POINT ( 'NONE',  ( 0.7499999999999920064, 4.764583334016150751, 1.299038105676669330 ) ) ;
#162154 = CARTESIAN_POINT ( 'NONE',  ( 4.983022828693913553, 6.814620138096638691, -1.425645453754071257 ) ) ;
#162155 = DIRECTION ( 'NONE',  ( -7.610300982150707428E-15, -1.000000000000000000, 7.722633184682877167E-15 ) ) ;
#162156 = CARTESIAN_POINT ( 'NONE',  ( 4.576008823784957436, -1.786506429242448624, -0.4446734633927542091 ) ) ;
#162157 = ORIENTED_EDGE ( 'NONE', *, *, #109604, .T. ) ;
#162158 = CARTESIAN_POINT ( 'NONE',  ( -1.360316468750021768, -1.109374999658574446, -3.122502256758252770E-14 ) ) ;
#162159 = CARTESIAN_POINT ( 'NONE',  ( -7.914208982075130905, 10.25632978388623684, -1.599625672291263179 ) ) ;
#162160 = CYLINDRICAL_SURFACE ( 'NONE', #6580, 1.500000000000000222 ) ;
#162161 = CARTESIAN_POINT ( 'NONE',  ( 6.152600690169603759, 2.097733681304454034, 0.3095894981632040244 ) ) ;
#162162 = SURFACE_STYLE_USAGE ( .BOTH. , #79823 ) ;
#162163 = CARTESIAN_POINT ( 'NONE',  ( 5.880485940025228508, 7.883652901494672349, 1.599625672291267398 ) ) ;
#162164 = CARTESIAN_POINT ( 'NONE',  ( 6.661407821810922947, 0.3568556019579691707, -2.029490769664368255 ) ) ;
#162165 = MECHANICAL_DESIGN_GEOMETRIC_PRESENTATION_REPRESENTATION (  '', ( #103387 ), #127616 ) ;
#162168 = CARTESIAN_POINT ( 'NONE',  ( 3.298233973420101606, 1.449563003725433896, -1.135193286699177628 ) ) ;
#162167 = CARTESIAN_POINT ( 'NONE',  ( 1.785388869275974955, -1.753811856250932610, 0.6230531623785877660 ) ) ;
#162166 = CARTESIAN_POINT ( 'NONE',  ( -10.41415007634638989, 5.040604921122249671, 5.873056126304751601 ) ) ;
#162169 = CARTESIAN_POINT ( 'NONE',  ( 7.476431642932036326, 10.80992178580769014, 1.199719254218460707 ) ) ;
#162170 = CARTESIAN_POINT ( 'NONE',  ( -11.21553972792701259, 3.696394713403124754, 3.679259263401783553 ) ) ;
#162171 = CARTESIAN_POINT ( 'NONE',  ( -7.632314129850253259, 7.869064337772231355, 0.7998128361456341429 ) ) ;
#162172 = CARTESIAN_POINT ( 'NONE',  ( -9.501690547401159037, -8.186910008819943130, 0.4655726814551116033 ) ) ;
#162173 = CARTESIAN_POINT ( 'NONE',  ( 2.842613246588860942, 2.190307313262893185, 0.2694104812042824038 ) ) ;
#162174 = CARTESIAN_POINT ( 'NONE',  ( 5.800151253372650473, -2.262578822528161560, -0.008439264561578212892 ) ) ;
#162175 = CARTESIAN_POINT ( 'NONE',  ( -5.531363484695544841, 8.436712584578003771, 1.082531754730548412 ) ) ;
#162176 = CARTESIAN_POINT ( 'NONE',  ( 6.258062559271784231, 0.6844122130202813237, -1.677549884021255933 ) ) ;
#162177 = CARTESIAN_POINT ( 'NONE',  ( 5.542171544414384421, 0.7827158775690710169, 1.748735243013665785 ) ) ;
#162178 = CARTESIAN_POINT ( 'NONE',  ( 3.912682303000288631, 8.998411203033816363, 0.7749999999999996891 ) ) ;
#162179 = CARTESIAN_POINT ( 'NONE',  ( 6.157094445334826638, -1.605393284960114242, -0.9600186418455139981 ) ) ;
#162180 = AXIS2_PLACEMENT_3D ( 'NONE', #49781, #84412, #67064 ) ;
#162181 = CARTESIAN_POINT ( 'NONE',  ( 5.916418678859147740, 0.7547467877644217227, 1.701316312257817875 ) ) ;
#162182 = CARTESIAN_POINT ( 'NONE',  ( -10.50059885609813115, 5.377696206510352184, -5.808392519734754345 ) ) ;
#162183 = CARTESIAN_POINT ( 'NONE',  ( 5.998865924308096176, 1.444533723251522073, -1.022291996631684574 ) ) ;
#162184 = CARTESIAN_POINT ( 'NONE',  ( 0.9191581010105540628, -1.820984308097562954, 0.8666112775468015617 ) ) ;
#162186 = CARTESIAN_POINT ( 'NONE',  ( 2.895255201988570892, 1.806112693971681615, -1.083030686944158161 ) ) ;
#162185 = CARTESIAN_POINT ( 'NONE',  ( -9.450196763925152510, 10.98398329845622001, -1.199719254218441611 ) ) ;
#162187 = CARTESIAN_POINT ( 'NONE',  ( 9.097684769969825780, 10.57271930550834860, -1.199719254218446718 ) ) ;
#162189 = CARTESIAN_POINT ( 'NONE',  ( -9.989660255170729641, 10.54902514065433827, -0.7998128361456291469 ) ) ;
#162188 = CARTESIAN_POINT ( 'NONE',  ( -1.500000000000013101, -0.07916666666664513852, 0.8660254037844403729 ) ) ;
#162190 = DIRECTION ( 'NONE',  ( 0.000000000000000000, 0.000000000000000000, 1.000000000000000000 ) ) ;
#162191 = CARTESIAN_POINT ( 'NONE',  ( 3.322525440707891242, -0.8223705904544276191, -1.844992516297422780 ) ) ;
#162192 = CARTESIAN_POINT ( 'NONE',  ( -1.201851678989727383E-14, 2.821875000341418804, 1.575800808251672791 ) ) ;
#162193 = CARTESIAN_POINT ( 'NONE',  ( 3.979481780810941949, 4.601482484822914998, 1.199719254218464037 ) ) ;
#162194 = CARTESIAN_POINT ( 'NONE',  ( 3.585389192675687564, 1.955840111083558597, -0.9206723451176119788 ) ) ;
#162195 = CARTESIAN_POINT ( 'NONE',  ( 6.003228155800906407, 10.22579295840155744, 0.000000000000000000 ) ) ;
#162197 = CARTESIAN_POINT ( 'NONE',  ( -10.99999999999737632, 0.000000000000000000, 0.4330127018937083849 ) ) ;
#162196 = CARTESIAN_POINT ( 'NONE',  ( 5.993586425693011144, 9.150212042353954800, -1.199719254218452047 ) ) ;
#162198 = CARTESIAN_POINT ( 'NONE',  ( 8.053180056393003383, 12.33920113252646367, 1.040834085586084257E-14 ) ) ;
#162200 = CARTESIAN_POINT ( 'NONE',  ( 1.220146605508150803E-14, 9.937500000000000000, -1.499999999999998446 ) ) ;
#162199 = CARTESIAN_POINT ( 'NONE',  ( 1.082764339582122481, 1.293380948865870073, -1.743738868014677035 ) ) ;
#162201 = CARTESIAN_POINT ( 'NONE',  ( -5.558479791922849245, 9.428717490644563881, 0.7216878364870458196 ) ) ;
#162202 = CARTESIAN_POINT ( 'NONE',  ( -1.201851678989727383E-14, 1.071875000341418138, 1.575800808251672791 ) ) ;
#162203 = CARTESIAN_POINT ( 'NONE',  ( 2.085717061910817183, -0.9337068281064246911, 1.982830571388309204 ) ) ;
#162204 = CARTESIAN_POINT ( 'NONE',  ( 0.4465194593917913846, 3.080450244942120719, -0.4155024747329958412 ) ) ;
#162205 = CARTESIAN_POINT ( 'NONE',  ( 3.081239027650189310, -0.1650901621712965450, -2.256537306257479614 ) ) ;
#162206 = CARTESIAN_POINT ( 'NONE',  ( -6.984421689334302741, 11.30024240419870374, 0.000000000000000000 ) ) ;
#162207 = ADVANCED_FACE ( 'NONE', ( #27477 ), #157502, .F. ) ;
#162208 = CARTESIAN_POINT ( 'NONE',  ( -4.243338890952911058, 5.013278796608906518, -1.082531754730543971 ) ) ;
#162210 = AXIS2_PLACEMENT_3D ( 'NONE', #149674, #166995, #1255 ) ;
#162209 = CARTESIAN_POINT ( 'NONE',  ( -1.201851678989727383E-14, 3.759375000341422801, -1.575800808251660134 ) ) ;
#162211 = CARTESIAN_POINT ( 'NONE',  ( 5.370783296855561773, 7.572579728427998091, 1.242435897699250891 ) ) ;
#162212 = CARTESIAN_POINT ( 'NONE',  ( -1.500000000000015099, 10.72916666666666607, -0.8660254037844309360 ) ) ;
#162213 = CARTESIAN_POINT ( 'NONE',  ( 5.709392085130549077, 9.675058176045386205, 0.000000000000000000 ) ) ;
#162214 = CARTESIAN_POINT ( 'NONE',  ( 3.321328847770131709, -1.706417891748934546, 0.4689366942724793041 ) ) ;
#162215 = CARTESIAN_POINT ( 'NONE',  ( 9.596473800374404561, 10.09030761005864285, 0.000000000000000000 ) ) ;
#162216 = CARTESIAN_POINT ( 'NONE',  ( 5.930760676324511316, 2.125237774816424619, 0.5940772278362898007 ) ) ;
#162217 = CARTESIAN_POINT ( 'NONE',  ( -1.364683531250010295, 9.130208333674731946, 0.7879004041258445001 ) ) ;
#162218 = CIRCLE ( 'NONE', #75777, 0.07999999999999993228 ) ;
#162219 = CARTESIAN_POINT ( 'NONE',  ( -5.798046968499580345, 6.793418213784815585, 1.199719254218452935 ) ) ;
#162220 = CARTESIAN_POINT ( 'NONE',  ( 5.782827418265350516, 1.646828846085298448, -1.163285542026312847 ) ) ;
#162221 = ORIENTED_EDGE ( 'NONE', *, *, #2058, .F. ) ;
#162222 = B_SPLINE_CURVE_WITH_KNOTS ( 'NONE', 3,
 ( #44285, #174297, #189452, #24806, #43230, #110406 ),
 .UNSPECIFIED., .F., .F.,
 ( 4, 2, 4 ),
 ( 0.000000000000000000, 0.0007391056041462109151, 0.001478211208292421830 ),
 .UNSPECIFIED. ) ;
#162223 = CARTESIAN_POINT ( 'NONE',  ( 3.449935675575486638, 1.870836310073907827, 0.001118452434160921221 ) ) ;
#162224 = CARTESIAN_POINT ( 'NONE',  ( 3.379797469122407083, -1.996479967689598789, 0.5476083754193948883 ) ) ;
#162225 = CARTESIAN_POINT ( 'NONE',  ( -6.577113915960836721, 8.766661883411348555, -1.443375672974066548 ) ) ;
#162226 = CARTESIAN_POINT ( 'NONE',  ( -11.00592740523952351, 11.11020242468316788, 1.444008943503716225 ) ) ;
#162227 = CARTESIAN_POINT ( 'NONE',  ( -9.979823206198361163, 5.589814398814591634, -5.978750339097100408 ) ) ;
#162228 = CARTESIAN_POINT ( 'NONE',  ( -5.817856928050925802, 5.960123635580414359, -1.359047942450207100E-08 ) ) ;
#162229 = CARTESIAN_POINT ( 'NONE',  ( -1.364683531250000748, -1.240624999658580752, 0.000000000000000000 ) ) ;
#162230 = CARTESIAN_POINT ( 'NONE',  ( 3.244534624505683418, -1.932379277470747558, -0.3379807920969243873 ) ) ;
#162231 = CARTESIAN_POINT ( 'NONE',  ( 1.458361007166041112, 1.524808354686446599, 1.319028796778199508 ) ) ;
#162232 = CARTESIAN_POINT ( 'NONE',  ( -10.50000000000000000, 10.19999999999999929, -3.600000000000000977 ) ) ;
#162234 = DIRECTION ( 'NONE',  ( -1.000000000000000000, 1.224646799147352714E-16, 0.000000000000000000 ) ) ;
#162233 = CARTESIAN_POINT ( 'NONE',  ( 6.909851844459134362, 11.21324425184434936, -0.7998128361456291469 ) ) ;
#162235 = CARTESIAN_POINT ( 'NONE',  ( 0.5263522483448194178, 1.788089326329355577, 0.5492086291003297482 ) ) ;
#162236 = CARTESIAN_POINT ( 'NONE',  ( -1.364683531249997417, 3.759375000341423689, 1.214306433183764966E-14 ) ) ;
#162237 = CARTESIAN_POINT ( 'NONE',  ( 2.215092046557234795, 1.614471179978003823, -1.202476892717120105 ) ) ;
#162239 = CARTESIAN_POINT ( 'NONE',  ( 2.759486767256282391, 2.009531813720342175, -0.6668115938158604150 ) ) ;
#162238 = CARTESIAN_POINT ( 'NONE',  ( -7.131225611108100715, 9.342849184424693476, 1.443375672974078761 ) ) ;
#162240 = CARTESIAN_POINT ( 'NONE',  ( 6.928203230275524760, 14.48154074412737202, -9.797958971132702644 ) ) ;
#162241 = CARTESIAN_POINT ( 'NONE',  ( 3.771986465066007099, -2.040223509676724500, 0.3510349978646867264 ) ) ;
#162242 = CARTESIAN_POINT ( 'NONE',  ( 5.806634928402749196, 9.996434193103704402, -0.7998128361456481317 ) ) ;
#162243 = CARTESIAN_POINT ( 'NONE',  ( 6.333939708931282553, 2.067699390258682879, 0.3079354192142729763 ) ) ;
#162245 = ORIENTED_EDGE ( 'NONE', *, *, #14587, .F. ) ;
#162244 = CARTESIAN_POINT ( 'NONE',  ( 4.401258566127845384, 1.466438172381477445, 1.087111955044787859 ) ) ;
#162246 = CARTESIAN_POINT ( 'NONE',  ( 8.204655514564224816, 12.72384853363364066, 1.040834085586084257E-14 ) ) ;
#162247 = DIRECTION ( 'NONE',  ( 0.000000000000000000, 0.000000000000000000, -1.000000000000000000 ) ) ;
#162248 = CARTESIAN_POINT ( 'NONE',  ( 12.00693267275518572, 8.237831693621128437, -3.583085096157309302 ) ) ;
#162249 = CARTESIAN_POINT ( 'NONE',  ( -10.43230948805442893, 5.066484524551064794, 5.254757398418679060 ) ) ;
#162250 = CARTESIAN_POINT ( 'NONE',  ( -0.6823417656250039265, 10.88020833367472839, -1.181850606188755259 ) ) ;
#162251 = CARTESIAN_POINT ( 'NONE',  ( 5.654919265238161685, 0.3773621422162172223, 1.874504418562010999 ) ) ;
#162252 = CARTESIAN_POINT ( 'NONE',  ( -9.592557376868645846, 11.15007068022363157, -1.199719254218441611 ) ) ;
#162253 = VECTOR ( 'NONE', #29399, 1000.000000000000000 ) ;
#162254 = CARTESIAN_POINT ( 'NONE',  ( 6.337546739384100292, 9.481222731668410120, 1.199719254218460707 ) ) ;
#162255 = CARTESIAN_POINT ( 'NONE',  ( 1.360316468750005781, 1.567708333674729504, -0.7853790794158981292 ) ) ;
#162256 = CARTESIAN_POINT ( 'NONE',  ( 4.216222583725566686, 4.981643104843690217, -1.082531754730548412 ) ) ;
#162257 = CARTESIAN_POINT ( 'NONE',  ( 9.492545994385622521, -8.199730735665681891, -0.3846410972799483852 ) ) ;
#162258 = CARTESIAN_POINT ( 'NONE',  ( 0.8547319020580852467, 0.3593373433725781108, -1.805665335529122784 ) ) ;
#162259 = EDGE_LOOP ( 'NONE', ( #111595, #135538, #166785, #24799 ) ) ;
#162260 = CARTESIAN_POINT ( 'NONE',  ( -5.915100157312088491, 10.12297696016459092, -0.7998128361456362523 ) ) ;
#162261 = ADVANCED_FACE ( 'NONE', ( #93575 ), #48571, .T. ) ;
